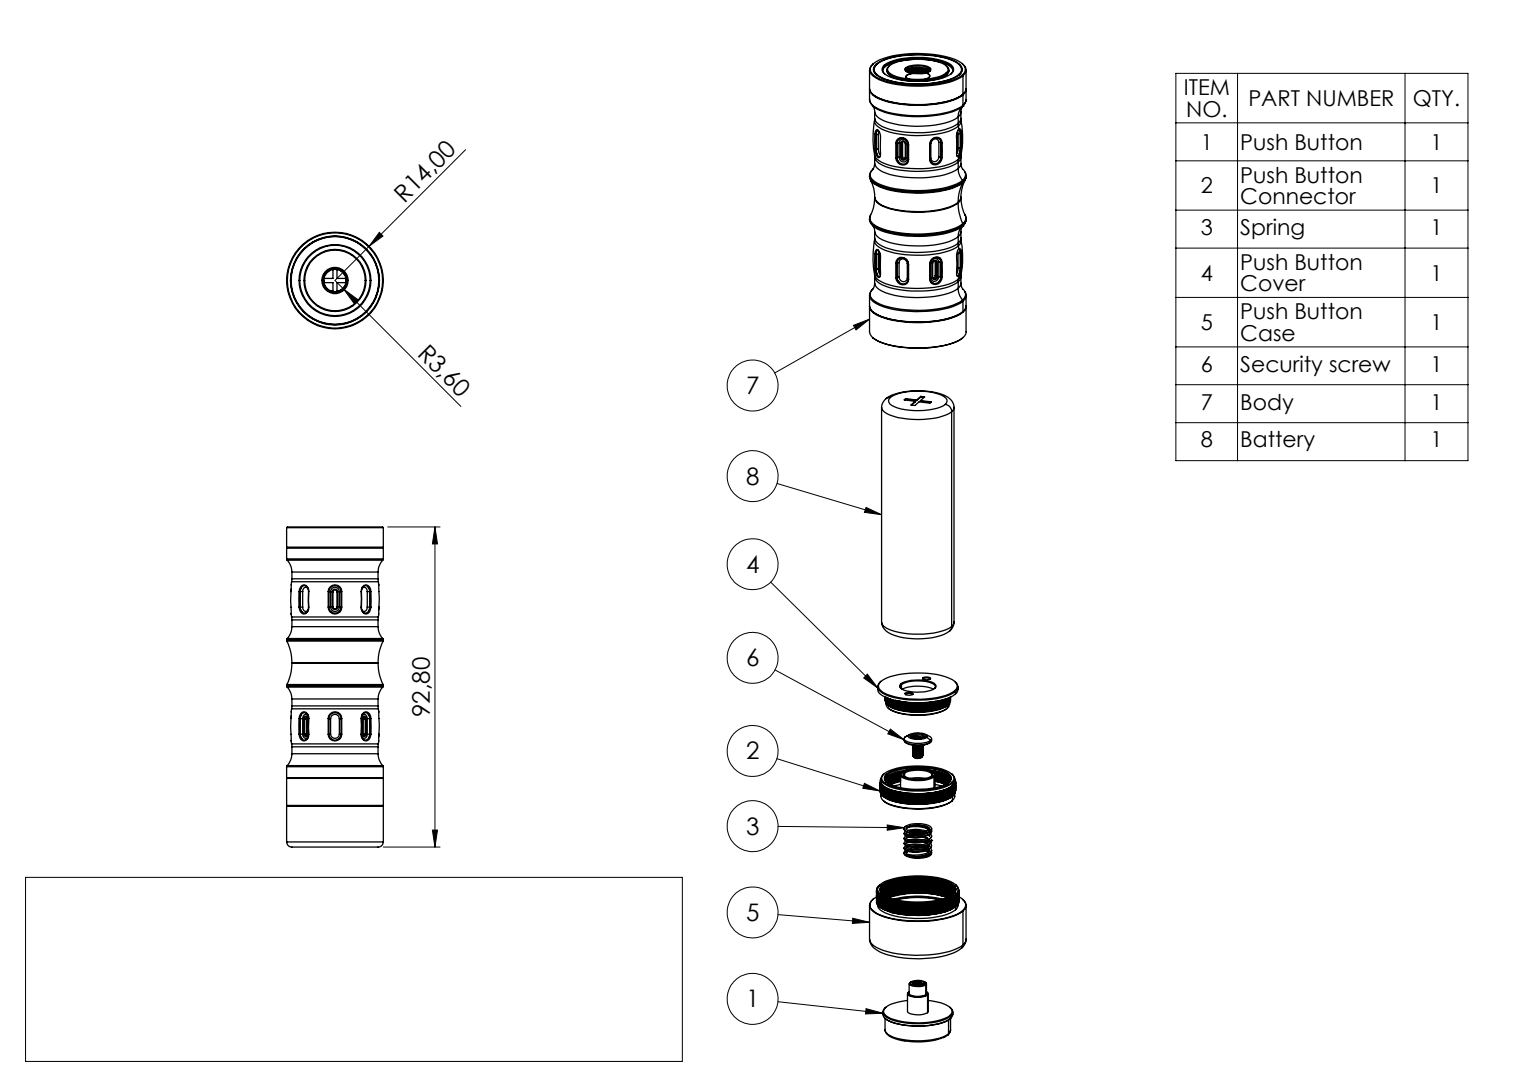
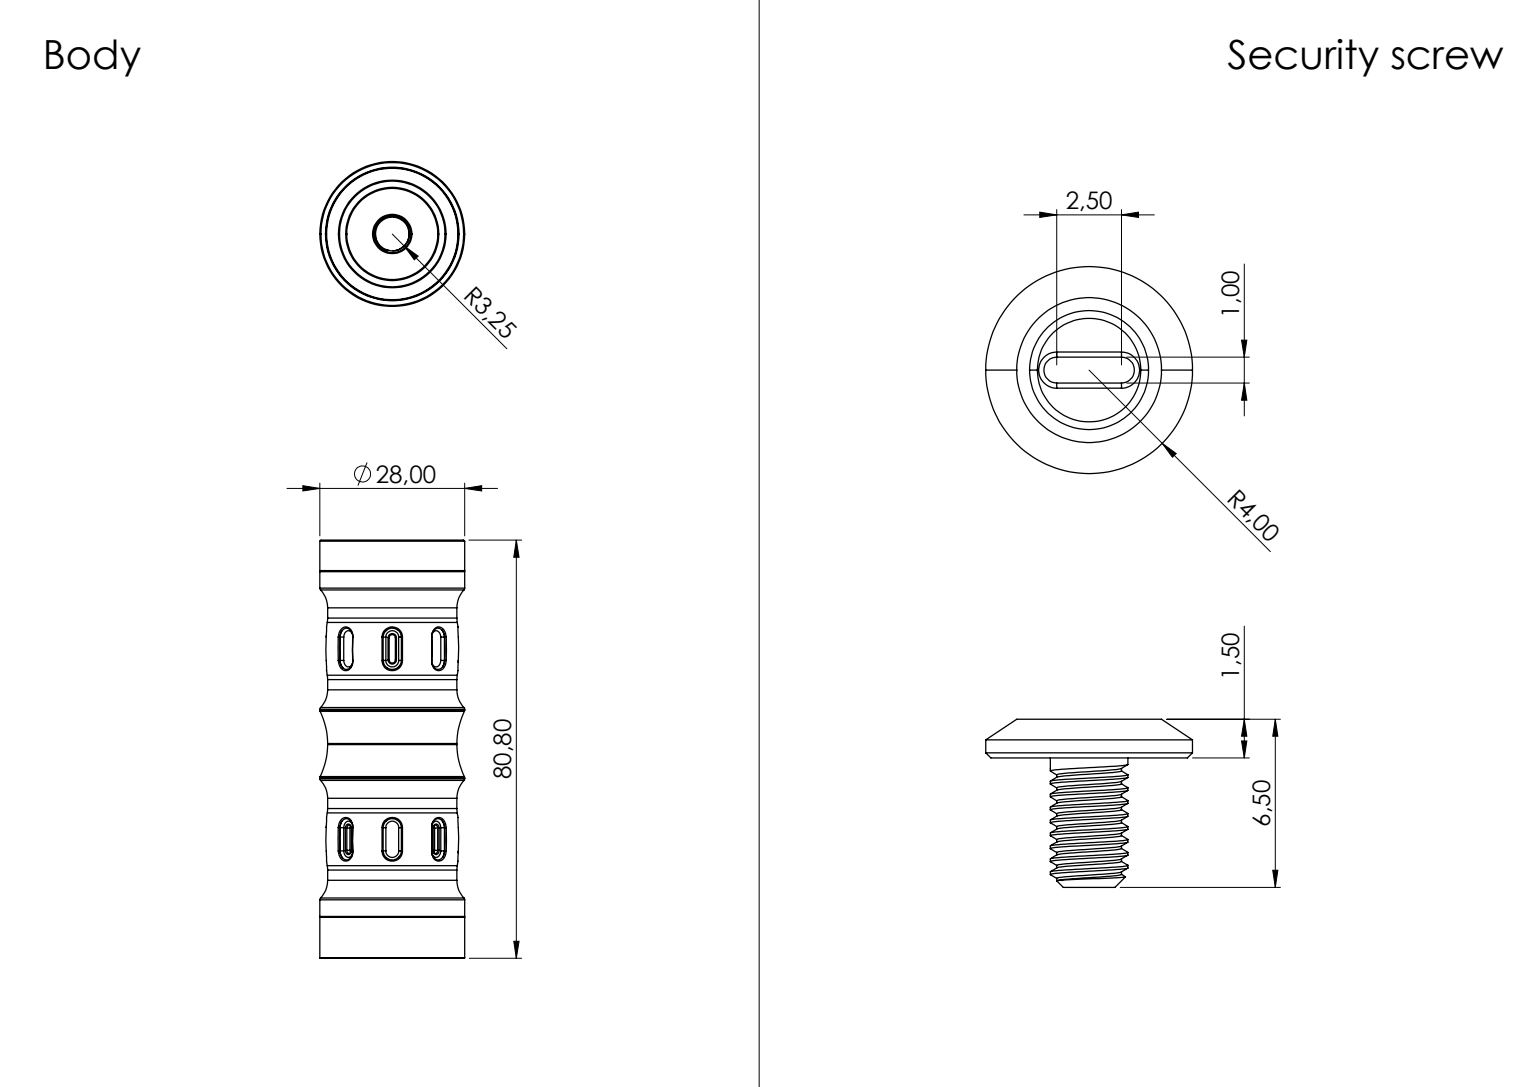
ISO-10303-21;
HEADER;
FILE_DESCRIPTION (('STEP AP214'),
    '1' );
FILE_NAME ('MAS-694',
    '2026-10-07T19:06:49',
    ( '' ),
    ( '' ),
    'SwSTEP 2.0',
    'SolidWorks 2020',
    '' );
FILE_SCHEMA (( 'AUTOMOTIVE_DESIGN' ));
ENDSEC;

DATA;
#1 = CIRCLE ( 'NONE', #2803, 1.199999999999999956 ) ;
#2 = CARTESIAN_POINT ( 'NONE',  ( 2.783482194004999855, -79.54451332859899537, 9.108908728793998932 ) ) ;
#3 = EDGE_CURVE ( 'NONE', #26450, #22997, #2825, .T. ) ;
#4 = CARTESIAN_POINT ( 'NONE',  ( 1.472546342128999930, -80.60010221862999913, -0.7790162248558000213 ) ) ;
#5 = EDGE_LOOP ( 'NONE', ( #45388, #8761, #11979 ) ) ;
#6 = EDGE_CURVE ( 'NONE', #36712, #34390, #42931, .T. ) ;
#7 = CARTESIAN_POINT ( 'NONE',  ( 5.443609589771999602, -77.26340414414998747, 9.675369385899999841 ) ) ;
#8 = CARTESIAN_POINT ( 'NONE',  ( 7.169653208691478596, -77.87460860825220266, -9.346314528427997814 ) ) ;
#9 = CARTESIAN_POINT ( 'NONE',  ( -3.165411199172024848, -1.020833333333333703, -0.8506806241676611036 ) ) ;
#10 = ORIENTED_EDGE ( 'NONE', *, *, #20290, .T. ) ;
#11 = ORIENTED_EDGE ( 'NONE', *, *, #14208, .F. ) ;
#12 = CARTESIAN_POINT ( 'NONE',  ( -9.835237363953000411, -54.71864156536999957, -7.760968332694998750 ) ) ;
#13 = CARTESIAN_POINT ( 'NONE',  ( 8.944729675425000082, -79.55274183760799644, 3.923329690209000908 ) ) ;
#14 = EDGE_CURVE ( 'NONE', #5429, #41516, #2225, .T. ) ;
#15 = EDGE_LOOP ( 'NONE', ( #31939, #1109, #23065, #57706 ) ) ;
#16 = CARTESIAN_POINT ( 'NONE',  ( 3.109033293168000256, -77.33638120859698972, -11.95479571607999958 ) ) ;
#17 = CARTESIAN_POINT ( 'NONE',  ( -7.954951288349001004, -60.04999999966999980, 9.722718241315000398 ) ) ;
#18 = CARTESIAN_POINT ( 'NONE',  ( -1.435687946562000272, -77.69186995290999675, 0.2750228405014999988 ) ) ;
#19 = VERTEX_POINT ( 'NONE', #36148 ) ;
#20 = CARTESIAN_POINT ( 'NONE',  ( 4.897371265365999982, -76.96065194988499059, 7.847181321287999722 ) ) ;
#21 = CARTESIAN_POINT ( 'NONE',  ( 0.06046471609518229429, -80.22932665438294464, -1.248482646815343600 ) ) ;
#22 = CARTESIAN_POINT ( 'NONE',  ( 11.95031029473000039, -77.77814994903998524, 5.399609419473999417 ) ) ;
#23 = CARTESIAN_POINT ( 'NONE',  ( -2.309466437478999712, -77.64150279751002870, 10.97654204954999990 ) ) ;
#24 = CARTESIAN_POINT ( 'NONE',  ( -2.375816180258031540, -86.25171435493598437, 3.206979491546134931 ) ) ;
#25 = CARTESIAN_POINT ( 'NONE',  ( 8.240135455977000589, -77.95571942709864288, -5.125512367919999868 ) ) ;
#26 = CARTESIAN_POINT ( 'NONE',  ( 6.712914363625387182, -79.91051976297769954, 6.366836982130202216 ) ) ;
#27 = CARTESIAN_POINT ( 'NONE',  ( -10.75000000000000000, -80.44999999999998863, 5.225043809877999334E-10 ) ) ;
#28 = ORIENTED_EDGE ( 'NONE', *, *, #14602, .F. ) ;
#29 = CARTESIAN_POINT ( 'NONE',  ( 7.764258067048000811, -77.05084123326183487, 5.767450660628000492 ) ) ;
#30 = CARTESIAN_POINT ( 'NONE',  ( -9.844172144369998989, -76.00075078459998679, 7.391061701651999272 ) ) ;
#31 = CARTESIAN_POINT ( 'NONE',  ( -1.435212230719999926, -80.44593403531600018, -0.7398511866349000154 ) ) ;
#32 = AXIS2_PLACEMENT_3D ( 'NONE', #6356, #50954, #38231 ) ;
#33 = ADVANCED_FACE ( 'NONE', ( #3684 ), #39982, .F. ) ;
#34 = B_SPLINE_SURFACE_WITH_KNOTS ( 'NONE', 3, 3, ( 
 ( #2089, #37490, #2662, #20656, #6495, #56101, #24505, #42521, #42233, #28631, #6789, #20087, #38079, #55512, #1505, #24796, #1797, #15059, #42810, #33053, #25080, #24214, #38655, #46967, #15646, #19794, #43104, #51683, #56674, #55808, #19495, #11231, #29210, #7079, #2374 ),
 ( #11521, #15360, #29498, #51101, #47553, #10652, #47257, #41935, #28333, #32758, #46681, #50806, #38365, #51387, #56387, #15937, #33925, #6201, #33354, #10944, #10350, #46384, #5908, #23917, #28924, #44244, #34791, #3513, #4087, #3796, #20938, #21798, #39803, #57525, #44532 ),
 ( #52815, #57816, #48399, #17375, #35362, #53387, #12933, #7650, #48682, #38940, #56957, #21514, #30931, #16518, #48971, #8512, #21224, #17086, #26506, #43963, #3233, #22085, #35069, #40099, #16230, #34209, #53105, #12654, #52246, #30648, #12085, #8226, #43380, #12370, #11803 ),
 ( #39520, #25649, #48118, #7364, #26228, #34499, #29777, #47833, #43675, #25364, #2939, #39229, #52528, #30067, #57242, #16806, #30358, #7936, #25938, #36844, #4690, #584, #41281, #27399, #45139, #46026, #18566, #5547, #54856, #9997, #36557, #54579, #14403, #14119, #53990 ) ),
 .UNSPECIFIED., .F., .F., .F.,
 ( 4, 4 ),
 ( 4, 1, 1, 1, 1, 1, 1, 1, 1, 1, 1, 1, 1, 1, 1, 1, 1, 1, 1, 1, 1, 1, 1, 1, 1, 1, 1, 1, 1, 1, 1, 1, 4 ),
 ( -0.1387574078320999993, 1.138757407831999968 ),
 ( 0.3298824860954999716, 0.3512342696267000131, 0.3725860531579999746, 0.3939378366892999916, 0.4152896202206000087, 0.4366414037517999946, 0.4579931872831000117, 0.4793449708143999732, 0.5006967543456000147, 0.5220485378768999762, 0.5434003214082000488, 0.5647521049395000103, 0.5861038884707000518, 0.6074556720019999023, 0.6288074555332999749, 0.6501592390646000474, 0.6715110225957999779, 0.6928628061271000504, 0.7142145896584000120, 0.7355663731896000535, 0.7569181567209000150, 0.7782699402522000875, 0.7996217237835000491, 0.8209735073147000906, 0.8423252908460000521, 0.8636770743773000136, 0.8850288579085000551, 0.9063806414398000166, 0.9277324249710999782, 0.9490842085024000507, 0.9704359920335999812, 0.9917877755649000537, 1.013139559096000175 ),
 .UNSPECIFIED. ) ;
#35 = CARTESIAN_POINT ( 'NONE',  ( -0.2380956042587999977, -78.76861702419900269, -1.297642515519999984 ) ) ;
#36 = CARTESIAN_POINT ( 'NONE',  ( -0.9024763166187672603, -2.953607843777506403, -3.403194172902606951 ) ) ;
#37 = AXIS2_PLACEMENT_3D ( 'NONE', #47276, #15952, #33942 ) ;
#38 = CARTESIAN_POINT ( 'NONE',  ( 12.71658872084999992, -23.31584731985000047, 1.931087888240000217 ) ) ;
#39 = CARTESIAN_POINT ( 'NONE',  ( -6.620362748380999918, -76.28137637478999977, -10.34376132320999986 ) ) ;
#40 = CARTESIAN_POINT ( 'NONE',  ( -9.243123480579969353, -61.71653773535206966, -8.441201026360992898 ) ) ;
#41 = CARTESIAN_POINT ( 'NONE',  ( 9.855576673225998618, -79.76811006564999218, -5.230603033304000782 ) ) ;
#42 = CARTESIAN_POINT ( 'NONE',  ( -6.243826001791999758, -76.87571332859899087, 7.064314876436000645 ) ) ;
#43 = CARTESIAN_POINT ( 'NONE',  ( 10.81044927328497174, -77.33600844987223866, 5.253279465540470206 ) ) ;
#44 = CARTESIAN_POINT ( 'NONE',  ( -0.9806565569677715422, -83.04738115356282435, 0.7753017405169410070 ) ) ;
#45 = CARTESIAN_POINT ( 'NONE',  ( 3.708203932500000022, -75.80000000000001137, 11.41267819554000162 ) ) ;
#46 = CARTESIAN_POINT ( 'NONE',  ( 2.813789756862229652, -77.85416666666665719, 10.47020627418440064 ) ) ;
#47 = ORIENTED_EDGE ( 'NONE', *, *, #21166, .F. ) ;
#48 = CARTESIAN_POINT ( 'NONE',  ( 1.362316189135000188, -81.60059162671998934, -0.8114345006153000917 ) ) ;
#49 = CARTESIAN_POINT ( 'NONE',  ( -1.300896064473999969, -80.54177512065000144, -0.3655689422679000433 ) ) ;
#50 = CARTESIAN_POINT ( 'NONE',  ( -10.20076187689604374, -79.12621043184928737, -3.463739626987611064 ) ) ;
#51 = DIRECTION ( 'NONE',  ( 0.000000000000000000, 0.000000000000000000, -1.000000000000000000 ) ) ;
#52 = CARTESIAN_POINT ( 'NONE',  ( 8.130811096541000538, -24.68523690389000080, 9.546858433121998999 ) ) ;
#53 = EDGE_CURVE ( 'NONE', #3236, #26282, #39951, .T. ) ;
#54 = CARTESIAN_POINT ( 'NONE',  ( -1.508789225394999933, -82.23555239048998544, 0.7062677124845000431 ) ) ;
#55 = CARTESIAN_POINT ( 'NONE',  ( -11.91766194687999914, -78.07234609596400787, 0.6362673702790999641 ) ) ;
#56 = CARTESIAN_POINT ( 'NONE',  ( 1.899930039692999895, -78.36919415034600434, 9.535935523283001203 ) ) ;
#57 = CARTESIAN_POINT ( 'NONE',  ( -1.698401934078999975, -54.57985954063000378, -12.66748707609000135 ) ) ;
#58 = CARTESIAN_POINT ( 'NONE',  ( 8.691395350247656637, -76.00817847884788137, 7.907189969528280571 ) ) ;
#59 = CARTESIAN_POINT ( 'NONE',  ( 7.698699457163000304, -79.83930274324279708, 7.739857405570000459 ) ) ;
#60 = CARTESIAN_POINT ( 'NONE',  ( 3.757989199629864441, -86.07389998728977787, 2.729540522068179875 ) ) ;
#61 = ORIENTED_EDGE ( 'NONE', *, *, #20316, .F. ) ;
#62 = CARTESIAN_POINT ( 'NONE',  ( 11.83799436920362957, -75.81835910994890071, 2.768346231419584136 ) ) ;
#63 = CARTESIAN_POINT ( 'NONE',  ( 1.978576907476575553, -78.62148120184446043, -3.425895241845613892 ) ) ;
#64 = AXIS2_PLACEMENT_3D ( 'NONE', #12751, #31031, #13327 ) ;
#65 = CARTESIAN_POINT ( 'NONE',  ( -14.00000000000000000, -46.09579702914000165, 0.000000000000000000 ) ) ;
#66 = CARTESIAN_POINT ( 'NONE',  ( -6.405050160242000246, -78.85473773677898635, 8.912875463421000788 ) ) ;
#67 = CARTESIAN_POINT ( 'NONE',  ( 11.00000000000000000, -79.34999999999999432, -1.064824513673000067E-14 ) ) ;
#68 = CARTESIAN_POINT ( 'NONE',  ( 1.570796326794856590, -77.76458333333333428, 12.00000000000000711 ) ) ;
#69 = CARTESIAN_POINT ( 'NONE',  ( -0.5999999999999999778, -5.000000000000000000, 0.5999999999999999778 ) ) ;
#70 = FACE_OUTER_BOUND ( 'NONE', #58213, .T. ) ;
#71 = ORIENTED_EDGE ( 'NONE', *, *, #32080, .F. ) ;
#72 = CARTESIAN_POINT ( 'NONE',  ( 6.724228645090999379, -79.38539396382098801, -8.890407735272999545 ) ) ;
#73 = CARTESIAN_POINT ( 'NONE',  ( 0.8787695232493443198, -79.91340179010917666, 0.8885763300944270471 ) ) ;
#74 = CARTESIAN_POINT ( 'NONE',  ( 7.921865660077126670, -75.80000000000001137, -8.886071780246803442 ) ) ;
#75 = CARTESIAN_POINT ( 'NONE',  ( -4.006190210801564788, -78.54828561723800817, 2.263637798799203349 ) ) ;
#76 = EDGE_CURVE ( 'NONE', #36029, #6234, #44439, .T. ) ;
#78 = CARTESIAN_POINT ( 'NONE',  ( -0.5731630996927263855, -81.51327970983244597, 1.110821756836525287 ) ) ;
#77 = CARTESIAN_POINT ( 'NONE',  ( 1.232689987415999999, -80.87906169571699877, -0.4701533967999000363 ) ) ;
#79 = CARTESIAN_POINT ( 'NONE',  ( -5.793600105730999594, -78.22586176634699484, 9.408086495002001115 ) ) ;
#80 = ADVANCED_FACE ( 'NONE', ( #13408 ), #31504, .F. ) ;
#81 = DIRECTION ( 'NONE',  ( -0.7071067811865475727, 0.000000000000000000, -0.7071067811865475727 ) ) ;
#82 = CARTESIAN_POINT ( 'NONE',  ( 10.98965142020543517, -23.51557447649318888, -0.4775239249309967127 ) ) ;
#83 = AXIS2_PLACEMENT_3D ( 'NONE', #16611, #21316, #34596 ) ;
#84 = TOROIDAL_SURFACE ( 'NONE', #10300, 17.50000000000000000, 5.000000000000000000 ) ;
#85 = CARTESIAN_POINT ( 'NONE',  ( -11.65000000000000036, -75.20000000000000284, 0.000000000000000000 ) ) ;
#86 = CARTESIAN_POINT ( 'NONE',  ( -12.00000000000000000, -60.04999999966999980, -1.250000000000000000 ) ) ;
#87 = DIRECTION ( 'NONE',  ( 0.000000000000000000, 1.000000000000000000, 0.000000000000000000 ) ) ;
#88 = CARTESIAN_POINT ( 'NONE',  ( -1.250000000000000000, -80.00000000000000000, 0.000000000000000000 ) ) ;
#89 = VERTEX_POINT ( 'NONE', #22267 ) ;
#90 = EDGE_CURVE ( 'NONE', #54593, #16250, #40282, .T. ) ;
#91 = ORIENTED_EDGE ( 'NONE', *, *, #55507, .T. ) ;
#92 = CARTESIAN_POINT ( 'NONE',  ( 0.000000000000000000, -18.75000000000000000, 12.00000000000000000 ) ) ;
#93 = CARTESIAN_POINT ( 'NONE',  ( 3.039902587998999817, -77.28013998579800159, -9.045419714114000698 ) ) ;
#94 = ORIENTED_EDGE ( 'NONE', *, *, #34546, .F. ) ;
#95 = CARTESIAN_POINT ( 'NONE',  ( -12.02296678431999943, -78.53620577153000681, 2.418109797047000242 ) ) ;
#96 = ORIENTED_EDGE ( 'NONE', *, *, #34117, .T. ) ;
#97 = CARTESIAN_POINT ( 'NONE',  ( 7.956422463014998669, -24.52889896183999596, 9.787948076355000637 ) ) ;
#98 = CARTESIAN_POINT ( 'NONE',  ( 6.225574660483999878, -77.96842036916400787, 9.107357164861998200 ) ) ;
#99 = CARTESIAN_POINT ( 'NONE',  ( 7.342356150419300675, -55.61035107871643390, -8.190836719257356791 ) ) ;
#100 = CARTESIAN_POINT ( 'NONE',  ( -9.706274203897999442, -78.20406332859900544, -1.344096209030999800 ) ) ;
#101 = FACE_OUTER_BOUND ( 'NONE', #29091, .T. ) ;
#102 = CARTESIAN_POINT ( 'NONE',  ( 10.54265532893000135, -78.47604828264000787, 3.830212845596999927 ) ) ;
#103 = CARTESIAN_POINT ( 'NONE',  ( 10.87736683009447525, -81.00000000000001421, 1.725104219249947057 ) ) ;
#104 = EDGE_LOOP ( 'NONE', ( #8306, #56264, #8122, #44410 ) ) ;
#105 = AXIS2_PLACEMENT_3D ( 'NONE', #46882, #51305, #55725 ) ;
#106 = ORIENTED_EDGE ( 'NONE', *, *, #28761, .F. ) ;
#107 = B_SPLINE_CURVE_WITH_KNOTS ( 'NONE', 3,
 ( #7548, #48867, #4281, #31114, #3130, #21981 ),
 .UNSPECIFIED., .F., .F.,
 ( 4, 2, 4 ),
 ( 0.000000000000000000, 0.5000000000000000000, 1.000000000000000000 ),
 .UNSPECIFIED. ) ;
#108 = CARTESIAN_POINT ( 'NONE',  ( -6.065106684382000068, -77.35143450949497890, 9.224892016835999797 ) ) ;
#109 = CARTESIAN_POINT ( 'NONE',  ( 1.243547092045969915, -77.53541666666666288, -9.500000000000000000 ) ) ;
#110 = CARTESIAN_POINT ( 'NONE',  ( -9.778086933892000232, -75.88734000069999297, -8.273004691245001041 ) ) ;
#111 = CARTESIAN_POINT ( 'NONE',  ( -5.219189444926520594, -79.47847823290939573, -7.938071756665344481 ) ) ;
#112 = DIRECTION ( 'NONE',  ( 0.000000000000000000, 0.7071067811866525998, -0.7071067811864425456 ) ) ;
#113 = CARTESIAN_POINT ( 'NONE',  ( -5.761654615528584600, -79.37404003602567570, -7.593432905074549488 ) ) ;
#114 = CARTESIAN_POINT ( 'NONE',  ( 12.61117324689999997, -18.78448536116999890, -1.798979683802999885 ) ) ;
#115 = CARTESIAN_POINT ( 'NONE',  ( -1.249999999999999778, -78.01041666666664298, -0.1636246173744686228 ) ) ;
#116 = CARTESIAN_POINT ( 'NONE',  ( 9.009247259181924150, -78.72916666666665719, -2.421167930323326001 ) ) ;
#117 = CARTESIAN_POINT ( 'NONE',  ( 2.039467698388000017, -84.90729426542299052, -3.154669836245999726 ) ) ;
#118 = ORIENTED_EDGE ( 'NONE', *, *, #11311, .T. ) ;
#119 = CARTESIAN_POINT ( 'NONE',  ( -10.96659098533000076, -79.41245439073298940, -5.858662427812999951 ) ) ;
#120 = CONICAL_SURFACE ( 'NONE', #10463, 13.94999999997000018, 0.7853981633972997312 ) ;
#121 = CARTESIAN_POINT ( 'NONE',  ( 2.970805461283999804, -76.56305898269899046, 11.10324980701000008 ) ) ;
#122 = CARTESIAN_POINT ( 'NONE',  ( -5.476929600924019148, -78.01766025678556105, 9.250714535254271453 ) ) ;
#123 = CARTESIAN_POINT ( 'NONE',  ( -4.085659785884999451, -78.53658950733898791, 11.26159174134999930 ) ) ;
#124 = CARTESIAN_POINT ( 'NONE',  ( 0.000000000000000000, -75.00000000000000000, -7.200000000000000178 ) ) ;
#125 = EDGE_CURVE ( 'NONE', #28960, #7174, #2934, .T. ) ;
#126 = AXIS2_PLACEMENT_3D ( 'NONE', #7144, #26004, #48189 ) ;
#127 = DIRECTION ( 'NONE',  ( 0.000000000000000000, -1.000000000000000000, 0.000000000000000000 ) ) ;
#128 = CYLINDRICAL_SURFACE ( 'NONE', #42114, 0.5000000000000004441 ) ;
#129 = CARTESIAN_POINT ( 'NONE',  ( 4.095273378172390899, -80.94411864974023274, 9.939233580224922093 ) ) ;
#130 = CARTESIAN_POINT ( 'NONE',  ( 11.22519961651999942, -80.38483504313998651, 1.998589004412999692 ) ) ;
#131 = CARTESIAN_POINT ( 'NONE',  ( 8.300970689365456678, -78.50833333333332575, -4.784380313523530326 ) ) ;
#132 = CARTESIAN_POINT ( 'NONE',  ( 8.145565103785999739, -77.70092985212998826, 7.609492079688000565 ) ) ;
#133 = CARTESIAN_POINT ( 'NONE',  ( 11.68767212001977995, -78.07083333333333997, 3.140974612311385972 ) ) ;
#134 = CARTESIAN_POINT ( 'NONE',  ( -1.803444444386999912, -80.27907522661350015, 10.99384993464000004 ) ) ;
#135 = ORIENTED_EDGE ( 'NONE', *, *, #46483, .F. ) ;
#136 = CARTESIAN_POINT ( 'NONE',  ( 2.839779323407650047, -1.393182233394845593, 1.634486084188475852 ) ) ;
#137 = CARTESIAN_POINT ( 'NONE',  ( 0.5154756746320998673, -53.66759400203999775, 12.66205448068000017 ) ) ;
#138 = CARTESIAN_POINT ( 'NONE',  ( 2.459440699436000077, -77.29584903538302854, -9.171074077620000153 ) ) ;
#139 = CARTESIAN_POINT ( 'NONE',  ( -9.850507815892395769, -24.30508874547875564, 7.836744050302930198 ) ) ;
#140 = CARTESIAN_POINT ( 'NONE',  ( 0.2654799511899000319, -78.39298939775198960, -11.21373274707999990 ) ) ;
#141 = CARTESIAN_POINT ( 'NONE',  ( -9.499999999999998224, -77.31041666666664014, -1.243547092045960367 ) ) ;
#142 = CYLINDRICAL_SURFACE ( 'NONE', #54331, 3.250000000000000000 ) ;
#143 = CARTESIAN_POINT ( 'NONE',  ( -1.484804496640999893, -61.51869153350000374, 12.77261165612999960 ) ) ;
#144 = CARTESIAN_POINT ( 'NONE',  ( 12.72554264791999934, -18.79839278105999867, 1.930240062458999928 ) ) ;
#145 = CARTESIAN_POINT ( 'NONE',  ( 2.284785568762000008, -82.74324735065199832, 3.494178859388000102 ) ) ;
#146 = CARTESIAN_POINT ( 'NONE',  ( 0.000000000000000000, -86.20000000000000284, 0.000000000000000000 ) ) ;
#147 = CARTESIAN_POINT ( 'NONE',  ( 10.31444587876999996, -54.49924218061999426, -7.758886158083000417 ) ) ;
#148 = AXIS2_PLACEMENT_3D ( 'NONE', #56838, #53267, #47996 ) ;
#149 = B_SPLINE_CURVE_WITH_KNOTS ( 'NONE', 3,
 ( #55404, #38266, #46279, #42423, #24107, #37685, #55701, #15248, #52939, #7198, #42935, #33761, #52652, #47672, #2489, #16927, #57077, #43805 ),
 .UNSPECIFIED., .F., .F.,
 ( 4, 2, 2, 2, 2, 2, 2, 2, 4 ),
 ( 0.000000000000000000, 0.1250000000000000833, 0.2500000000000001110, 0.3750000000000000000, 0.4999999999999999445, 0.6249999999999998890, 0.7499999999999997780, 0.8749999999999998890, 1.000000000000000000 ),
 .UNSPECIFIED. ) ;
#150 = CARTESIAN_POINT ( 'NONE',  ( 0.1384068119873999858, -77.08287542851299179, 11.14609546546000018 ) ) ;
#151 = EDGE_CURVE ( 'NONE', #15969, #4126, #39694, .T. ) ;
#152 = CARTESIAN_POINT ( 'NONE',  ( -0.8033051684372000123, -80.29613481679999154, -1.459438184619000101 ) ) ;
#153 = CARTESIAN_POINT ( 'NONE',  ( -1.297701781740999927, -78.99170572834999859, -0.6115961818822999163 ) ) ;
#154 = CARTESIAN_POINT ( 'NONE',  ( -1.722320550025187025, -61.03663688784200048, 12.71171904440437928 ) ) ;
#155 = DIRECTION ( 'NONE',  ( -0.0001230612157835738363, 0.000000000000000000, 0.9999999924279686647 ) ) ;
#156 = CARTESIAN_POINT ( 'NONE',  ( -12.72394223973000038, -60.02159774832999517, 1.930881086224999876 ) ) ;
#157 = DIRECTION ( 'NONE',  ( 0.000000000000000000, -1.000000000000000000, 0.000000000000000000 ) ) ;
#158 = CARTESIAN_POINT ( 'NONE',  ( 0.000000000000000000, -75.19999999999998863, -4.999999999999962697 ) ) ;
#159 = CARTESIAN_POINT ( 'NONE',  ( 10.58961540942159729, -78.57316667069575544, -3.698874623828772634 ) ) ;
#160 = LINE ( 'NONE', #46472, #43214 ) ;
#161 = ORIENTED_EDGE ( 'NONE', *, *, #35079, .T. ) ;
#162 = DIRECTION ( 'NONE',  ( 0.000000000000000000, 1.000000000000000000, 0.000000000000000000 ) ) ;
#163 = CARTESIAN_POINT ( 'NONE',  ( -5.539808784079908399, -79.51666666666666572, 9.611650271896829523 ) ) ;
#164 = CARTESIAN_POINT ( 'NONE',  ( -0.4120475804594999625, -79.51319421340399174, -11.13933648663000042 ) ) ;
#165 = CARTESIAN_POINT ( 'NONE',  ( -12.50000000000000000, -17.31762331506999786, -1.005384022379999909 ) ) ;
#166 = ORIENTED_EDGE ( 'NONE', *, *, #27076, .T. ) ;
#167 = EDGE_CURVE ( 'NONE', #8218, #23965, #8695, .T. ) ;
#168 = ORIENTED_EDGE ( 'NONE', *, *, #42200, .F. ) ;
#169 = CARTESIAN_POINT ( 'NONE',  ( -0.06134698815010001388, -80.66909307349899905, -1.515015350337000077 ) ) ;
#170 = AXIS2_PLACEMENT_3D ( 'NONE', #825, #36799, #54241 ) ;
#171 = EDGE_CURVE ( 'NONE', #313, #521, #53642, .T. ) ;
#172 = ORIENTED_EDGE ( 'NONE', *, *, #44103, .T. ) ;
#173 = CARTESIAN_POINT ( 'NONE',  ( -6.000000000000000000, -81.99999999999998579, 0.000000000000000000 ) ) ;
#174 = ORIENTED_EDGE ( 'NONE', *, *, #20456, .F. ) ;
#175 = CIRCLE ( 'NONE', #40670, 12.90000000000000036 ) ;
#176 = CARTESIAN_POINT ( 'NONE',  ( 1.250000000000000000, -78.75000000000000000, 0.000000000000000000 ) ) ;
#177 = CARTESIAN_POINT ( 'NONE',  ( 3.250000000000000000, -1.250000000000000000, 0.000000000000000000 ) ) ;
#178 = CARTESIAN_POINT ( 'NONE',  ( 0.000000000000000000, 0.000000000000000000, 0.000000000000000000 ) ) ;
#179 = CARTESIAN_POINT ( 'NONE',  ( -0.1963495408493673433, -78.38541666666668561, 1.499999999999999334 ) ) ;
#180 = CARTESIAN_POINT ( 'NONE',  ( 2.061649843245999758, -23.20561307587000144, -12.83797346714000120 ) ) ;
#181 = CARTESIAN_POINT ( 'NONE',  ( -3.368292805027000014, -80.61420806598900413, -1.663121790705999858 ) ) ;
#182 = CARTESIAN_POINT ( 'NONE',  ( -9.065329452404249366, -79.37552650030312407, 2.840436040226053560 ) ) ;
#183 = CARTESIAN_POINT ( 'NONE',  ( 4.145485675599949182, -78.25643109645689321, -9.984513293680489454 ) ) ;
#184 = CARTESIAN_POINT ( 'NONE',  ( -12.05956633327999938, -78.83299827204000110, -0.2332108555899000124 ) ) ;
#185 = VERTEX_POINT ( 'NONE', #55030 ) ;
#186 = ORIENTED_EDGE ( 'NONE', *, *, #27821, .T. ) ;
#187 = FACE_OUTER_BOUND ( 'NONE', #5, .T. ) ;
#188 = CARTESIAN_POINT ( 'NONE',  ( -0.8465867926663999121, -80.83273884615699956, -0.9556525628790000226 ) ) ;
#189 = CARTESIAN_POINT ( 'NONE',  ( -7.843978203195000276, -77.65945010111499869, 5.713380375430999969 ) ) ;
#190 = EDGE_CURVE ( 'NONE', #21248, #3192, #25838, .T. ) ;
#191 = CARTESIAN_POINT ( 'NONE',  ( -1.569340319482204205, -86.39318692756697260, -3.437241610844480988 ) ) ;
#192 = DIRECTION ( 'NONE',  ( 0.000000000000000000, -1.000000000000000000, 0.000000000000000000 ) ) ;
#193 = CARTESIAN_POINT ( 'NONE',  ( -3.331828115504000376, -76.81423739310000087, 12.52045872913000046 ) ) ;
#194 = B_SPLINE_CURVE_WITH_KNOTS ( 'NONE', 3,
 ( #52120, #52408, #39679, #34947 ),
 .UNSPECIFIED., .F., .F.,
 ( 4, 4 ),
 ( 0.000000000000000000, 1.000000000000000000 ),
 .UNSPECIFIED. ) ;
#195 = CARTESIAN_POINT ( 'NONE',  ( -0.6515920321739999688, -80.16498426945000233, -1.183807013712999900 ) ) ;
#196 = CARTESIAN_POINT ( 'NONE',  ( -7.859650249856000137, -76.58738468523199572, -7.529696512734999736 ) ) ;
#197 = CARTESIAN_POINT ( 'NONE',  ( 12.00000000000000000, -78.14999999999999147, 0.000000000000000000 ) ) ;
#198 = AXIS2_PLACEMENT_3D ( 'NONE', #57985, #8985, #18719 ) ;
#199 = CARTESIAN_POINT ( 'NONE',  ( 3.909622331879000434, -81.21546018839499936, -0.6487244410423000929 ) ) ;
#200 = CARTESIAN_POINT ( 'NONE',  ( -11.26045488449999965, -80.83153675553073469, 0.3336940576009999604 ) ) ;
#201 = LINE ( 'NONE', #48879, #40279 ) ;
#202 = CARTESIAN_POINT ( 'NONE',  ( 7.624341766639000539, -23.26485146254000114, 10.42531125024000005 ) ) ;
#203 = CARTESIAN_POINT ( 'NONE',  ( 0.7883518021343000060, -81.29032046129098887, 3.458764816093999883 ) ) ;
#204 = EDGE_CURVE ( 'NONE', #1538, #36787, #12747, .T. ) ;
#205 = CARTESIAN_POINT ( 'NONE',  ( -0.8668440880359000733, -77.83435542797239748, -1.013523202003999923 ) ) ;
#206 = CYLINDRICAL_SURFACE ( 'NONE', #36450, 4.100000000000000533 ) ;
#207 = CARTESIAN_POINT ( 'NONE',  ( 8.440675369999999234, -80.13928997744719140, 7.053722371789000967 ) ) ;
#208 = CARTESIAN_POINT ( 'NONE',  ( 0.6793464540269460450, -80.58066705791090101, 1.078661931325863188 ) ) ;
#209 = EDGE_CURVE ( 'NONE', #23895, #25757, #23322, .T. ) ;
#210 = ORIENTED_EDGE ( 'NONE', *, *, #29786, .F. ) ;
#211 = CARTESIAN_POINT ( 'NONE',  ( -0.5999663639300912843, -23.18964892095168295, 10.98362601162691199 ) ) ;
#212 = CARTESIAN_POINT ( 'NONE',  ( 8.130813118348999780, -54.11476110100999648, -9.546856411313999757 ) ) ;
#213 = DIRECTION ( 'NONE',  ( 0.000000000000000000, 0.000000000000000000, 1.000000000000000000 ) ) ;
#214 = CARTESIAN_POINT ( 'NONE',  ( 1.931087888049999979, -60.11584477251999203, 12.71658889743999943 ) ) ;
#215 = CARTESIAN_POINT ( 'NONE',  ( -10.59876350475000173, -77.46807671118999394, 7.550195564144000393 ) ) ;
#216 = AXIS2_PLACEMENT_3D ( 'NONE', #10223, #37949, #14925 ) ;
#217 = CARTESIAN_POINT ( 'NONE',  ( 8.824144518603999288, -79.29006001420199823, -3.570895061352000077 ) ) ;
#218 = CARTESIAN_POINT ( 'NONE',  ( 12.82904109062999964, -23.32452273707999879, -2.062673488410000200 ) ) ;
#219 = ORIENTED_EDGE ( 'NONE', *, *, #4233, .T. ) ;
#220 = DIRECTION ( 'NONE',  ( 0.7071067811865475727, 0.000000000000000000, 0.7071067811865475727 ) ) ;
#221 = LINE ( 'NONE', #4907, #38945 ) ;
#222 = CARTESIAN_POINT ( 'NONE',  ( 1.058064258495000187, -81.94170750542799908, -0.7735121372284999852 ) ) ;
#223 = CARTESIAN_POINT ( 'NONE',  ( 7.678690995204998870, -21.75648180056000314, -10.59551070212000035 ) ) ;
#224 = CARTESIAN_POINT ( 'NONE',  ( -0.5444512524326000635, -78.07738533478699594, -9.506521396690999381 ) ) ;
#226 = CARTESIAN_POINT ( 'NONE',  ( -1.182840957218999955, -1.349210179781999752, -3.838043326965000279 ) ) ;
#225 = CARTESIAN_POINT ( 'NONE',  ( 3.634969262962000069, -85.51626360600299392, 2.053437490576000446 ) ) ;
#227 = FACE_OUTER_BOUND ( 'NONE', #43271, .T. ) ;
#228 = CARTESIAN_POINT ( 'NONE',  ( -0.9898995639662998558, -79.60058255474299926, 0.8721608040441000131 ) ) ;
#229 = EDGE_LOOP ( 'NONE', ( #45666, #3172, #6374, #35575 ) ) ;
#230 = CARTESIAN_POINT ( 'NONE',  ( 0.2080084001491119827, -77.22664242507777033, -10.74806830262927981 ) ) ;
#231 = DIRECTION ( 'NONE',  ( -1.000000000000000000, 0.000000000000000000, 0.000000000000000000 ) ) ;
#232 = DIRECTION ( 'NONE',  ( 0.000000000000000000, -1.000000000000000000, 0.000000000000000000 ) ) ;
#233 = VERTEX_POINT ( 'NONE', #25182 ) ;
#234 = ORIENTED_EDGE ( 'NONE', *, *, #57744, .T. ) ;
#235 = CARTESIAN_POINT ( 'NONE',  ( 3.166366903731000271, -79.72244757809599491, 10.47195928638999973 ) ) ;
#236 = LINE ( 'NONE', #58354, #29407 ) ;
#237 = VERTEX_POINT ( 'NONE', #51785 ) ;
#238 = CARTESIAN_POINT ( 'NONE',  ( -0.7898276719169999849, -78.74313915747200099, -11.90847071177000061 ) ) ;
#239 = ORIENTED_EDGE ( 'NONE', *, *, #27026, .F. ) ;
#240 = ORIENTED_EDGE ( 'NONE', *, *, #54504, .F. ) ;
#241 = LINE ( 'NONE', #35610, #56530 ) ;
#242 = CARTESIAN_POINT ( 'NONE',  ( 9.597438627498371844, -76.59723940367341299, -7.375897342311914073 ) ) ;
#243 = CARTESIAN_POINT ( 'NONE',  ( 2.866892793968622843, -1.159673730758707721, 2.818444692989894751 ) ) ;
#244 = ORIENTED_EDGE ( 'NONE', *, *, #50771, .T. ) ;
#245 = VERTEX_POINT ( 'NONE', #11335 ) ;
#246 = CARTESIAN_POINT ( 'NONE',  ( 1.251671508224674323, -80.38505487870085631, -0.2410332141617578250 ) ) ;
#247 = CARTESIAN_POINT ( 'NONE',  ( 3.992904449609000483, -78.77851881763733388, -2.356505974700060513 ) ) ;
#248 = CARTESIAN_POINT ( 'NONE',  ( 0.000000000000000000, -80.69999999999998863, -2.899999999999999911 ) ) ;
#249 = ADVANCED_FACE ( 'NONE', ( #43204 ), #20212, .F. ) ;
#250 = CARTESIAN_POINT ( 'NONE',  ( -0.3116081092031571242, -18.31315380223933786, 10.99615594221668857 ) ) ;
#251 = CARTESIAN_POINT ( 'NONE',  ( 3.075537641221509411, -77.15416666666668277, 11.44417895085272008 ) ) ;
#252 = EDGE_CURVE ( 'NONE', #52871, #40540, #47362, .T. ) ;
#253 = AXIS2_PLACEMENT_3D ( 'NONE', #30100, #47864, #51996 ) ;
#254 = DIRECTION ( 'NONE',  ( 0.9957542217973192056, 0.04890179604787090600, -0.07798810240099150748 ) ) ;
#255 = CARTESIAN_POINT ( 'NONE',  ( 7.642147947524999374, -56.01514526721999943, -10.55910102243999837 ) ) ;
#256 = CARTESIAN_POINT ( 'NONE',  ( 7.620617093578522905, -78.80203626096795233, -5.244489908162002223 ) ) ;
#257 = CARTESIAN_POINT ( 'NONE',  ( -10.18949719146000099, -23.21529250218000229, 7.645392405660000001 ) ) ;
#258 = CARTESIAN_POINT ( 'NONE',  ( -7.396886230003165252, -77.65219327641052871, -5.684603129138253053 ) ) ;
#259 = CARTESIAN_POINT ( 'NONE',  ( 0.9082395157416487397, -78.08405139807857154, -12.04149494368141227 ) ) ;
#260 = CARTESIAN_POINT ( 'NONE',  ( 0.8807115773125999691, -80.96678455456799384, 3.863978249925000164 ) ) ;
#261 = CARTESIAN_POINT ( 'NONE',  ( -7.282392150664000141, -77.69888667140099869, 6.502067388700999651 ) ) ;
#262 = VECTOR ( 'NONE', #19954, 1000.000000000000000 ) ;
#263 = CARTESIAN_POINT ( 'NONE',  ( -1.879551087701830880, -76.29218749999812133, 11.88134584529343485 ) ) ;
#264 = FACE_BOUND ( 'NONE', #18208, .T. ) ;
#265 = CARTESIAN_POINT ( 'NONE',  ( -0.005119011380138999839, -24.93813862189000119, 12.43705489344000092 ) ) ;
#266 = CARTESIAN_POINT ( 'NONE',  ( 1.862898869916999933, -85.71183183321298316, 3.018969991366999839 ) ) ;
#267 = EDGE_CURVE ( 'NONE', #43339, #56949, #56033, .T. ) ;
#268 = AXIS2_PLACEMENT_3D ( 'NONE', #41715, #55289, #29005 ) ;
#269 = CARTESIAN_POINT ( 'NONE',  ( -3.200978647831000501, -0.8315460165489000355, 2.321879312794999706 ) ) ;
#270 = CARTESIAN_POINT ( 'NONE',  ( 7.686918321195999937, -58.55560170965000566, 10.48771805380999922 ) ) ;
#271 = CARTESIAN_POINT ( 'NONE',  ( 8.599926684958175471, -79.81921486858095705, -3.562059774102686038 ) ) ;
#272 = CARTESIAN_POINT ( 'NONE',  ( 12.70556836347999941, -25.22772277227999993, 2.424222353299999887E-09 ) ) ;
#273 = CARTESIAN_POINT ( 'NONE',  ( 0.1201880509156493942, -80.71773650514016651, 1.541718551563904693 ) ) ;
#274 = CARTESIAN_POINT ( 'NONE',  ( 12.65989858210999941, -61.74344101100000159, -0.9743214026256999949 ) ) ;
#275 = CARTESIAN_POINT ( 'NONE',  ( 2.269106295766999856E-14, -92.56607767729998670, -10.93038838648999977 ) ) ;
#276 = CARTESIAN_POINT ( 'NONE',  ( -12.99510751537000353, -26.30294702886003222, -6.911973076623003642 ) ) ;
#277 = CARTESIAN_POINT ( 'NONE',  ( 5.013494814495999208, -77.86362032395699373, 9.697434492446999954 ) ) ;
#278 = CARTESIAN_POINT ( 'NONE',  ( 12.18149635271999820, -78.11332874153899297, -1.551427017228999894 ) ) ;
#279 = FACE_OUTER_BOUND ( 'NONE', #48060, .T. ) ;
#280 = EDGE_CURVE ( 'NONE', #6234, #56598, #9324, .T. ) ;
#281 = CARTESIAN_POINT ( 'NONE',  ( 0.000000000000000000, -3.000000000000000000, 0.000000000000000000 ) ) ;
#282 = CARTESIAN_POINT ( 'NONE',  ( 0.000000000000000000, -86.20000000000000284, 0.000000000000000000 ) ) ;
#283 = EDGE_LOOP ( 'NONE', ( #8504, #30368, #4564, #9836 ) ) ;
#284 = CARTESIAN_POINT ( 'NONE',  ( 3.273752395723000586, -82.55440783550699280, -1.206381456434000077 ) ) ;
#285 = ADVANCED_FACE ( 'NONE', ( #47941, #16045, #34029, #6309 ), #29659, .T. ) ;
#286 = CARTESIAN_POINT ( 'NONE',  ( -4.648821459404000045, -81.05100055871760389, 9.896537447400001852 ) ) ;
#287 = FACE_OUTER_BOUND ( 'NONE', #40391, .T. ) ;
#288 = CARTESIAN_POINT ( 'NONE',  ( -2.857465951524460479, -84.55833334385054911, 1.921468474764645995 ) ) ;
#289 = CARTESIAN_POINT ( 'NONE',  ( 7.508079800428999917, -77.01725177193199556, -8.333477563431999968 ) ) ;
#290 = CARTESIAN_POINT ( 'NONE',  ( 0.000000000000000000, -76.75499999999999545, 0.000000000000000000 ) ) ;
#291 = CARTESIAN_POINT ( 'NONE',  ( 0.8649477812003000254, -78.46126277754198952, -9.701111330267998767 ) ) ;
#292 = VECTOR ( 'NONE', #35631, 1000.000000000000227 ) ;
#293 = CARTESIAN_POINT ( 'NONE',  ( 12.20990109347999919, -76.98480431993999673, -3.270330254029999661 ) ) ;
#294 = CARTESIAN_POINT ( 'NONE',  ( 8.002843206562666012, -78.09666666666663559, 5.305121725754472273 ) ) ;
#295 = FACE_OUTER_BOUND ( 'NONE', #22680, .T. ) ;
#296 = CARTESIAN_POINT ( 'NONE',  ( -1.799490220168999954, -56.02870851050000311, 12.64502302235999842 ) ) ;
#297 = ORIENTED_EDGE ( 'NONE', *, *, #43829, .F. ) ;
#298 = CARTESIAN_POINT ( 'NONE',  ( 1.495357591673911246, -54.24123662600908347, -12.70444646756140550 ) ) ;
#299 = DIRECTION ( 'NONE',  ( 0.000000000000000000, -1.000000000000000000, 1.006602208993000011E-13 ) ) ;
#300 = LINE ( 'NONE', #27694, #13909 ) ;
#301 = FACE_OUTER_BOUND ( 'NONE', #47142, .T. ) ;
#302 = AXIS2_PLACEMENT_3D ( 'NONE', #58162, #9457, #44888 ) ;
#303 = CARTESIAN_POINT ( 'NONE',  ( -12.82904109059999875, -55.47547726255000100, -2.062673488410000200 ) ) ;
#304 = CARTESIAN_POINT ( 'NONE',  ( 10.98960559191261765, -23.51693928699155833, 0.4813395862318616270 ) ) ;
#305 = ORIENTED_EDGE ( 'NONE', *, *, #4247, .T. ) ;
#306 = DIRECTION ( 'NONE',  ( 0.000000000000000000, -1.000000000000000000, 0.000000000000000000 ) ) ;
#307 = ORIENTED_EDGE ( 'NONE', *, *, #4039, .F. ) ;
#308 = VERTEX_POINT ( 'NONE', #1507 ) ;
#309 = TOROIDAL_SURFACE ( 'NONE', #16338, 13.50000000000000000, 0.5000000000000000000 ) ;
#310 = CARTESIAN_POINT ( 'NONE',  ( -7.605690612596999856, -55.37434870709000023, -10.52682230156000109 ) ) ;
#311 = AXIS2_PLACEMENT_3D ( 'NONE', #35658, #30929, #8510 ) ;
#312 = CARTESIAN_POINT ( 'NONE',  ( 8.944729675425000082, -79.61304476327899238, 3.923329690209000908 ) ) ;
#313 = VERTEX_POINT ( 'NONE', #37790 ) ;
#314 = CARTESIAN_POINT ( 'NONE',  ( 1.293235748077000036, -76.48998211639099054, 12.16612483867000094 ) ) ;
#315 = CARTESIAN_POINT ( 'NONE',  ( -10.47027344149396377, -78.61824586144523153, -2.436629557234976762 ) ) ;
#316 = CARTESIAN_POINT ( 'NONE',  ( 1.009608792702000102, -77.94743573086999788, -1.302912760256000224 ) ) ;
#317 = ORIENTED_EDGE ( 'NONE', *, *, #37608, .T. ) ;
#318 = CARTESIAN_POINT ( 'NONE',  ( 7.430757984336000099, -77.37342305011499377, 5.911115298933000695 ) ) ;
#319 = CARTESIAN_POINT ( 'NONE',  ( 1.156290009273217123, -80.31913236748124518, -0.4746485085928086600 ) ) ;
#320 = CARTESIAN_POINT ( 'NONE',  ( 0.3695519436384570033, -77.84114583351794181, -1.371859334843410050 ) ) ;
#321 = CARTESIAN_POINT ( 'NONE',  ( -1.570796326794885012, -78.91458333333333997, -12.00000000000000178 ) ) ;
#322 = CARTESIAN_POINT ( 'NONE',  ( -3.677663026309978989, -86.17851881763699851, 1.555017880481419423 ) ) ;
#323 = CARTESIAN_POINT ( 'NONE',  ( -7.203390125892000562, -78.80843430096776103, -6.502451851937000704 ) ) ;
#324 = CARTESIAN_POINT ( 'NONE',  ( 8.238920321119756807, -79.88802510210236107, 4.204434926243399318 ) ) ;
#325 = CARTESIAN_POINT ( 'NONE',  ( 1.131620348041424196, -79.14322915056125396, -3.849499586317910449 ) ) ;
#326 = VERTEX_POINT ( 'NONE', #36627 ) ;
#327 = CARTESIAN_POINT ( 'NONE',  ( -9.497876546326999403, -77.25168256874098915, -0.2008509664869000122 ) ) ;
#328 = CARTESIAN_POINT ( 'NONE',  ( 0.09829970619593025871, -77.22591789683764318, -9.271508350125035491 ) ) ;
#329 = CARTESIAN_POINT ( 'NONE',  ( 0.5881506857339000582, -79.69598562025299771, 1.397505295191999952 ) ) ;
#330 = AXIS2_PLACEMENT_3D ( 'NONE', #48177, #7132, #57011 ) ;
#331 = CARTESIAN_POINT ( 'NONE',  ( 1.081559480311999888, -3.500000000000000000, -3.328697807033000000 ) ) ;
#332 = CARTESIAN_POINT ( 'NONE',  ( 12.53241208775999915, -19.23537109840999904, 1.667936697358999965 ) ) ;
#333 = LINE ( 'NONE', #13274, #40446 ) ;
#334 = DIRECTION ( 'NONE',  ( 0.000000000000000000, 1.000000000000000000, 1.686839199259000058E-13 ) ) ;
#335 = ADVANCED_FACE ( 'NONE', ( #15362 ), #37204, .T. ) ;
#336 = CARTESIAN_POINT ( 'NONE',  ( 8.828604248290998768, -77.09468998579799859, -4.107095029376999662 ) ) ;
#337 = CARTESIAN_POINT ( 'NONE',  ( 11.73341735579898248, -77.28263860279511732, -2.603816878860229167 ) ) ;
#338 = CARTESIAN_POINT ( 'NONE',  ( 12.29321436482372754, -76.17567889517343360, -4.311296892563305505 ) ) ;
#339 = AXIS2_PLACEMENT_3D ( 'NONE', #14294, #32288, #37316 ) ;
#340 = B_SPLINE_SURFACE_WITH_KNOTS ( 'NONE', 3, 3, ( 
 ( #36923, #41947, #19221, #6213, #37214, #50233, #55227, #23928, #24228, #31902, #42247, #37801, #55822, #49944, #39721, #48600, #53600, #44746, #26424, #44446, #4297, #3998, #30274, #3150, #13435, #57729, #35875, #48887, #58323, #53307, #57447, #21432, #39146, #8430, #34703 ),
 ( #8725, #16720, #57155, #3713, #48315, #49172, #22002, #22298, #43587, #52734, #17286, #48037, #12850, #34988, #44166, #12285, #26718, #21716, #7855, #40314, #40008, #17886, #21139, #25855, #35274, #7567, #30850, #53017, #58025, #43884, #53904, #3430, #12570, #13140, #17586 ),
 ( #35573, #39440, #17006, #31133, #30567, #8146, #26145, #25567, #18470, #45931, #36461, #54769, #4602, #32306, #1348, #14311, #4892, #1063, #19341, #50354, #5464, #5751, #19052, #46227, #31729, #14024, #45049, #41773, #27596, #37336, #18758, #18182, #54488, #36177, #37041 ),
 ( #55058, #50064, #27310, #14605, #45341, #32600, #40901, #45638, #49476, #50648, #778, #23183, #41189, #9027, #27013, #22600, #22889, #490, #19628, #2500, #42945, #56231, #1935, #15781, #20505, #38502, #24051, #32892, #56518, #15194, #52095, #43230, #7208, #2219, #50937 ) ),
 .UNSPECIFIED., .F., .F., .F.,
 ( 4, 4 ),
 ( 4, 1, 1, 1, 1, 1, 1, 1, 1, 1, 1, 1, 1, 1, 1, 1, 1, 1, 1, 1, 1, 1, 1, 1, 1, 1, 1, 1, 1, 1, 1, 1, 4 ),
 ( -0.02000000000000999936, 1.020000000000000018 ),
 ( 0.1112507840917000002, 0.1395687738142999956, 0.1678867635369000189, 0.1962047532594000110, 0.2245227429820000065, 0.2528407327046000019, 0.2811587224271000496, 0.3094767121496999618, 0.3377947018722999850, 0.3661126915947999771, 0.3944306813174000004, 0.4227486710400000236, 0.4510666607625000157, 0.4793846504851000390, 0.5077026402076999512, 0.5360206299302000543, 0.5643386196528000776, 0.5926566093753999898, 0.6209745990978999819, 0.6492925888205000051, 0.6776105785431000283, 0.7059285682657000516, 0.7342465579881999327, 0.7625645477107999559, 0.7908825374333999791, 0.8192005271558999713, 0.8475185168785001055, 0.8758365066010999067, 0.9041544963236000099, 0.9324724860462000331, 0.9607904757688000563, 0.9891084654913000485, 1.017426455213999992 ),
 .UNSPECIFIED. ) ;
#341 = ORIENTED_EDGE ( 'NONE', *, *, #14163, .T. ) ;
#342 = CARTESIAN_POINT ( 'NONE',  ( 1.349879140156000190, -82.67445575724998719, -0.5781647238538999423 ) ) ;
#343 = CARTESIAN_POINT ( 'NONE',  ( -9.500000000000000000, -77.79999999999999716, 0.000000000000000000 ) ) ;
#344 = FACE_OUTER_BOUND ( 'NONE', #38978, .T. ) ;
#345 = CARTESIAN_POINT ( 'NONE',  ( -1.217465845835396188, -78.97916666666668561, 0.3271848554490955907 ) ) ;
#346 = CARTESIAN_POINT ( 'NONE',  ( 8.913108430814103755, -77.00000000000000000, -3.200251741501357383 ) ) ;
#347 = LINE ( 'NONE', #54049, #11944 ) ;
#348 = CARTESIAN_POINT ( 'NONE',  ( 1.899930039692999895, -78.42929805011500832, 9.535935523283001203 ) ) ;
#349 = CARTESIAN_POINT ( 'NONE',  ( -7.229693382246000333, -78.82924743682598034, -6.526195624661000672 ) ) ;
#350 = CARTESIAN_POINT ( 'NONE',  ( 8.381754473445653275, -76.01120442237058228, 8.234170154212950621 ) ) ;
#351 = CARTESIAN_POINT ( 'NONE',  ( -1.612912635236000147, -78.84554001676799828, 10.91330597072999886 ) ) ;
#352 = CARTESIAN_POINT ( 'NONE',  ( 3.647699722740942452, -86.02148118236289065, -1.624060551956035381 ) ) ;
#353 = VERTEX_POINT ( 'NONE', #51103 ) ;
#354 = AXIS2_PLACEMENT_3D ( 'NONE', #7083, #38659, #33359 ) ;
#355 = CARTESIAN_POINT ( 'NONE',  ( -7.450482419345999752, -76.12327025406412417, -9.799277032148999922 ) ) ;
#356 = EDGE_CURVE ( 'NONE', #56848, #20424, #2309, .T. ) ;
#357 = CARTESIAN_POINT ( 'NONE',  ( 3.485499217011998940, -78.48547957940618858, -2.057048905967550745 ) ) ;
#358 = CARTESIAN_POINT ( 'NONE',  ( -9.091539081997000338, -78.88283009111098920, 6.148815634104000338 ) ) ;
#359 = DIRECTION ( 'NONE',  ( 0.000000000000000000, 1.000000000000000000, 0.000000000000000000 ) ) ;
#360 = CARTESIAN_POINT ( 'NONE',  ( -3.140974612311405512, -77.79583333333334849, 11.68767212001977640 ) ) ;
#361 = CARTESIAN_POINT ( 'NONE',  ( -0.5999999999999999778, -5.200000000000000178, 0.5999999999999999778 ) ) ;
#362 = CARTESIAN_POINT ( 'NONE',  ( -0.2019459281704069076, -77.99218750000888178, 1.256926119276726483 ) ) ;
#363 = ORIENTED_EDGE ( 'NONE', *, *, #29731, .T. ) ;
#364 = CARTESIAN_POINT ( 'NONE',  ( -9.018305195942000196, -79.72548445825199792, 6.745675351750000104 ) ) ;
#365 = CARTESIAN_POINT ( 'NONE',  ( 12.74331394907039261, -55.27353206544193398, 1.980611464663725618 ) ) ;
#366 = CARTESIAN_POINT ( 'NONE',  ( 2.782842193290164801, -75.80000000000001137, -11.52882899609856082 ) ) ;
#367 = CARTESIAN_POINT ( 'NONE',  ( -2.309340847114626616, -78.43735716284257364, 3.830055409267042688 ) ) ;
#368 = CARTESIAN_POINT ( 'NONE',  ( -0.5212558242701900157, -81.50950461384270795, 1.136067814103569606 ) ) ;
#369 = CARTESIAN_POINT ( 'NONE',  ( -7.138937464960999790, -79.17331078153999613, 8.574798629027000629 ) ) ;
#370 = CYLINDRICAL_SURFACE ( 'NONE', #8132, 1.250000000000000000 ) ;
#371 = CARTESIAN_POINT ( 'NONE',  ( -0.9788204679455345669, -81.78049098935534289, 1.151159408688467778 ) ) ;
#372 = EDGE_CURVE ( 'NONE', #4267, #17174, #51583, .T. ) ;
#373 = DIRECTION ( 'NONE',  ( 1.000000000000000000, 0.000000000000000000, 0.000000000000000000 ) ) ;
#374 = CARTESIAN_POINT ( 'NONE',  ( -5.413904038987206846, -78.41666666666665719, 9.393203674808249914 ) ) ;
#375 = VECTOR ( 'NONE', #25081, 1000.000000000000000 ) ;
#376 =( LENGTH_UNIT ( ) NAMED_UNIT ( * ) SI_UNIT ( .MILLI., .METRE. ) );
#377 = DIRECTION ( 'NONE',  ( 0.000000000000000000, -1.000000000000000000, 0.000000000000000000 ) ) ;
#378 = VERTEX_POINT ( 'NONE', #14185 ) ;
#379 = EDGE_LOOP ( 'NONE', ( #35458, #39042, #39899, #1106 ) ) ;
#380 = DIRECTION ( 'NONE',  ( 0.000000000000000000, -1.000000000000000000, 0.000000000000000000 ) ) ;
#381 = CARTESIAN_POINT ( 'NONE',  ( -3.140974612311405512, -79.69583333333332575, 11.68767212001977640 ) ) ;
#382 = EDGE_LOOP ( 'NONE', ( #44129, #54601, #18071, #20029, #55022, #27124, #7591, #40469, #14418, #38243, #20068 ) ) ;
#383 = CARTESIAN_POINT ( 'NONE',  ( 8.628867348358941314, -76.05332450398152844, 6.837351357443815836 ) ) ;
#384 = ORIENTED_EDGE ( 'NONE', *, *, #55559, .T. ) ;
#385 = CARTESIAN_POINT ( 'NONE',  ( 7.620012114215000132, -23.20560398649000078, 10.53562503194000044 ) ) ;
#386 = AXIS2_PLACEMENT_3D ( 'NONE', #45632, #45042, #41184 ) ;
#387 = CARTESIAN_POINT ( 'NONE',  ( 11.00720109383000000, -77.39645716612599813, 0.7370606905150999255 ) ) ;
#388 = LINE ( 'NONE', #31625, #21184 ) ;
#389 = CARTESIAN_POINT ( 'NONE',  ( -3.218338554480999925, -78.22738998579799841, -9.136931980783000284 ) ) ;
#390 = CARTESIAN_POINT ( 'NONE',  ( -3.539318067648058452, -78.19389790816430263, -8.545993076014068990 ) ) ;
#391 = CARTESIAN_POINT ( 'NONE',  ( 1.099819419251000019, -79.63329055598900652, 11.16281809564999961 ) ) ;
#392 = CARTESIAN_POINT ( 'NONE',  ( 12.00000000000000000, -60.04999999966999980, 0.000000000000000000 ) ) ;
#393 = VERTEX_POINT ( 'NONE', #50514 ) ;
#394 = CARTESIAN_POINT ( 'NONE',  ( -9.848022987176388909, -24.82869493595770649, 8.114799025119214804 ) ) ;
#395 = EDGE_LOOP ( 'NONE', ( #41385, #43194, #13742, #37838 ) ) ;
#396 = CARTESIAN_POINT ( 'NONE',  ( 1.433348699817989180, -77.46263244500043754, 9.138269204909326149 ) ) ;
#397 = CARTESIAN_POINT ( 'NONE',  ( 7.528714304401000312, -78.05456459179299600, -8.074838600060001426 ) ) ;
#398 = DIRECTION ( 'NONE',  ( -0.7071067811865475727, 0.000000000000000000, 0.7071067811865475727 ) ) ;
#399 = CARTESIAN_POINT ( 'NONE',  ( 4.186942200393000135, -78.55095460635199345, -8.754440266352000677 ) ) ;
#400 = CARTESIAN_POINT ( 'NONE',  ( -9.898328264071000859, -75.97442085042999338, -8.374737995046999117 ) ) ;
#401 = CARTESIAN_POINT ( 'NONE',  ( -8.419758540101616617, -79.43829028770473144, -4.400681399932081739 ) ) ;
#402 = CARTESIAN_POINT ( 'NONE',  ( -0.9347040216968000026, -78.69407608247999519, 1.332288049216000081 ) ) ;
#403 = CARTESIAN_POINT ( 'NONE',  ( -8.838834764832000701, -60.04999999966999980, 8.838834764832000701 ) ) ;
#404 = CARTESIAN_POINT ( 'NONE',  ( -10.78159125964999987, -79.41561974942199242, 1.856099740267000087 ) ) ;
#405 = EDGE_CURVE ( 'NONE', #17140, #15196, #41355, .T. ) ;
#406 = CARTESIAN_POINT ( 'NONE',  ( -10.18114973714000016, -23.39009320411999937, -7.633087466104000463 ) ) ;
#407 = CARTESIAN_POINT ( 'NONE',  ( -11.49731019796060316, -76.68331092814908345, 2.423775870982253444 ) ) ;
#408 = CARTESIAN_POINT ( 'NONE',  ( 3.473823996146999882, -83.70093064074599454, -0.9034887262636999150 ) ) ;
#409 = VERTEX_POINT ( 'NONE', #50221 ) ;
#410 = EDGE_CURVE ( 'NONE', #18942, #44068, #5336, .T. ) ;
#411 = CARTESIAN_POINT ( 'NONE',  ( -12.01465389393999850, -78.95880199243299558, -2.711845028153999859 ) ) ;
#412 = CARTESIAN_POINT ( 'NONE',  ( -10.26547038271000112, -76.61176894222799660, 3.946724975948999958 ) ) ;
#413 = CARTESIAN_POINT ( 'NONE',  ( -6.822290318485905836, -78.02980255133013543, 8.307683877974495701 ) ) ;
#414 = CARTESIAN_POINT ( 'NONE',  ( 8.770451247185000909, -78.94352923869598726, 8.160602927202999624 ) ) ;
#415 = CARTESIAN_POINT ( 'NONE',  ( -0.8506806241676722058, -3.395833333333332593, 3.165411199172022627 ) ) ;
#417 = DIRECTION ( 'NONE',  ( 0.000000000000000000, -1.000000000000000000, 0.000000000000000000 ) ) ;
#416 = CARTESIAN_POINT ( 'NONE',  ( -11.44417895085270942, -78.32083333333335418, -3.075537641221545826 ) ) ;
#418 = DIRECTION ( 'NONE',  ( -6.735242868878000753E-11, 1.000000000000000000, 0.000000000000000000 ) ) ;
#419 = CARTESIAN_POINT ( 'NONE',  ( 6.307978547608708020, -80.92535043715515997, 8.704505370279399301 ) ) ;
#420 = CARTESIAN_POINT ( 'NONE',  ( -11.13667185325999931, -80.13800688576898779, -2.444338232200999439 ) ) ;
#421 = DIRECTION ( 'NONE',  ( -0.7071067811864976127, 0.7071067811865975328, -1.591673720108993631E-09 ) ) ;
#422 = CARTESIAN_POINT ( 'NONE',  ( -10.52129323452999898, -77.86434791014099233, 3.681981700656000278 ) ) ;
#423 = CARTESIAN_POINT ( 'NONE',  ( -3.250000000000002665, -1.989583333333334147, 0.4254240051736044581 ) ) ;
#424 = CARTESIAN_POINT ( 'NONE',  ( -11.00676540241999923, -80.45419303504098707, 0.6467430135644000044 ) ) ;
#425 = VERTEX_POINT ( 'NONE', #23343 ) ;
#426 = AXIS2_PLACEMENT_3D ( 'NONE', #17397, #35382, #53716 ) ;
#427 = CARTESIAN_POINT ( 'NONE',  ( 9.684822944874866835, -77.90969691107382289, -5.379607873393639217 ) ) ;
#428 = CARTESIAN_POINT ( 'NONE',  ( 0.7635722663974530144, -77.01859038055819440, 9.343284614800793975 ) ) ;
#429 = EDGE_CURVE ( 'NONE', #41458, #33230, #30416, .T. ) ;
#430 = CARTESIAN_POINT ( 'NONE',  ( -1.382299254417000078, -2.123118309747999977, 3.546132182520000065 ) ) ;
#431 = CARTESIAN_POINT ( 'NONE',  ( 9.070694317316998934, -77.99836472845399271, 6.598531290616000078 ) ) ;
#432 = CARTESIAN_POINT ( 'NONE',  ( -1.417334032777999964, -79.42654225787899236, -0.4910847579886000736 ) ) ;
#433 = CARTESIAN_POINT ( 'NONE',  ( -8.500000000000000000, -73.00000000000001421, 0.000000000000000000 ) ) ;
#434 = DIRECTION ( 'NONE',  ( 0.000000000000000000, -1.000000000000000000, 0.000000000000000000 ) ) ;
#435 = AXIS2_PLACEMENT_3D ( 'NONE', #56778, #6892, #24899 ) ;
#436 = CARTESIAN_POINT ( 'NONE',  ( -10.65295200446612967, -78.51231955895573833, -1.664190318615639042 ) ) ;
#437 = CARTESIAN_POINT ( 'NONE',  ( 12.57354471038000021, -18.27622323986999930, 1.757967544833999973 ) ) ;
#438 = CARTESIAN_POINT ( 'NONE',  ( -3.903103493260999812, -86.12136169985498668, 1.102340964906999954 ) ) ;
#439 = CARTESIAN_POINT ( 'NONE',  ( -4.801183948719927486, -76.05000000000001137, 10.79468190462868016 ) ) ;
#440 = CARTESIAN_POINT ( 'NONE',  ( 9.992014434659999722, -54.63915351680999777, -7.762970980286999279 ) ) ;
#441 = CARTESIAN_POINT ( 'NONE',  ( -3.610459473067000324, -77.11011177151499396, 10.54605058607999979 ) ) ;
#442 = CARTESIAN_POINT ( 'NONE',  ( 1.520902128651999918, -80.92772696789998577, -0.6797894616744000196 ) ) ;
#443 = CARTESIAN_POINT ( 'NONE',  ( 1.082149117140000172, -79.20679688847999955, 1.108446078784000033 ) ) ;
#444 = CARTESIAN_POINT ( 'NONE',  ( 7.559982449049000408, -77.02655527933319490, -6.032732969207000195 ) ) ;
#445 = CARTESIAN_POINT ( 'NONE',  ( 0.01073940206318611812, -82.87549824373742524, -1.509945108508129907 ) ) ;
#446 = CARTESIAN_POINT ( 'NONE',  ( -12.43410103870000150, -61.24137177736000126, 1.192638008239000014 ) ) ;
#447 = CARTESIAN_POINT ( 'NONE',  ( -7.579570500035162972, -80.16319179611589618, -7.622759937838323729 ) ) ;
#448 = DIRECTION ( 'NONE',  ( 0.000000000000000000, -1.000000000000000000, 0.000000000000000000 ) ) ;
#449 = CARTESIAN_POINT ( 'NONE',  ( -0.3527936601020746354, -78.04753704632268807, 1.224052721373980690 ) ) ;
#450 = CARTESIAN_POINT ( 'NONE',  ( 0.8593825103163911239, -81.78595333969393266, -0.9078339653130700349 ) ) ;
#451 = DIRECTION ( 'NONE',  ( 0.000000000000000000, 1.000000000000000000, 0.000000000000000000 ) ) ;
#452 = CARTESIAN_POINT ( 'NONE',  ( 0.9518616847512999524, -79.02294003937198852, -11.10623968335000100 ) ) ;
#453 = CIRCLE ( 'NONE', #45692, 1.750000000000001332 ) ;
#454 = FACE_OUTER_BOUND ( 'NONE', #42226, .T. ) ;
#455 = ORIENTED_EDGE ( 'NONE', *, *, #16747, .F. ) ;
#456 = VERTEX_POINT ( 'NONE', #36913 ) ;
#457 = CARTESIAN_POINT ( 'NONE',  ( 0.8888964087114000767, -80.66333400915199547, -1.347979478730999991 ) ) ;
#458 = ORIENTED_EDGE ( 'NONE', *, *, #10797, .T. ) ;
#460 = EDGE_CURVE ( 'NONE', #4894, #43600, #23630, .T. ) ;
#459 = EDGE_LOOP ( 'NONE', ( #6292, #27187, #8033, #17546, #22644, #44404 ) ) ;
#461 = CARTESIAN_POINT ( 'NONE',  ( -2.062312494845999655, -18.77284340107000205, 12.83634740209000036 ) ) ;
#462 = CARTESIAN_POINT ( 'NONE',  ( -12.50000000000000000, -60.04999999966999980, 0.000000000000000000 ) ) ;
#463 = ADVANCED_BREP_SHAPE_REPRESENTATION ( '', ( #16630, #43526 ), #6767 ) ;
#464 = CARTESIAN_POINT ( 'NONE',  ( -0.3695879074652637097, -80.54999998998307831, -3.516391212123742616 ) ) ;
#465 = CONICAL_SURFACE ( 'NONE', #46690, 11.09999999881999955, 0.7853981633972997312 ) ;
#466 = CARTESIAN_POINT ( 'NONE',  ( 0.7977265213099999919, -81.45982051858098316, 3.499625350527999945 ) ) ;
#467 = DIRECTION ( 'NONE',  ( 0.000000000000000000, 1.000000000000000000, 0.000000000000000000 ) ) ;
#468 = CARTESIAN_POINT ( 'NONE',  ( -9.088900789933001434, -78.68843598616000179, 7.702160993204000050 ) ) ;
#469 = VERTEX_POINT ( 'NONE', #14763 ) ;
#470 = VERTEX_POINT ( 'NONE', #32760 ) ;
#471 = CARTESIAN_POINT ( 'NONE',  ( 0.000000000000000000, -32.88214388149999934, 0.000000000000000000 ) ) ;
#472 = CARTESIAN_POINT ( 'NONE',  ( 10.75000000000000000, -78.25000000000000000, 1.005550720961999908E-14 ) ) ;
#473 = CARTESIAN_POINT ( 'NONE',  ( -1.154258600661999923, -79.76363727870300124, -0.6680293646364998672 ) ) ;
#474 = CARTESIAN_POINT ( 'NONE',  ( -1.959694873104000257, -77.31836415156699616, -9.504225410855001499 ) ) ;
#475 = CARTESIAN_POINT ( 'NONE',  ( 3.620209227049934420, -86.25171438276198899, -1.611820994701147480 ) ) ;
#476 = CARTESIAN_POINT ( 'NONE',  ( -10.59551070215999857, -20.24351820077000141, 7.678690995240000206 ) ) ;
#477 = CARTESIAN_POINT ( 'NONE',  ( -9.134707332315000983, -77.39321223492000001, -8.964724163292999037 ) ) ;
#478 = CARTESIAN_POINT ( 'NONE',  ( -0.5035993198763999423, -79.23880658815998856, -1.271638408173999979 ) ) ;
#479 = CARTESIAN_POINT ( 'NONE',  ( -12.56594317823000040, -23.25000001387000026, 1.750000000000000000 ) ) ;
#480 = CARTESIAN_POINT ( 'NONE',  ( 12.56594317825999951, -60.05000001354000005, -1.750000000000000000 ) ) ;
#481 = EDGE_CURVE ( 'NONE', #23446, #29038, #48572, .T. ) ;
#482 = CARTESIAN_POINT ( 'NONE',  ( 1.620852308002999953, -80.65768892718899963, -3.844855067022000306 ) ) ;
#483 = CARTESIAN_POINT ( 'NONE',  ( 9.755626371838998168, -80.97443200427989041, -5.633583086437000453 ) ) ;
#484 = CARTESIAN_POINT ( 'NONE',  ( 12.65375411752000012, -20.25022861081000158, 1.750000000000000000 ) ) ;
#485 = CARTESIAN_POINT ( 'NONE',  ( -10.66325342011819188, -78.26486258876667534, 5.043235781625580394 ) ) ;
#486 = CARTESIAN_POINT ( 'NONE',  ( -3.412705351263000342, -78.68490379462421913, 0.4935355394736000156 ) ) ;
#487 = CARTESIAN_POINT ( 'NONE',  ( 0.2086861075963999945, -78.58438338449100513, 1.317203954600000060 ) ) ;
#488 = FACE_BOUND ( 'NONE', #45895, .T. ) ;
#489 = CARTESIAN_POINT ( 'NONE',  ( 7.551392188974999975, -80.21711109272469287, 8.117862728809001283 ) ) ;
#490 = CARTESIAN_POINT ( 'NONE',  ( -0.3113020967593000399, -2.733516015699999802, 3.793306396812999637 ) ) ;
#491 = CARTESIAN_POINT ( 'NONE',  ( 10.25292700656883760, -77.20000000000000284, -3.413936412999044823 ) ) ;
#492 = ORIENTED_EDGE ( 'NONE', *, *, #5295, .T. ) ;
#493 = CARTESIAN_POINT ( 'NONE',  ( -10.75000000000000000, -80.00000000000000000, 0.000000000000000000 ) ) ;
#494 = CARTESIAN_POINT ( 'NONE',  ( 1.569236785184999737E-14, 0.000000000000000000, 0.000000000000000000 ) ) ;
#495 = LINE ( 'NONE', #35880, #7209 ) ;
#496 = VECTOR ( 'NONE', #9749, 1000.000000000000114 ) ;
#497 = EDGE_CURVE ( 'NONE', #24745, #8613, #21219, .T. ) ;
#498 = FACE_OUTER_BOUND ( 'NONE', #54806, .T. ) ;
#500 = EDGE_CURVE ( 'NONE', #21107, #21244, #3663, .T. ) ;
#499 = CARTESIAN_POINT ( 'NONE',  ( 3.414307247564000392, -79.67572032229998058, 9.134133468150000823 ) ) ;
#501 = CARTESIAN_POINT ( 'NONE',  ( 12.55073801092999908, -77.24605814734000830, -3.437763296274999991 ) ) ;
#502 = CARTESIAN_POINT ( 'NONE',  ( -6.340838181001343443, -79.52523374718921900, 8.680779125499762827 ) ) ;
#503 = CARTESIAN_POINT ( 'NONE',  ( -8.717770243732999802, -79.47198667140099815, 4.088898379276000306 ) ) ;
#504 = DIRECTION ( 'NONE',  ( 0.000000000000000000, 1.000000000000000000, 0.000000000000000000 ) ) ;
#505 = ORIENTED_EDGE ( 'NONE', *, *, #666, .F. ) ;
#506 = VECTOR ( 'NONE', #47712, 1000.000000000000000 ) ;
#507 = FACE_OUTER_BOUND ( 'NONE', #47869, .T. ) ;
#508 = CARTESIAN_POINT ( 'NONE',  ( -0.8958779135676999683, -82.17683127161700440, 0.9567003624791000638 ) ) ;
#509 = CARTESIAN_POINT ( 'NONE',  ( 7.705119999441000012, -20.24828923609000242, -10.24996238031000040 ) ) ;
#510 = CARTESIAN_POINT ( 'NONE',  ( 1.825776387079000029, -78.88028063292298953, 9.234594473601999809 ) ) ;
#512 = CARTESIAN_POINT ( 'NONE',  ( -1.488596180559999871, -0.8774472721615999005, -3.730054860412999940 ) ) ;
#511 = CARTESIAN_POINT ( 'NONE',  ( 3.297963199104999799, -82.02128429901999596, -1.885709654497000010 ) ) ;
#513 = CARTESIAN_POINT ( 'NONE',  ( -0.7681833999686477066, -82.42708333333332860, 0.9995835529977223910 ) ) ;
#514 = CARTESIAN_POINT ( 'NONE',  ( -0.4820197951951999960, -79.25329419107600870, -1.228125725326999929 ) ) ;
#515 = VERTEX_POINT ( 'NONE', #57244 ) ;
#516 = CARTESIAN_POINT ( 'NONE',  ( 0.01050698433460529012, -77.22515890467916222, -10.74994752102681339 ) ) ;
#517 = FACE_OUTER_BOUND ( 'NONE', #48566, .T. ) ;
#518 = PRODUCT_DEFINITION ( 'UNKNOWN', '', #41419, #21544 ) ;
#519 = CARTESIAN_POINT ( 'NONE',  ( -3.992904449609034678, -78.77851881763731967, 7.985808899218018730 ) ) ;
#520 = ORIENTED_EDGE ( 'NONE', *, *, #57168, .F. ) ;
#521 = VERTEX_POINT ( 'NONE', #12372 ) ;
#522 = CARTESIAN_POINT ( 'NONE',  ( -10.75843888410000027, -79.38533932610398836, -1.985902594052000092 ) ) ;
#523 = DIRECTION ( 'NONE',  ( 0.000000000000000000, 1.000000000000000000, 0.000000000000000000 ) ) ;
#524 = CARTESIAN_POINT ( 'NONE',  ( 6.436424241555000592, -80.32391735373440156, 8.610165096135999008 ) ) ;
#525 = VERTEX_POINT ( 'NONE', #2664 ) ;
#526 = CARTESIAN_POINT ( 'NONE',  ( 11.27339212957999948, -77.96985744374799765, 4.255161755617000274 ) ) ;
#527 = ORIENTED_EDGE ( 'NONE', *, *, #54959, .T. ) ;
#529 = ADVANCED_FACE ( 'NONE', ( #2091 ), #20293, .T. ) ;
#528 = EDGE_LOOP ( 'NONE', ( #13546, #35244, #44133, #4500 ) ) ;
#530 = CARTESIAN_POINT ( 'NONE',  ( -0.4127567104095349881, -2.716300734224319946, -3.229589481510274585 ) ) ;
#531 = EDGE_CURVE ( 'NONE', #49275, #46028, #19327, .T. ) ;
#532 = CARTESIAN_POINT ( 'NONE',  ( -1.750000000000000000, -18.75000000310999937, -12.50000000000000000 ) ) ;
#533 = FACE_OUTER_BOUND ( 'NONE', #5641, .T. ) ;
#534 = CIRCLE ( 'NONE', #25023, 12.09999999999999964 ) ;
#535 = ORIENTED_EDGE ( 'NONE', *, *, #50020, .F. ) ;
#536 = DIRECTION ( 'NONE',  ( 0.000000000000000000, 0.7071067811866525998, -0.7071067811864425456 ) ) ;
#537 = EDGE_LOOP ( 'NONE', ( #15741, #44098, #34888 ) ) ;
#538 = CARTESIAN_POINT ( 'NONE',  ( -0.1647286073852369803, -79.76489708643704546, -1.263362412047110306 ) ) ;
#539 = CIRCLE ( 'NONE', #2291, 14.00000000000000000 ) ;
#540 = CARTESIAN_POINT ( 'NONE',  ( 3.999999999999675815, -78.69999999999997442, -1.477225460011499791E-15 ) ) ;
#541 = CARTESIAN_POINT ( 'NONE',  ( 0.000000000000000000, -74.99999999999998579, 0.000000000000000000 ) ) ;
#542 = VECTOR ( 'NONE', #54840, 1000.000000000000114 ) ;
#543 = CARTESIAN_POINT ( 'NONE',  ( -11.08400893143999966, -76.20894737471998326, -1.489506537590000068 ) ) ;
#544 = CARTESIAN_POINT ( 'NONE',  ( 0.000000000000000000, -15.89905023022000030, 0.000000000000000000 ) ) ;
#545 = CARTESIAN_POINT ( 'NONE',  ( 14.00000000000000000, -46.09579702914000165, 0.000000000000000000 ) ) ;
#546 = CARTESIAN_POINT ( 'NONE',  ( -11.92766985523999956, -77.65742819841213418, -1.116582401450000095 ) ) ;
#547 = CARTESIAN_POINT ( 'NONE',  ( -1.374291557126987362, -78.71317509820548253, -9.148177845238967265 ) ) ;
#548 = CARTESIAN_POINT ( 'NONE',  ( -6.660059710594288696, -76.92432036743132073, -9.025807911732075084 ) ) ;
#549 = CARTESIAN_POINT ( 'NONE',  ( -6.920864301812000186, -77.01268501420199186, 6.182201926393999791 ) ) ;
#550 = CARTESIAN_POINT ( 'NONE',  ( -13.94241847916999966, -9.539970597795999652, -4.312626734363999664E-05 ) ) ;
#551 = CARTESIAN_POINT ( 'NONE',  ( 1.323534079420999987, -79.87453973706999477, -0.1638099207045999872 ) ) ;
#552 = CARTESIAN_POINT ( 'NONE',  ( -9.250401410528953150, -77.61051319238347901, -1.210813435511432834 ) ) ;
#553 = CARTESIAN_POINT ( 'NONE',  ( 10.26699006316251683, -76.59166666666665435, 5.917523019358090330 ) ) ;
#554 = CARTESIAN_POINT ( 'NONE',  ( -2.970001969328999625, -81.56803455456798702, -2.623941025421000273 ) ) ;
#555 = DIRECTION ( 'NONE',  ( 0.000000000000000000, -1.000000000000000000, 0.000000000000000000 ) ) ;
#556 = LINE ( 'NONE', #14374, #7797 ) ;
#557 = LINE ( 'NONE', #55415, #9432 ) ;
#558 = CARTESIAN_POINT ( 'NONE',  ( -0.5506765233277000071, -25.25954292244000143, 12.77514798311000099 ) ) ;
#559 = CARTESIAN_POINT ( 'NONE',  ( -1.250002149560441644, -82.24413779550083348, 0.09476315643046410997 ) ) ;
#560 = CARTESIAN_POINT ( 'NONE',  ( 2.902193781656972504, -80.00000000000000000, 8.901354151454830443 ) ) ;
#561 = CARTESIAN_POINT ( 'NONE',  ( -2.851845075913000294, -2.090913946620000186, -1.354809779547999860 ) ) ;
#562 = CARTESIAN_POINT ( 'NONE',  ( -0.2428088493965334382, -78.22329368912637904, -10.77973457647781785 ) ) ;
#563 = EDGE_CURVE ( 'NONE', #20195, #7399, #29212, .T. ) ;
#564 = CARTESIAN_POINT ( 'NONE',  ( 0.7999999999999001243, -18.84999999997999964, 12.00000000000000000 ) ) ;
#565 = CARTESIAN_POINT ( 'NONE',  ( -1.511461402894981321, -79.84725243224966107, 0.03864653979242833881 ) ) ;
#566 = CARTESIAN_POINT ( 'NONE',  ( 7.686941364964000378, -58.55472017773000459, -10.48774103561000182 ) ) ;
#567 = CARTESIAN_POINT ( 'NONE',  ( -3.465920916155000420, -3.052832871923000013, -0.3696040369545000037 ) ) ;
#568 = EDGE_CURVE ( 'NONE', #9279, #11445, #48735, .T. ) ;
#569 = CARTESIAN_POINT ( 'NONE',  ( 1.764045786578000152, -77.01006991430598703, -11.99279291753999921 ) ) ;
#570 = CARTESIAN_POINT ( 'NONE',  ( -8.485281374238999419, -23.25000000000000000, -8.485281374238999419 ) ) ;
#572 = CARTESIAN_POINT ( 'NONE',  ( 0.6680689699263999692, -78.46136003831350081, -1.250497193771000104 ) ) ;
#571 = CARTESIAN_POINT ( 'NONE',  ( 0.000000000000000000, -18.75000000000000000, -12.00000000000000000 ) ) ;
#573 = CARTESIAN_POINT ( 'NONE',  ( -0.5918520097389999846, -82.86672773667999081, -1.596724312065999962 ) ) ;
#574 = ORIENTED_EDGE ( 'NONE', *, *, #53036, .T. ) ;
#575 = B_SPLINE_SURFACE_WITH_KNOTS ( 'NONE', 3, 3, ( 
 ( #12579, #9256, #48608, #54128, #29991, #34424, #52454, #57162, #48044, #8155, #7577, #25576, #21148, #39156, #26155, #46752, #46163, #1286, #33424, #51461, #37270, #11015, #28406, #50289, #28112, #9843, #10723, #36691, #23698, #15430, #1871, #41125, #19565, #36981, #27823, #50582, #28999, #41711, #18989, #45869, #28701, #19280, #54994, #47039, #33127, #19865, #5688, #1004, #6271, #24287, #10136, #23410, #6569, #55285, #42304, #14833, #37859, #55880, #719, #18697, #37566, #14543, #51169, #54706, #14250, #32536, #32830 ),
 ( #50875, #10421, #32246, #46453, #5402, #23988, #5981, #42004, #1572, #41421, #55581, #15129, #56458, #34575, #29282, #39020, #12159, #52608, #20445, #20159, #21300, #11301, #39308, #34863, #48195, #11594, #57318, #2158, #43753, #38441, #47910, #38148, #16012, #25728, #21014, #12443, #25441, #52893, #29855, #34001, #52037, #15718, #43460, #47331, #42886, #34289, #56748, #42596, #2732, #7149, #29570, #20731, #57032, #33714, #47626, #25151, #52323, #6860, #30438, #38729, #7442, #43177, #48469, #11877, #16308, #3017, #16591 ),
 ( #30145, #7727, #3306, #16882, #24580, #56170, #51751, #24868, #2443, #13596, #18336, #36328, #4752, #39595, #49044, #30719, #31886, #48754, #44315, #44035, #40764, #8301, #40472, #8590, #4460, #45204, #54353, #66, #358, #54060, #57892, #53767, #13892, #3871, #22754, #22460, #26578, #31593, #36036, #9182, #21871, #17448, #13006, #8012, #44905, #35736, #44612, #4167, #53464, #22165, #13303, #26009, #49635, #12726, #27167, #3585, #49340, #21588, #40172, #57598, #26301, #17159, #35145, #53176, #39879, #35435, #31006 ),
 ( #58185, #17748, #31296, #8886, #26881, #18044, #32756, #41932, #10348, #1217, #23914, #27461, #41637, #50509, #55510, #46676, #28331, #46381, #6199, #5905, #45796, #1503, #18630, #28042, #24212, #45499, #5331, #5614, #1795, #14179, #42231, #19493, #37199, #14758, #50803, #37488, #19208, #55212, #645, #51098, #15057, #33051, #10649, #28629, #19792, #46088, #37786, #23625, #54641, #36907, #55806, #15358, #49930, #9475, #23044, #32463, #32176, #5046, #50216, #27752, #41059, #36622, #9764, #23338, #10062, #41350, #932 ) ),
 .UNSPECIFIED., .F., .F., .F.,
 ( 4, 4 ),
 ( 4, 1, 1, 1, 1, 1, 1, 1, 1, 1, 1, 1, 1, 1, 1, 1, 1, 1, 1, 1, 1, 1, 1, 1, 1, 1, 1, 1, 1, 1, 1, 1, 1, 1, 1, 1, 1, 1, 1, 1, 1, 1, 1, 1, 1, 1, 1, 1, 1, 1, 1, 1, 1, 1, 1, 1, 1, 1, 1, 1, 1, 1, 1, 1, 4 ),
 ( -0.4045438850611000059, 1.404543885061000141 ),
 ( -0.02000000000000000042, -0.003749999999999999861, 0.01250000000000000069, 0.02875000000000000125, 0.04499999999999999833, 0.06124999999999999889, 0.07749999999999999944, 0.09375000000000000000, 0.1100000000000000006, 0.1262500000000000011, 0.1424999999999999878, 0.1587500000000000022, 0.1749999999999999889, 0.1912500000000000033, 0.2074999999999999900, 0.2237500000000000044, 0.2399999999999999911, 0.2562499999999999778, 0.2725000000000000200, 0.2887500000000000067, 0.3049999999999999933, 0.3212499999999999800, 0.3375000000000000222, 0.3537500000000000089, 0.3699999999999999956, 0.3862499999999999822, 0.4025000000000000244, 0.4187500000000000111, 0.4349999999999999978, 0.4512499999999999845, 0.4675000000000000266, 0.4837500000000000133, 0.5000000000000000000, 0.5162499999999999867, 0.5324999999999999734, 0.5487499999999999600, 0.5649999999999999467, 0.5812500000000000444, 0.5975000000000000311, 0.6137500000000000178, 0.6300000000000000044, 0.6462499999999999911, 0.6624999999999999778, 0.6787499999999999645, 0.6949999999999999512, 0.7112500000000000488, 0.7275000000000000355, 0.7437500000000000222, 0.7600000000000000089, 0.7762499999999999956, 0.7924999999999999822, 0.8087499999999999689, 0.8249999999999999556, 0.8412500000000000533, 0.8575000000000000400, 0.8737500000000000266, 0.8900000000000000133, 0.9062500000000000000, 0.9224999999999999867, 0.9387499999999999734, 0.9549999999999999600, 0.9712499999999999467, 0.9875000000000000444, 1.003749999999999920, 1.020000000000000018 ),
 .UNSPECIFIED. ) ;
#576 = CARTESIAN_POINT ( 'NONE',  ( 3.640440263105999552, -84.31421544543098889, 0.9265833904223998996 ) ) ;
#577 = AXIS2_PLACEMENT_3D ( 'NONE', #17957, #12922, #35948 ) ;
#578 = CARTESIAN_POINT ( 'NONE',  ( -7.249076177254000442, -80.50531345225510904, 8.347662706485998285 ) ) ;
#579 = CARTESIAN_POINT ( 'NONE',  ( -9.599999999999999645, -90.39999999999999147, 0.000000000000000000 ) ) ;
#580 = CARTESIAN_POINT ( 'NONE',  ( 1.992291055985653481, -85.67604167370414814, 2.768826960839078311 ) ) ;
#581 = CYLINDRICAL_SURFACE ( 'NONE', #57781, 12.00000000000000000 ) ;
#582 = CARTESIAN_POINT ( 'NONE',  ( -8.623695280723000067, -78.29071980276798115, 4.526762133323999571 ) ) ;
#583 = CARTESIAN_POINT ( 'NONE',  ( -12.59654320151999940, -77.26232752475000609, -1.064070293361000008 ) ) ;
#584 = CARTESIAN_POINT ( 'NONE',  ( 5.916979755548000597, -79.44684362032798219, -7.926218594775000348 ) ) ;
#585 = CARTESIAN_POINT ( 'NONE',  ( -8.441176280277392863, -61.71652561705167983, 9.243148036170415693 ) ) ;
#586 = DIRECTION ( 'NONE',  ( 0.000000000000000000, -1.000000000000000000, 0.000000000000000000 ) ) ;
#587 = VERTEX_POINT ( 'NONE', #21516 ) ;
#588 = AXIS2_PLACEMENT_3D ( 'NONE', #42436, #2004, #24713 ) ;
#589 = CARTESIAN_POINT ( 'NONE',  ( -0.9870767835202884921, -80.56949413944577998, -1.171048524979026340 ) ) ;
#590 = DIRECTION ( 'NONE',  ( 0.7071067811865969777, 1.533578360404995178E-11, 0.7071067811864980568 ) ) ;
#591 = ADVANCED_FACE ( 'NONE', ( #7938 ), #54289, .F. ) ;
#592 = DIRECTION ( 'NONE',  ( -1.000000000000000000, 0.000000000000000000, 0.000000000000000000 ) ) ;
#593 = CARTESIAN_POINT ( 'NONE',  ( 0.6849175148897999055, -77.80225862199890230, -1.144319635748999975 ) ) ;
#594 = CARTESIAN_POINT ( 'NONE',  ( -12.53239398061000109, -59.56486430393999854, -1.667936688463999895 ) ) ;
#595 = ORIENTED_EDGE ( 'NONE', *, *, #38393, .T. ) ;
#596 = CARTESIAN_POINT ( 'NONE',  ( -7.370930946996000266, -78.06097405823999225, -8.448440252239999282 ) ) ;
#597 = CARTESIAN_POINT ( 'NONE',  ( -12.70556836347999941, -25.22772277227999993, -2.424223956931999920E-09 ) ) ;
#598 = EDGE_LOOP ( 'NONE', ( #27192, #166, #40123, #43861 ) ) ;
#599 = ORIENTED_EDGE ( 'NONE', *, *, #4461, .F. ) ;
#600 = CARTESIAN_POINT ( 'NONE',  ( -10.53495272788000214, -55.57289072595000334, -7.618387390351999855 ) ) ;
#601 = ADVANCED_FACE ( 'NONE', ( #35967 ), #30933, .T. ) ;
#602 =( LENGTH_UNIT ( ) NAMED_UNIT ( * ) SI_UNIT ( .MILLI., .METRE. ) );
#603 = CARTESIAN_POINT ( 'NONE',  ( -4.465297566879000257, -79.92309116543150083, 8.686876450551999085 ) ) ;
#604 = VERTEX_POINT ( 'NONE', #30650 ) ;
#605 = DIRECTION ( 'NONE',  ( -1.000000000000000000, 0.000000000000000000, 0.000000000000000000 ) ) ;
#606 = DIRECTION ( 'NONE',  ( 1.000000000000000000, 0.000000000000000000, 0.000000000000000000 ) ) ;
#607 = CARTESIAN_POINT ( 'NONE',  ( -1.485771955761999941, -77.72682433276000324, -0.3846555688014000052 ) ) ;
#608 = ORIENTED_EDGE ( 'NONE', *, *, #33338, .F. ) ;
#609 = CARTESIAN_POINT ( 'NONE',  ( 8.256620083228000340, -77.33895194988498645, -4.688888258373000717 ) ) ;
#610 = CARTESIAN_POINT ( 'NONE',  ( -10.75000000000000000, -76.50000000000000000, 0.000000000000000000 ) ) ;
#611 = CARTESIAN_POINT ( 'NONE',  ( 0.8048611780553004413, -80.28119307227865420, -0.9591988868156666737 ) ) ;
#612 = CARTESIAN_POINT ( 'NONE',  ( -13.06702859930000038, -77.00108497556999509, -1.103813699724999875 ) ) ;
#613 = LINE ( 'NONE', #54606, #57976 ) ;
#614 = CARTESIAN_POINT ( 'NONE',  ( 7.027773501905277165, -79.90642805933067905, 6.014294227121073533 ) ) ;
#615 = CARTESIAN_POINT ( 'NONE',  ( -1.232226823824171147, -24.52290911267661144, 12.50408896749710053 ) ) ;
#616 = VERTEX_POINT ( 'NONE', #44246 ) ;
#617 = CARTESIAN_POINT ( 'NONE',  ( 2.632967082928999947, -77.10305996719816335, 9.306700570505000769 ) ) ;
#618 = CARTESIAN_POINT ( 'NONE',  ( -12.22985280536000019, -76.56108432191999214, -1.402219185755000153 ) ) ;
#619 = CARTESIAN_POINT ( 'NONE',  ( -0.5539667471886999817, -79.44792250334801054, -1.411437496924000001 ) ) ;
#620 = CIRCLE ( 'NONE', #30735, 0.5000000000000000000 ) ;
#621 = CARTESIAN_POINT ( 'NONE',  ( 0.9174690372081734102, -2.203321940176160343, 3.400067753488194011 ) ) ;
#622 = CARTESIAN_POINT ( 'NONE',  ( 12.60552522436000089, -18.71082434677000350, 1.799501877760999902 ) ) ;
#623 = CARTESIAN_POINT ( 'NONE',  ( -11.55418265775999842, -78.99013131216000261, 4.110954701505000308 ) ) ;
#624 = CARTESIAN_POINT ( 'NONE',  ( 2.548493721447000038, -77.06004840258400179, 12.01365081398999912 ) ) ;
#625 = DIRECTION ( 'NONE',  ( -0.8320502943378438321, -0.5547001962252288143, -2.960716109815154402E-12 ) ) ;
#626 = AXIS2_PLACEMENT_3D ( 'NONE', #27825, #9845, #41713 ) ;
#627 = CARTESIAN_POINT ( 'NONE',  ( 9.014599915542000019, -77.66018998579799870, 3.680982378367999797 ) ) ;
#628 = CARTESIAN_POINT ( 'NONE',  ( 1.347303718401573480, -77.41606322048822619, 11.98951635918131764 ) ) ;
#629 = CARTESIAN_POINT ( 'NONE',  ( -9.971217743844798420, -75.89688248555343364, 8.384385000145641698 ) ) ;
#630 = MECHANICAL_DESIGN_GEOMETRIC_PRESENTATION_REPRESENTATION (  '', ( #12843 ), #25113 ) ;
#631 = ORIENTED_EDGE ( 'NONE', *, *, #11984, .F. ) ;
#632 = CARTESIAN_POINT ( 'NONE',  ( 0.6959559787155999988, -82.23218377781998356, 1.424795421937999906 ) ) ;
#633 = CARTESIAN_POINT ( 'NONE',  ( 8.838834764832000701, -18.75000000000000000, 8.838834764832000701 ) ) ;
#634 = CARTESIAN_POINT ( 'NONE',  ( -0.1636246173744726473, -79.38541666666664298, 1.249999999999999112 ) ) ;
#635 = CARTESIAN_POINT ( 'NONE',  ( 11.20799393363000007, -77.77703814603999888, 4.230477091134000389 ) ) ;
#636 = CARTESIAN_POINT ( 'NONE',  ( 9.443547551318811628, -77.00000000000000000, 0.1845321678459553028 ) ) ;
#637 = CARTESIAN_POINT ( 'NONE',  ( 4.928445265185000146, -78.16739492409399759, -10.99573548889999941 ) ) ;
#638 = CARTESIAN_POINT ( 'NONE',  ( -9.375068251199000002, -78.22531894259199703, -2.204836785425999590 ) ) ;
#639 = CARTESIAN_POINT ( 'NONE',  ( 0.007133794492888097249, -76.07462582236088622, 11.74977943346025455 ) ) ;
#640 = CARTESIAN_POINT ( 'NONE',  ( -10.57985553746999940, -78.98172173177698596, -3.125442558719000008 ) ) ;
#641 = CARTESIAN_POINT ( 'NONE',  ( -0.4871519710315541096, -86.07390000031791999, 3.917790784211977240 ) ) ;
#642 = ORIENTED_EDGE ( 'NONE', *, *, #17291, .F. ) ;
#643 = CARTESIAN_POINT ( 'NONE',  ( 6.099999999940000528, -80.79999999975800051, 5.338249915816000005E-09 ) ) ;
#644 = CARTESIAN_POINT ( 'NONE',  ( -2.171318179221914058, -78.40681307385639798, -3.601143365367586835 ) ) ;
#645 = CARTESIAN_POINT ( 'NONE',  ( 10.74341457190999982, -79.22405656010899122, -2.245675826504000216 ) ) ;
#646 = CARTESIAN_POINT ( 'NONE',  ( -14.00000000000000000, -80.89999999999999147, 0.000000000000000000 ) ) ;
#647 = CARTESIAN_POINT ( 'NONE',  ( -7.374560639699019760, -77.82708333333329165, 9.596002108778129980 ) ) ;
#648 = DIRECTION ( 'NONE',  ( 0.7071067811865473507, 1.433669009702094715E-08, 0.7071067811865473507 ) ) ;
#649 = CARTESIAN_POINT ( 'NONE',  ( 7.618386520043000765, -18.77287536652999833, -10.53495200520000097 ) ) ;
#650 = CARTESIAN_POINT ( 'NONE',  ( 12.51072239526000196, -63.10294702885996543, 0.7871079366006996647 ) ) ;
#651 = ORIENTED_EDGE ( 'NONE', *, *, #26448, .T. ) ;
#652 = CARTESIAN_POINT ( 'NONE',  ( 10.16136252780999882, -79.56206640024099386, 4.855993836148999598 ) ) ;
#653 = CARTESIAN_POINT ( 'NONE',  ( 12.70457850620686990, -16.82128713317816704, 0.5106122238172051686 ) ) ;
#654 = CARTESIAN_POINT ( 'NONE',  ( 9.393203674808260573, -79.79166666666665719, 5.413904038987188194 ) ) ;
#655 = CARTESIAN_POINT ( 'NONE',  ( -2.089807114238836583, -78.48547957940617437, 3.465957419068643297 ) ) ;
#656 = EDGE_CURVE ( 'NONE', #20949, #16041, #34601, .T. ) ;
#657 = CARTESIAN_POINT ( 'NONE',  ( 11.41636098306275215, -76.43082762775702577, -2.781676017839413539 ) ) ;
#658 = CARTESIAN_POINT ( 'NONE',  ( 10.92979202429999930, -79.06863239632698992, 1.617881315982000245 ) ) ;
#659 = CARTESIAN_POINT ( 'NONE',  ( 1.250000000000000000, -23.25000000000000000, -12.00000000000000000 ) ) ;
#660 = CARTESIAN_POINT ( 'NONE',  ( 10.48771805367000098, -20.24439828562999821, 7.686918321060999482 ) ) ;
#661 = VECTOR ( 'NONE', #54709, 1000.000000000000000 ) ;
#662 = CARTESIAN_POINT ( 'NONE',  ( -0.7554284705563480973, -81.08333333333332860, -1.310679582531387277 ) ) ;
#663 = DIRECTION ( 'NONE',  ( -2.716802477432000171E-13, 0.000000000000000000, 1.000000000000000000 ) ) ;
#664 = CIRCLE ( 'NONE', #23179, 0.5000000000000006661 ) ;
#665 = CARTESIAN_POINT ( 'NONE',  ( 8.318716844523411424, -78.25665627052904938, 7.160083125396178083 ) ) ;
#666 = EDGE_CURVE ( 'NONE', #18159, #52919, #43291, .T. ) ;
#667 = CARTESIAN_POINT ( 'NONE',  ( 0.000000000000000000, -76.79999999999999716, 0.000000000000000000 ) ) ;
#668 = ORIENTED_EDGE ( 'NONE', *, *, #34683, .T. ) ;
#669 = TOROIDAL_SURFACE ( 'NONE', #20457, 1.250000000000000000, 0.5000000000000000000 ) ;
#670 = VERTEX_POINT ( 'NONE', #3515 ) ;
#671 = CARTESIAN_POINT ( 'NONE',  ( 7.605248831740031967, -78.78754124960966010, -7.597529869121465218 ) ) ;
#672 = CARTESIAN_POINT ( 'NONE',  ( -12.00000000000000000, -79.79999999999999716, 6.639246269807000381E-13 ) ) ;
#673 = CIRCLE ( 'NONE', #41223, 10.14999999999999858 ) ;
#674 = ORIENTED_EDGE ( 'NONE', *, *, #44519, .F. ) ;
#675 = CARTESIAN_POINT ( 'NONE',  ( -12.49999991316347270, -39.30476017083000073, -0.001473401919593436823 ) ) ;
#676 = CARTESIAN_POINT ( 'NONE',  ( 8.643979526155998627, -25.25953772911000073, 9.422807787372999400 ) ) ;
#677 = ADVANCED_FACE ( 'NONE', ( #12656 ), #53694, .F. ) ;
#678 = CARTESIAN_POINT ( 'NONE',  ( 8.870414881026999154, -61.86963060230000622, 8.878264461126001095 ) ) ;
#679 = CARTESIAN_POINT ( 'NONE',  ( -6.549634241348975650, -76.96947804690607597, 10.29244451497932467 ) ) ;
#680 = CARTESIAN_POINT ( 'NONE',  ( 6.917883603915965907, -78.72389193389439299, -9.780740130690492862 ) ) ;
#681 = CARTESIAN_POINT ( 'NONE',  ( 10.93160348586000019, -79.03409100994899461, 2.513594203403000105 ) ) ;
#682 = CARTESIAN_POINT ( 'NONE',  ( 10.14177821597014173, -81.00000000000002842, 4.213176577505078235 ) ) ;
#683 = EDGE_CURVE ( 'NONE', #40118, #56133, #44534, .T. ) ;
#684 = ORIENTED_EDGE ( 'NONE', *, *, #58361, .T. ) ;
#685 = CARTESIAN_POINT ( 'NONE',  ( 7.958776490642000212, -61.27699850017000216, -9.723157983989999309 ) ) ;
#686 = ORIENTED_EDGE ( 'NONE', *, *, #25485, .T. ) ;
#687 = CARTESIAN_POINT ( 'NONE',  ( -1.468596516428545717, -77.48775315375499417, 9.132634440082403771 ) ) ;
#688 = CARTESIAN_POINT ( 'NONE',  ( -10.79754810892000094, -77.44686363549098473, -2.301543980133000211 ) ) ;
#689 = DIRECTION ( 'NONE',  ( 0.000000000000000000, 1.000000000000000000, 0.000000000000000000 ) ) ;
#690 = CARTESIAN_POINT ( 'NONE',  ( 7.405962610586999340, -77.52424149029599221, -6.270759699041999369 ) ) ;
#691 = CARTESIAN_POINT ( 'NONE',  ( -2.192937812663000141, -76.11726098207999769, -12.93882154009999930 ) ) ;
#692 = CARTESIAN_POINT ( 'NONE',  ( -10.75000000000000000, -81.00000000000000000, 2.851355842494999902E-13 ) ) ;
#693 = CARTESIAN_POINT ( 'NONE',  ( -0.9347040216968000026, -78.63485975860999133, 1.332288049216000081 ) ) ;
#694 = DIRECTION ( 'NONE',  ( 0.000000000000000000, -1.000000000000000000, 0.000000000000000000 ) ) ;
#695 = CARTESIAN_POINT ( 'NONE',  ( -3.661365483191000081, -79.33134268642398013, 10.30932680317000028 ) ) ;
#696 = CARTESIAN_POINT ( 'NONE',  ( -7.633478499826000352, -23.20098177597000344, -10.36292345935000014 ) ) ;
#697 = CARTESIAN_POINT ( 'NONE',  ( -7.452378523309739045, -60.34721902435786234, 8.090910852015730015 ) ) ;
#698 = CARTESIAN_POINT ( 'NONE',  ( 1.964355310900000262, -82.49842648807799605, 3.004164177009000181 ) ) ;
#699 = ORIENTED_EDGE ( 'NONE', *, *, #33110, .F. ) ;
#700 = CARTESIAN_POINT ( 'NONE',  ( -12.29903597714999997, -79.44542282429898705, -0.6631160193374000533 ) ) ;
#701 = CARTESIAN_POINT ( 'NONE',  ( -3.222839321634999976, -76.53899580226399735, 10.90918487679000037 ) ) ;
#702 = CARTESIAN_POINT ( 'NONE',  ( 1.078297123321654505, -77.96723831660007420, 10.71709050783147710 ) ) ;
#703 = CARTESIAN_POINT ( 'NONE',  ( -8.885616033064000163, -78.07539114513500067, 8.035041515002001589 ) ) ;
#704 = ADVANCED_FACE ( 'NONE', ( #4089 ), #7371, .F. ) ;
#705 = FACE_OUTER_BOUND ( 'NONE', #29095, .T. ) ;
#706 = AXIS2_PLACEMENT_3D ( 'NONE', #56290, #17001, #47739 ) ;
#707 = CARTESIAN_POINT ( 'NONE',  ( 0.000000000000000000, -75.19999999999998863, 0.000000000000000000 ) ) ;
#708 = CARTESIAN_POINT ( 'NONE',  ( 1.320786595080246428, -2.595329183020129271, 3.336226784969741566 ) ) ;
#709 = CARTESIAN_POINT ( 'NONE',  ( 8.032001238464035353, -80.90813382219710093, 7.145123807818250405 ) ) ;
#710 = CARTESIAN_POINT ( 'NONE',  ( -9.163349670171998085, -78.09756746102598868, -2.155044623588000086 ) ) ;
#711 = CARTESIAN_POINT ( 'NONE',  ( -6.019522479259990178, -85.88547957940599531, -4.950643703664905360 ) ) ;
#712 = CARTESIAN_POINT ( 'NONE',  ( -11.10013370946000144, -76.88383956207499637, 1.020686637641000205 ) ) ;
#713 = CARTESIAN_POINT ( 'NONE',  ( -0.6669403506045999963, -76.27067270026404344, -12.26286337364000012 ) ) ;
#714 = VECTOR ( 'NONE', #13948, 1000.000000000000000 ) ;
#715 = ORIENTED_EDGE ( 'NONE', *, *, #40383, .T. ) ;
#716 = DIRECTION ( 'NONE',  ( -1.000000000000000000, 0.000000000000000000, 0.000000000000000000 ) ) ;
#717 = CARTESIAN_POINT ( 'NONE',  ( -0.5366960857496999582, -3.191422503149000001, 3.929767262548999884 ) ) ;
#718 = CARTESIAN_POINT ( 'NONE',  ( 1.633411169670999863, -77.83494667044399762, -11.09730050697999992 ) ) ;
#719 = CARTESIAN_POINT ( 'NONE',  ( 9.233664981878000333, -79.60499486974998717, 5.933249305785000871 ) ) ;
#720 = CIRCLE ( 'NONE', #32727, 1.000000000000000000 ) ;
#721 = CARTESIAN_POINT ( 'NONE',  ( 7.620037246293000166, -23.20567269824999812, -10.53559750859000133 ) ) ;
#722 = CYLINDRICAL_SURFACE ( 'NONE', #626, 1.500000000000000000 ) ;
#723 = CARTESIAN_POINT ( 'NONE',  ( -11.75000000000000000, -76.79999999999999716, -1.435311119447000145E-14 ) ) ;
#724 = CARTESIAN_POINT ( 'NONE',  ( 12.55458938220999876, -17.83720883386000011, 1.575070636625000242 ) ) ;
#725 = CARTESIAN_POINT ( 'NONE',  ( -3.976098536387000060, -86.16144503318800218, 0.4347513405908999817 ) ) ;
#726 = CARTESIAN_POINT ( 'NONE',  ( -7.624341764923000753, -18.73514850530999709, -10.42531124853000080 ) ) ;
#727 = CARTESIAN_POINT ( 'NONE',  ( 10.18948933931000234, -55.58467389893999666, -7.645397892281000196 ) ) ;
#728 = CARTESIAN_POINT ( 'NONE',  ( -11.25716098398999954, -78.18238734777798982, -0.4530573336216000002 ) ) ;
#729 = CARTESIAN_POINT ( 'NONE',  ( 0.7545134501129999727, -80.60798800110998741, 1.485250302772000097 ) ) ;
#730 = CARTESIAN_POINT ( 'NONE',  ( 1.315513048017999953, -78.77661456821999764, 0.1100150488083000005 ) ) ;
#731 = CARTESIAN_POINT ( 'NONE',  ( 7.764258067048000811, -77.13099274720589449, 5.767450660628000492 ) ) ;
#732 = CARTESIAN_POINT ( 'NONE',  ( 1.328728262137743421, -81.53943792409916114, 0.7184295318478360892 ) ) ;
#733 = CARTESIAN_POINT ( 'NONE',  ( -1.321725462025712616, -83.30889907083121670, 0.7346322590915946860 ) ) ;
#734 = CARTESIAN_POINT ( 'NONE',  ( -1.297526016723000053, -78.46556992798305430, -10.89864408161000142 ) ) ;
#735 = DIRECTION ( 'NONE',  ( -1.000000000000000000, 0.000000000000000000, 0.000000000000000000 ) ) ;
#736 = ORIENTED_EDGE ( 'NONE', *, *, #4110, .T. ) ;
#737 = CARTESIAN_POINT ( 'NONE',  ( 1.250000000000000000, -81.84999999999999432, 0.000000000000000000 ) ) ;
#738 = EDGE_CURVE ( 'NONE', #45494, #38673, #46264, .T. ) ;
#739 = FACE_OUTER_BOUND ( 'NONE', #12321, .T. ) ;
#740 = CARTESIAN_POINT ( 'NONE',  ( -0.2300833467695000134, -78.44680123892500490, -11.11357981391999949 ) ) ;
#741 = CARTESIAN_POINT ( 'NONE',  ( 0.9995835529977264988, -80.19791666666665719, -0.7681833999686417114 ) ) ;
#742 = ORIENTED_EDGE ( 'NONE', *, *, #42939, .F. ) ;
#743 = ORIENTED_EDGE ( 'NONE', *, *, #12057, .F. ) ;
#744 = EDGE_CURVE ( 'NONE', #35616, #18221, #56482, .T. ) ;
#745 = CARTESIAN_POINT ( 'NONE',  ( -1.570404433027000168, -81.01062237281999501, -0.3755580415715000231 ) ) ;
#746 = ORIENTED_EDGE ( 'NONE', *, *, #37529, .T. ) ;
#747 = CIRCLE ( 'NONE', #43161, 1.750000000000000000 ) ;
#748 = EDGE_LOOP ( 'NONE', ( #31767, #5492, #24875, #32117, #7880, #37736, #17183, #44247, #13256, #15462, #16551 ) ) ;
#749 = CARTESIAN_POINT ( 'NONE',  ( -1.798336774608999988, -18.80355501948000096, 12.61277771566000006 ) ) ;
#750 = FACE_OUTER_BOUND ( 'NONE', #23794, .T. ) ;
#751 = CARTESIAN_POINT ( 'NONE',  ( 3.425474844296876764, -80.97395832166205309, 0.3498287032621968939 ) ) ;
#752 = CARTESIAN_POINT ( 'NONE',  ( -3.329695900066999670, -78.41871001420200571, -9.453077866293002174 ) ) ;
#753 = CARTESIAN_POINT ( 'NONE',  ( 3.185848383111141935, -78.25305747739967899, -8.692436244180706595 ) ) ;
#754 = CARTESIAN_POINT ( 'NONE',  ( 10.75000000000000355, -78.23958333333330017, -1.407171709420407035 ) ) ;
#756 = EDGE_CURVE ( 'NONE', #5144, #34885, #31774, .T. ) ;
#755 = CARTESIAN_POINT ( 'NONE',  ( 0.4408833872559000389, -78.45936893705000159, -12.05376079588999971 ) ) ;
#757 = ORIENTED_EDGE ( 'NONE', *, *, #19037, .T. ) ;
#758 = ORIENTED_EDGE ( 'NONE', *, *, #11996, .T. ) ;
#759 = DIRECTION ( 'NONE',  ( 0.000000000000000000, 0.000000000000000000, -1.000000000000000000 ) ) ;
#760 = CARTESIAN_POINT ( 'NONE',  ( -0.3926218265389255779, -79.39583333333335702, 1.460959015002472494 ) ) ;
#761 = VECTOR ( 'NONE', #45339, 1000.000000000000000 ) ;
#762 = LINE ( 'NONE', #36733, #5023 ) ;
#763 = CARTESIAN_POINT ( 'NONE',  ( 2.260091721765999928, -78.85325092453199147, -9.437303113984999214 ) ) ;
#764 = AXIS2_PLACEMENT_3D ( 'NONE', #15536, #51568, #1982 ) ;
#765 = CARTESIAN_POINT ( 'NONE',  ( -1.181111693982000110, -79.17654225787899236, -0.4092372983238000139 ) ) ;
#766 = CARTESIAN_POINT ( 'NONE',  ( -10.55911395187000146, -19.21538333566000034, 7.642160924884000117 ) ) ;
#767 = CARTESIAN_POINT ( 'NONE',  ( -9.194628130165000357, -76.98075131598999121, -9.128060447331000304 ) ) ;
#768 = CARTESIAN_POINT ( 'NONE',  ( -1.436931233250000162, -79.65986802222998620, -0.3027821832741999786 ) ) ;
#769 = CARTESIAN_POINT ( 'NONE',  ( -12.92177931904999966, -21.75736537952000305, -2.062503053667999797 ) ) ;
#770 = CARTESIAN_POINT ( 'NONE',  ( 10.07627163191000008, -18.75000000310999937, 7.601397897754999633 ) ) ;
#771 = CARTESIAN_POINT ( 'NONE',  ( 2.775756403448000231, -81.13869062511399477, 3.115324875632000001 ) ) ;
#772 = CARTESIAN_POINT ( 'NONE',  ( -9.578166812159000898, -80.15420130091290218, 5.930253639820000089 ) ) ;
#773 = CARTESIAN_POINT ( 'NONE',  ( -5.809342935555999787, -78.93238667140099096, 7.891128111295000025 ) ) ;
#774 = CARTESIAN_POINT ( 'NONE',  ( 2.986710853074932448, -2.883334572040014088, 1.279778411999374477 ) ) ;
#775 = CARTESIAN_POINT ( 'NONE',  ( 9.494399870356199145, -76.17369791634894227, -7.297544775540704798 ) ) ;
#776 = CARTESIAN_POINT ( 'NONE',  ( -0.1765672563250000049, -78.38009428516419064, -1.321892640673999919 ) ) ;
#777 = DIRECTION ( 'NONE',  ( 0.000000000000000000, 0.000000000000000000, 1.000000000000000000 ) ) ;
#778 = CARTESIAN_POINT ( 'NONE',  ( 3.594201416108000036, -3.128676228555999916, 1.252117639952999850 ) ) ;
#779 = CARTESIAN_POINT ( 'NONE',  ( 0.04837777540751588695, -77.19999999999998863, -10.99285280508881080 ) ) ;
#780 = EDGE_LOOP ( 'NONE', ( #684, #45447, #45553, #30245 ) ) ;
#781 = CARTESIAN_POINT ( 'NONE',  ( -1.439896632895311113, -78.31458333333333144, -11.00000000000000355 ) ) ;
#782 = CARTESIAN_POINT ( 'NONE',  ( 8.140250184781665510, -60.25160423313176494, -7.398464061246547097 ) ) ;
#783 = CARTESIAN_POINT ( 'NONE',  ( -9.344422729779601866, -77.64679824576278122, 7.168946966961233791 ) ) ;
#784 = CARTESIAN_POINT ( 'NONE',  ( 5.348414924440999307, -79.50038437275298975, -8.153793349671000001 ) ) ;
#785 = CARTESIAN_POINT ( 'NONE',  ( -12.97295173694999981, -77.52358135215001766, -1.020668466325000079 ) ) ;
#786 = CARTESIAN_POINT ( 'NONE',  ( -9.038474301085981821, -79.55454762255861567, 5.819977710880431587 ) ) ;
#787 = EDGE_CURVE ( 'NONE', #12448, #10446, #50841, .T. ) ;
#788 = CARTESIAN_POINT ( 'NONE',  ( -8.611000706001480154, -61.97488119190911959, -9.355851007328045199 ) ) ;
#789 = CYLINDRICAL_SURFACE ( 'NONE', #25534, 11.00000000000000000 ) ;
#790 = ORIENTED_EDGE ( 'NONE', *, *, #51975, .F. ) ;
#791 = DIRECTION ( 'NONE',  ( 0.000000000000000000, -1.000000000000000000, 0.000000000000000000 ) ) ;
#792 = CARTESIAN_POINT ( 'NONE',  ( -11.06454125523000087, -77.73236022357899344, 1.497041118686999850 ) ) ;
#793 = CARTESIAN_POINT ( 'NONE',  ( 0.5862232456189999663, -82.13815345286899117, 1.280678996225000033 ) ) ;
#794 = DIRECTION ( 'NONE',  ( 0.000000000000000000, -1.000000000000000000, 0.000000000000000000 ) ) ;
#795 = CARTESIAN_POINT ( 'NONE',  ( 4.459991035765999534, -77.79314704349698673, 8.413017068390001185 ) ) ;
#797 = CARTESIAN_POINT ( 'NONE',  ( -3.616527695712999702, -1.828510311347000039, -0.5438149879621999583 ) ) ;
#796 = CARTESIAN_POINT ( 'NONE',  ( -4.092573046463000352, -82.97942814914499365, 0.5562009154790999998 ) ) ;
#798 = CARTESIAN_POINT ( 'NONE',  ( 0.3271848554490964789, -82.35416666666665719, 1.217465845835395521 ) ) ;
#799 = CARTESIAN_POINT ( 'NONE',  ( -1.199500263597274685, -81.44791666666668561, 0.9218200799623673669 ) ) ;
#800 = VERTEX_POINT ( 'NONE', #46611 ) ;
#801 = CARTESIAN_POINT ( 'NONE',  ( -6.221842943951165772, -77.17604202210270614, -8.766351684138484757 ) ) ;
#802 = FACE_OUTER_BOUND ( 'NONE', #19750, .T. ) ;
#803 = TOROIDAL_SURFACE ( 'NONE', #14878, 17.50000000000000000, 5.000000000000000000 ) ;
#804 = EDGE_LOOP ( 'NONE', ( #53108, #929, #5072, #12373 ) ) ;
#805 = ORIENTED_EDGE ( 'NONE', *, *, #405, .F. ) ;
#806 = CARTESIAN_POINT ( 'NONE',  ( 9.468750000004000356, -79.53124999999600675, -6.681056941828999630E-10 ) ) ;
#807 = DIRECTION ( 'NONE',  ( 0.000000000000000000, 1.000000000000000000, 0.000000000000000000 ) ) ;
#808 = CARTESIAN_POINT ( 'NONE',  ( 12.50000000000000000, -63.73717104351998586, 1.868318442826999995E-13 ) ) ;
#809 = ORIENTED_EDGE ( 'NONE', *, *, #15642, .T. ) ;
#810 = ADVANCED_FACE ( 'NONE', ( #55743 ), #50973, .T. ) ;
#811 = CARTESIAN_POINT ( 'NONE',  ( 7.527227981725999939, -78.51244375222299254, 9.409389490551998136 ) ) ;
#812 = EDGE_LOOP ( 'NONE', ( #37953, #24356, #35317, #52754 ) ) ;
#813 = ORIENTED_EDGE ( 'NONE', *, *, #41982, .F. ) ;
#814 = DIRECTION ( 'NONE',  ( 0.000000000000000000, 1.000000000000000000, 0.000000000000000000 ) ) ;
#815 = ORIENTED_EDGE ( 'NONE', *, *, #52470, .F. ) ;
#816 = CARTESIAN_POINT ( 'NONE',  ( -11.68619273497913014, -76.42035715448702149, -3.140303762288782163 ) ) ;
#817 = CARTESIAN_POINT ( 'NONE',  ( -12.80088938722999892, -22.76256651757000071, -1.980532758767000301 ) ) ;
#818 = B_SPLINE_SURFACE_WITH_KNOTS ( 'NONE', 3, 3, ( 
 ( #39006, #21856, #17146, #8578, #52308, #11864, #12432, #20715, #44020, #25714, #16866, #29841, #57878, #34561, #43740, #3858, #35133, #7424, #26565, #12713, #26288, #8000, #30425, #3572, #34847, #53164, #52878, #25428, #57304, #38715, #52593, #12143, #30131, #48180, #48457 ),
 ( #25997, #21576, #30706, #39581, #48743, #13881, #36609, #54631, #14168, #5322, #4446, #27154, #41337, #4151, #58171, #36896, #22447, #54909, #54, #17737, #18029, #36021, #25219, #43239, #9841, #26576, #58184, #12725, #44610, #35735, #21870, #22164, #35433, #39306, #30717 ),
 ( #4165, #39878, #26008, #34574, #8299, #3305, #53462, #16880, #30437, #40171, #57891, #17447, #48468, #44034, #34861, #39593, #31005, #47909, #8588, #52607, #7441, #25440, #43458, #21013, #39018, #16589, #12157, #30144, #48193, #7726, #32983, #11453, #2595, #25012, #20022 ),
 ( #15871, #33280, #10282, #55444, #14986, #46316, #32692, #6427, #6135, #51320, #15580, #24442, #10878, #38299, #29432, #11170, #29145, #47485, #47191, #51029, #5841, #56605, #42456, #20593, #33575, #43033, #38006, #42162, #24142, #23847, #51614, #19432, #10578, #2024, #56031 ) ),
 .UNSPECIFIED., .F., .F., .F.,
 ( 4, 4 ),
 ( 4, 1, 1, 1, 1, 1, 1, 1, 1, 1, 1, 1, 1, 1, 1, 1, 1, 1, 1, 1, 1, 1, 1, 1, 1, 1, 1, 1, 1, 1, 1, 1, 4 ),
 ( -0.3882448580381000491, 1.388244858038000018 ),
 ( -0.02000000000000000042, 0.01250000000000000069, 0.04499999999999999833, 0.07749999999999999944, 0.1100000000000000006, 0.1424999999999999878, 0.1749999999999999889, 0.2074999999999999900, 0.2399999999999999911, 0.2725000000000000200, 0.3049999999999999933, 0.3375000000000000222, 0.3699999999999999956, 0.4025000000000000244, 0.4349999999999999978, 0.4675000000000000266, 0.5000000000000000000, 0.5324999999999999734, 0.5649999999999999467, 0.5975000000000000311, 0.6300000000000000044, 0.6624999999999999778, 0.6949999999999999512, 0.7275000000000000355, 0.7600000000000000089, 0.7924999999999999822, 0.8249999999999999556, 0.8575000000000000400, 0.8900000000000000133, 0.9224999999999999867, 0.9549999999999999600, 0.9875000000000000444, 1.020000000000000018 ),
 .UNSPECIFIED. ) ;
#819 = ORIENTED_EDGE ( 'NONE', *, *, #11465, .T. ) ;
#821 = EDGE_CURVE ( 'NONE', #25723, #3607, #50108, .T. ) ;
#820 = CARTESIAN_POINT ( 'NONE',  ( 0.8847132563061232968, -82.78824692404089092, -0.8824945250560863874 ) ) ;
#822 = VERTEX_POINT ( 'NONE', #43035 ) ;
#823 = CARTESIAN_POINT ( 'NONE',  ( 0.000000000000000000, -76.00000000000000000, 0.000000000000000000 ) ) ;
#824 = DIRECTION ( 'NONE',  ( 0.000000000000000000, 0.000000000000000000, 1.000000000000000000 ) ) ;
#825 = CARTESIAN_POINT ( 'NONE',  ( 0.000000000000000000, -74.64999999999999147, 0.000000000000000000 ) ) ;
#826 = DIRECTION ( 'NONE',  ( 0.000000000000000000, -1.000000000000000000, 0.000000000000000000 ) ) ;
#827 = CARTESIAN_POINT ( 'NONE',  ( -10.61943132853148697, -78.49189918985904058, -6.134787038820419092 ) ) ;
#828 = CONICAL_SURFACE ( 'NONE', #33783, 10.96250000000000036, 0.7853981633972997312 ) ;
#829 = CARTESIAN_POINT ( 'NONE',  ( -4.800187936532999800, -76.10861960676400884, 10.10109298474000106 ) ) ;
#830 = CARTESIAN_POINT ( 'NONE',  ( 0.000000000000000000, -92.79999999999999716, 0.000000000000000000 ) ) ;
#831 = LINE ( 'NONE', #40059, #35552 ) ;
#832 = CARTESIAN_POINT ( 'NONE',  ( -7.627487525433000570, -60.09778754156999980, -10.35845608626999947 ) ) ;
#833 = CARTESIAN_POINT ( 'NONE',  ( 0.03267024647290020511, -78.72542977318258295, -9.249861488902391571 ) ) ;
#834 = CARTESIAN_POINT ( 'NONE',  ( -0.4515105396345309163, -23.54721902468446615, -10.99076531923747169 ) ) ;
#835 = CARTESIAN_POINT ( 'NONE',  ( -1.261445002938999860, -79.14688792748098933, -0.1968185027220000216 ) ) ;
#836 = CARTESIAN_POINT ( 'NONE',  ( -9.170121691637055150, -80.14671525588798318, -6.075096402074364299 ) ) ;
#837 = CARTESIAN_POINT ( 'NONE',  ( 6.877869950458871173, -78.27974359454508146, 9.927636754982094303 ) ) ;
#838 = CARTESIAN_POINT ( 'NONE',  ( 2.359552285272000116, -78.92253455456848599, -3.184099749658000356 ) ) ;
#839 = CARTESIAN_POINT ( 'NONE',  ( -8.920186055527000946, -77.16191332859899887, 3.688297430249000364 ) ) ;
#840 = CARTESIAN_POINT ( 'NONE',  ( 0.1762382865323051384, -79.63606589178333195, -1.250387681160788134 ) ) ;
#841 = CIRCLE ( 'NONE', #12100, 9.250000000000000000 ) ;
#842 = LINE ( 'NONE', #22663, #35837 ) ;
#843 = CARTESIAN_POINT ( 'NONE',  ( -8.022734517049746273E-06, -82.01564364893640402, -1.484164386985079798 ) ) ;
#844 = CARTESIAN_POINT ( 'NONE',  ( 2.076026496572000113, -1.729178536415000078, -2.969150124377000211 ) ) ;
#845 = FACE_OUTER_BOUND ( 'NONE', #7013, .T. ) ;
#846 = CARTESIAN_POINT ( 'NONE',  ( 2.264809212410999647E-14, -92.79999999999999716, 0.000000000000000000 ) ) ;
#847 = CARTESIAN_POINT ( 'NONE',  ( 12.70722176274191106, -24.41036110619398869, -1.610175936229214955 ) ) ;
#848 = CARTESIAN_POINT ( 'NONE',  ( -0.4056890888208716794, -79.74603335400661308, 1.458054600993641259 ) ) ;
#849 = CARTESIAN_POINT ( 'NONE',  ( 13.98934701301999972, -69.37813015403000350, 1.420884290687999928E-05 ) ) ;
#850 = CARTESIAN_POINT ( 'NONE',  ( 0.5999999999999999778, -18.84999999999999787, -12.00000000000000000 ) ) ;
#851 = EDGE_CURVE ( 'NONE', #37067, #54376, #38681, .T. ) ;
#852 = CARTESIAN_POINT ( 'NONE',  ( 11.48873525783000105, -77.65213037933499152, 4.336443399433000501 ) ) ;
#853 = LINE ( 'NONE', #23260, #22232 ) ;
#855 = CARTESIAN_POINT ( 'NONE',  ( 0.7281259072094999896, -77.96523380450278751, -1.216509659635999885 ) ) ;
#854 = FACE_OUTER_BOUND ( 'NONE', #17770, .T. ) ;
#856 = CARTESIAN_POINT ( 'NONE',  ( 1.606311393998999915, -82.99304616690000103, -0.5653197666394998988 ) ) ;
#857 = ORIENTED_EDGE ( 'NONE', *, *, #38891, .F. ) ;
#858 = ADVANCED_FACE ( 'NONE', ( #52466 ), #2310, .T. ) ;
#859 = CARTESIAN_POINT ( 'NONE',  ( -3.348285028641999617, -83.47632450217398059, -1.293338634809000132 ) ) ;
#860 = CARTESIAN_POINT ( 'NONE',  ( -6.095058532100999571, -81.19811224954469253, 9.210169058603000281 ) ) ;
#861 = DIRECTION ( 'NONE',  ( -1.205798306211979422E-11, -1.868136817095964273E-07, -0.9999999999999824585 ) ) ;
#862 = CARTESIAN_POINT ( 'NONE',  ( 0.8812128323519314854, -85.13645834205065910, -3.328407071930476580 ) ) ;
#863 = CARTESIAN_POINT ( 'NONE',  ( 12.54981748959999877, -53.75163512338999539, 0.03767836620429999839 ) ) ;
#864 = CARTESIAN_POINT ( 'NONE',  ( -3.180509609271000127, -77.65086001149001049, 12.23476839664999893 ) ) ;
#865 = CARTESIAN_POINT ( 'NONE',  ( 11.75000000000000000, -79.80000000000002558, -1.240340237986687466 ) ) ;
#866 = CARTESIAN_POINT ( 'NONE',  ( 0.9783655976132111798, -77.00000000000000000, 9.249733681752722703 ) ) ;
#867 = ORIENTED_EDGE ( 'NONE', *, *, #17371, .T. ) ;
#868 = CARTESIAN_POINT ( 'NONE',  ( 1.779623408300066600, -54.66369130952791267, -12.71471627654026193 ) ) ;
#869 = CARTESIAN_POINT ( 'NONE',  ( 9.235752227612000098, -79.39493998579798983, 1.834089355993999915 ) ) ;
#870 = VECTOR ( 'NONE', #48376, 1000.000000000000000 ) ;
#871 = CARTESIAN_POINT ( 'NONE',  ( 9.533274928461036524, -75.89964387654679001, -6.929128638878494506 ) ) ;
#872 = CARTESIAN_POINT ( 'NONE',  ( -1.295435361468000091, -77.65342075185570536, -0.3166359884281000348 ) ) ;
#873 = CARTESIAN_POINT ( 'NONE',  ( -12.50000000000000000, -17.31762331506999786, -1.005384022379999909 ) ) ;
#874 = CARTESIAN_POINT ( 'NONE',  ( 1.249565383984963862, -80.84028809121133463, -0.1639645281534745924 ) ) ;
#875 = ORIENTED_EDGE ( 'NONE', *, *, #15950, .F. ) ;
#876 = EDGE_CURVE ( 'NONE', #34959, #39806, #20595, .T. ) ;
#877 = CARTESIAN_POINT ( 'NONE',  ( 11.26957934775000147, -79.10909624325299205, 4.877733875464000057 ) ) ;
#878 = CARTESIAN_POINT ( 'NONE',  ( 8.003872304214999289, -77.24441679105500214, -8.008117534469000987 ) ) ;
#879 = CARTESIAN_POINT ( 'NONE',  ( -2.062597265787999845, -19.21538333566000034, 12.87024489160000051 ) ) ;
#880 = ORIENTED_EDGE ( 'NONE', *, *, #55863, .T. ) ;
#881 = AXIS2_PLACEMENT_3D ( 'NONE', #18000, #35097, #17705 ) ;
#882 = CARTESIAN_POINT ( 'NONE',  ( 12.50485692589171194, -24.86593462704852797, -0.6924071800257274312 ) ) ;
#883 = SHAPE_REPRESENTATION_RELATIONSHIP ( 'NONE' , 'NONE' ,  #7439, #51784 ) ;
#884 = CARTESIAN_POINT ( 'NONE',  ( 6.728605944993000243, -79.69578255762351660, -7.080011783993000130 ) ) ;
#885 = ORIENTED_EDGE ( 'NONE', *, *, #57938, .F. ) ;
#887 = EDGE_CURVE ( 'NONE', #29780, #37236, #38592, .T. ) ;
#886 = CARTESIAN_POINT ( 'NONE',  ( 5.438910196678000020, -76.28506842486599737, -10.95925680354000065 ) ) ;
#888 = CARTESIAN_POINT ( 'NONE',  ( 7.861032689861890077, -24.46660299217103329, -10.10708926022225107 ) ) ;
#889 = CARTESIAN_POINT ( 'NONE',  ( -1.113811846534999983, -78.14627689099999941, 1.056031667973999832 ) ) ;
#890 = EDGE_CURVE ( 'NONE', #52925, #8280, #49060, .T. ) ;
#891 = VERTEX_POINT ( 'NONE', #42458 ) ;
#892 = CARTESIAN_POINT ( 'NONE',  ( 1.009320482739999969, -77.49657694988499657, 9.441330439200999791 ) ) ;
#893 = DIRECTION ( 'NONE',  ( -0.7071067811865475727, 0.000000000000000000, 0.7071067811865475727 ) ) ;
#894 = CARTESIAN_POINT ( 'NONE',  ( -0.8733059116898821417, -80.16394694085556694, -0.8939094887366128006 ) ) ;
#895 = CARTESIAN_POINT ( 'NONE',  ( 0.5135400119170026034, -16.82131466139542297, -12.70453250098683284 ) ) ;
#896 = CARTESIAN_POINT ( 'NONE',  ( -3.485499217011999828, -78.48547958007489456, -1.904403262310999906E-08 ) ) ;
#897 = CARTESIAN_POINT ( 'NONE',  ( 9.249687267056886597, -79.85225412240586707, 0.2014328667283708241 ) ) ;
#898 = CARTESIAN_POINT ( 'NONE',  ( 0.4567011726104230895, -78.99889090922864909, -1.468873967789304125 ) ) ;
#899 = CARTESIAN_POINT ( 'NONE',  ( 0.8163124805188861632, -79.12395831701307714, -3.929161116704327217 ) ) ;
#900 = VERTEX_POINT ( 'NONE', #11455 ) ;
#901 = CARTESIAN_POINT ( 'NONE',  ( -8.300970689365472666, -77.75833333333333997, 4.784380313523514339 ) ) ;
#902 = CARTESIAN_POINT ( 'NONE',  ( 6.153863461931999623, -76.18399160466999831, -10.66140155521000032 ) ) ;
#903 = CARTESIAN_POINT ( 'NONE',  ( 0.3023484132065000218, -79.99366136053998844, -1.485775080250999913 ) ) ;
#904 = CARTESIAN_POINT ( 'NONE',  ( -0.05152873501919019023, -1.973120583389267546, -3.519131412915782242 ) ) ;
#906 = ADVANCED_FACE ( 'NONE', ( #47487 ), #15853, .F. ) ;
#905 = CIRCLE ( 'NONE', #55587, 0.5000000000000001110 ) ;
#907 = CARTESIAN_POINT ( 'NONE',  ( 12.49306764015999960, -18.71943464842000182, 1.667917367065999912 ) ) ;
#908 = CARTESIAN_POINT ( 'NONE',  ( 10.16243366810999937, -79.22005705677000265, -6.864696462387000153 ) ) ;
#909 = FACE_OUTER_BOUND ( 'NONE', #1382, .T. ) ;
#910 = CARTESIAN_POINT ( 'NONE',  ( 9.386754667005000385, -79.85238712864799027, 6.031619700400000283 ) ) ;
#911 = CARTESIAN_POINT ( 'NONE',  ( 1.337313094397592161, -2.759813985991205865, -2.961831082111990643 ) ) ;
#912 = B_SPLINE_CURVE_WITH_KNOTS ( 'NONE', 3,
 ( #17029, #35299, #12028, #30008, #21457, #34727, #52756, #30299, #53328, #12874, #12309, #4021, #30876, #2881, #48911, #53625, #48340, #8452 ),
 .UNSPECIFIED., .F., .F.,
 ( 4, 2, 2, 2, 2, 2, 2, 2, 4 ),
 ( 0.000000000000000000, 0.1249999999999999722, 0.2499999999999999445, 0.3749999999999998890, 0.4999999999999998890, 0.6249999999999998890, 0.7499999999999997780, 0.8749999999999998890, 1.000000000000000000 ),
 .UNSPECIFIED. ) ;
#913 = CARTESIAN_POINT ( 'NONE',  ( -1.206136157490516725, -77.16700393412037329, -11.95863077309826750 ) ) ;
#914 = CARTESIAN_POINT ( 'NONE',  ( -2.848564863371000122, -78.85456761274453186, -10.84913769894000168 ) ) ;
#915 = EDGE_LOOP ( 'NONE', ( #29593, #53331, #24815, #5796 ) ) ;
#916 = CARTESIAN_POINT ( 'NONE',  ( -0.3643839585117999991, -81.91670264959000747, 1.301227969886000091 ) ) ;
#917 = CARTESIAN_POINT ( 'NONE',  ( -1.322249586278000155, -80.03650139976998901, -0.2786171024073000324 ) ) ;
#918 = DIRECTION ( 'NONE',  ( 1.558073931336000057E-11, -1.000000000000000000, 1.336740861260999965E-10 ) ) ;
#919 = CIRCLE ( 'NONE', #14073, 10.25000000000000000 ) ;
#920 = DIRECTION ( 'NONE',  ( 0.000000000000000000, -0.7071067811866525998, -0.7071067811864425456 ) ) ;
#921 = CARTESIAN_POINT ( 'NONE',  ( 7.970414252932632060, -24.52292089079952930, 9.713036876646206963 ) ) ;
#922 = ADVANCED_FACE ( 'NONE', ( #50957, #28492, #5484, #46543, #10509, #6065 ), #55373, .F. ) ;
#923 = CONICAL_SURFACE ( 'NONE', #8425, 0.6999999997695030007, 0.7853981633972997312 ) ;
#924 = CARTESIAN_POINT ( 'NONE',  ( -4.771559678803999560, -78.60146397087400771, -11.06471824780000013 ) ) ;
#925 = CARTESIAN_POINT ( 'NONE',  ( 8.177883213696999221, -77.91265682217398592, -5.086790354254000057 ) ) ;
#926 = CARTESIAN_POINT ( 'NONE',  ( 1.068457326610549929, -76.06767717856887145, 11.70300179015460351 ) ) ;
#927 = CARTESIAN_POINT ( 'NONE',  ( 10.41480047653000085, -78.68212195875699422, -3.637813056042999982 ) ) ;
#928 = CARTESIAN_POINT ( 'NONE',  ( 3.549939863155112008, -85.80681307243297340, 2.578428034955769999 ) ) ;
#929 = ORIENTED_EDGE ( 'NONE', *, *, #4950, .T. ) ;
#930 = ADVANCED_FACE ( 'NONE', ( #13751 ), #32043, .F. ) ;
#931 = CARTESIAN_POINT ( 'NONE',  ( 5.684875707061095795, -77.92308321104999891, 7.397310562483891516 ) ) ;
#932 = CARTESIAN_POINT ( 'NONE',  ( -10.69701368780000017, -79.98255012709098821, 1.066019776055000090 ) ) ;
#933 = CARTESIAN_POINT ( 'NONE',  ( -10.71369944335147473, -79.12083333333333712, -2.879226727952079123 ) ) ;
#934 = CARTESIAN_POINT ( 'NONE',  ( 12.50483450299711130, -17.13545441866522623, -0.6958183770738737284 ) ) ;
#935 = CARTESIAN_POINT ( 'NONE',  ( 0.1759108568145950069, -79.23653620316339641, -1.251611073654840034 ) ) ;
#936 = CARTESIAN_POINT ( 'NONE',  ( 8.533817832784000856, -16.99473856456000220, -9.213092693308000847 ) ) ;
#937 = CARTESIAN_POINT ( 'NONE',  ( 8.096452064242996016, -56.01421830980998351, -13.15643568217000769 ) ) ;
#938 = ORIENTED_EDGE ( 'NONE', *, *, #40154, .T. ) ;
#939 = CARTESIAN_POINT ( 'NONE',  ( -3.994755123096000560, -79.11303053380299843, 10.40656197200999955 ) ) ;
#940 = CARTESIAN_POINT ( 'NONE',  ( 1.500000000000000000, -80.65000000000000568, 0.000000000000000000 ) ) ;
#941 = CARTESIAN_POINT ( 'NONE',  ( -3.037998163973060883, -79.44541822414515764, 11.43917581953734697 ) ) ;
#942 = CARTESIAN_POINT ( 'NONE',  ( 3.485499217012000717, -78.48547957940617437, 2.057048811703057645 ) ) ;
#943 = CARTESIAN_POINT ( 'NONE',  ( -7.713973254602257690, -76.88321291978049032, 9.284400534344989353 ) ) ;
#945 = CARTESIAN_POINT ( 'NONE',  ( -1.173001147021014212, -81.57218295784426232, 0.4318201719082435108 ) ) ;
#944 = CARTESIAN_POINT ( 'NONE',  ( -1.220882145615000081, -81.12712481262300912, 0.5000124012157000086 ) ) ;
#946 = B_SPLINE_CURVE_WITH_KNOTS ( 'NONE', 3,
 ( #53761, #12615, #7899, #26191, #7041, #7324 ),
 .UNSPECIFIED., .F., .F.,
 ( 4, 1, 1, 4 ),
 ( 0.000000000000000000, 0.3333333333333000081, 0.6666666666667000474, 1.000000000000000000 ),
 .UNSPECIFIED. ) ;
#947 = LINE ( 'NONE', #41653, #22243 ) ;
#948 = DIRECTION ( 'NONE',  ( -1.000000000000000000, 0.000000000000000000, 0.000000000000000000 ) ) ;
#949 = CARTESIAN_POINT ( 'NONE',  ( -0.9491653955992001013, -78.01964351345999660, 0.8999264274451000967 ) ) ;
#950 = B_SPLINE_CURVE_WITH_KNOTS ( 'NONE', 3,
 ( #46073, #45780, #6184, #14456, #37471, #23607, #15041, #51080, #28612, #20350, #48379, #16211, #43654, #11783, #39207, #57222, #25631, #7630, #34479, #15919, #48098, #25060, #3214, #20919, #33904, #38920, #7060, #47535, #51946, #16787, #56655, #51666, #56938, #38638, #29756, #11503, #30047, #21202, #38060, #29476, #43084, #11213, #3492, #47813, #25918, #16498, #7917, #43358, #2642, #34770, #52510, #12066, #52794, #12349, #38347, #29191, #56081, #7344, #43941, #30336, #15627, #24778, #33622, #47239, #6769, #20635, #42791, #2354, #56368, #34188, #2919, #52226, #25343, #16064, #11355, #29621, #10475, #10775, #29051, #25203, #37617, #46509, #2778, #51511, #28753, #33474, #15186, #38778, #43222, #42644, #2210, #55634, #42058, #47090, #19919, #42356, #15484, #32884, #1924, #29333, #37909, #20777, #14886, #11643, #6034, #55933, #33176 ),
 .UNSPECIFIED., .F., .F.,
 ( 4, 2, 2, 2, 2, 2, 1, 2, 2, 2, 2, 2, 2, 2, 2, 2, 2, 2, 2, 2, 2, 2, 2, 2, 2, 2, 2, 1, 2, 2, 2, 2, 2, 2, 2, 2, 2, 2, 2, 2, 2, 2, 2, 2, 2, 2, 2, 2, 1, 2, 2, 2, 2, 2, 4 ),
 ( 0.000000000000000000, 0.01562500000000001388, 0.03125000000000003469, 0.04687500000000005551, 0.06250000000000008327, 0.07812500000000009714, 0.09375000000000011102, 0.1093750000000001249, 0.1250000000000001388, 0.1406250000000001110, 0.1562500000000001110, 0.1718750000000000833, 0.1875000000000000833, 0.2031250000000000833, 0.2187500000000001110, 0.2343750000000001110, 0.2500000000000001110, 0.2656250000000001110, 0.2812500000000001110, 0.2968750000000001665, 0.3125000000000001665, 0.3281250000000001665, 0.3437500000000001665, 0.3750000000000001665, 0.4062500000000001110, 0.4375000000000001110, 0.4687500000000000555, 0.5000000000000000000, 0.5312500000000000000, 0.5624999999999998890, 0.5937499999999998890, 0.6249999999999997780, 0.6562499999999997780, 0.6718749999999997780, 0.6874999999999997780, 0.7031249999999998890, 0.7187499999999998890, 0.7343749999999998890, 0.7499999999999998890, 0.7656249999999998890, 0.7812499999999998890, 0.7968749999999998890, 0.8124999999999998890, 0.8281250000000000000, 0.8437500000000000000, 0.8593750000000000000, 0.8750000000000000000, 0.8906250000000000000, 0.9062500000000000000, 0.9218750000000000000, 0.9375000000000000000, 0.9531250000000001110, 0.9687500000000001110, 0.9843750000000001110, 1.000000000000000000 ),
 .UNSPECIFIED. ) ;
#951 = CARTESIAN_POINT ( 'NONE',  ( -2.421167930323375295, -79.89583333333331439, 9.009247259181911716 ) ) ;
#952 = CARTESIAN_POINT ( 'NONE',  ( -0.5194061720425894313, -79.07133454617610369, -10.96348649343952353 ) ) ;
#953 = DIRECTION ( 'NONE',  ( -1.000000000000000000, 0.000000000000000000, 0.000000000000000000 ) ) ;
#954 = ORIENTED_EDGE ( 'NONE', *, *, #20729, .T. ) ;
#955 = EDGE_LOOP ( 'NONE', ( #118, #10532, #10822 ) ) ;
#956 = CARTESIAN_POINT ( 'NONE',  ( 1.958352037450999727, -78.23868998579800405, 9.829161269560000136 ) ) ;
#957 = CARTESIAN_POINT ( 'NONE',  ( 7.478737840490471633, -78.78621029007136656, -7.724116019082565288 ) ) ;
#958 = CIRCLE ( 'NONE', #32, 10.25000000000000000 ) ;
#959 = ORIENTED_EDGE ( 'NONE', *, *, #25485, .F. ) ;
#960 = CARTESIAN_POINT ( 'NONE',  ( 10.63539757175482059, -80.28072916675431259, -2.857308679526295414 ) ) ;
#961 = CARTESIAN_POINT ( 'NONE',  ( 3.441149770290139909, -83.94166667910380397, -0.1250751152382284792 ) ) ;
#962 = AXIS2_PLACEMENT_3D ( 'NONE', #18788, #9054, #54519 ) ;
#963 = CARTESIAN_POINT ( 'NONE',  ( 8.950141054477999347, -62.00112627243999697, 8.958565985388998953 ) ) ;
#964 = DIRECTION ( 'NONE',  ( 0.9999548435846228323, 0.000000000000000000, 0.009503199022040118363 ) ) ;
#965 = CARTESIAN_POINT ( 'NONE',  ( -9.690759288037638086, -78.09991767914834782, -7.043378150385348313 ) ) ;
#966 = CARTESIAN_POINT ( 'NONE',  ( 2.407803015296000382, -80.19133328329790800, 10.73324203768999929 ) ) ;
#967 = CARTESIAN_POINT ( 'NONE',  ( 4.500641208133613347, -81.00000000000001421, 9.880214559888472081 ) ) ;
#968 = ORIENTED_EDGE ( 'NONE', *, *, #8365, .F. ) ;
#969 = PLANE ( 'NONE',  #18971 ) ;
#970 = ORIENTED_EDGE ( 'NONE', *, *, #39826, .F. ) ;
#971 = CARTESIAN_POINT ( 'NONE',  ( 8.041760575514985021, -77.39131006114457989, 4.573409923808502420 ) ) ;
#972 = CARTESIAN_POINT ( 'NONE',  ( -11.00724581733999941, -77.92400926547099971, 0.8512868710715000287 ) ) ;
#973 = CARTESIAN_POINT ( 'NONE',  ( 9.576266942756152645, -76.04999999999998295, 5.533717098124343536 ) ) ;
#974 = CARTESIAN_POINT ( 'NONE',  ( 0.3299670982549000042, -78.85056507792100433, 1.580613947285000043 ) ) ;
#975 = CARTESIAN_POINT ( 'NONE',  ( 6.139551537448999063, -76.07905556059000673, 11.06116137296999824 ) ) ;
#976 = ADVANCED_FACE ( 'NONE', ( #22913 ), #84, .F. ) ;
#977 = CARTESIAN_POINT ( 'NONE',  ( 1.570796326794910547, -78.53541666666664867, -11.99999999999999822 ) ) ;
#978 = CARTESIAN_POINT ( 'NONE',  ( 0.4326115402657000342, -78.91680236158998696, -1.568920109259999807 ) ) ;
#979 = DIRECTION ( 'NONE',  ( 0.000000000000000000, 0.000000000000000000, -1.000000000000000000 ) ) ;
#980 = CARTESIAN_POINT ( 'NONE',  ( 5.312973029106999867, -78.26383322178199364, 9.563478878364000124 ) ) ;
#981 = EDGE_CURVE ( 'NONE', #9701, #31705, #54281, .T. ) ;
#982 = CARTESIAN_POINT ( 'NONE',  ( -7.981656248348999227, -24.71865039503999739, -10.08154475890999890 ) ) ;
#983 = CARTESIAN_POINT ( 'NONE',  ( -7.387512494710427369, -60.21532333328988784, 8.150146600852218981 ) ) ;
#984 = CARTESIAN_POINT ( 'NONE',  ( -3.341510155812000171, -84.42243313234698121, 1.310745937740000144 ) ) ;
#985 = EDGE_LOOP ( 'NONE', ( #21475, #16744, #42328, #26988, #17962 ) ) ;
#986 = DIRECTION ( 'NONE',  ( 0.000000000000000000, 1.000000000000000000, 0.000000000000000000 ) ) ;
#987 = CARTESIAN_POINT ( 'NONE',  ( -8.615867236575999399, -76.71811381506900318, 7.785367480540000606 ) ) ;
#988 = FACE_OUTER_BOUND ( 'NONE', #44636, .T. ) ;
#989 = CARTESIAN_POINT ( 'NONE',  ( -11.86109855473999986, -78.57731821575799813, -1.682380905046999997 ) ) ;
#990 = CARTESIAN_POINT ( 'NONE',  ( -12.70556836352000118, -62.02772277195000328, -2.424224025342999716E-09 ) ) ;
#991 = LINE ( 'NONE', #50567, #22240 ) ;
#992 = CARTESIAN_POINT ( 'NONE',  ( 1.577025133314267302, -2.911963968962991700, -3.150092931446307087 ) ) ;
#993 = CARTESIAN_POINT ( 'NONE',  ( 1.544981608555010544, -80.96391980284444401, 10.63828215852447023 ) ) ;
#994 = FACE_OUTER_BOUND ( 'NONE', #35902, .T. ) ;
#995 = CARTESIAN_POINT ( 'NONE',  ( 0.3402453830687809933, -86.10000000000019327, -7.595013698427217186 ) ) ;
#996 = CARTESIAN_POINT ( 'NONE',  ( 10.69210609810000001, -78.16394768316000352, 3.151740433137000252 ) ) ;
#997 = FACE_OUTER_BOUND ( 'NONE', #46850, .T. ) ;
#998 = CARTESIAN_POINT ( 'NONE',  ( 8.209261416751999718, -80.19853216860269640, 7.218337095169999884 ) ) ;
#999 = ORIENTED_EDGE ( 'NONE', *, *, #41614, .F. ) ;
#1000 = EDGE_CURVE ( 'NONE', #57298, #36426, #32062, .T. ) ;
#1001 = CARTESIAN_POINT ( 'NONE',  ( 0.000000000000000000, -77.49999999999998579, 0.000000000000000000 ) ) ;
#1002 = CARTESIAN_POINT ( 'NONE',  ( 2.352429030880999861, -3.130096044169000447, 3.193304126848000024 ) ) ;
#1003 = CARTESIAN_POINT ( 'NONE',  ( -6.984027423104000043, -77.12680175239600544, 8.777327129872999123 ) ) ;
#1004 = CARTESIAN_POINT ( 'NONE',  ( -10.81649518602000093, -79.29597897209099244, 1.862108609190000097 ) ) ;
#1005 = CARTESIAN_POINT ( 'NONE',  ( 9.422842877294000274, -25.25952027282999879, -8.643944052295999825 ) ) ;
#1006 = LINE ( 'NONE', #27243, #16655 ) ;
#1007 = CARTESIAN_POINT ( 'NONE',  ( 7.056385154380720337, -79.75000000000000000, -6.024759004142000940 ) ) ;
#1008 = CARTESIAN_POINT ( 'NONE',  ( -8.485281374238999419, -55.54999999966999980, -8.485281374238999419 ) ) ;
#1009 = B_SPLINE_SURFACE_WITH_KNOTS ( 'NONE', 3, 3, ( 
 ( #41246, #835, #14955, #14085, #50997, #55409, #41834, #15255, #51290, #32953, #10545, #23240, #10845, #4944, #28529, #46578, #551, #18817, #18528, #36809, #36520, #32082, #54828, #32369, #27942, #45990, #5516, #23526, #1120, #37099, #55115, #14659, #10249, #56001, #57149 ),
 ( #15842, #33544, #24983, #2847, #19990, #33830, #38269, #56576, #11141, #16714, #43004, #52155, #51868, #34696, #38560, #11422, #42713, #38847, #16135, #11712, #29115, #15550, #2561, #29401, #47454, #6980, #20562, #6693, #24411, #29688, #47738, #2279, #7271, #52725, #25272 ),
 ( #28820, #56866, #16425, #6396, #39138, #29975, #48027, #7560, #46869, #25560, #42427, #3696, #473, #49758, #45323, #17566, #9008, #57712, #44731, #36442, #22871, #21698, #49462, #12836, #4875, #54177, #9298, #26993, #53887, #45028, #58307, #27287, #4580, #26407, #40593 ),
 ( #32004, #18452, #35259, #4282, #44430, #27578, #3983, #39994, #39705, #54471, #53289, #17868, #40881, #26700, #14007, #21985, #50045, #58007, #13418, #30836, #17269, #9592, #35558, #48869, #18164, #22279, #8410, #31709, #53584, #13122, #31116, #8709, #49157, #188, #22580 ) ),
 .UNSPECIFIED., .F., .F., .F.,
 ( 4, 4 ),
 ( 4, 1, 1, 1, 1, 1, 1, 1, 1, 1, 1, 1, 1, 1, 1, 1, 1, 1, 1, 1, 1, 1, 1, 1, 1, 1, 1, 1, 1, 1, 1, 1, 4 ),
 ( -0.1566102636784000024, 1.156610263678000017 ),
 ( -0.02000000000000000042, 0.01250000000000000069, 0.04499999999999999833, 0.07749999999999999944, 0.1100000000000000006, 0.1424999999999999878, 0.1749999999999999889, 0.2074999999999999900, 0.2399999999999999911, 0.2725000000000000200, 0.3049999999999999933, 0.3375000000000000222, 0.3699999999999999956, 0.4025000000000000244, 0.4349999999999999978, 0.4675000000000000266, 0.5000000000000000000, 0.5324999999999999734, 0.5649999999999999467, 0.5975000000000000311, 0.6300000000000000044, 0.6624999999999999778, 0.6949999999999999512, 0.7275000000000000355, 0.7600000000000000089, 0.7924999999999999822, 0.8249999999999999556, 0.8575000000000000400, 0.8900000000000000133, 0.9224999999999999867, 0.9549999999999999600, 0.9875000000000000444, 1.020000000000000018 ),
 .UNSPECIFIED. ) ;
#1010 = CIRCLE ( 'NONE', #13211, 1.250000000000000444 ) ;
#1011 = CARTESIAN_POINT ( 'NONE',  ( 12.00000000000000000, -23.15000000000000213, -0.5999999999999999778 ) ) ;
#1012 = VECTOR ( 'NONE', #4692, 1000.000000000000114 ) ;
#1013 = CARTESIAN_POINT ( 'NONE',  ( -10.48774103543000180, -21.75472018390999907, -7.686941364778000718 ) ) ;
#1014 = EDGE_CURVE ( 'NONE', #4724, #21904, #41618, .T. ) ;
#1016 = ADVANCED_FACE ( 'NONE', ( #23425 ), #43407, .T. ) ;
#1015 = CARTESIAN_POINT ( 'NONE',  ( 9.414496040419999545, -53.53736393982000408, -8.652369398682999702 ) ) ;
#1017 = CARTESIAN_POINT ( 'NONE',  ( 8.229676506584999274, -77.58638398095499156, 7.688067972860000765 ) ) ;
#1018 = CARTESIAN_POINT ( 'NONE',  ( -0.8981901762082999952, -79.79086109591999332, -1.403037214508999986 ) ) ;
#1019 = CARTESIAN_POINT ( 'NONE',  ( 0.06763567127574998672, -79.64895916143998988, -1.247532485737999908 ) ) ;
#1020 = CARTESIAN_POINT ( 'NONE',  ( -9.596002108778161954, -79.35208333333332575, -7.374560639698982456 ) ) ;
#1021 = CARTESIAN_POINT ( 'NONE',  ( 0.6046126565052558632, -81.40785622595326743, -1.385375599882785025 ) ) ;
#1022 = CARTESIAN_POINT ( 'NONE',  ( -1.181111693982000110, -79.27654225787900089, -0.4092372983238000139 ) ) ;
#1023 = CARTESIAN_POINT ( 'NONE',  ( -5.970525758963701080, -80.17821961223123139, -8.939477884329102508 ) ) ;
#1024 = CARTESIAN_POINT ( 'NONE',  ( 9.252740428349003565, -78.02916666666668277, -2.486604901413146607 ) ) ;
#1025 = VERTEX_POINT ( 'NONE', #19004 ) ;
#1026 = CARTESIAN_POINT ( 'NONE',  ( -0.8193159871064622513, -81.66856760969551488, -0.9439107478074511004 ) ) ;
#1027 =( NAMED_UNIT ( * ) SI_UNIT ( $, .STERADIAN. ) SOLID_ANGLE_UNIT ( ) );
#1028 = CARTESIAN_POINT ( 'NONE',  ( -10.27879708628000088, -78.85952198136099867, 4.312879667924000238 ) ) ;
#1029 = CARTESIAN_POINT ( 'NONE',  ( -0.7999999999999001243, -23.15000000002000036, 12.00000000000000000 ) ) ;
#1030 = ORIENTED_EDGE ( 'NONE', *, *, #26943, .F. ) ;
#1031 = EDGE_LOOP ( 'NONE', ( #26691, #45091, #56194 ) ) ;
#1032 = CARTESIAN_POINT ( 'NONE',  ( -0.6920646488899999671, -81.51826673532400491, 1.237378641307999905 ) ) ;
#1033 = VERTEX_POINT ( 'NONE', #32844 ) ;
#1034 = B_SPLINE_CURVE_WITH_KNOTS ( 'NONE', 3,
 ( #49375, #18950, #54094, #41384, #54954, #14506, #40408, #3520, #4396, #22091, #26235, #52821, #30938, #21521, #13236, #12660, #58118 ),
 .UNSPECIFIED., .F., .F.,
 ( 4, 2, 1, 2, 2, 2, 2, 2, 4 ),
 ( 0.000000000000000000, 0.1250000000000000278, 0.2500000000000000555, 0.3750000000000001110, 0.5000000000000001110, 0.6250000000000001110, 0.7500000000000002220, 0.8750000000000002220, 1.000000000000000000 ),
 .UNSPECIFIED. ) ;
#1035 = ORIENTED_EDGE ( 'NONE', *, *, #29087, .T. ) ;
#1036 = DIRECTION ( 'NONE',  ( -0.7071067811865474617, 0.000000000000000000, -0.7071067811865474617 ) ) ;
#1037 = FACE_OUTER_BOUND ( 'NONE', #4709, .T. ) ;
#1038 = CARTESIAN_POINT ( 'NONE',  ( 0.6175300363197693265, -81.28229165379221399, 3.388491480252034282 ) ) ;
#1039 = CARTESIAN_POINT ( 'NONE',  ( -0.5475862000146000108, -78.94131001420200278, -10.00738244094000073 ) ) ;
#1040 = CARTESIAN_POINT ( 'NONE',  ( 6.432069509746887626, -78.28619479064511211, -6.649389305992823296 ) ) ;
#1041 = LINE ( 'NONE', #37019, #38264 ) ;
#1042 = VERTEX_POINT ( 'NONE', #55012 ) ;
#1043 = VERTEX_POINT ( 'NONE', #41143 ) ;
#1044 = AXIS2_PLACEMENT_3D ( 'NONE', #18633, #54064, #19210 ) ;
#1045 = CARTESIAN_POINT ( 'NONE',  ( -1.733997378023027114, -18.47616783230456861, -12.54437956612009764 ) ) ;
#1046 = CARTESIAN_POINT ( 'NONE',  ( 0.7554284705563453217, -79.33333333333334281, 1.310679582531389276 ) ) ;
#1047 = CARTESIAN_POINT ( 'NONE',  ( 0.2494208068450905480, -17.00711039237138422, 12.50614183113019529 ) ) ;
#1048 = AXIS2_PLACEMENT_3D ( 'NONE', #52317, #57594, #33995 ) ;
#1049 = CARTESIAN_POINT ( 'NONE',  ( 4.545264886168000729, -77.60605771026999378, 8.573871732259998879 ) ) ;
#1050 = DIRECTION ( 'NONE',  ( -1.000000000000000000, 0.000000000000000000, 0.000000000000000000 ) ) ;
#1051 = CARTESIAN_POINT ( 'NONE',  ( -0.7770281622696295631, -85.98458445108748549, 3.914531931580598645 ) ) ;
#1052 = CARTESIAN_POINT ( 'NONE',  ( 5.488127745643000210, -77.17119367106998595, 11.56242237764000080 ) ) ;
#1053 = CARTESIAN_POINT ( 'NONE',  ( 0.6229729438976999711, -81.04952822830999537, 1.458184003450999855 ) ) ;
#1054 = CARTESIAN_POINT ( 'NONE',  ( -9.221371799403371483, -77.06727193750342053, -2.052095926117649682 ) ) ;
#1055 = CARTESIAN_POINT ( 'NONE',  ( 4.163357712510999953, -79.52423699984079519, 0.3099401135692000375 ) ) ;
#1056 = CARTESIAN_POINT ( 'NONE',  ( 11.02326530841000007, -81.02459481428599020, 1.187788371667000131 ) ) ;
#1057 = CARTESIAN_POINT ( 'NONE',  ( -7.459109567305000077, -79.06303667140099378, -6.354485205484000865 ) ) ;
#1058 = CYLINDRICAL_SURFACE ( 'NONE', #386, 12.00000000000000000 ) ;
#1059 = CARTESIAN_POINT ( 'NONE',  ( 3.098607378237295595, -76.14114583267888747, -11.53327867144136043 ) ) ;
#1060 = CARTESIAN_POINT ( 'NONE',  ( 0.9384621721472999889, -78.57854477868900744, 0.9475573338641000154 ) ) ;
#1061 = DIRECTION ( 'NONE',  ( -1.000000000000000000, 0.000000000000000000, 0.000000000000000000 ) ) ;
#1062 = DIRECTION ( 'NONE',  ( 0.000000000000000000, 0.000000000000000000, 1.000000000000000000 ) ) ;
#1063 = CARTESIAN_POINT ( 'NONE',  ( -0.3113020967593000399, -2.698849349032999889, 3.793306396812999637 ) ) ;
#1064 = CARTESIAN_POINT ( 'NONE',  ( -1.250000000000000000, -79.00000000000000000, 0.000000000000000000 ) ) ;
#1065 = B_SPLINE_CURVE_WITH_KNOTS ( 'NONE', 3,
 ( #13567, #49605, #16421, #24978, #38844, #21128, #30263, #34404, #16710, #29972, #33825, #29683, #34692, #38265, #33540, #29398, #51864, #11709, #47158 ),
 .UNSPECIFIED., .F., .F.,
 ( 4, 1, 1, 1, 1, 1, 1, 1, 1, 1, 1, 1, 1, 1, 1, 1, 4 ),
 ( 0.000000000000000000, 0.04500013125675292325, 0.1100001148193760075, 0.1750000983819555711, 0.2400000819445786693, 0.3050000655072017119, 0.3700000490698248656, 0.4350000326324479638, 0.5000000161948968680, 0.5649999997576505839, 0.6299999833204042998, 0.6949999668831581268, 0.7599999504454763022, 0.8249999340082300181, 0.8899999175709837340, 0.9549999011333020205, 1.000000000000000000 ),
 .UNSPECIFIED. ) ;
#1066 = VERTEX_POINT ( 'NONE', #5137 ) ;
#1067 = CARTESIAN_POINT ( 'NONE',  ( -1.230457122653977109, -78.91666666666665719, -11.75000000000022737 ) ) ;
#1068 = EDGE_CURVE ( 'NONE', #47711, #11745, #22843, .T. ) ;
#1069 = CARTESIAN_POINT ( 'NONE',  ( 7.555116226634086551, -60.48684619743404056, -7.995796640818108258 ) ) ;
#1070 = FACE_BOUND ( 'NONE', #30736, .T. ) ;
#1071 = CIRCLE ( 'NONE', #52915, 4.000000000000000000 ) ;
#1072 = CARTESIAN_POINT ( 'NONE',  ( -0.09271117443256000901, -79.70494298055800186, 9.750963687110999700 ) ) ;
#1073 = CARTESIAN_POINT ( 'NONE',  ( 12.50409217856652511, -17.47871355535288629, -1.233808107085542449 ) ) ;
#1074 = CARTESIAN_POINT ( 'NONE',  ( 7.189755216797094839, -79.41669502080303289, 7.992951545765084376 ) ) ;
#1075 = CARTESIAN_POINT ( 'NONE',  ( -8.895437731725001740, -79.41463998579799011, -4.226908468493999038 ) ) ;
#1076 = CARTESIAN_POINT ( 'NONE',  ( 8.356119038218036366, -78.50935930058759027, 8.269166890618505406 ) ) ;
#1077 = DIRECTION ( 'NONE',  ( 0.000000000000000000, 0.000000000000000000, -1.000000000000000000 ) ) ;
#1078 = CARTESIAN_POINT ( 'NONE',  ( 4.884263559594000270, -77.83984273478799309, -10.16119218727999929 ) ) ;
#1079 = EDGE_CURVE ( 'NONE', #43122, #24529, #36790, .T. ) ;
#1080 = CARTESIAN_POINT ( 'NONE',  ( 0.2104032054905000115, -81.54352552975799995, -1.590243660542000059 ) ) ;
#1081 = CARTESIAN_POINT ( 'NONE',  ( 0.7999999997951999786, -18.85000000927000130, -11.99999999979999821 ) ) ;
#1082 = AXIS2_PLACEMENT_3D ( 'NONE', #46716, #41673, #6235 ) ;
#1083 = CARTESIAN_POINT ( 'NONE',  ( 3.151000900302999952, -78.36865170860198759, 8.870309342620000592 ) ) ;
#1085 = CARTESIAN_POINT ( 'NONE',  ( 3.165411199172024848, -2.770833333333333481, 0.8506806241676669877 ) ) ;
#1084 = CARTESIAN_POINT ( 'NONE',  ( 3.835477222130000197, -83.58453969748799750, -0.9975492235297998000 ) ) ;
#1086 = CARTESIAN_POINT ( 'NONE',  ( 12.00000000000000000, -76.64999999999999147, 0.000000000000000000 ) ) ;
#1087 = CARTESIAN_POINT ( 'NONE',  ( -1.092232985442822102, -82.54166666666664298, -0.6295237254636245616 ) ) ;
#1088 = CARTESIAN_POINT ( 'NONE',  ( 0.000000000000000000, -80.99999999999998579, 0.000000000000000000 ) ) ;
#1089 = CARTESIAN_POINT ( 'NONE',  ( -10.75033332359620708, -77.11068282368783855, -1.411355356088692670 ) ) ;
#1090 = CARTESIAN_POINT ( 'NONE',  ( -1.417334032777999964, -79.42654225787899236, -0.4910847579886000736 ) ) ;
#1091 = AXIS2_PLACEMENT_3D ( 'NONE', #18206, #13750, #55665 ) ;
#1092 = CARTESIAN_POINT ( 'NONE',  ( -3.999999999999815259, -78.72610001270986402, -1.678385095468384722E-14 ) ) ;
#1093 = ORIENTED_EDGE ( 'NONE', *, *, #15590, .T. ) ;
#1094 = ORIENTED_EDGE ( 'NONE', *, *, #7570, .F. ) ;
#1095 = CARTESIAN_POINT ( 'NONE',  ( 6.536979956083999177, -79.30461158636299501, -10.09826910480999906 ) ) ;
#1096 = CARTESIAN_POINT ( 'NONE',  ( 1.249999992656000147, -76.50000000027618796, -0.4999999997238000482 ) ) ;
#1097 = DIRECTION ( 'NONE',  ( 0.000000000000000000, -1.000000000000000000, 0.000000000000000000 ) ) ;
#1098 = ORIENTED_EDGE ( 'NONE', *, *, #44386, .F. ) ;
#1099 = CARTESIAN_POINT ( 'NONE',  ( 11.66178877871000097, -78.39045805696299851, 2.537357863477000208 ) ) ;
#1100 = EDGE_CURVE ( 'NONE', #27284, #51275, #44330, .T. ) ;
#1101 = VERTEX_POINT ( 'NONE', #40564 ) ;
#1102 = EDGE_LOOP ( 'NONE', ( #2121, #31598, #23793, #22455 ) ) ;
#1103 = EDGE_LOOP ( 'NONE', ( #58066, #39904, #42472, #9931 ) ) ;
#1104 = CARTESIAN_POINT ( 'NONE',  ( -3.480702090310999974, -78.73368213548980066, -0.6826041573473999868 ) ) ;
#1105 = CARTESIAN_POINT ( 'NONE',  ( -8.343860018000999190, -60.54999999966955926, 8.343860018000999190 ) ) ;
#1106 = ORIENTED_EDGE ( 'NONE', *, *, #18235, .F. ) ;
#1107 = CARTESIAN_POINT ( 'NONE',  ( 1.228744581380641687, -82.83562427784806914, -0.2287525698557267839 ) ) ;
#1108 = CIRCLE ( 'NONE', #35958, 5.000000000000000000 ) ;
#1109 = ORIENTED_EDGE ( 'NONE', *, *, #57711, .T. ) ;
#1110 = CARTESIAN_POINT ( 'NONE',  ( -10.75000000000000000, -80.50000000000000000, -1.711887504597999906E-14 ) ) ;
#1111 = CARTESIAN_POINT ( 'NONE',  ( 6.983681292383111305, -78.53882967120196668, -6.738102358712994011 ) ) ;
#1112 = CARTESIAN_POINT ( 'NONE',  ( 2.318769295210185710, -78.77851881763733388, -4.014936526035610243 ) ) ;
#1113 = LINE ( 'NONE', #19098, #19955 ) ;
#1114 = CARTESIAN_POINT ( 'NONE',  ( 9.776276929627000456, -75.90796407085099418, -5.431214116490000521 ) ) ;
#1115 = DIRECTION ( 'NONE',  ( 0.000000000000000000, -1.000000000000000000, 0.000000000000000000 ) ) ;
#1116 = CARTESIAN_POINT ( 'NONE',  ( -7.641012386020999969, -55.51082434643999619, -10.18589234707000202 ) ) ;
#1117 = CARTESIAN_POINT ( 'NONE',  ( 0.3203968975889366910, -78.72793535945164933, -9.244731248301008009 ) ) ;
#1118 = CARTESIAN_POINT ( 'NONE',  ( 2.296255511297609964, -76.55894423758236655, 11.52317862450651198 ) ) ;
#1119 = CARTESIAN_POINT ( 'NONE',  ( 9.515085579998999066, -77.75946167140099874, 0.3080020932329999850 ) ) ;
#1120 = CARTESIAN_POINT ( 'NONE',  ( 0.6343572851480000496, -80.46989121764299568, 1.173101423079000005 ) ) ;
#1121 = CARTESIAN_POINT ( 'NONE',  ( -9.147467037885974150, -80.14699925185365714, -6.109202993256466208 ) ) ;
#1122 = CARTESIAN_POINT ( 'NONE',  ( 11.23426925451733283, -78.17300239647218518, -4.441224278447778673 ) ) ;
#1123 = CARTESIAN_POINT ( 'NONE',  ( -3.617957113613000431, -78.32128455456849281, 1.158813396440000032 ) ) ;
#1124 = VECTOR ( 'NONE', #51841, 1000.000000000000000 ) ;
#1125 = CARTESIAN_POINT ( 'NONE',  ( -1.750000000001000089, -55.54999998977000075, 12.56594317853999954 ) ) ;
#1126 = CARTESIAN_POINT ( 'NONE',  ( -0.4851089960429650905, -83.00678479282305489, 1.152015161174709146 ) ) ;
#1127 = DIRECTION ( 'NONE',  ( 0.000000000000000000, 0.000000000000000000, 1.000000000000000000 ) ) ;
#1128 = CARTESIAN_POINT ( 'NONE',  ( 0.5515549627219517026, -82.09100159915311679, 1.204941737300085691 ) ) ;
#1129 = CARTESIAN_POINT ( 'NONE',  ( 9.499693205731109202, -80.00008708754018016, -1.997583897032410100E-06 ) ) ;
#1130 = CARTESIAN_POINT ( 'NONE',  ( 6.100000000000000533, -80.79999999999999716, 0.000000000000000000 ) ) ;
#1131 = EDGE_CURVE ( 'NONE', #31999, #28960, #48632, .T. ) ;
#1132 = CARTESIAN_POINT ( 'NONE',  ( 10.38645071868999992, -56.02180874340999850, 7.655542440077000244 ) ) ;
#1134 = EDGE_CURVE ( 'NONE', #37723, #31238, #6712, .T. ) ;
#1133 = CARTESIAN_POINT ( 'NONE',  ( 0.1624548541070857943, -79.48286375057362818, -1.504788102669172734 ) ) ;
#1135 = DIRECTION ( 'NONE',  ( 0.000000000000000000, 1.000000000000000000, 0.000000000000000000 ) ) ;
#1136 = CARTESIAN_POINT ( 'NONE',  ( 4.009386773507102042, -79.41013248972129190, -8.520383303337226266 ) ) ;
#1137 = CARTESIAN_POINT ( 'NONE',  ( -7.864802647417423742, -24.45123893519480163, -10.10444599041134417 ) ) ;
#1138 = CARTESIAN_POINT ( 'NONE',  ( 10.68454778250440640, -77.21060221147246239, 1.377222071623238620 ) ) ;
#1139 = LINE ( 'NONE', #27384, #57130 ) ;
#1141 = CARTESIAN_POINT ( 'NONE',  ( -2.928603948516999900, -78.74649347130959143, 10.57767911663000149 ) ) ;
#1140 = CARTESIAN_POINT ( 'NONE',  ( 2.065550207748000133, -60.22565079297999802, 12.82162303857000119 ) ) ;
#1142 = CARTESIAN_POINT ( 'NONE',  ( -11.56077433994999915, -76.14243477331000065, 3.934723564722999445 ) ) ;
#1143 = ORIENTED_EDGE ( 'NONE', *, *, #46270, .T. ) ;
#1144 = CARTESIAN_POINT ( 'NONE',  ( -2.892792818793000542, -85.03957450217399128, -2.124967581011000028 ) ) ;
#1145 = CARTESIAN_POINT ( 'NONE',  ( -10.20620196243999978, -80.81341270350478112, -5.091275341613999750 ) ) ;
#1146 = EDGE_CURVE ( 'NONE', #4486, #43269, #17668, .T. ) ;
#1147 =( GEOMETRIC_REPRESENTATION_CONTEXT ( 3 ) GLOBAL_UNCERTAINTY_ASSIGNED_CONTEXT ( ( #42560 ) ) GLOBAL_UNIT_ASSIGNED_CONTEXT ( ( #602, #9716, #54595 ) ) REPRESENTATION_CONTEXT ( 'NONE', 'WORKASPACE' ) );
#1148 = CARTESIAN_POINT ( 'NONE',  ( 8.244325742278693525, -78.31259323136428918, -4.194771269908470934 ) ) ;
#1149 = FACE_OUTER_BOUND ( 'NONE', #35371, .T. ) ;
#1150 = CARTESIAN_POINT ( 'NONE',  ( 10.79417609527999922, -77.62976718524500086, -3.050225076229999832 ) ) ;
#1151 = CARTESIAN_POINT ( 'NONE',  ( 12.43645963087999995, -53.88248289507999544, 0.05235777564056001004 ) ) ;
#1152 = CARTESIAN_POINT ( 'NONE',  ( 1.867960828343000035, -78.75252915135698117, 9.447959161044998666 ) ) ;
#1153 = DIRECTION ( 'NONE',  ( 0.000000000000000000, -1.000000000000000000, 0.000000000000000000 ) ) ;
#1154 = CARTESIAN_POINT ( 'NONE',  ( 4.000000000000000000, -78.69999999999998863, 0.000000000000000000 ) ) ;
#1155 = CARTESIAN_POINT ( 'NONE',  ( 1.147008568205678536, -76.09166666666237688, 10.95833333328629067 ) ) ;
#1156 = ORIENTED_EDGE ( 'NONE', *, *, #53762, .F. ) ;
#1157 = CARTESIAN_POINT ( 'NONE',  ( 1.980611416588874185, -55.27402268162217780, -12.74335092660349389 ) ) ;
#1158 = CARTESIAN_POINT ( 'NONE',  ( 6.052764987364000149, -79.37291332859899740, -7.354162135516000731 ) ) ;
#1159 = CARTESIAN_POINT ( 'NONE',  ( 0.000000000000000000, -87.64999999984398471, 0.000000000000000000 ) ) ;
#1160 = EDGE_LOOP ( 'NONE', ( #26593, #42845, #38961, #39472 ) ) ;
#1161 = CARTESIAN_POINT ( 'NONE',  ( 1.500000000000000000, -78.64999999999999147, 0.000000000000000000 ) ) ;
#1162 = DIRECTION ( 'NONE',  ( 0.000000000000000000, -1.000000000000000000, 5.958196898821999917E-14 ) ) ;
#1163 = ORIENTED_EDGE ( 'NONE', *, *, #16816, .F. ) ;
#1164 = CARTESIAN_POINT ( 'NONE',  ( 2.263099670254000273, -78.11897245443199722, 11.95244370277000101 ) ) ;
#1165 = CARTESIAN_POINT ( 'NONE',  ( -11.07550907487999936, -77.92372890012597964, 0.7607607059370000702 ) ) ;
#1166 = CARTESIAN_POINT ( 'NONE',  ( 8.838834764832000701, -55.54999999966999980, -8.838834764832000701 ) ) ;
#1167 = AXIS2_PLACEMENT_3D ( 'NONE', #42050, #50336, #23163 ) ;
#1168 = ORIENTED_EDGE ( 'NONE', *, *, #49819, .F. ) ;
#1169 = AXIS2_PLACEMENT_3D ( 'NONE', #31596, #41353, #13599 ) ;
#1170 = ORIENTED_EDGE ( 'NONE', *, *, #30015, .T. ) ;
#1171 = CARTESIAN_POINT ( 'NONE',  ( 12.50728630770444560, -24.99975539312146822, -0.1757873578727420505 ) ) ;
#1172 = CARTESIAN_POINT ( 'NONE',  ( 9.523132023602000729, -80.26946618684752366, 1.108936319727999997 ) ) ;
#1173 = VERTEX_POINT ( 'NONE', #7578 ) ;
#1174 = CARTESIAN_POINT ( 'NONE',  ( 12.44180763921999855, -54.70743932605000026, 1.459474665415000150 ) ) ;
#1175 = CARTESIAN_POINT ( 'NONE',  ( 8.586577278446998918, -79.87637572403669139, 6.741381070085999738 ) ) ;
#1176 = CARTESIAN_POINT ( 'NONE',  ( -12.61117499582000079, -23.21550664553999965, -1.798980867984000032 ) ) ;
#1177 = CARTESIAN_POINT ( 'NONE',  ( -9.204193785523999694, -77.14980194988498852, -2.332437886131999871 ) ) ;
#1178 = EDGE_CURVE ( 'NONE', #29062, #16887, #38796, .T. ) ;
#1179 = DIRECTION ( 'NONE',  ( 0.000000000000000000, -1.000000000000000000, 0.000000000000000000 ) ) ;
#1180 = CARTESIAN_POINT ( 'NONE',  ( -1.190204951956445267, -80.12538959866201083, -0.3913796594779095916 ) ) ;
#1181 = CARTESIAN_POINT ( 'NONE',  ( 0.9935076046793005489, -17.03183812245195483, -12.70250268216991962 ) ) ;
#1182 = CARTESIAN_POINT ( 'NONE',  ( -10.31421052434999908, -76.72175206120299151, 3.823226550887000030 ) ) ;
#1183 = CARTESIAN_POINT ( 'NONE',  ( 9.707557378189999753, -77.00399869373629258, -2.082535605504000298 ) ) ;
#1184 = CARTESIAN_POINT ( 'NONE',  ( -0.7887420553019258707, -78.26716755245251989, 1.320791577295096442 ) ) ;
#1185 = CARTESIAN_POINT ( 'NONE',  ( -1.618935784642312470, -23.92751168673102669, 12.52134385800258798 ) ) ;
#1186 = VERTEX_POINT ( 'NONE', #51887 ) ;
#1187 = CARTESIAN_POINT ( 'NONE',  ( -9.662446363796000526, -76.46415837332999388, 7.627099640079999965 ) ) ;
#1188 = CARTESIAN_POINT ( 'NONE',  ( -10.75000000000000000, -77.51041666666665719, -1.407171709420429018 ) ) ;
#1189 = B_SPLINE_CURVE_WITH_KNOTS ( 'NONE', 3,
 ( #4361, #44223, #31494, #12630, #4058, #30626, #12911, #35936, #45113, #4665, #39201, #13202, #3772, #57216, #30910, #48944, #22062, #31197, #22957, #40968, #36237, #32377, #54552, #41256, #23533, #50420, #18826, #46292, #19408, #1128, #19117, #55417, #37107, #559, #54260 ),
 .UNSPECIFIED., .F., .F.,
 ( 4, 1, 1, 1, 1, 1, 1, 1, 1, 1, 1, 1, 1, 1, 1, 1, 1, 1, 1, 1, 1, 1, 1, 1, 1, 1, 1, 1, 1, 1, 1, 1, 4 ),
 ( 0.000000000000000000, 0.01250524777966226068, 0.04500492809905208558, 0.07750460841844190873, 0.1100042887377895434, 0.1425039690572004469, 0.1750036493766114198, 0.2075033296960223372, 0.2400030100154332546, 0.2725026903347386731, 0.3050023706541495905, 0.3375020509735605079, 0.3700017312929714808, 0.4025014116123823427, 0.4350010919316877334, 0.4675007722510986508, 0.5000004525705096237, 0.5325001328899204855, 0.5649998132093314585, 0.5974994935287424314, 0.6299991738480477110, 0.6624988541674586839, 0.6949985344868696568, 0.7274982148062805187, 0.7599978951256914916, 0.7924975754449967713, 0.8249972557644078552, 0.8574969360838187171, 0.8899966164032295790, 0.9224962967226405519, 0.9549959770419459426, 0.9874956573613570265, 1.000000000000000000 ),
 .UNSPECIFIED. ) ;
#1190 = CARTESIAN_POINT ( 'NONE',  ( -3.184394476902560722, -2.314159630480875141, 1.502279350439443606 ) ) ;
#1191 = CARTESIAN_POINT ( 'NONE',  ( 7.647735717269999789, -60.52294882350999927, -10.13404777204000062 ) ) ;
#1192 = CARTESIAN_POINT ( 'NONE',  ( 7.914613980750001332, -79.36968659573999219, 9.019916049260999102 ) ) ;
#1193 = CARTESIAN_POINT ( 'NONE',  ( 10.16964605767000052, -76.26874748315199781, -6.884832982024000181 ) ) ;
#1194 = DIRECTION ( 'NONE',  ( -1.000000000000000000, 0.000000000000000000, 0.000000000000000000 ) ) ;
#1195 = DIRECTION ( 'NONE',  ( 0.7071067811865475727, 0.000000000000000000, -0.7071067811865475727 ) ) ;
#1196 = CARTESIAN_POINT ( 'NONE',  ( -8.811774560614452412, -78.10987123251830155, -8.257849517617557922 ) ) ;
#1197 = CARTESIAN_POINT ( 'NONE',  ( -6.324515969367999979, -78.82733126974268600, -9.263833350438000380 ) ) ;
#1198 = ORIENTED_EDGE ( 'NONE', *, *, #12691, .T. ) ;
#1200 = EDGE_CURVE ( 'NONE', #35836, #20895, #57455, .T. ) ;
#1199 = CARTESIAN_POINT ( 'NONE',  ( 0.4274279416557000277, -83.36936459712099179, 1.281884980902999960 ) ) ;
#1201 = CARTESIAN_POINT ( 'NONE',  ( -3.075537641221531615, -77.90416666666671119, -11.44417895085270942 ) ) ;
#1202 = CARTESIAN_POINT ( 'NONE',  ( 9.841120606706802221, -24.83627250047061352, 8.121699444506939258 ) ) ;
#1203 = AXIS2_PLACEMENT_3D ( 'NONE', #10695, #42275, #13936 ) ;
#1204 = CYLINDRICAL_SURFACE ( 'NONE', #30513, 9.500000000000000000 ) ;
#1205 = CARTESIAN_POINT ( 'NONE',  ( 1.785023577804000228, -3.459384265120000190, -3.219039020423000164 ) ) ;
#1206 = CARTESIAN_POINT ( 'NONE',  ( 10.75624577990000041, -78.22165355494099970, -5.431293436759999871 ) ) ;
#1207 = CARTESIAN_POINT ( 'NONE',  ( -2.552693750765000047, -78.31059042997900121, -9.286385980553001573 ) ) ;
#1208 = CARTESIAN_POINT ( 'NONE',  ( 1.986041313562282973, -76.06139900838468293, 11.58506530393337286 ) ) ;
#1209 = CARTESIAN_POINT ( 'NONE',  ( -1.288646058034000008, -83.05573296103600001, 0.4058063692239000098 ) ) ;
#1210 = CARTESIAN_POINT ( 'NONE',  ( 4.020839152126976401, -85.88547957940600952, 0.4615274515358095964 ) ) ;
#1211 = ORIENTED_EDGE ( 'NONE', *, *, #32322, .T. ) ;
#1212 = CARTESIAN_POINT ( 'NONE',  ( 1.343749999883000035, -77.90625000011999646, 3.156563468101999814E-09 ) ) ;
#1213 = CIRCLE ( 'NONE', #8729, 9.499999999999996447 ) ;
#1214 = CARTESIAN_POINT ( 'NONE',  ( 4.658318423525466656, -77.93349885897991669, 8.082338094468221712 ) ) ;
#1215 = EDGE_CURVE ( 'NONE', #44340, #8841, #2830, .T. ) ;
#1216 = CARTESIAN_POINT ( 'NONE',  ( 0.000000000000000000, -46.43897132165000130, 0.000000000000000000 ) ) ;
#1217 = CARTESIAN_POINT ( 'NONE',  ( -5.755176823513999729, -78.40937828446098479, 9.345691860246999383 ) ) ;
#1218 = EDGE_CURVE ( 'NONE', #30942, #41447, #16073, .T. ) ;
#1219 = CARTESIAN_POINT ( 'NONE',  ( 6.758989304250999197, -77.04505930305400341, -10.14916591256000089 ) ) ;
#1220 = CARTESIAN_POINT ( 'NONE',  ( 1.062167859419960614, -79.30478719906479057, -0.6841706396682687430 ) ) ;
#1221 = CARTESIAN_POINT ( 'NONE',  ( 8.950130560568000604, -16.79887407354000217, -8.958576480220999727 ) ) ;
#1222 = CARTESIAN_POINT ( 'NONE',  ( -7.714303428875997959, -63.10294702886003648, -12.53545825868000385 ) ) ;
#1223 = ORIENTED_EDGE ( 'NONE', *, *, #43625, .T. ) ;
#1224 = AXIS2_PLACEMENT_3D ( 'NONE', #7015, #33862, #6432 ) ;
#1225 = CARTESIAN_POINT ( 'NONE',  ( -2.299999999264999762, -77.49999999927000260, -2.080610052828999912E-10 ) ) ;
#1226 = CARTESIAN_POINT ( 'NONE',  ( -11.77076513002849012, -79.55082450634814961, -0.1443961957164959509 ) ) ;
#1227 = CARTESIAN_POINT ( 'NONE',  ( -1.720923278860959860, -77.83943615250160519, 11.89782049558834487 ) ) ;
#1228 = CIRCLE ( 'NONE', #34175, 0.5000000000000006661 ) ;
#1229 = CARTESIAN_POINT ( 'NONE',  ( -1.143190144809757669, -81.56692634864619151, 0.5063306831769307514 ) ) ;
#1230 = B_SPLINE_CURVE_WITH_KNOTS ( 'NONE', 3,
 ( #22828, #141, #18409, #57669, #53244, #53839, #17225, #26948, #36401, #54129, #35214, #44981, #40248, #35809, #35510, #13670, #31666, #12793 ),
 .UNSPECIFIED., .F., .F.,
 ( 4, 2, 2, 2, 2, 2, 2, 2, 4 ),
 ( 0.000000000000000000, 0.1250000000000000833, 0.2500000000000001665, 0.3750000000000002220, 0.5000000000000002220, 0.6250000000000002220, 0.7500000000000001110, 0.8750000000000001110, 1.000000000000000000 ),
 .UNSPECIFIED. ) ;
#1231 = CARTESIAN_POINT ( 'NONE',  ( 0.000000000000000000, -77.19999999999998863, 0.000000000000000000 ) ) ;
#1232 = CARTESIAN_POINT ( 'NONE',  ( 1.249999993052000047, -76.30000000069199473, 0.6999999993075000093 ) ) ;
#1233 = EDGE_CURVE ( 'NONE', #47045, #42541, #31119, .T. ) ;
#1234 = CARTESIAN_POINT ( 'NONE',  ( -1.280405559996000031, -78.59639078104000021, -0.2671032044805999872 ) ) ;
#1235 = CARTESIAN_POINT ( 'NONE',  ( 9.393203674808260573, -79.29166666666665719, 5.413904038987188194 ) ) ;
#1236 = CARTESIAN_POINT ( 'NONE',  ( 9.694993915875986801, -79.66127398716234609, -5.145377715137363417 ) ) ;
#1237 = LINE ( 'NONE', #18653, #57315 ) ;
#1238 = ORIENTED_EDGE ( 'NONE', *, *, #38746, .F. ) ;
#1239 = VERTEX_POINT ( 'NONE', #21149 ) ;
#1240 = CARTESIAN_POINT ( 'NONE',  ( 6.874531804813999614, -78.06448998579800502, -7.293035489291000317 ) ) ;
#1241 = CARTESIAN_POINT ( 'NONE',  ( 6.122270975308672369, -78.77338805014832701, -8.836258741097333669 ) ) ;
#1242 = EDGE_LOOP ( 'NONE', ( #57133, #25375, #53679, #42631 ) ) ;
#1243 = LINE ( 'NONE', #28361, #50083 ) ;
#1244 = CARTESIAN_POINT ( 'NONE',  ( 0.8378965770218049780, -83.63333334673063746, -3.340896199513284870 ) ) ;
#1245 = EDGE_CURVE ( 'NONE', #20659, #25961, #47754, .T. ) ;
#1246 = CARTESIAN_POINT ( 'NONE',  ( -8.428125188755409170, -79.36138179854771124, 4.406741964346048590 ) ) ;
#1247 = EDGE_CURVE ( 'NONE', #50686, #10829, #57163, .T. ) ;
#1248 = CARTESIAN_POINT ( 'NONE',  ( 7.753906807064999462, -61.08933445950000163, 10.31979621052999896 ) ) ;
#1249 = CARTESIAN_POINT ( 'NONE',  ( 8.190859204290999784, -55.64999999967000122, -7.342331066867000544 ) ) ;
#1250 = CARTESIAN_POINT ( 'NONE',  ( 8.049776716670494991, -77.23386658315779130, -8.806146062382781636 ) ) ;
#1251 = AXIS2_PLACEMENT_3D ( 'NONE', #2632, #56072, #6466 ) ;
#1252 = CARTESIAN_POINT ( 'NONE',  ( -7.301194973305000779, -79.19750906795999867, 8.515319286630999684 ) ) ;
#1253 = VERTEX_POINT ( 'NONE', #11443 ) ;
#1254 = DIRECTION ( 'NONE',  ( 0.000000000000000000, -1.000000000000000000, 0.000000000000000000 ) ) ;
#1255 = VERTEX_POINT ( 'NONE', #57739 ) ;
#1256 = CARTESIAN_POINT ( 'NONE',  ( 8.765487326333861517, -77.37590140598007338, 2.954454027020771978 ) ) ;
#1257 = CARTESIAN_POINT ( 'NONE',  ( -0.4820197951951999960, -79.33717912789200000, -1.228125725326999929 ) ) ;
#1258 = CARTESIAN_POINT ( 'NONE',  ( 9.500000000000000000, -79.14999999999999147, 0.000000000000000000 ) ) ;
#1259 = CARTESIAN_POINT ( 'NONE',  ( -1.568439782227999846, -77.51102424663160662, -0.3833649254202000090 ) ) ;
#1260 = CIRCLE ( 'NONE', #4991, 0.5000000000000000000 ) ;
#1261 = CARTESIAN_POINT ( 'NONE',  ( 6.675876141078999737, -76.41361125212999639, -10.74461650742999907 ) ) ;
#1262 = CARTESIAN_POINT ( 'NONE',  ( -0.1360749694821127842, -2.121642350341124139, -3.272092924714451456 ) ) ;
#1263 = CARTESIAN_POINT ( 'NONE',  ( 1.341343219651000229, -78.97248393136999312, -0.9216622887798999741 ) ) ;
#1264 = LINE ( 'NONE', #48090, #9187 ) ;
#1265 = CARTESIAN_POINT ( 'NONE',  ( 7.294482259529999624, -79.61226622975098621, -8.153425347847999660 ) ) ;
#1266 = CARTESIAN_POINT ( 'NONE',  ( 12.70259419122522360, -61.53882758488509808, 1.314635108493669824 ) ) ;
#1267 = CARTESIAN_POINT ( 'NONE',  ( 12.82904091336000008, -55.47547470607999998, -2.062673488738000049 ) ) ;
#1268 = CARTESIAN_POINT ( 'NONE',  ( -2.936781018647000252, -85.86543811554798822, 2.063666607083000315 ) ) ;
#1269 = ORIENTED_EDGE ( 'NONE', *, *, #11855, .T. ) ;
#1270 = CARTESIAN_POINT ( 'NONE',  ( -3.140974612311352221, -79.50416666666664867, -11.68767212001979061 ) ) ;
#1271 = CARTESIAN_POINT ( 'NONE',  ( -0.9334586162929999764, -81.40447863951000329, -1.282259494539000011 ) ) ;
#1272 = CARTESIAN_POINT ( 'NONE',  ( 3.165837231865861856, -77.95154321140272202, 10.30965284180923724 ) ) ;
#1273 = CARTESIAN_POINT ( 'NONE',  ( -7.618386520043000765, -18.77287536652999833, 10.53495200520000097 ) ) ;
#1274 = CARTESIAN_POINT ( 'NONE',  ( 0.000000000000000000, -80.35000000001998899, 0.000000000000000000 ) ) ;
#1275 = CARTESIAN_POINT ( 'NONE',  ( -3.520054962697148238, -3.246692171245472824, 0.1437326420056305454 ) ) ;
#1276 = CARTESIAN_POINT ( 'NONE',  ( 10.45256899451774757, -80.86916725350319268, 2.510129016786621925 ) ) ;
#1277 = CARTESIAN_POINT ( 'NONE',  ( -2.495045882587000108, -78.18283894841299286, -9.076670124625998426 ) ) ;
#1278 = CARTESIAN_POINT ( 'NONE',  ( 3.380118192975977820, -85.79678895079199208, -1.504925579246050527 ) ) ;
#1279 = CARTESIAN_POINT ( 'NONE',  ( -3.573177736666999671, -77.36011177151499396, 10.43715168250999881 ) ) ;
#1280 = CARTESIAN_POINT ( 'NONE',  ( 2.548493721447000038, -77.00836198975264324, 12.01365081398999912 ) ) ;
#1281 = CARTESIAN_POINT ( 'NONE',  ( -6.382578252665999763, -80.53473609305189029, -8.990542599477999275 ) ) ;
#1282 = ORIENTED_EDGE ( 'NONE', *, *, #26492, .F. ) ;
#1283 = CARTESIAN_POINT ( 'NONE',  ( 7.479653633103032995, -77.95140769025543648, 5.651087642253929566 ) ) ;
#1284 = CARTESIAN_POINT ( 'NONE',  ( -7.342331066867000544, -55.64999999967000122, 8.190859204290999784 ) ) ;
#1285 = CARTESIAN_POINT ( 'NONE',  ( -7.712695008784000272, -77.26298346740499312, -8.144473358846001432 ) ) ;
#1286 = CARTESIAN_POINT ( 'NONE',  ( 2.550499813263000348, -78.45320834210998839, -10.67515654612000020 ) ) ;
#1287 = CARTESIAN_POINT ( 'NONE',  ( 7.760939450736999312, -24.23085356333000107, -10.15321588359000060 ) ) ;
#1288 = EDGE_CURVE ( 'NONE', #26886, #33815, #5598, .T. ) ;
#1289 = CARTESIAN_POINT ( 'NONE',  ( -0.3065357972716182267, -82.84322915123868825, 4.000656104458952811 ) ) ;
#1290 = CARTESIAN_POINT ( 'NONE',  ( 0.000000000000000000, -0.09999999858569999511, -8.899999998586000771 ) ) ;
#1291 = DIRECTION ( 'NONE',  ( 0.000000000000000000, 1.000000000000000000, 0.000000000000000000 ) ) ;
#1292 = CARTESIAN_POINT ( 'NONE',  ( 3.044330217611999956, -84.11092953870900146, 2.852822925048999814 ) ) ;
#1293 = CARTESIAN_POINT ( 'NONE',  ( 1.310679582531385279, -80.29166666666668561, 0.7554284705563519831 ) ) ;
#1294 = AXIS2_PLACEMENT_3D ( 'NONE', #2770, #29610, #20769 ) ;
#1295 = CARTESIAN_POINT ( 'NONE',  ( 10.53494359612999887, -55.57285042800999264, -7.618393753177000072 ) ) ;
#1296 = B_SPLINE_SURFACE_WITH_KNOTS ( 'NONE', 3, 3, ( 
 ( #3151, #6406, #48038, #56011 ),
 ( #43015, #29125, #29984, #25282 ),
 ( #24422, #37986, #38571, #46877 ),
 ( #15852, #24994, #15561, #7568 ),
 ( #51877, #52446, #7280, #33554 ),
 ( #20853, #16433, #16145, #34122 ),
 ( #2571, #43300, #11721, #51592 ),
 ( #25568, #57156, #16721, #43588 ) ),
 .UNSPECIFIED., .F., .F., .F.,
 ( 4, 1, 1, 1, 1, 4 ),
 ( 4, 4 ),
 ( -0.01200407345747999885, 0.000000000000000000, 0.3333333333333000081, 0.6666666666667000474, 1.000000000000000000, 1.011997855551999947 ),
 ( -0.3559705542741000150, 1.355970554273999928 ),
 .UNSPECIFIED. ) ;
#1297 = CARTESIAN_POINT ( 'NONE',  ( -2.226613147434000073, -78.07001793044798887, 11.04405396508999893 ) ) ;
#1298 = CARTESIAN_POINT ( 'NONE',  ( 1.640574411872000038, -79.59349766811000393, 0.2893137654249999802 ) ) ;
#1299 = CARTESIAN_POINT ( 'NONE',  ( -1.000000000000000000, -78.00000000000000000, 7.200000000000000178 ) ) ;
#1300 = CARTESIAN_POINT ( 'NONE',  ( -7.374560639698971798, -79.37291666666664014, -9.596002108778163731 ) ) ;
#1301 = CARTESIAN_POINT ( 'NONE',  ( -0.1061383120418225301, -81.63053294589249731, 1.507463295298500761 ) ) ;
#1302 = CARTESIAN_POINT ( 'NONE',  ( -13.86363625866555438, -46.43897132165000130, -0.001706075946091080518 ) ) ;
#1303 = CARTESIAN_POINT ( 'NONE',  ( -7.600460745173878152, -80.16297109611984695, -7.601925197388003319 ) ) ;
#1304 = CARTESIAN_POINT ( 'NONE',  ( 8.300970689365456678, -78.00833333333332575, -4.784380313523530326 ) ) ;
#1305 = VECTOR ( 'NONE', #37563, 1000.000000000000000 ) ;
#1306 = EDGE_CURVE ( 'NONE', #10320, #25686, #34712, .T. ) ;
#1307 = ORIENTED_EDGE ( 'NONE', *, *, #22440, .T. ) ;
#1308 = CONICAL_SURFACE ( 'NONE', #57824, 9.431249999994999911, 0.7853981633972997312 ) ;
#1309 = CARTESIAN_POINT ( 'NONE',  ( -0.5392730711932351984, -81.68971611294774959, -1.130938875651418929 ) ) ;
#1310 = EDGE_CURVE ( 'NONE', #19532, #6714, #17878, .T. ) ;
#1311 = CARTESIAN_POINT ( 'NONE',  ( -5.305451056584999492, -80.04393910884809316, -9.672327717035999584 ) ) ;
#1312 = CARTESIAN_POINT ( 'NONE',  ( 8.799999998347999508, 1.651506244335999933E-09, 5.811483786157999589E-09 ) ) ;
#1313 = EDGE_LOOP ( 'NONE', ( #17606, #9356, #29670, #17047, #4604 ) ) ;
#1314 = ORIENTED_EDGE ( 'NONE', *, *, #47629, .F. ) ;
#1315 = CARTESIAN_POINT ( 'NONE',  ( -0.6310361675857999453, -82.01439296913500243, 1.269589084679000113 ) ) ;
#1316 = ORIENTED_EDGE ( 'NONE', *, *, #31004, .F. ) ;
#1317 = VERTEX_POINT ( 'NONE', #7865 ) ;
#1318 = CARTESIAN_POINT ( 'NONE',  ( 1.761265949708000100, -18.29141781213999707, 12.57448205042999945 ) ) ;
#1319 = CARTESIAN_POINT ( 'NONE',  ( -1.447950951198242908, -77.76302083339091098, -0.3900009942188623069 ) ) ;
#1320 = APPLICATION_PROTOCOL_DEFINITION ( 'draft international standard', 'automotive_design', 1998, #39066 ) ;
#1321 = CARTESIAN_POINT ( 'NONE',  ( 3.159418921492714638, -79.54791666055969301, 1.368597868856442856 ) ) ;
#1322 = EDGE_CURVE ( 'NONE', #23950, #1742, #20864, .T. ) ;
#1323 = CARTESIAN_POINT ( 'NONE',  ( 1.902005808056935310, -78.24161995856391627, -9.052334553967094521 ) ) ;
#1324 = LINE ( 'NONE', #28445, #17527 ) ;
#1325 = ORIENTED_EDGE ( 'NONE', *, *, #7961, .F. ) ;
#1326 = ORIENTED_EDGE ( 'NONE', *, *, #45707, .F. ) ;
#1327 = CARTESIAN_POINT ( 'NONE',  ( -8.805853231905880207, -77.57526559296016444, 2.831825794683833220 ) ) ;
#1328 = CARTESIAN_POINT ( 'NONE',  ( 0.000000000000000000, -75.67500000000001137, 0.000000000000000000 ) ) ;
#1329 = CARTESIAN_POINT ( 'NONE',  ( 1.460959015002472494, -79.27083333333335702, 0.3926218265389233020 ) ) ;
#1330 = CARTESIAN_POINT ( 'NONE',  ( -1.247385801055000076, -17.52277743740000204, 12.50301438876999960 ) ) ;
#1331 = CARTESIAN_POINT ( 'NONE',  ( -6.766389538252999714, -77.83344834330198125, -6.956053621355001049 ) ) ;
#1332 = DIRECTION ( 'NONE',  ( -1.000000000000000000, 0.000000000000000000, 0.000000000000000000 ) ) ;
#1333 = CARTESIAN_POINT ( 'NONE',  ( -10.04115011118000211, -22.76486430425999785, 7.682331425175999762 ) ) ;
#1334 = CARTESIAN_POINT ( 'NONE',  ( -12.00000000000000000, -76.89999999999999147, 0.000000000000000000 ) ) ;
#1335 = CARTESIAN_POINT ( 'NONE',  ( -1.125831293927000099, -79.53339211834999389, 0.7473110439769999891 ) ) ;
#1336 = AXIS2_PLACEMENT_3D ( 'NONE', #29778, #12086, #56675 ) ;
#1337 = EDGE_CURVE ( 'NONE', #38648, #12253, #38058, .T. ) ;
#1338 = CARTESIAN_POINT ( 'NONE',  ( -8.932802644879007659, -77.57622193750340500, -3.074066805765899080 ) ) ;
#1339 = CARTESIAN_POINT ( 'NONE',  ( 0.1632771479509232126, -76.57380765581523008, 11.74886050266104220 ) ) ;
#1340 = B_SPLINE_CURVE_WITH_KNOTS ( 'NONE', 3,
 ( #54873, #14420, #882, #32417, #1171, #1749 ),
 .UNSPECIFIED., .F., .F.,
 ( 4, 2, 4 ),
 ( 0.000000000000000000, 0.5000000000000001110, 1.000000000000000000 ),
 .UNSPECIFIED. ) ;
#1341 = CARTESIAN_POINT ( 'NONE',  ( -2.068348282409000038, -80.00523869776598929, 3.626505972287000112 ) ) ;
#1342 = CARTESIAN_POINT ( 'NONE',  ( 8.440675369999999234, -80.07150142417098948, 7.053722371789000967 ) ) ;
#1343 = LINE ( 'NONE', #46804, #52543 ) ;
#1344 = CARTESIAN_POINT ( 'NONE',  ( 5.413936244485441307, -76.76681587759365755, -9.393431973814015734 ) ) ;
#1345 = CARTESIAN_POINT ( 'NONE',  ( 2.971106681726000343, -79.60682046129089429, 1.938318254092999959 ) ) ;
#1346 = CARTESIAN_POINT ( 'NONE',  ( -1.210648453353548426, -79.48564454928481382, 9.248615044363743820 ) ) ;
#1347 = FACE_BOUND ( 'NONE', #23375, .T. ) ;
#1348 = CARTESIAN_POINT ( 'NONE',  ( -3.054513261463999818, -2.868203725971999685, -2.270689576097000284 ) ) ;
#1349 = CARTESIAN_POINT ( 'NONE',  ( 9.865351076058296087, -77.19999999999998863, -4.411030472467261987 ) ) ;
#1350 = EDGE_LOOP ( 'NONE', ( #56104, #21727, #7177, #50239 ) ) ;
#1351 = CARTESIAN_POINT ( 'NONE',  ( 0.8205724371039223586, -3.500000000000000000, -3.402696673547657813 ) ) ;
#1352 = DIRECTION ( 'NONE',  ( -5.380858151921000126E-11, -1.000000000000000000, 8.802973286544000911E-11 ) ) ;
#1353 = CARTESIAN_POINT ( 'NONE',  ( 1.439896632895317108, -79.06458333333331723, 10.99999999999999822 ) ) ;
#1354 = CARTESIAN_POINT ( 'NONE',  ( 1.931086388455000025, -60.09778595451999905, 12.71798280857999863 ) ) ;
#1355 = FACE_OUTER_BOUND ( 'NONE', #6251, .T. ) ;
#1356 = CARTESIAN_POINT ( 'NONE',  ( 10.07201971379686967, -79.37863564844947462, 3.781752685250035828 ) ) ;
#1357 = DIRECTION ( 'NONE',  ( 0.000000000000000000, 0.000000000000000000, -1.000000000000000000 ) ) ;
#1358 = CARTESIAN_POINT ( 'NONE',  ( -12.00000000000000000, -23.15000000002000036, -0.7999999999999001243 ) ) ;
#1359 = CARTESIAN_POINT ( 'NONE',  ( -6.565417933280000895, -77.81803934957498825, -9.031084880605000365 ) ) ;
#1360 = CIRCLE ( 'NONE', #7946, 12.50000000000000000 ) ;
#1361 = CARTESIAN_POINT ( 'NONE',  ( -1.414458455730000175, -82.43699584127701030, -0.5383077919788999965 ) ) ;
#1362 = LINE ( 'NONE', #9627, #50266 ) ;
#1363 = CARTESIAN_POINT ( 'NONE',  ( -8.420145992286000691, -77.48751300560297750, 3.744741888101000171 ) ) ;
#1365 = CARTESIAN_POINT ( 'NONE',  ( -1.818468715484000065E-14, -79.21250000010999770, 0.000000000000000000 ) ) ;
#1364 = CARTESIAN_POINT ( 'NONE',  ( 3.755995663163999687, -82.14153471428599573, -0.05909197296705000213 ) ) ;
#1366 = CARTESIAN_POINT ( 'NONE',  ( 7.507056363060000237, -79.76904805011500343, -5.572808305725000189 ) ) ;
#1367 = CARTESIAN_POINT ( 'NONE',  ( 0.7554284705563452107, -80.73333333333332007, 1.310679582531388609 ) ) ;
#1368 = CARTESIAN_POINT ( 'NONE',  ( 0.3256773761571999937, -79.30290681445698908, -1.278468177226000035 ) ) ;
#1369 = CARTESIAN_POINT ( 'NONE',  ( -6.271765859646529329, -77.17558322877896160, -8.730771744879000096 ) ) ;
#1370 = CARTESIAN_POINT ( 'NONE',  ( 9.252740428348992907, -77.17083333333333428, 2.486604901413179025 ) ) ;
#1371 = ADVANCED_FACE ( 'NONE', ( #22609 ), #37635, .F. ) ;
#1372 = LINE ( 'NONE', #42391, #21489 ) ;
#1373 = ORIENTED_EDGE ( 'NONE', *, *, #42922, .T. ) ;
#1374 = CARTESIAN_POINT ( 'NONE',  ( 2.377756013412999803, -79.34251650879200213, -11.79209151100000064 ) ) ;
#1375 = AXIS2_PLACEMENT_3D ( 'NONE', #5775, #23782, #51256 ) ;
#1376 = DIRECTION ( 'NONE',  ( 0.000000000000000000, -1.000000000000000000, 0.000000000000000000 ) ) ;
#1377 = CARTESIAN_POINT ( 'NONE',  ( -8.414570695956999913, -60.64999999943950826, -8.414570695956999913 ) ) ;
#1378 = EDGE_LOOP ( 'NONE', ( #40195, #20507, #12745, #17622 ) ) ;
#1379 = B_SPLINE_CURVE_WITH_KNOTS ( 'NONE', 3,
 ( #54929, #32472, #36631, #36336, #46687, #49939, #54361, #10071, #37209, #28052, #41359, #5340, #36918, #27471, #654, #51107, #41940, #10659 ),
 .UNSPECIFIED., .F., .F.,
 ( 4, 2, 2, 2, 2, 2, 2, 2, 4 ),
 ( 0.000000000000000000, 0.1250000000000000000, 0.2500000000000000000, 0.3750000000000000000, 0.5000000000000000000, 0.6250000000000000000, 0.7500000000000000000, 0.8750000000000000000, 1.000000000000000000 ),
 .UNSPECIFIED. ) ;
#1380 = CARTESIAN_POINT ( 'NONE',  ( 10.65351345285000129, -78.33619942611500164, -5.379419444189999844 ) ) ;
#1381 = VECTOR ( 'NONE', #38761, 1000.000000000000000 ) ;
#1382 = EDGE_LOOP ( 'NONE', ( #1591, #17664, #4339, #1641 ) ) ;
#1383 = ORIENTED_EDGE ( 'NONE', *, *, #50103, .T. ) ;
#1384 = CARTESIAN_POINT ( 'NONE',  ( 8.180687091746225548, -60.10655143787244725, 7.353725627631166439 ) ) ;
#1385 = ORIENTED_EDGE ( 'NONE', *, *, #17552, .F. ) ;
#1386 = ADVANCED_FACE ( 'NONE', ( #41198 ), #6893, .F. ) ;
#1387 = CARTESIAN_POINT ( 'NONE',  ( -3.180479912003000287, -80.29693765374598513, -1.570387657113000213 ) ) ;
#1388 = CARTESIAN_POINT ( 'NONE',  ( -12.80090744921000123, -19.23767312576000066, -1.980532734072999901 ) ) ;
#1389 = ORIENTED_EDGE ( 'NONE', *, *, #429, .F. ) ;
#1390 = CARTESIAN_POINT ( 'NONE',  ( 1.179782483562120010, -82.82318035081991070, -0.4135125750267664158 ) ) ;
#1391 = CARTESIAN_POINT ( 'NONE',  ( -7.678690995210999404, -58.55648180022999583, 10.59551070212999946 ) ) ;
#1392 = ORIENTED_EDGE ( 'NONE', *, *, #10378, .T. ) ;
#1393 = CARTESIAN_POINT ( 'NONE',  ( -10.75000000000000000, -80.51041666666664298, -1.407171709420429018 ) ) ;
#1394 = CARTESIAN_POINT ( 'NONE',  ( 9.703646361260002351, -77.60084330994595803, 0.1143463288009116258 ) ) ;
#1395 = CARTESIAN_POINT ( 'NONE',  ( -2.170944906844886724, -79.79999999999999716, -11.61767828058813024 ) ) ;
#1396 = DIRECTION ( 'NONE',  ( 0.000000000000000000, 1.000000000000000000, 0.000000000000000000 ) ) ;
#1397 = B_SPLINE_CURVE_WITH_KNOTS ( 'NONE', 3,
 ( #16488, #34467, #48651, #35328, #26198, #53356, #25907, #12337, #48937, #12902, #30902, #39194, #43644, #8479, #43930, #16776, #22052, #21193, #52497, #39491, #48088, #57493, #3202, #12622, #30326, #40061, #48367, #17056, #35037, #53072, #14366, #49826, #14656, #54541, #37096, #41243, #23523, #9372, #40663, #36227, #35927, #27939, #54249, #256, #32654, #50706, #18239, #55112, #58374, #10246, #45987, #41534, #13782, #5233, #53957, #40957, #28229, #19104, #17936, #36805, #31783, #27362, #4942, #46281, #54824, #45694, #13494, #5806, #5514, #18524, #23237, #23813, #1117, #4655, #31485, #49530, #833, #9076, #36516, #27063, #22653, #32077, #45101, #45399, #22947, #547, #14082, #32366, #50118, #9662, #18814, #27652, #50409, #9959, #20561, #46867, #42711, #24982, #11138, #28818, #29685, #42127, #11711, #47737, #33828, #51866, #41831, #15252, #11419, #46575, #56289, #29400, #47453, #37687, #37388, #38559, #28526, #56575, #52153, #6978, #19987, #16133, #7270, #10842, #34110, #32949, #6394, #6101, #37976, #15840, #50993, #24409, #33244, #29114, #24110, #1405, #19396, #15546, #6690, #33542, #51581, #47160, #24699, #10542, #43003, #2560, #55407, #1693, #14952, #19686, #2277, #42425, #55703, #20274, #51287, #1994, #55999, #38268, #25271, #3704, #21130, #34695, #30265, #17578, #21708, #12562, #43290, #44438, #53299, #43874, #30560, #13130, #12844, #29974, #30843, #48877, #8137, #53591, #3423, #40001, #48025, #57439, #26416, #3990, #8419, #21993, #16712, #57719, #7559, #25558, #48591, #58016, #43578, #35565 ),
 .UNSPECIFIED., .F., .F.,
 ( 4, 2, 2, 1, 1, 1, 1, 1, 2, 2, 2, 2, 2, 1, 1, 1, 1, 1, 2, 2, 2, 2, 2, 1, 1, 1, 1, 2, 2, 2, 2, 2, 2, 2, 2, 1, 1, 1, 1, 2, 2, 2, 2, 2, 2, 2, 1, 1, 1, 1, 1, 2, 2, 2, 2, 2, 1, 1, 1, 2, 2, 2, 2, 1, 1, 1, 2, 2, 2, 2, 1, 1, 1, 1, 1, 2, 2, 2, 2, 2, 1, 1, 1, 2, 2, 2, 1, 2, 2, 1, 1, 2, 2, 2, 2, 2, 1, 2, 2, 2, 2, 2, 2, 2, 2, 1, 1, 1, 2, 2, 2, 2, 2, 2, 2, 2, 1, 1, 2, 4 ),
 ( 0.000000000000000000, 0.03124999999998840511, 0.04687499999998261807, 0.05468749999997975231, 0.05859374999997830208, 0.06054687499997758043, 0.06152343749997721267, 0.06201171874997703226, 0.06225585937497695593, 0.06249999999997687961, 0.09374999999996236344, 0.1093749999999550915, 0.1171874999999514694, 0.1210937499999496514, 0.1230468749999487216, 0.1240234374999482914, 0.1245117187499480693, 0.1247558593749479861, 0.1248779296874479167, 0.1249999999999478612, 0.1562499999999539535, 0.1718749999999570344, 0.1796874999999586442, 0.1835937499999594491, 0.1855468749999598932, 0.1865234374999601152, 0.1870117187499601985, 0.1872558593749602263, 0.1874999999999602263, 0.2031249999999644174, 0.2109374999999664713, 0.2148437499999675537, 0.2187499999999686362, 0.2343749999999729661, 0.2421874999999751310, 0.2460937499999762690, 0.2480468749999769074, 0.2490234374999772959, 0.2495117187499775180, 0.2497558593749775180, 0.2499999999999775180, 0.3124999999999837352, 0.3749999999999899525, 0.4374999999999962252, 0.4687499999999993894, 0.4843750000000009437, 0.4921875000000017208, 0.4960937500000021094, 0.4980468750000022760, 0.4990234375000023870, 0.4995117187500023870, 0.4997558593750024425, 0.5000000000000024425, 0.5312500000000072164, 0.5468750000000095479, 0.5546875000000107692, 0.5585937500000113243, 0.5605468750000116573, 0.5615234375000117684, 0.5620117187500118794, 0.5625000000000118794, 0.5937500000000155431, 0.6093750000000173195, 0.6171875000000182077, 0.6210937500000186517, 0.6230468750000188738, 0.6240234375000189848, 0.6250000000000189848, 0.6562500000000210942, 0.6718750000000220934, 0.6796875000000224265, 0.6835937500000226485, 0.6855468750000228706, 0.6865234375000229816, 0.6870117187500229816, 0.6872558593750229816, 0.6875000000000229816, 0.7187500000000279776, 0.7343750000000304201, 0.7421875000000316414, 0.7460937500000323075, 0.7480468750000325295, 0.7490234375000327516, 0.7495117187500327516, 0.7500000000000327516, 0.7812500000000329736, 0.7851562500000329736, 0.7856445312500329736, 0.7861328125000330846, 0.7871093750000330846, 0.7890625000000331957, 0.7968750000000335287, 0.8125000000000343059, 0.8203125000000346390, 0.8212890625000344169, 0.8222656250000343059, 0.8242187500000338618, 0.8281250000000331957, 0.8437500000000311973, 0.8515625000000301981, 0.8593750000000291989, 0.8750000000000273115, 0.8906250000000254241, 0.8925781250000250910, 0.8930664062500248690, 0.8935546875000247580, 0.8945312500000244249, 0.8984375000000235367, 0.9062500000000217604, 0.9375000000000144329, 0.9453125000000125455, 0.9492187500000116573, 0.9531250000000107692, 0.9687500000000071054, 0.9726562500000062172, 0.9736328125000059952, 0.9746093750000057732, 0.9765625000000053291, 0.9843750000000035527, 1.000000000000000000 ),
 .UNSPECIFIED. ) ;
#1398 = CARTESIAN_POINT ( 'NONE',  ( -8.771427373352999268, -77.78517645232463451, -4.151237309591000013 ) ) ;
#1400 = EDGE_CURVE ( 'NONE', #3338, #53933, #13132, .T. ) ;
#1399 = CARTESIAN_POINT ( 'NONE',  ( 11.09875712452000052, -76.02591650810499857, 1.375294608629999971 ) ) ;
#1401 = CARTESIAN_POINT ( 'NONE',  ( -3.250000000000000000, -3.100000000000000089, 0.000000000000000000 ) ) ;
#1402 = EDGE_CURVE ( 'NONE', #2960, #30023, #33196, .T. ) ;
#1403 = AXIS2_PLACEMENT_3D ( 'NONE', #46658, #38348, #55199 ) ;
#1404 = CARTESIAN_POINT ( 'NONE',  ( -7.640030139773000606, -60.10716934574000447, -10.18491068061999982 ) ) ;
#1405 = CARTESIAN_POINT ( 'NONE',  ( -7.198099468258734035, -78.65408334510459554, -5.809580251814940866 ) ) ;
#1406 = CARTESIAN_POINT ( 'NONE',  ( 8.944043683863377225, -76.50578467936081495, 7.623615284876848364 ) ) ;
#1407 = CARTESIAN_POINT ( 'NONE',  ( -0.5200379331645087477, -23.45155696398142808, -10.98772212209864385 ) ) ;
#1408 = DIRECTION ( 'NONE',  ( 1.000000000000000000, 0.000000000000000000, 0.000000000000000000 ) ) ;
#1409 = VECTOR ( 'NONE', #7391, 1000.000000000000000 ) ;
#1410 = DIRECTION ( 'NONE',  ( 0.000000000000000000, -1.000000000000000000, 0.000000000000000000 ) ) ;
#1411 = CARTESIAN_POINT ( 'NONE',  ( -0.5668640744825168554, -61.71659694886608349, -12.50470739229184325 ) ) ;
#1412 = CARTESIAN_POINT ( 'NONE',  ( -0.4317228448582000055, -80.36167549782599906, -4.107568489194999728 ) ) ;
#1413 = LINE ( 'NONE', #40964, #10798 ) ;
#1414 = PLANE ( 'NONE',  #5891 ) ;
#1415 = CARTESIAN_POINT ( 'NONE',  ( 1.136635571591867233, -82.88416972722252751, 0.5202534302794125098 ) ) ;
#1416 = CARTESIAN_POINT ( 'NONE',  ( -2.226051307435857662, -77.00624999999999432, -9.265603215652616242 ) ) ;
#1417 = DIRECTION ( 'NONE',  ( -1.000000000000000000, 0.000000000000000000, 0.000000000000000000 ) ) ;
#1418 = CARTESIAN_POINT ( 'NONE',  ( 1.101534974885716833, -79.99999999999997158, 9.249201346533595824 ) ) ;
#1419 = B_SPLINE_CURVE_WITH_KNOTS ( 'NONE', 3,
 ( #10060, #14755, #10346, #5902, #41633, #10938, #24210, #19206, #32754, #50801 ),
 .UNSPECIFIED., .F., .F.,
 ( 4, 2, 2, 2, 4 ),
 ( 0.000000000000000000, 0.2500000000000000000, 0.5000000000000000000, 0.7500000000000000000, 1.000000000000000000 ),
 .UNSPECIFIED. ) ;
#1420 = CARTESIAN_POINT ( 'NONE',  ( -10.53494356941000021, -60.02715052954999919, -7.618393677181999557 ) ) ;
#1421 = CONICAL_SURFACE ( 'NONE', #16485, 1.546875000130000011, 0.7853981633972997312 ) ;
#1423 = CARTESIAN_POINT ( 'NONE',  ( 9.250054636821570142, -79.84526209104460293, -0.6055073710143449306 ) ) ;
#1422 = SHAPE_REPRESENTATION ( 'Push Button Cover', ( #43526 ), #24646 ) ;
#1424 = CARTESIAN_POINT ( 'NONE',  ( -1.669849926071999890, -23.37228600417000024, -12.48404299553000030 ) ) ;
#1425 = CARTESIAN_POINT ( 'NONE',  ( -3.170501611485000204, -2.010283069270999867, 1.448148066727999783 ) ) ;
#1426 = CARTESIAN_POINT ( 'NONE',  ( -0.5312504855272001114, -78.63049415034599576, -9.708839960653000034 ) ) ;
#1427 = CARTESIAN_POINT ( 'NONE',  ( -7.712213536729100483, -24.06179137615005814, -10.27334987165781399 ) ) ;
#1428 = EDGE_CURVE ( 'NONE', #49604, #32986, #23478, .T. ) ;
#1429 = CARTESIAN_POINT ( 'NONE',  ( 10.68616709762000028, -77.08241475543599108, -6.049920594266999352 ) ) ;
#1430 = CARTESIAN_POINT ( 'NONE',  ( 7.651160336710000287, -19.23767313813999991, 10.45205658995999976 ) ) ;
#1431 = CARTESIAN_POINT ( 'NONE',  ( 9.233664981878000333, -79.64544880995556753, 5.933249305785000871 ) ) ;
#1432 = CARTESIAN_POINT ( 'NONE',  ( -6.591778134092000307, -75.74638372273000186, -9.790090750544999665 ) ) ;
#1433 = ORIENTED_EDGE ( 'NONE', *, *, #28938, .T. ) ;
#1434 = CARTESIAN_POINT ( 'NONE',  ( -1.739781828957000176, -86.23821544543099549, 3.560805514105999769 ) ) ;
#1435 = CARTESIAN_POINT ( 'NONE',  ( -9.360432184603999062, -80.25606803504099673, -6.310659218800999781 ) ) ;
#1436 = CARTESIAN_POINT ( 'NONE',  ( 7.548260755434943903, -78.30112507871334060, -5.346425350760562800 ) ) ;
#1437 = CYLINDRICAL_SURFACE ( 'NONE', #24296, 1.750000000000000000 ) ;
#1438 = CARTESIAN_POINT ( 'NONE',  ( 5.151324428776999476, -77.73871255725200058, 9.964033682248000900 ) ) ;
#1439 = CARTESIAN_POINT ( 'NONE',  ( 10.28132586880103894, -76.61033914466867145, -6.022081058836299405 ) ) ;
#1440 = CARTESIAN_POINT ( 'NONE',  ( 6.930806504809000401, -78.58198617658298701, -6.687086896242999678 ) ) ;
#1441 = CARTESIAN_POINT ( 'NONE',  ( 2.283260173233999879, -82.70557145154198508, 3.491877656328999713 ) ) ;
#1442 = CARTESIAN_POINT ( 'NONE',  ( -1.000000000000000000, -81.99999999999998579, -7.000000000000000000 ) ) ;
#1443 = DIRECTION ( 'NONE',  ( 0.000000000000000000, 1.000000000000000000, 0.000000000000000000 ) ) ;
#1444 = ORIENTED_EDGE ( 'NONE', *, *, #36214, .F. ) ;
#1445 = CARTESIAN_POINT ( 'NONE',  ( 3.599999993293999889, -0.2000000067061999953, 5.600095136020000205E-09 ) ) ;
#1446 = DIRECTION ( 'NONE',  ( 0.000000000000000000, 1.000000000000000000, 0.000000000000000000 ) ) ;
#1447 = ORIENTED_EDGE ( 'NONE', *, *, #10114, .F. ) ;
#1448 = CARTESIAN_POINT ( 'NONE',  ( 0.2725326480772000126, -78.99296158314500360, 1.305490477442999842 ) ) ;
#1449 = CARTESIAN_POINT ( 'NONE',  ( 0.000000000000000000, -78.69999999999998863, 0.000000000000000000 ) ) ;
#1450 = CARTESIAN_POINT ( 'NONE',  ( -0.2327570447753271599, -80.71078059628793255, -1.249194938801351462 ) ) ;
#1451 = EDGE_LOOP ( 'NONE', ( #14582, #26391, #19013, #53979, #53142, #45615, #22892 ) ) ;
#1452 = CARTESIAN_POINT ( 'NONE',  ( -0.08650930969203998733, -78.63442944748399555, 12.16449944406000050 ) ) ;
#1453 = CARTESIAN_POINT ( 'NONE',  ( -8.699139934798001406, -77.54738813692499377, -7.073312318721999503 ) ) ;
#1454 = AXIS2_PLACEMENT_3D ( 'NONE', #14439, #40440, #50479 ) ;
#1455 = CARTESIAN_POINT ( 'NONE',  ( 10.10447584125107490, -61.25118490511742664, -7.864774383105173960 ) ) ;
#1456 = ORIENTED_EDGE ( 'NONE', *, *, #46971, .F. ) ;
#1457 = ORIENTED_EDGE ( 'NONE', *, *, #20680, .F. ) ;
#1458 = FACE_OUTER_BOUND ( 'NONE', #537, .T. ) ;
#1459 = EDGE_CURVE ( 'NONE', #10086, #28795, #8421, .T. ) ;
#1460 = AXIS2_PLACEMENT_3D ( 'NONE', #35793, #57963, #39088 ) ;
#1461 = CARTESIAN_POINT ( 'NONE',  ( -9.687172913667000174, -80.02050914020550465, -1.248753675804000096 ) ) ;
#1462 = VERTEX_POINT ( 'NONE', #46530 ) ;
#1463 = CARTESIAN_POINT ( 'NONE',  ( -7.639893379675799068, -55.41284423887100985, 10.11462454828661528 ) ) ;
#1464 = CARTESIAN_POINT ( 'NONE',  ( 10.20678250197623882, -24.23575784472138039, -7.770339463571165339 ) ) ;
#1465 = EDGE_CURVE ( 'NONE', #49740, #9279, #54779, .T. ) ;
#1466 = ORIENTED_EDGE ( 'NONE', *, *, #21295, .F. ) ;
#1467 = CARTESIAN_POINT ( 'NONE',  ( 4.763443004301499251, -80.76150222777162924, -9.661361922714023720 ) ) ;
#1468 = FACE_OUTER_BOUND ( 'NONE', #54531, .T. ) ;
#1469 = CARTESIAN_POINT ( 'NONE',  ( -0.4548846362379543873, -80.19556477582571574, -1.164187075856578879 ) ) ;
#1470 = CARTESIAN_POINT ( 'NONE',  ( 1.718598679953219799, -17.75037066952814513, -12.71111582767946935 ) ) ;
#1471 = CARTESIAN_POINT ( 'NONE',  ( -1.850935023731000051, -77.10928756760588954, 9.663325317366000533 ) ) ;
#1472 = EDGE_CURVE ( 'NONE', #35427, #47711, #38605, .T. ) ;
#1473 = CARTESIAN_POINT ( 'NONE',  ( 0.7757320150892573762, -78.51702430842580327, -1.327015570253983867 ) ) ;
#1474 = CARTESIAN_POINT ( 'NONE',  ( -1.711240663526480743, -78.96979164862780465, -3.629922989123440136 ) ) ;
#1475 = VERTEX_POINT ( 'NONE', #10794 ) ;
#1476 = CARTESIAN_POINT ( 'NONE',  ( -12.19234209666000091, -75.99367673319000005, -1.697737568323999913 ) ) ;
#1477 = B_SPLINE_SURFACE_WITH_KNOTS ( 'NONE', 3, 3, ( 
 ( #29757, #29477, #47536, #7061 ),
 ( #47814, #25632, #43360, #2643 ),
 ( #43655, #39208, #20920, #26489 ),
 ( #4368, #26785, #58389, #17355 ),
 ( #13799, #44814, #22670, #30914 ),
 ( #28475, #58092, #45415, #22369 ),
 ( #18253, #274, #32898, #27378 ),
 ( #40381, #17951, #50943, #10490 ),
 ( #46526, #45121, #8493, #35943 ),
 ( #4958, #53366, #53970, #6050 ),
 ( #57797, #36245, #53668, #44513 ) ),
 .UNSPECIFIED., .F., .F., .F.,
 ( 4, 1, 1, 1, 1, 1, 1, 1, 4 ),
 ( 4, 4 ),
 ( -0.02001474922158999817, 0.000000000000000000, 0.1666666666667000196, 0.3333333333333000081, 0.5000000000000000000, 0.6666666666667000474, 0.8333333333333000637, 1.000000000000000000, 1.020283381528000133 ),
 ( -0.3582002740342999925, 1.358862457857999972 ),
 .UNSPECIFIED. ) ;
#1478 = CARTESIAN_POINT ( 'NONE',  ( -3.219784822078160857, -2.382367439899148565, -1.420610107900855068 ) ) ;
#1479 = CARTESIAN_POINT ( 'NONE',  ( 7.762981007074000850, -60.96089459184000248, -9.992000916374999875 ) ) ;
#1480 = CARTESIAN_POINT ( 'NONE',  ( 11.03890801094999929, -78.69679818280999939, -5.342433469444999972 ) ) ;
#1481 = CARTESIAN_POINT ( 'NONE',  ( -3.699256142337000064, -76.96545403433599120, 11.71059914860999918 ) ) ;
#1482 = CARTESIAN_POINT ( 'NONE',  ( -3.518657424384993959, -85.83735716284299144, 1.566607219110014659 ) ) ;
#1483 = CARTESIAN_POINT ( 'NONE',  ( 10.12290050255000118, -60.04999997790999799, -7.648026768390999486 ) ) ;
#1484 = CARTESIAN_POINT ( 'NONE',  ( 11.55486890050020143, -78.32335062082758270, 3.501387709252974823 ) ) ;
#1485 = FACE_OUTER_BOUND ( 'NONE', #53120, .T. ) ;
#1486 = AXIS2_PLACEMENT_3D ( 'NONE', #44518, #48386, #13514 ) ;
#1487 = ORIENTED_EDGE ( 'NONE', *, *, #35079, .F. ) ;
#1488 = DIRECTION ( 'NONE',  ( 0.000000000000000000, 0.000000000000000000, -1.000000000000000000 ) ) ;
#1489 = CARTESIAN_POINT ( 'NONE',  ( 7.792609338710000166, -77.13002767319579789, 5.788510568612999840 ) ) ;
#1490 = CARTESIAN_POINT ( 'NONE',  ( 7.730443418312603399, -24.12191635826273739, 10.25197760564498140 ) ) ;
#1491 = CARTESIAN_POINT ( 'NONE',  ( -0.3271848554491046945, -78.89583333333328596, 1.217465845835393301 ) ) ;
#1492 = CARTESIAN_POINT ( 'NONE',  ( -0.4714591427245999888, -2.679096200086999779, 3.841621304652000024 ) ) ;
#1493 = CARTESIAN_POINT ( 'NONE',  ( -10.32936100969000037, -78.46581739375498898, 6.204842689816000068 ) ) ;
#1494 = CARTESIAN_POINT ( 'NONE',  ( -4.491587152465999822, -78.85767126595499121, -8.642068059767000321 ) ) ;
#1496 = CARTESIAN_POINT ( 'NONE',  ( 0.000000000000000000, -28.92928575306000383, 0.000000000000000000 ) ) ;
#1495 = CARTESIAN_POINT ( 'NONE',  ( -11.06942781765597239, -76.17262117212699479, 3.959973230732274807 ) ) ;
#1497 = CARTESIAN_POINT ( 'NONE',  ( -10.76888293467999880, -79.53970297022300429, -1.790677617362999907 ) ) ;
#1498 = CARTESIAN_POINT ( 'NONE',  ( 1.387607402548059143, -85.88547957940599531, 3.197381817704088469 ) ) ;
#1499 = EDGE_LOOP ( 'NONE', ( #5788, #41984, #28707, #17470, #27775, #26159 ) ) ;
#1500 = CARTESIAN_POINT ( 'NONE',  ( 12.70249480706760359, -24.96498603299019692, 0.9989402950733060615 ) ) ;
#1501 = CARTESIAN_POINT ( 'NONE',  ( 9.250000000000000000, -77.84999999999999432, 0.000000000000000000 ) ) ;
#1502 = DIRECTION ( 'NONE',  ( 0.000000000000000000, 0.000000000000000000, -1.000000000000000000 ) ) ;
#1503 = CARTESIAN_POINT ( 'NONE',  ( 10.94409238582999855, -78.74648653645297713, 0.8311789410725000105 ) ) ;
#1504 = DIRECTION ( 'NONE',  ( 0.000000000000000000, -1.000000000000000000, 0.000000000000000000 ) ) ;
#1505 = CARTESIAN_POINT ( 'NONE',  ( -6.756755724436000143, -79.51665000578398690, 6.762936965852000881 ) ) ;
#1506 = CARTESIAN_POINT ( 'NONE',  ( 10.31444587878999997, -17.69924218095000157, -7.758886158107999975 ) ) ;
#1507 = CARTESIAN_POINT ( 'NONE',  ( -8.130813118010999929, -17.31476110167000115, 9.546856411653001473 ) ) ;
#1508 = EDGE_LOOP ( 'NONE', ( #37769, #21742, #3756, #37883, #53212, #55093 ) ) ;
#1509 = ADVANCED_FACE ( 'NONE', ( #10204 ), #6533, .F. ) ;
#1510 = CARTESIAN_POINT ( 'NONE',  ( -6.349996674360999904, -78.85392148219399644, -9.301156207373001195 ) ) ;
#1511 = CARTESIAN_POINT ( 'NONE',  ( 12.70619604129601754, -54.33855724441239943, 1.571828507126210583 ) ) ;
#1512 = CARTESIAN_POINT ( 'NONE',  ( 11.75000000000000000, -79.79999999999999716, -4.009019365174000020E-13 ) ) ;
#1513 = CARTESIAN_POINT ( 'NONE',  ( -3.444390397065229426, -78.62148120184446043, 1.946201225192911943 ) ) ;
#1514 = CARTESIAN_POINT ( 'NONE',  ( -5.207681435413956450, -77.36354831110318742, 10.89428926699400613 ) ) ;
#1515 = CARTESIAN_POINT ( 'NONE',  ( 1.137232763453390971, -81.38436038258944905, 0.5186267222472648042 ) ) ;
#1516 = CARTESIAN_POINT ( 'NONE',  ( -9.735746418238305111, -79.30854793174478345, 5.571072665431956672 ) ) ;
#1517 = CARTESIAN_POINT ( 'NONE',  ( -9.155305986995932344, -76.99999999999998579, 1.687095892431314637 ) ) ;
#1518 = CARTESIAN_POINT ( 'NONE',  ( 10.98676125741665643, -23.41445108201793346, -0.5397229578417962470 ) ) ;
#1519 = CARTESIAN_POINT ( 'NONE',  ( 1.980532734072999901, -22.76232686847000153, 12.80090744964000038 ) ) ;
#1520 = CARTESIAN_POINT ( 'NONE',  ( 10.92224869643393070, -78.20263265991563628, 0.3426835237561569047 ) ) ;
#1521 = AXIS2_PLACEMENT_3D ( 'NONE', #570, #37410, #50142 ) ;
#1522 = CARTESIAN_POINT ( 'NONE',  ( -1.570796326794938524, -77.18541666666666856, 11.99999999999999645 ) ) ;
#1523 = VERTEX_POINT ( 'NONE', #42081 ) ;
#1524 = VERTEX_POINT ( 'NONE', #16378 ) ;
#1525 = FACE_OUTER_BOUND ( 'NONE', #27120, .T. ) ;
#1526 = CARTESIAN_POINT ( 'NONE',  ( 7.078252940824787842, -78.78224352234950345, -8.090973445952867493 ) ) ;
#1527 = EDGE_CURVE ( 'NONE', #5139, #52771, #40497, .T. ) ;
#1528 = EDGE_LOOP ( 'NONE', ( #31135, #36616, #40114, #40612 ) ) ;
#1529 = CARTESIAN_POINT ( 'NONE',  ( 5.177752511601999785, -76.58669514303510084, 9.912858493839999952 ) ) ;
#1530 = VECTOR ( 'NONE', #9099, 1000.000000000000227 ) ;
#1531 = CARTESIAN_POINT ( 'NONE',  ( -8.093517052318336624, -79.35576814611899010, 4.979337055998752426 ) ) ;
#1532 = CIRCLE ( 'NONE', #49613, 10.20000000000000107 ) ;
#1533 = CARTESIAN_POINT ( 'NONE',  ( 10.01749676171999859, -59.99181054660999735, 7.660430254678000317 ) ) ;
#1534 = DIRECTION ( 'NONE',  ( 0.000000000000000000, 0.000000000000000000, -1.000000000000000000 ) ) ;
#1535 = CARTESIAN_POINT ( 'NONE',  ( 3.925131995945446928, -78.39834014880939606, 11.31871592374366031 ) ) ;
#1536 = CARTESIAN_POINT ( 'NONE',  ( -9.735611069857000643, -79.22474541096200085, 5.570995215215999607 ) ) ;
#1537 = EDGE_CURVE ( 'NONE', #26186, #2183, #11950, .T. ) ;
#1538 = VERTEX_POINT ( 'NONE', #8091 ) ;
#1539 = CARTESIAN_POINT ( 'NONE',  ( 0.000000000000000000, -74.80000000000001137, 0.000000000000000000 ) ) ;
#1540 = ORIENTED_EDGE ( 'NONE', *, *, #15656, .T. ) ;
#1541 = CARTESIAN_POINT ( 'NONE',  ( 8.744325593625859483, -77.37646171839476494, 3.016781543199777094 ) ) ;
#1542 = CARTESIAN_POINT ( 'NONE',  ( -1.247892825656000015, -79.25449142225700427, -0.1947040076506000028 ) ) ;
#1543 = FACE_OUTER_BOUND ( 'NONE', #16314, .T. ) ;
#1544 = CARTESIAN_POINT ( 'NONE',  ( 4.545264886168000729, -77.72666356161099088, 8.573871732259998879 ) ) ;
#1545 = FACE_OUTER_BOUND ( 'NONE', #50328, .T. ) ;
#1546 = CARTESIAN_POINT ( 'NONE',  ( -6.043427764450784778, -78.48333333333333428, -10.48543666025109822 ) ) ;
#1547 = CARTESIAN_POINT ( 'NONE',  ( -0.6580604922749000441, -79.48068756757000131, -1.488334326434000099 ) ) ;
#1548 = CARTESIAN_POINT ( 'NONE',  ( -0.4361047888467999845, -80.56882046129099706, -4.149259901320998978 ) ) ;
#1549 = CARTESIAN_POINT ( 'NONE',  ( -6.447812191272999982, -78.91764840355199340, 8.972380486426999369 ) ) ;
#1550 = CARTESIAN_POINT ( 'NONE',  ( -7.646092217281999837, -23.70851177913000285, -10.13691708057999996 ) ) ;
#1551 = CARTESIAN_POINT ( 'NONE',  ( 12.60552511008000032, -55.51082276539999327, -1.799501877793999949 ) ) ;
#1552 = CARTESIAN_POINT ( 'NONE',  ( -2.265281180526000249, -84.43400986860198998, 2.726439490990999914 ) ) ;
#1553 = ORIENTED_EDGE ( 'NONE', *, *, #47173, .F. ) ;
#1554 = PLANE ( 'NONE',  #49481 ) ;
#1555 = CARTESIAN_POINT ( 'NONE',  ( -1.478021081765000133, -80.28866583923000633, 0.8457367421919999018 ) ) ;
#1556 = CARTESIAN_POINT ( 'NONE',  ( 10.44750279757892208, -77.86896311195575038, 2.532177459664171515 ) ) ;
#1557 = CARTESIAN_POINT ( 'NONE',  ( -4.743879332790999825, -78.65870616202899157, -11.00053059214000051 ) ) ;
#1558 = CARTESIAN_POINT ( 'NONE',  ( -7.761025538858000061, -17.91850014421000026, 9.835174270523999951 ) ) ;
#1559 = CARTESIAN_POINT ( 'NONE',  ( 0.7505602511881427352, -77.92510946887425405, -1.030241528371574677 ) ) ;
#1560 = CARTESIAN_POINT ( 'NONE',  ( 3.432173245281677776, -3.481906583660260068, -0.7953295766101289299 ) ) ;
#1561 = CARTESIAN_POINT ( 'NONE',  ( 10.56032766684168145, -80.86570825649420158, 2.052053817749484033 ) ) ;
#1562 = CARTESIAN_POINT ( 'NONE',  ( -9.411482030169999291, -78.58077255621898871, -0.1876179646513999877 ) ) ;
#1563 = CARTESIAN_POINT ( 'NONE',  ( 0.4002886859638069006, -86.07389998728979208, -8.935310233444662131 ) ) ;
#1564 = CARTESIAN_POINT ( 'NONE',  ( 5.176319218327999572, -78.12272937556599572, -9.742045664616000522 ) ) ;
#1565 = CARTESIAN_POINT ( 'NONE',  ( 3.350260413882198751, -0.8997395809787506193, -0.4376960103309309735 ) ) ;
#1566 = CARTESIAN_POINT ( 'NONE',  ( 7.215203368301000175, -80.84409233149752083, 8.184401438574999688 ) ) ;
#1567 = VERTEX_POINT ( 'NONE', #3093 ) ;
#1568 = CYLINDRICAL_SURFACE ( 'NONE', #18933, 1.000000000000000000 ) ;
#1569 = CARTESIAN_POINT ( 'NONE',  ( -1.288488638071999981, -61.33564939335000332, -12.54709296486000092 ) ) ;
#1570 = CARTESIAN_POINT ( 'NONE',  ( 9.329667775425885878, -80.39183487745914647, 5.387493164505086085 ) ) ;
#1571 = CARTESIAN_POINT ( 'NONE',  ( -7.712695008784000272, -77.33077202068200506, -8.144473358846001432 ) ) ;
#1572 = CARTESIAN_POINT ( 'NONE',  ( -2.169167664939000151, -78.26068007878699007, 10.75912301088999889 ) ) ;
#1573 = DIRECTION ( 'NONE',  ( 0.000000000000000000, -1.000000000000000000, 0.000000000000000000 ) ) ;
#1574 = CARTESIAN_POINT ( 'NONE',  ( -2.959121675647450989, -86.02291668546635606, 2.710146891174588291 ) ) ;
#1575 = DIRECTION ( 'NONE',  ( -0.7071067811865475727, 0.000000000000000000, 0.7071067811865475727 ) ) ;
#1576 = CARTESIAN_POINT ( 'NONE',  ( 7.601397897754999633, -60.04999999966999980, 9.369164850722000892 ) ) ;
#1577 = VECTOR ( 'NONE', #43379, 1000.000000000000114 ) ;
#1578 = EDGE_CURVE ( 'NONE', #53933, #18065, #51819, .T. ) ;
#1579 = CARTESIAN_POINT ( 'NONE',  ( -4.137408106676000230, -84.71844503318800434, -0.5402929373543000624 ) ) ;
#1580 = DIRECTION ( 'NONE',  ( -1.000000000000000000, 0.000000000000000000, 0.000000000000000000 ) ) ;
#1581 = AXIS2_PLACEMENT_3D ( 'NONE', #4302, #35280, #26150 ) ;
#1582 = EDGE_CURVE ( 'NONE', #30942, #30461, #15044, .T. ) ;
#1583 = CARTESIAN_POINT ( 'NONE',  ( 8.220399303298000504, -53.98050618241000365, -9.523318109972001011 ) ) ;
#1584 = AXIS2_PLACEMENT_3D ( 'NONE', #55642, #9900, #14892 ) ;
#1585 = CARTESIAN_POINT ( 'NONE',  ( 9.267785752250999209, -77.88273556822998955, -6.128505448192000493 ) ) ;
#1586 = CARTESIAN_POINT ( 'NONE',  ( 1.520902128651999918, -81.04615961563999349, -0.6797894616744000196 ) ) ;
#1587 = CARTESIAN_POINT ( 'NONE',  ( -0.7899273271878000102, -77.87807433275999358, 1.197381041534999913 ) ) ;
#1588 = DIRECTION ( 'NONE',  ( 0.000000000000000000, 1.000000000000000000, 1.898821519315000128E-14 ) ) ;
#1589 = CYLINDRICAL_SURFACE ( 'NONE', #17101, 1.500000000000000000 ) ;
#1590 = DIRECTION ( 'NONE',  ( -1.000000000000000000, 0.000000000000000000, 0.000000000000000000 ) ) ;
#1591 = ORIENTED_EDGE ( 'NONE', *, *, #32952, .F. ) ;
#1592 = CARTESIAN_POINT ( 'NONE',  ( 1.008924559857650838, -79.79982627189708921, -0.7395781483535016632 ) ) ;
#1593 = CARTESIAN_POINT ( 'NONE',  ( -9.164374456753368037, -53.58432317374141007, 8.803712804513708079 ) ) ;
#1594 = VERTEX_POINT ( 'NONE', #11378 ) ;
#1595 = CARTESIAN_POINT ( 'NONE',  ( -0.6881529071261847097, -81.67893781361996730, -1.045368128735210345 ) ) ;
#1596 = CARTESIAN_POINT ( 'NONE',  ( -1.751509483276000090, -80.07117545184989638, -10.89192126806999994 ) ) ;
#1597 = CARTESIAN_POINT ( 'NONE',  ( -8.061017305527000687, -55.64999999967000122, -8.909545442949999838 ) ) ;
#1598 = EDGE_LOOP ( 'NONE', ( #30301, #26182, #32852, #20081 ) ) ;
#1599 = ORIENTED_EDGE ( 'NONE', *, *, #8311, .T. ) ;
#1600 = CARTESIAN_POINT ( 'NONE',  ( 1.388711894915000133, -81.26444455407199996, -0.6086225636969000430 ) ) ;
#1601 = EDGE_CURVE ( 'NONE', #6077, #42913, #31029, .T. ) ;
#1602 = ORIENTED_EDGE ( 'NONE', *, *, #43595, .T. ) ;
#1603 = VERTEX_POINT ( 'NONE', #57101 ) ;
#1604 = CARTESIAN_POINT ( 'NONE',  ( -0.7554284705563544255, -81.91666666667600794, 1.310679582531384169 ) ) ;
#1605 = DIRECTION ( 'NONE',  ( 0.000000000000000000, 1.000000000000000000, 0.000000000000000000 ) ) ;
#1606 = SHAPE_DEFINITION_REPRESENTATION ( #29966, #7879 ) ;
#1607 = CARTESIAN_POINT ( 'NONE',  ( 2.124321423109925444, -81.16666665424342852, 2.711257319178282277 ) ) ;
#1608 = CARTESIAN_POINT ( 'NONE',  ( 7.265173101945999967, -78.12837668086899612, 6.414655419558000560 ) ) ;
#1609 = CARTESIAN_POINT ( 'NONE',  ( 6.558477970958472625, -78.28771851464713905, -6.522947137475199497 ) ) ;
#1610 = CARTESIAN_POINT ( 'NONE',  ( 10.34999999999999964, -82.00000000000000000, 0.000000000000000000 ) ) ;
#1611 = EDGE_CURVE ( 'NONE', #3961, #32937, #13372, .T. ) ;
#1612 = ORIENTED_EDGE ( 'NONE', *, *, #744, .T. ) ;
#1613 = VERTEX_POINT ( 'NONE', #15795 ) ;
#1614 = CARTESIAN_POINT ( 'NONE',  ( 12.56594317991999965, -60.04999999381999487, 1.750000000001000089 ) ) ;
#1615 = DIRECTION ( 'NONE',  ( 0.000000000000000000, 0.000000000000000000, -1.000000000000000000 ) ) ;
#1616 = CARTESIAN_POINT ( 'NONE',  ( -0.1963495408493673433, -79.38541666666668561, 1.499999999999999334 ) ) ;
#1617 = EDGE_CURVE ( 'NONE', #32631, #55158, #12186, .T. ) ;
#1618 = CIRCLE ( 'NONE', #53470, 5.000000000000000888 ) ;
#1619 = CARTESIAN_POINT ( 'NONE',  ( -1.495357591794768792, -61.35876337328221553, -12.70444646763206187 ) ) ;
#1620 = CARTESIAN_POINT ( 'NONE',  ( 9.051070938631999852, -77.54921005201198625, 3.499832029064999794 ) ) ;
#1621 = CARTESIAN_POINT ( 'NONE',  ( 1.750000000000000000, -23.24999999758999536, 12.50000000000000000 ) ) ;
#1622 = CARTESIAN_POINT ( 'NONE',  ( -10.35845608625999859, -23.29778754190000001, 7.627487525415999947 ) ) ;
#1623 = VECTOR ( 'NONE', #17349, 1000.000000000000000 ) ;
#1624 = CARTESIAN_POINT ( 'NONE',  ( -12.00000000000000000, -77.29999999999999716, 0.000000000000000000 ) ) ;
#1625 = CARTESIAN_POINT ( 'NONE',  ( -0.4634070002434999558, -79.17548989939000137, -1.170148800580000037 ) ) ;
#1626 = CARTESIAN_POINT ( 'NONE',  ( 8.414570695956999913, -55.64999999967000122, 8.414570695956999913 ) ) ;
#1627 = CARTESIAN_POINT ( 'NONE',  ( -7.814543345298289978, -76.63258160818318743, 8.778123181643341155 ) ) ;
#1628 = CARTESIAN_POINT ( 'NONE',  ( 3.793743692741000206, -79.33493425789589537, -1.737118776092000161 ) ) ;
#1629 = AXIS2_PLACEMENT_3D ( 'NONE', #41502, #32619, #24074 ) ;
#1630 = CARTESIAN_POINT ( 'NONE',  ( -10.18114972180999978, -55.40990354248999950, 7.633087078966999783 ) ) ;
#1631 = CARTESIAN_POINT ( 'NONE',  ( -9.595602112029999020, -78.08161001420199909, -1.328770664336999863 ) ) ;
#1632 = CARTESIAN_POINT ( 'NONE',  ( -10.75000000000000000, -76.59999999999999432, 0.000000000000000000 ) ) ;
#1633 = CARTESIAN_POINT ( 'NONE',  ( 1.930989144707000005, -20.24634220924000161, -12.80900240957999969 ) ) ;
#1635 = CARTESIAN_POINT ( 'NONE',  ( 0.5045596072230998930, -16.86471086961999788, -12.66210649709999991 ) ) ;
#1634 = CARTESIAN_POINT ( 'NONE',  ( -7.954951288349001004, -55.35321828636000419, 9.722718241315000398 ) ) ;
#1636 = ADVANCED_FACE ( 'NONE', ( #3379 ), #43531, .F. ) ;
#1637 = DIRECTION ( 'NONE',  ( 0.000000000000000000, 1.000000000000000000, 0.000000000000000000 ) ) ;
#1638 = DIRECTION ( 'NONE',  ( 0.000000000000000000, 1.000000000000000000, 0.000000000000000000 ) ) ;
#1639 = CARTESIAN_POINT ( 'NONE',  ( 0.000000000000000000, -80.79999999999999716, -9.000000000000000000 ) ) ;
#1640 = CARTESIAN_POINT ( 'NONE',  ( 3.469760739495959978, -77.20000000000000284, -10.38643556155824577 ) ) ;
#1641 = ORIENTED_EDGE ( 'NONE', *, *, #1869, .F. ) ;
#1642 = CARTESIAN_POINT ( 'NONE',  ( -1.729821627806567008, -3.500000000000000000, -2.913428096262390632 ) ) ;
#1643 = B_SPLINE_CURVE_WITH_KNOTS ( 'NONE', 3,
 ( #34375, #34084, #11680, #11964, #12528, #39107, #29655, #47707, #7236, #25241, #29940, #52690, #3108, #7529, #25527, #30236, #48279, #7815, #43844, #3391, #39399, #57408, #16965, #31391, #10665, #22555, #58278, #40566, #33064, #37502, #5921, #51111, #13982, #1516, #26967, #40265, #50817, #28345, #49431, #4257, #28642, #26670, #31093, #39968, #46395, #22254, #19508, #46692, #15069, #9273, #17841, #4553, #44702, #55521, #10360, #49130, #23926, #54446, #35829, #41945, #159, #57982, #13687, #18135, #21956 ),
 .UNSPECIFIED., .F., .F.,
 ( 4, 1, 1, 1, 1, 1, 1, 1, 1, 1, 1, 1, 1, 1, 1, 1, 1, 1, 1, 1, 1, 1, 1, 1, 1, 1, 1, 1, 1, 1, 1, 1, 1, 1, 1, 1, 1, 1, 1, 1, 1, 1, 1, 1, 1, 1, 1, 1, 1, 1, 1, 1, 1, 1, 1, 1, 1, 1, 1, 1, 1, 1, 4 ),
 ( 0.000000000000000000, 0.01249977918653635833, 0.02874978664248438107, 0.04499979409843239686, 0.06124980155438042306, 0.07749980901032844927, 0.09374981646627647547, 0.1099998239222245017, 0.1262498313781725279, 0.1424998388341205402, 0.1587498462900685803, 0.1749998537460165648, 0.1912498612019646049, 0.2074998686579126173, 0.2237498761138606573, 0.2399998835698086697, 0.2562498910257566265, 0.2724998984817046943, 0.2887499059376527066, 0.3049999133936007190, 0.3212499208495487313, 0.3374999283054967991, 0.3537499357614448114, 0.3699999432173928238, 0.3862499506733408361, 0.4024999581292889039, 0.4187499655852369163, 0.4349999730411849286, 0.4512499804971329409, 0.4674999879530810087, 0.4837499954090290211, 0.5000000028649770334, 0.5162500103209249902, 0.5325000177768730580, 0.5487500252328210149, 0.5650000326887690827, 0.5812500401447171505, 0.5975000476006652184, 0.6137500550566131752, 0.6300000625125612430, 0.6462500699685091998, 0.6625000774244572677, 0.6787500848804052245, 0.6950000923363532923, 0.7112500997923013601, 0.7275001072482493170, 0.7437501147041973848, 0.7600001221601453416, 0.7762501296160934094, 0.7925001370720413663, 0.8087501445279894341, 0.8250001519839373909, 0.8412501594398855698, 0.8575001668958335266, 0.8737501743517815944, 0.8900001818077295512, 0.9062501892636776191, 0.9225001967196255759, 0.9387502041755736437, 0.9550002116315216005, 0.9712502190874696684, 0.9875002265434177362, 1.000000000000000000 ),
 .UNSPECIFIED. ) ;
#1644 = CARTESIAN_POINT ( 'NONE',  ( -0.4820079653506728623, -18.48385402702410119, -10.98957811953281904 ) ) ;
#1645 = CARTESIAN_POINT ( 'NONE',  ( 6.760013919724070064, -79.02291666666666003, 8.796335266379978535 ) ) ;
#1646 = CARTESIAN_POINT ( 'NONE',  ( 0.1128515190273495367, -78.46792679642489077, 1.249931857778512345 ) ) ;
#1647 = CARTESIAN_POINT ( 'NONE',  ( 1.640398859540999954, -80.09569838644598860, -9.391438764149000917 ) ) ;
#1648 = CARTESIAN_POINT ( 'NONE',  ( 7.349802007153999561, -77.62076194170001031, -10.73869877321999944 ) ) ;
#1649 = CARTESIAN_POINT ( 'NONE',  ( 10.75346375278748745, -79.35200905115739545, 0.2566943562741798579 ) ) ;
#1650 = CARTESIAN_POINT ( 'NONE',  ( 1.848914204786999971, -79.30291332859900422, 9.561723555723999013 ) ) ;
#1651 = ADVANCED_FACE ( 'NONE', ( #6935 ), #57395, .F. ) ;
#1652 = CARTESIAN_POINT ( 'NONE',  ( 0.000000000000000000, -79.79999999999999716, -9.199999999999999289 ) ) ;
#1653 = CARTESIAN_POINT ( 'NONE',  ( -8.051994348227001552, -77.30396459359899097, -7.735023745693999864 ) ) ;
#1654 = CARTESIAN_POINT ( 'NONE',  ( 1.426927307065000150, -81.12030275061700024, -0.7328213294338999928 ) ) ;
#1655 = DIRECTION ( 'NONE',  ( 0.000000000000000000, 1.000000000000000000, 0.000000000000000000 ) ) ;
#1656 = CARTESIAN_POINT ( 'NONE',  ( -5.004442145019999622, -77.60120832211899256, -7.972877152348999630 ) ) ;
#1658 = CARTESIAN_POINT ( 'NONE',  ( 7.655983890326024444, -55.09663439855413714, 10.06694524866116147 ) ) ;
#1657 = CARTESIAN_POINT ( 'NONE',  ( 2.151616641007000119, -84.90729426542299052, -3.328142986482999888 ) ) ;
#1659 = CARTESIAN_POINT ( 'NONE',  ( -6.090475762158000350, -79.49994805011499466, 7.362120511650999788 ) ) ;
#1660 = CARTESIAN_POINT ( 'NONE',  ( 0.1963495408493571848, -80.76458333333334849, 1.500000000000000666 ) ) ;
#1661 = CARTESIAN_POINT ( 'NONE',  ( 10.75000000000000000, -80.34999999999999432, 0.000000000000000000 ) ) ;
#1662 = VECTOR ( 'NONE', #23671, 1000.000000000000000 ) ;
#1663 = DIRECTION ( 'NONE',  ( -1.000000000000000000, 0.000000000000000000, 0.000000000000000000 ) ) ;
#1664 = DIRECTION ( 'NONE',  ( 0.000000000000000000, 0.000000000000000000, -1.000000000000000000 ) ) ;
#1665 = ORIENTED_EDGE ( 'NONE', *, *, #51212, .F. ) ;
#1666 = ORIENTED_EDGE ( 'NONE', *, *, #14435, .T. ) ;
#1667 = CARTESIAN_POINT ( 'NONE',  ( 7.520016693046000178, -79.81263331077090584, -9.389162645085001202 ) ) ;
#1668 = CARTESIAN_POINT ( 'NONE',  ( 0.7677661701836960839, -78.27713689064573543, -0.9989898656190768778 ) ) ;
#1669 = CARTESIAN_POINT ( 'NONE',  ( 0.000000000000000000, -87.15000000002500258, 0.000000000000000000 ) ) ;
#1670 = VECTOR ( 'NONE', #32559, 1000.000000000000000 ) ;
#1671 = ORIENTED_EDGE ( 'NONE', *, *, #7254, .T. ) ;
#1672 = CARTESIAN_POINT ( 'NONE',  ( 2.687462146607000335, -77.76648380221600121, -11.62811462177000088 ) ) ;
#1673 = ORIENTED_EDGE ( 'NONE', *, *, #15183, .F. ) ;
#1674 = ORIENTED_EDGE ( 'NONE', *, *, #38865, .T. ) ;
#1675 = CARTESIAN_POINT ( 'NONE',  ( 7.889735440107603637, -60.55042584425824259, 7.666647577135394798 ) ) ;
#1676 = CIRCLE ( 'NONE', #40298, 12.80000000000000071 ) ;
#1677 = VERTEX_POINT ( 'NONE', #34934 ) ;
#1678 = CARTESIAN_POINT ( 'NONE',  ( -2.502852178527999794, -81.49944189855800403, 2.513424115303000139 ) ) ;
#1679 = CARTESIAN_POINT ( 'NONE',  ( 7.689480989199970473, -79.19964970209089472, 5.578385363880753012 ) ) ;
#1680 = ORIENTED_EDGE ( 'NONE', *, *, #30027, .T. ) ;
#1681 = DIRECTION ( 'NONE',  ( 0.000000000000000000, -1.000000000000000000, 0.000000000000000000 ) ) ;
#1682 = CARTESIAN_POINT ( 'NONE',  ( -7.655555357447999754, -59.57795407677000554, 10.38646360829999971 ) ) ;
#1683 = ORIENTED_EDGE ( 'NONE', *, *, #42399, .F. ) ;
#1684 = CARTESIAN_POINT ( 'NONE',  ( -1.249681228189473803, -79.59559394467255800, 0.07758196913156252539 ) ) ;
#1685 = CARTESIAN_POINT ( 'NONE',  ( -0.6712347860653230525, -78.16172226271685020, 1.350201467282728274 ) ) ;
#1686 = DIRECTION ( 'NONE',  ( 0.000000000000000000, 1.000000000000000000, 0.000000000000000000 ) ) ;
#1687 = CARTESIAN_POINT ( 'NONE',  ( -10.61294613146216115, -80.08761099959438923, 1.709916667674025392 ) ) ;
#1688 = CARTESIAN_POINT ( 'NONE',  ( 1.514295266944117202, -0.9609374997565883758, 2.965304924911553286 ) ) ;
#1689 = CARTESIAN_POINT ( 'NONE',  ( 7.658860137759998743, -78.55261983880677690, 5.959242465009999989 ) ) ;
#1690 = CARTESIAN_POINT ( 'NONE',  ( 9.886069181790999139, -76.40960291063299792, -5.228720670581999741 ) ) ;
#1691 = CARTESIAN_POINT ( 'NONE',  ( 9.470019493006097022, -76.39166030756085490, 5.309339906474421333 ) ) ;
#1692 = CARTESIAN_POINT ( 'NONE',  ( -7.612971414731999786, -60.12452529330000317, -10.53003223724999948 ) ) ;
#1693 = CARTESIAN_POINT ( 'NONE',  ( -7.826484408841155371, -78.64491150884613546, -4.930180270834215506 ) ) ;
#1694 = CARTESIAN_POINT ( 'NONE',  ( 4.595623807310805553, -76.54268455229363610, 10.81386401082669302 ) ) ;
#1695 = CARTESIAN_POINT ( 'NONE',  ( 8.533343070146999665, -77.28601001420200589, -3.969738581741999450 ) ) ;
#1696 = CYLINDRICAL_SURFACE ( 'NONE', #3139, 1.000000000000000000 ) ;
#1697 = CARTESIAN_POINT ( 'NONE',  ( -3.823994368487737994, -80.19708611470613846, -10.32339281103722328 ) ) ;
#1698 = CARTESIAN_POINT ( 'NONE',  ( -3.069186940681134068, -3.074782183695690563, 1.066787720914930793 ) ) ;
#1699 = CARTESIAN_POINT ( 'NONE',  ( 2.137066360725999647, -79.03892549782628407, -2.883865937898999920 ) ) ;
#1700 = CARTESIAN_POINT ( 'NONE',  ( 6.799660072434999591, -77.38031332859900147, -6.851122554325000280 ) ) ;
#1701 = CARTESIAN_POINT ( 'NONE',  ( -9.947467367995102450, -78.06912791544839081, 4.075482521126458479 ) ) ;
#1702 = ADVANCED_FACE ( 'NONE', ( #52967 ), #24938, .F. ) ;
#1703 = CARTESIAN_POINT ( 'NONE',  ( 0.4639973262319513347, -82.94477574862143854, 1.160677889351085623 ) ) ;
#1704 = CARTESIAN_POINT ( 'NONE',  ( -3.778552491321000240, -78.99318692756679638, -1.585466545969598184E-14 ) ) ;
#1705 = CARTESIAN_POINT ( 'NONE',  ( -8.748876674203279080, -76.25764068747936619, -7.844724932001823525 ) ) ;
#1706 = CARTESIAN_POINT ( 'NONE',  ( 0.7369903609914696396, -80.00000000000000000, 9.280290198084212960 ) ) ;
#1707 = B_SPLINE_SURFACE_WITH_KNOTS ( 'NONE', 3, 3, ( 
 ( #44007, #38, #17722, #54031 ),
 ( #7983, #35403, #57286, #25981 ),
 ( #57568, #17132, #35115, #53149 ),
 ( #12696, #30691, #8271, #26273 ),
 ( #44287, #17417, #18889, #10035 ),
 ( #41906, #36303, #45770, #332 ),
 ( #27140, #41322, #622, #907 ),
 ( #45181, #36882, #32729, #55189 ) ),
 .UNSPECIFIED., .F., .F., .F.,
 ( 4, 1, 1, 1, 1, 4 ),
 ( 4, 4 ),
 ( -0.01200407347462000007, 0.000000000000000000, 0.3333333333333000081, 0.6666666666667000474, 1.000000000000000000, 1.011997855551999947 ),
 ( -0.3559705542741999906, 1.355970554273999928 ),
 .UNSPECIFIED. ) ;
#1708 = CARTESIAN_POINT ( 'NONE',  ( 0.9356112518272206025, -24.74107830239327299, 12.50329130247346221 ) ) ;
#1709 = DIRECTION ( 'NONE',  ( 0.000000000000000000, 1.000000000000000000, 0.000000000000000000 ) ) ;
#1710 = AXIS2_PLACEMENT_3D ( 'NONE', #14779, #1816, #28063 ) ;
#1711 = CARTESIAN_POINT ( 'NONE',  ( -0.8719406389885000497, -81.20263150142500308, -1.009106372638000071 ) ) ;
#1712 = DIRECTION ( 'NONE',  ( -0.7071067811865475727, 0.000000000000000000, -0.7071067811865475727 ) ) ;
#1713 = CARTESIAN_POINT ( 'NONE',  ( -3.039602602086000083, -79.10954415034599663, -9.236151215514999180 ) ) ;
#1714 = DIRECTION ( 'NONE',  ( -0.7071067811865975328, 0.7071067811864976127, -4.569514892260985645E-09 ) ) ;
#1715 = CARTESIAN_POINT ( 'NONE',  ( 1.092232985442823212, -80.70833333333331439, -0.6295237254636224522 ) ) ;
#1716 = CARTESIAN_POINT ( 'NONE',  ( 6.075386672233462626, -78.12318722923399150, -8.895901220742821636 ) ) ;
#1717 = CARTESIAN_POINT ( 'NONE',  ( 7.764656528435081917, -78.37973930036693559, -8.854160864976853063 ) ) ;
#1718 = AXIS2_PLACEMENT_3D ( 'NONE', #37899, #17194, #40515 ) ;
#1719 = CARTESIAN_POINT ( 'NONE',  ( 6.718030245586000149, -79.02741701463656909, -8.679405866825000260 ) ) ;
#1720 = CARTESIAN_POINT ( 'NONE',  ( 6.025108025436000325, -76.50248118292999777, 10.62222322076999959 ) ) ;
#1721 = EDGE_LOOP ( 'NONE', ( #52266, #3590, #38822, #18146 ) ) ;
#1722 = ADVANCED_FACE ( 'NONE', ( #34071 ), #52108, .F. ) ;
#1723 = CARTESIAN_POINT ( 'NONE',  ( 3.766997741046000048, -82.55440783550699280, -1.388142923443000054 ) ) ;
#1724 = CARTESIAN_POINT ( 'NONE',  ( -3.103714625783000169, -80.67352195949028726, 10.97518102889000069 ) ) ;
#1725 = CYLINDRICAL_SURFACE ( 'NONE', #17188, 4.000000000000000000 ) ;
#1726 = CARTESIAN_POINT ( 'NONE',  ( 12.66315196852000113, -61.97802884675999735, -0.06065366946605000448 ) ) ;
#1727 = CARTESIAN_POINT ( 'NONE',  ( -4.531904799951000484, -77.49358547023599897, -10.26060180864999971 ) ) ;
#1728 = CARTESIAN_POINT ( 'NONE',  ( 12.44209697057999975, -54.71557297424000410, -1.464771213333999844 ) ) ;
#1729 = CARTESIAN_POINT ( 'NONE',  ( -3.549595971449000409, -78.23387214450998783, 9.069733410961998032 ) ) ;
#1730 = CARTESIAN_POINT ( 'NONE',  ( -0.8074440912466001041, -83.54732435840999472, -4.093237021270000220 ) ) ;
#1731 = DIRECTION ( 'NONE',  ( -0.9999999999999998890, 1.433665241479999788E-08, 0.000000000000000000 ) ) ;
#1732 = CARTESIAN_POINT ( 'NONE',  ( 11.00000000000000178, -81.00000000000002842, -0.5732958683357214369 ) ) ;
#1733 = ORIENTED_EDGE ( 'NONE', *, *, #18790, .F. ) ;
#1734 = CARTESIAN_POINT ( 'NONE',  ( -12.00000000000000000, -18.84999999997999964, 0.7999999999999001243 ) ) ;
#1735 = CARTESIAN_POINT ( 'NONE',  ( 9.755626371838998168, -80.90664345100368848, -5.633583086437000453 ) ) ;
#1736 = CARTESIAN_POINT ( 'NONE',  ( 2.433585806321822531, -78.97658474417778507, -2.631032898609783288 ) ) ;
#1737 = ADVANCED_FACE ( 'NONE', ( #2804 ), #31377, .F. ) ;
#1738 = ORIENTED_EDGE ( 'NONE', *, *, #53660, .F. ) ;
#1739 = CARTESIAN_POINT ( 'NONE',  ( -1.256362333281000110, -77.66411968718020375, 0.2270125678640999844 ) ) ;
#1740 = EDGE_CURVE ( 'NONE', #34146, #1317, #10335, .T. ) ;
#1741 = DIRECTION ( 'NONE',  ( 0.000000000000000000, 1.000000000000000000, 0.000000000000000000 ) ) ;
#1742 = VERTEX_POINT ( 'NONE', #48830 ) ;
#1743 = CARTESIAN_POINT ( 'NONE',  ( 8.400721904471998513, -78.44452423951798892, -8.798318138657000631 ) ) ;
#1744 = CARTESIAN_POINT ( 'NONE',  ( -8.784718048239000154, -77.61126387770899271, -7.142896292375000122 ) ) ;
#1745 = CARTESIAN_POINT ( 'NONE',  ( -1.009397235748368260, -81.20718188826208461, -0.8706472256294847112 ) ) ;
#1746 = ORIENTED_EDGE ( 'NONE', *, *, #40301, .T. ) ;
#1747 = VERTEX_POINT ( 'NONE', #53544 ) ;
#1748 = AXIS2_PLACEMENT_3D ( 'NONE', #19915, #3558, #48166 ) ;
#1749 = CARTESIAN_POINT ( 'NONE',  ( 12.50745077490000057, -24.99994448286999926, 2.662071812989000278E-09 ) ) ;
#1750 = CARTESIAN_POINT ( 'NONE',  ( 8.582508435409000214, -76.84333998579799641, -4.171307237795000233 ) ) ;
#1751 = CARTESIAN_POINT ( 'NONE',  ( 8.249323304235000265, -80.09549224630299591, -5.229696851825000437 ) ) ;
#1752 = EDGE_LOOP ( 'NONE', ( #3176, #25878, #22986, #48986 ) ) ;
#1753 = CARTESIAN_POINT ( 'NONE',  ( 12.77568125274000010, -53.53490786090000597, 0.5296379231471999294 ) ) ;
#1754 = DIRECTION ( 'NONE',  ( 0.0001230612157847738313, 0.000000000000000000, -0.9999999924279686647 ) ) ;
#1755 = VERTEX_POINT ( 'NONE', #50010 ) ;
#1756 = CARTESIAN_POINT ( 'NONE',  ( -12.46165725306000027, -23.67155322522999938, -1.631637378453000053 ) ) ;
#1757 = CARTESIAN_POINT ( 'NONE',  ( 8.130811096541000538, -24.68523690389000080, 9.546858433121998999 ) ) ;
#1758 = DIRECTION ( 'NONE',  ( 0.000000000000000000, 1.000000000000000000, 0.000000000000000000 ) ) ;
#1759 = TOROIDAL_SURFACE ( 'NONE', #4568, 26.50000000000000000, 14.00000000000000000 ) ;
#1760 = CARTESIAN_POINT ( 'NONE',  ( -0.5573453952815472512, -80.18842898730592594, -1.122125656035228625 ) ) ;
#1761 = DIRECTION ( 'NONE',  ( -0.7071067810866970005, -6.386274622742979319E-09, -0.7071067812863980340 ) ) ;
#1762 = CARTESIAN_POINT ( 'NONE',  ( 1.900228162289573586, -78.40847913613843900, 9.537431829883434631 ) ) ;
#1763 = CARTESIAN_POINT ( 'NONE',  ( -1.834092791198999928, -77.05770150572999455, 9.575395719654000715 ) ) ;
#1764 = CARTESIAN_POINT ( 'NONE',  ( 1.505383061368419151, -79.10597237606836529, 0.1212336400873940262 ) ) ;
#1765 =( REPRESENTATION_RELATIONSHIP ('NONE','NONE', #58051, #46016 ) REPRESENTATION_RELATIONSHIP_WITH_TRANSFORMATION ( #26040 )SHAPE_REPRESENTATION_RELATIONSHIP( ) );
#1766 = CARTESIAN_POINT ( 'NONE',  ( -1.213234814083022917, -81.39791667569573974, 3.866117327208635324 ) ) ;
#1767 = CARTESIAN_POINT ( 'NONE',  ( 3.295079792876999925, -76.33610278377001634, 11.86077433336000020 ) ) ;
#1768 = CARTESIAN_POINT ( 'NONE',  ( -6.606377239730330864, -77.57291666666665719, -8.596418555780440229 ) ) ;
#1769 = CARTESIAN_POINT ( 'NONE',  ( 3.456100946708223542, -2.083958273693990115, -0.6710332831642513707 ) ) ;
#1770 = FACE_OUTER_BOUND ( 'NONE', #2963, .T. ) ;
#1771 = CARTESIAN_POINT ( 'NONE',  ( -4.802691730569000228, -78.35556385665999812, 11.09149278351999968 ) ) ;
#1772 = CARTESIAN_POINT ( 'NONE',  ( -7.650089724727000551, -76.70538068117299701, -9.607224057717001386 ) ) ;
#1773 = CARTESIAN_POINT ( 'NONE',  ( -3.576074390005993475, -85.88547955769999476, 1.592170899228015024 ) ) ;
#1774 = CARTESIAN_POINT ( 'NONE',  ( 2.314286229412385598, -2.788778792593855638, -2.281192321292274894 ) ) ;
#1775 = CARTESIAN_POINT ( 'NONE',  ( 8.405332047648236937, -77.73628230296297659, -8.661069329411425599 ) ) ;
#1776 = CARTESIAN_POINT ( 'NONE',  ( 4.653115705712000505, -78.90904029874850778, -10.20620521156999949 ) ) ;
#1777 = B_SPLINE_CURVE_WITH_KNOTS ( 'NONE', 3,
 ( #32109, #22978, #18559, #18266, #22683, #13818 ),
 .UNSPECIFIED., .F., .F.,
 ( 4, 1, 1, 4 ),
 ( 0.000000000000000000, 0.3333333333333000081, 0.6666666666667000474, 1.000000000000000000 ),
 .UNSPECIFIED. ) ;
#1778 = ORIENTED_EDGE ( 'NONE', *, *, #11133, .F. ) ;
#1779 = CARTESIAN_POINT ( 'NONE',  ( -0.6142531002814000107, -83.43252381223099690, 1.203711489715000305 ) ) ;
#1780 = CARTESIAN_POINT ( 'NONE',  ( 1.500000000000000000, -80.75000000000000000, 0.000000000000000000 ) ) ;
#1781 = CARTESIAN_POINT ( 'NONE',  ( -1.750000000000000000, -23.24999999758999536, -12.50000000000000000 ) ) ;
#1782 = DIRECTION ( 'NONE',  ( 1.000000000000000000, 0.000000000000000000, 0.000000000000000000 ) ) ;
#1783 = CARTESIAN_POINT ( 'NONE',  ( 0.5334547282266999257, -3.244990180630999976, 3.675578036170999763 ) ) ;
#1784 = CARTESIAN_POINT ( 'NONE',  ( 3.268459929338999981, -78.65572260172200458, -11.59797143510999895 ) ) ;
#1785 = CARTESIAN_POINT ( 'NONE',  ( 9.546865209729000767, -78.00495639208598675, -1.927967938976999918 ) ) ;
#1786 = AXIS2_PLACEMENT_3D ( 'NONE', #26851, #36596, #14156 ) ;
#1788 = CARTESIAN_POINT ( 'NONE',  ( 3.747727186550271483, -77.85250684441733426, -10.42547443909606919 ) ) ;
#1787 = CARTESIAN_POINT ( 'NONE',  ( -8.706989617445008989, -76.14134214265790490, 7.890437978471732450 ) ) ;
#1789 = CARTESIAN_POINT ( 'NONE',  ( -0.5525270872808000222, -82.17150394948998837, -1.233160589678000019 ) ) ;
#1790 = ORIENTED_EDGE ( 'NONE', *, *, #40283, .F. ) ;
#1791 = ADVANCED_FACE ( 'NONE', ( #35516 ), #44242, .T. ) ;
#1792 = CARTESIAN_POINT ( 'NONE',  ( 12.74366183107850858, -23.52185227222615183, 1.980611001122018822 ) ) ;
#1793 = FACE_OUTER_BOUND ( 'NONE', #34736, .T. ) ;
#1794 = CARTESIAN_POINT ( 'NONE',  ( -1.997276839918484148, -2.427083333333333481, 2.598917237794077018 ) ) ;
#1795 = CARTESIAN_POINT ( 'NONE',  ( -9.091539081997000338, -78.94313301678198513, 6.148815634104000338 ) ) ;
#1796 = CARTESIAN_POINT ( 'NONE',  ( -1.821913034590999979E-14, -80.79999999999999716, -12.24999999999996980 ) ) ;
#1797 = CARTESIAN_POINT ( 'NONE',  ( 1.463649432154999985, -79.44195468926798753, 9.447158020454001104 ) ) ;
#1798 = CARTESIAN_POINT ( 'NONE',  ( 7.761025538858000061, -17.91850014422000115, -9.835174270523999951 ) ) ;
#1799 = CARTESIAN_POINT ( 'NONE',  ( 0.000000000000000000, -75.15999999999999659, 0.000000000000000000 ) ) ;
#1800 = ORIENTED_EDGE ( 'NONE', *, *, #8778, .F. ) ;
#1801 = CARTESIAN_POINT ( 'NONE',  ( -5.290207344092000774, -78.69050342418300659, 9.942216594703999988 ) ) ;
#1802 = CARTESIAN_POINT ( 'NONE',  ( 8.155100784587984819, -76.15986216400646924, 7.653265680561434969 ) ) ;
#1803 = TOROIDAL_SURFACE ( 'NONE', #34751, 13.50000000000000000, 0.5000000000000000000 ) ;
#1804 = CARTESIAN_POINT ( 'NONE',  ( 12.50386430097127999, -54.01495444323656869, 0.8574444996622476722 ) ) ;
#1805 = ADVANCED_BREP_SHAPE_REPRESENTATION ( '', ( #17895, #43526 ), #24646 ) ;
#1806 = CARTESIAN_POINT ( 'NONE',  ( -13.99609303072000088, -45.84137733103999324, -3.303213538035000172E-05 ) ) ;
#1807 = CARTESIAN_POINT ( 'NONE',  ( -9.420089102920373492, -77.39912871045925158, 7.564612592004372082 ) ) ;
#1808 = CARTESIAN_POINT ( 'NONE',  ( 0.9748194815771379362, -81.40464457030101642, 0.7859197306878139555 ) ) ;
#1809 = EDGE_CURVE ( 'NONE', #22170, #17027, #27255, .T. ) ;
#1810 = CARTESIAN_POINT ( 'NONE',  ( -12.50409217853025190, -54.27871355468437287, 1.233808106764427315 ) ) ;
#1811 = CARTESIAN_POINT ( 'NONE',  ( -7.401644128749154561, -77.00000000000002842, -5.852483073979606765 ) ) ;
#1812 = CARTESIAN_POINT ( 'NONE',  ( 13.98934701867000108, -9.421869816320000979, 1.420930502849999897E-05 ) ) ;
#1813 = CARTESIAN_POINT ( 'NONE',  ( 0.05227849266716000365, -79.20809242846999609, -1.244609249457999889 ) ) ;
#1814 = CARTESIAN_POINT ( 'NONE',  ( -1.980532734072999901, -19.23767313188999850, 12.80090744966999949 ) ) ;
#1815 = CARTESIAN_POINT ( 'NONE',  ( 0.9090516009123569274, -78.81850335718206679, 10.93807314156140542 ) ) ;
#1816 = DIRECTION ( 'NONE',  ( 0.000000000000000000, 1.000000000000000000, 0.000000000000000000 ) ) ;
#1817 = ORIENTED_EDGE ( 'NONE', *, *, #6048, .F. ) ;
#1818 = ORIENTED_EDGE ( 'NONE', *, *, #32581, .T. ) ;
#1819 = CARTESIAN_POINT ( 'NONE',  ( 6.894123566350000232, -77.49915716295998891, -10.09017945751000056 ) ) ;
#1820 = CARTESIAN_POINT ( 'NONE',  ( 9.939632792372378844, -78.81897174444549137, -4.094538100961752747 ) ) ;
#1821 = AXIS2_PLACEMENT_3D ( 'NONE', #11334, #46489, #50906 ) ;
#1822 = ORIENTED_EDGE ( 'NONE', *, *, #37892, .T. ) ;
#1823 = ADVANCED_FACE ( 'NONE', ( #39668 ), #54136, .F. ) ;
#1824 = CARTESIAN_POINT ( 'NONE',  ( 7.619389775686000732, -18.59213701582999789, 10.35398629635000134 ) ) ;
#1825 = AXIS2_PLACEMENT_3D ( 'NONE', #48424, #20395, #7104 ) ;
#1826 = CARTESIAN_POINT ( 'NONE',  ( 1.199500263597268246, -80.20208333333334849, 0.9218200799623752495 ) ) ;
#1827 = CARTESIAN_POINT ( 'NONE',  ( -4.665534009026000462, -78.15194258207000644, 10.77473627194999928 ) ) ;
#1828 = CARTESIAN_POINT ( 'NONE',  ( 9.643350356198000739, -61.74034317005999384, 8.260133465614998727 ) ) ;
#1829 = CARTESIAN_POINT ( 'NONE',  ( -11.00000000000000000, -77.19999999999998863, 5.688460190305999883E-13 ) ) ;
#1830 = CARTESIAN_POINT ( 'NONE',  ( -3.085217259120516697, -78.15417630999539256, -11.57589848832679280 ) ) ;
#1831 = CARTESIAN_POINT ( 'NONE',  ( -11.06493808903000087, -79.34700665024199395, -1.839906431680000010 ) ) ;
#1832 = ORIENTED_EDGE ( 'NONE', *, *, #17700, .T. ) ;
#1833 = DIRECTION ( 'NONE',  ( 0.7071067811865474617, -0.7071067811865474617, 3.010143267812197750E-10 ) ) ;
#1834 = ORIENTED_EDGE ( 'NONE', *, *, #5380, .F. ) ;
#1835 = CARTESIAN_POINT ( 'NONE',  ( 9.215540093376933584, -77.35694448704265369, 0.7975452914727456655 ) ) ;
#1836 = CARTESIAN_POINT ( 'NONE',  ( -0.5413127449341000874, -78.11155102580298148, -11.02683867434999954 ) ) ;
#1837 = VECTOR ( 'NONE', #32904, 1000.000000000000114 ) ;
#1838 = CARTESIAN_POINT ( 'NONE',  ( -10.93323770240847814, -78.36784654652733195, -2.507174414007888430 ) ) ;
#1839 = EDGE_CURVE ( 'NONE', #54390, #24385, #25400, .T. ) ;
#1840 = CARTESIAN_POINT ( 'NONE',  ( -1.347317391812999920, -79.03247803031800345, -0.7577098654840999092 ) ) ;
#1841 = CARTESIAN_POINT ( 'NONE',  ( -8.838834764832000701, -18.75000000000000000, 8.838834764832000701 ) ) ;
#1842 = TOROIDAL_SURFACE ( 'NONE', #25412, 13.50000000000000000, 0.5000000000000000000 ) ;
#1843 = CARTESIAN_POINT ( 'NONE',  ( -0.06603165175717734536, -81.62109302337999850, -1.273657571949194489 ) ) ;
#1844 = CARTESIAN_POINT ( 'NONE',  ( 0.1660104325307999729, -78.25569303241999819, 1.618982269915999916 ) ) ;
#1845 = CARTESIAN_POINT ( 'NONE',  ( 11.04877620194000087, -78.24343189956698552, 0.05135089858452999978 ) ) ;
#1846 = CARTESIAN_POINT ( 'NONE',  ( 10.98362417419999915, -23.15000000000000213, 0.5999999999999999778 ) ) ;
#1847 = CARTESIAN_POINT ( 'NONE',  ( 12.70556836333273409, -62.02772277294081960, 0.2642470008508416290 ) ) ;
#1848 = DIRECTION ( 'NONE',  ( 0.000000000000000000, -1.000000000000000000, 0.000000000000000000 ) ) ;
#1849 = CARTESIAN_POINT ( 'NONE',  ( -0.6865545683297000767, -83.54732435840999472, -3.480402676389000138 ) ) ;
#1850 = ORIENTED_EDGE ( 'NONE', *, *, #25889, .F. ) ;
#1851 = CARTESIAN_POINT ( 'NONE',  ( -10.82422835087974278, -77.20000000000001705, 1.830986660789992504 ) ) ;
#1852 = FACE_OUTER_BOUND ( 'NONE', #12679, .T. ) ;
#1853 = CARTESIAN_POINT ( 'NONE',  ( -2.102085772900874616, -77.99079252367346271, 10.54238248243097686 ) ) ;
#1854 = CARTESIAN_POINT ( 'NONE',  ( 10.99419336675999936, -78.84861136999599296, 4.758540471090999979 ) ) ;
#1855 = CARTESIAN_POINT ( 'NONE',  ( -8.588893914429998944, -16.86760216306999993, 9.317954958010000510 ) ) ;
#1856 = CARTESIAN_POINT ( 'NONE',  ( -2.814036715996205196, -78.99599336343645462, 10.47066865085466958 ) ) ;
#1857 = CARTESIAN_POINT ( 'NONE',  ( 3.354383128917739487, -2.975290926151756832, -1.074698072248829295 ) ) ;
#1858 = CARTESIAN_POINT ( 'NONE',  ( -8.997179024602999675, -79.15920584965400053, 3.687079342327000298 ) ) ;
#1859 = CARTESIAN_POINT ( 'NONE',  ( -6.987523971486999663, -78.63762021447698203, -6.307590925213999888 ) ) ;
#1860 = DIRECTION ( 'NONE',  ( 0.000000000000000000, -1.000000000000000000, 0.000000000000000000 ) ) ;
#1861 = CARTESIAN_POINT ( 'NONE',  ( -6.868829560331000117, -77.38734811451699613, 8.632549730677999023 ) ) ;
#1862 = CARTESIAN_POINT ( 'NONE',  ( 12.24159337356999977, -76.39362091517861586, -0.9828625608234000666 ) ) ;
#1863 = CARTESIAN_POINT ( 'NONE',  ( -9.596002108778161954, -78.35208333333332575, -7.374560639698982456 ) ) ;
#1864 = ORIENTED_EDGE ( 'NONE', *, *, #30051, .T. ) ;
#1865 = CARTESIAN_POINT ( 'NONE',  ( -0.9657971644277000278, -82.32620602178199931, -0.9195906491977999808 ) ) ;
#1866 = EDGE_CURVE ( 'NONE', #50613, #31027, #57970, .T. ) ;
#1867 = CARTESIAN_POINT ( 'NONE',  ( 1.890224871705999954, -60.54789247981999267, -12.68696160876999990 ) ) ;
#1868 = CARTESIAN_POINT ( 'NONE',  ( 10.75087127669428000, -80.36060727671831216, 1.407091297144698938 ) ) ;
#1869 = EDGE_CURVE ( 'NONE', #14050, #10331, #7738, .T. ) ;
#1870 = CARTESIAN_POINT ( 'NONE',  ( 10.75916580684000046, -78.03891693872900248, 3.171507801093999657 ) ) ;
#1871 = CARTESIAN_POINT ( 'NONE',  ( -10.90760146693999921, -78.81840894843499257, -1.219937219691999974 ) ) ;
#1872 = CARTESIAN_POINT ( 'NONE',  ( 8.596763593952999827, -25.13532396123000012, -9.310159863706001460 ) ) ;
#1873 = CARTESIAN_POINT ( 'NONE',  ( -0.9057240420843423179, -85.02083334134603376, -3.948137167706869288 ) ) ;
#1874 = CARTESIAN_POINT ( 'NONE',  ( -9.546819346760001324, -61.48527546573999558, 8.130850182904000079 ) ) ;
#1875 = CARTESIAN_POINT ( 'NONE',  ( -11.79999999999999893, -18.84999999999000053, 0.5999999999999999778 ) ) ;
#1876 = EDGE_LOOP ( 'NONE', ( #7673, #4757, #30532, #1778 ) ) ;
#1877 = CARTESIAN_POINT ( 'NONE',  ( -0.4900037880837543325, -80.00730615406503432, 1.149793150307434342 ) ) ;
#1878 = VECTOR ( 'NONE', #57307, 1000.000000000000000 ) ;
#1879 = CARTESIAN_POINT ( 'NONE',  ( -0.7554284705563544255, -80.41666666666667140, 1.310679582531384169 ) ) ;
#1880 = CARTESIAN_POINT ( 'NONE',  ( 7.606021555054999439, -55.37841460039999930, -10.52692944503000128 ) ) ;
#1881 = EDGE_CURVE ( 'NONE', #7116, #37205, #34789, .T. ) ;
#1882 = CARTESIAN_POINT ( 'NONE',  ( 6.459716167540999976, -77.45020226594600388, -9.225293035625000471 ) ) ;
#1883 = CARTESIAN_POINT ( 'NONE',  ( 1.417725061834000044, -79.97639585000999318, -0.8748226493128999914 ) ) ;
#1884 = CARTESIAN_POINT ( 'NONE',  ( -1.375650254229000113, -77.93375590253999974, 0.4072090767667999600 ) ) ;
#1885 = CARTESIAN_POINT ( 'NONE',  ( 10.98362417419999915, -23.15000000000000213, -0.5999999999999999778 ) ) ;
#1886 = CARTESIAN_POINT ( 'NONE',  ( 1.076979181859827106, -81.43822123321770334, -1.059161443897362664 ) ) ;
#1887 = CIRCLE ( 'NONE', #6584, 13.79999999999999893 ) ;
#1888 = LINE ( 'NONE', #10740, #54428 ) ;
#1889 = CARTESIAN_POINT ( 'NONE',  ( -1.980584515752000119, -18.73514853375999678, -12.76303204602000108 ) ) ;
#1890 = CIRCLE ( 'NONE', #16031, 9.549999999999998934 ) ;
#1891 = CARTESIAN_POINT ( 'NONE',  ( 0.000000000000000000, -13.07071424677999971, 0.000000000000000000 ) ) ;
#1892 = ORIENTED_EDGE ( 'NONE', *, *, #36548, .T. ) ;
#1893 = CARTESIAN_POINT ( 'NONE',  ( -0.4068589336182526495, -81.69886620421327450, -1.181800740598763166 ) ) ;
#1894 = CARTESIAN_POINT ( 'NONE',  ( 10.46019799182000121, -80.23459350986080096, 3.505129431450999977 ) ) ;
#1895 = B_SPLINE_CURVE_WITH_KNOTS ( 'NONE', 3,
 ( #56841, #11971, #44130, #11685, #30534, #51843 ),
 .UNSPECIFIED., .F., .F.,
 ( 4, 2, 4 ),
 ( 0.000000000000000000, 0.5000000000000000000, 1.000000000000000000 ),
 .UNSPECIFIED. ) ;
#1896 = CARTESIAN_POINT ( 'NONE',  ( -1.249999999999999778, -80.01041666666664298, -0.1636246173744686228 ) ) ;
#1897 = VERTEX_POINT ( 'NONE', #18415 ) ;
#1898 = ORIENTED_EDGE ( 'NONE', *, *, #44653, .F. ) ;
#1899 = CARTESIAN_POINT ( 'NONE',  ( -1.340601520916999911, -82.00863390478799886, 0.7083111249264000264 ) ) ;
#1900 = ORIENTED_EDGE ( 'NONE', *, *, #42868, .F. ) ;
#1901 = ORIENTED_EDGE ( 'NONE', *, *, #36924, .F. ) ;
#1902 = CARTESIAN_POINT ( 'NONE',  ( -0.9113424693944999211, -17.17464206440000041, 12.54674099557999867 ) ) ;
#1903 = CARTESIAN_POINT ( 'NONE',  ( 1.250000000000000000, -80.74999999999998579, 0.000000000000000000 ) ) ;
#1904 = APPLICATION_PROTOCOL_DEFINITION ( 'draft international standard', 'automotive_design', 1998, #16063 ) ;
#1905 = CARTESIAN_POINT ( 'NONE',  ( -0.1963495408493605987, -78.11458333333332860, -1.500000000000000444 ) ) ;
#1906 = CARTESIAN_POINT ( 'NONE',  ( -5.674993058560000136, -78.89776001420199236, -8.260872093916999503 ) ) ;
#1907 = CARTESIAN_POINT ( 'NONE',  ( 6.614009670233677696, -78.28839456110405592, -6.466760316368186601 ) ) ;
#1908 = CARTESIAN_POINT ( 'NONE',  ( 1.343749999883000035, -77.90625000011999646, 3.156563468101999814E-09 ) ) ;
#1909 = ORIENTED_EDGE ( 'NONE', *, *, #16619, .F. ) ;
#1910 = AXIS2_PLACEMENT_3D ( 'NONE', #58084, #57214, #26204 ) ;
#1911 = VERTEX_POINT ( 'NONE', #57674 ) ;
#1912 = FACE_OUTER_BOUND ( 'NONE', #13839, .T. ) ;
#1913 = CARTESIAN_POINT ( 'NONE',  ( -12.70722176274329485, -24.41036110618716748, 1.610175936224433002 ) ) ;
#1914 = ADVANCED_FACE ( 'NONE', ( #13969 ), #18807, .F. ) ;
#1915 = CARTESIAN_POINT ( 'NONE',  ( 11.05000000000000071, -81.00000000000000000, 0.000000000000000000 ) ) ;
#1916 = CARTESIAN_POINT ( 'NONE',  ( 4.186942200393000135, -78.43034875501000158, -8.754440266352000677 ) ) ;
#1917 = FACE_OUTER_BOUND ( 'NONE', #16158, .T. ) ;
#1918 = CARTESIAN_POINT ( 'NONE',  ( 0.000000000000000000, -76.00000000000000000, 0.000000000000000000 ) ) ;
#1919 = CARTESIAN_POINT ( 'NONE',  ( 8.743470003752999986, -79.05248508179001021, 7.836700939358999030 ) ) ;
#1920 = CARTESIAN_POINT ( 'NONE',  ( 1.676986109946000170, -79.53386453932999700, 0.2957349343760000138 ) ) ;
#1921 = CARTESIAN_POINT ( 'NONE',  ( -1.500000000000000000, -81.50000000000000000, 0.000000000000000000 ) ) ;
#1922 = CARTESIAN_POINT ( 'NONE',  ( 1.330267261658839351, -76.56584803886862289, 11.68086291702384116 ) ) ;
#1923 = CARTESIAN_POINT ( 'NONE',  ( -3.198047453352999892, -78.84766706549169157, -2.679415071575999896 ) ) ;
#1925 = VECTOR ( 'NONE', #56762, 1000.000000000000000 ) ;
#1924 = CARTESIAN_POINT ( 'NONE',  ( 1.434073767539737476, -79.47461743011145074, -0.4734074842604066302 ) ) ;
#1926 = B_SPLINE_CURVE_WITH_KNOTS ( 'NONE', 3,
 ( #18537, #14092, #32091, #50131, #9673, #9970 ),
 .UNSPECIFIED., .F., .F.,
 ( 4, 2, 4 ),
 ( 0.000000000000000000, 0.4999999999999998890, 1.000000000000000000 ),
 .UNSPECIFIED. ) ;
#1927 = CARTESIAN_POINT ( 'NONE',  ( -0.5292728922702000238, -78.69131001420200278, -9.672698560386999489 ) ) ;
#1928 = CARTESIAN_POINT ( 'NONE',  ( 6.043427764450763462, -77.23333333333330586, 10.48543666025111065 ) ) ;
#1929 = CARTESIAN_POINT ( 'NONE',  ( 1.799501877760999902, -18.71082434677000350, -12.60552522436000089 ) ) ;
#1930 = VECTOR ( 'NONE', #10304, 1000.000000000000114 ) ;
#1932 = CARTESIAN_POINT ( 'NONE',  ( 0.2725326480772000126, -79.12428363588000479, 1.305490477442999842 ) ) ;
#1931 = DIRECTION ( 'NONE',  ( 0.000000000000000000, 1.000000000000000000, 0.000000000000000000 ) ) ;
#1933 = DIRECTION ( 'NONE',  ( 0.000000000000000000, 3.441642669434999888E-11, 1.000000000000000000 ) ) ;
#1934 = DIRECTION ( 'NONE',  ( 0.000000000000000000, -1.000000000000000000, 0.000000000000000000 ) ) ;
#1935 = CARTESIAN_POINT ( 'NONE',  ( -1.209804193477999945, -2.451258720802000024, -3.608664049297999998 ) ) ;
#1936 = CARTESIAN_POINT ( 'NONE',  ( -3.463096647710298903, -1.235411181636255629, 0.6470415087195192649 ) ) ;
#1937 = ORIENTED_EDGE ( 'NONE', *, *, #30455, .T. ) ;
#1938 = CARTESIAN_POINT ( 'NONE',  ( 9.611650271896843734, -78.40833333333330302, -5.539808784079876425 ) ) ;
#1939 = CARTESIAN_POINT ( 'NONE',  ( -0.6999999999999999556, -21.00000000000000000, -11.90000000000000036 ) ) ;
#1940 = CARTESIAN_POINT ( 'NONE',  ( 0.7924526256690966886, -78.42054099154100300, 0.9668092435737775103 ) ) ;
#1941 = EDGE_CURVE ( 'NONE', #51047, #53789, #919, .T. ) ;
#1942 = CARTESIAN_POINT ( 'NONE',  ( -9.629491761460998944, -79.38892416398799412, 0.5011777547001000643 ) ) ;
#1943 = LINE ( 'NONE', #9911, #18716 ) ;
#1944 = DIRECTION ( 'NONE',  ( -0.7071067811865475727, 0.000000000000000000, -0.7071067811865475727 ) ) ;
#1945 = CARTESIAN_POINT ( 'NONE',  ( -1.399903487910991728, -79.48551242492223423, 10.65869450429586962 ) ) ;
#1946 = CARTESIAN_POINT ( 'NONE',  ( -6.239533324134999503, -79.44973998579799002, -7.619964241536999694 ) ) ;
#1947 = FACE_OUTER_BOUND ( 'NONE', #780, .T. ) ;
#1948 = CARTESIAN_POINT ( 'NONE',  ( -7.895114074556000006, -77.43171607516499932, -7.584319138910000646 ) ) ;
#1949 = EDGE_CURVE ( 'NONE', #5424, #31838, #47110, .T. ) ;
#1950 = AXIS2_PLACEMENT_3D ( 'NONE', #10801, #37352, #28487 ) ;
#1951 = CARTESIAN_POINT ( 'NONE',  ( -0.4716608572466999827, -81.25303007584000170, 1.430537295918000051 ) ) ;
#1952 = CARTESIAN_POINT ( 'NONE',  ( 9.377128579935000374, -78.37869514476064126, -2.571625947824999869 ) ) ;
#1953 = CARTESIAN_POINT ( 'NONE',  ( -9.163349670171998085, -78.53919468337598175, -2.155044623588000086 ) ) ;
#1954 = EDGE_CURVE ( 'NONE', #4693, #53569, #56526, .T. ) ;
#1956 = CARTESIAN_POINT ( 'NONE',  ( 0.8506806241676515556, -2.854166666666666963, 3.165411199172028844 ) ) ;
#1955 = CARTESIAN_POINT ( 'NONE',  ( -2.415600723022000462, -83.10353803642099990, -2.876846102162000207 ) ) ;
#1957 = CARTESIAN_POINT ( 'NONE',  ( -2.317989000404999889, -79.73555194988499295, -9.269382932261999386 ) ) ;
#1958 = CARTESIAN_POINT ( 'NONE',  ( -0.3926218265389256890, -80.79583333333334849, 1.460959015002472050 ) ) ;
#1959 = CARTESIAN_POINT ( 'NONE',  ( 10.70855674592274909, -80.34275261640850374, -1.007396462679471805 ) ) ;
#1960 = CARTESIAN_POINT ( 'NONE',  ( -6.227654752595058518, -77.17598872457767811, -8.762225621070838244 ) ) ;
#1961 = CARTESIAN_POINT ( 'NONE',  ( 4.999999999872000167, -80.49999999987198862, -4.857398774947999725E-10 ) ) ;
#1962 = ORIENTED_EDGE ( 'NONE', *, *, #31274, .F. ) ;
#1963 = ORIENTED_EDGE ( 'NONE', *, *, #25227, .F. ) ;
#1964 = CARTESIAN_POINT ( 'NONE',  ( 7.313768098873999257, -78.95596922647499127, 9.313141831727000053 ) ) ;
#1965 = CARTESIAN_POINT ( 'NONE',  ( -5.051502324002999760E-14, -80.79999999999999716, 0.000000000000000000 ) ) ;
#1966 = DIRECTION ( 'NONE',  ( 1.040437577282999923E-11, 1.000000000000000000, -2.038011343141999906E-09 ) ) ;
#1967 = ORIENTED_EDGE ( 'NONE', *, *, #20245, .T. ) ;
#1968 = B_SPLINE_CURVE_WITH_KNOTS ( 'NONE', 3,
 ( #13129, #31125, #31425, #49162, #26706, #40305, #58313, #17875, #23747, #14300, #10472, #28750, #1338, #41761, #15182, #28458, #46506, #6032, #46800, #32588, #5168, #41176, #10772, #24041, #32293, #28162, #33174, #36739, #37615, #55339, #1054, #27584, #5740, #54757, #42056 ),
 .UNSPECIFIED., .F., .F.,
 ( 4, 1, 1, 1, 1, 1, 1, 1, 1, 1, 1, 1, 1, 1, 1, 1, 1, 1, 1, 1, 1, 1, 1, 1, 1, 1, 1, 1, 1, 1, 1, 1, 4 ),
 ( 0.000000000000000000, 0.01250064086135114876, 0.04500059900521829331, 0.07750055714907158610, 0.1100005152929402902, 0.1425004734368089665, 0.1750004315807084654, 0.2075003897244847573, 0.2400003478684150648, 0.2725003060121913845, 0.3050002641561216365, 0.3375002223000519441, 0.3700001804438282638, 0.4025001385877585158, 0.4350000967315347800, 0.4675000548754650875, 0.5000000130192413517, 0.5324999711631716037, 0.5649999293071019668, 0.5974998874508783420, 0.6299998455948085940, 0.6624998037385848582, 0.6949997618825151102, 0.7274997200262914854, 0.7599996781702217374, 0.7924996363141521005, 0.8249995944579283647, 0.8574995526018586167, 0.8899995107456349919, 0.9224994688895652439, 0.9549994270333415081, 0.9874993851772717601, 1.000000000000000000 ),
 .UNSPECIFIED. ) ;
#1969 = CARTESIAN_POINT ( 'NONE',  ( -0.08487245167305000615, -78.49897531865799749, 11.93433278878999992 ) ) ;
#1970 = EDGE_LOOP ( 'NONE', ( #26913, #5398, #49202, #22425, #58036, #56197 ) ) ;
#1971 = EDGE_LOOP ( 'NONE', ( #53330, #3740, #34324, #47946 ) ) ;
#1972 = VECTOR ( 'NONE', #18173, 1000.000000000000000 ) ;
#1973 = ADVANCED_FACE ( 'NONE', ( #17526 ), #8669, .F. ) ;
#1974 = ORIENTED_EDGE ( 'NONE', *, *, #13655, .T. ) ;
#1975 = CARTESIAN_POINT ( 'NONE',  ( -2.719239774786999853, -78.84766706549169157, -2.278256386769999864 ) ) ;
#1976 = CARTESIAN_POINT ( 'NONE',  ( 8.331125690395985828, -79.18975047827684932, 4.575408606511675913 ) ) ;
#1977 = ORIENTED_EDGE ( 'NONE', *, *, #13124, .T. ) ;
#1978 = CARTESIAN_POINT ( 'NONE',  ( -0.6292794791536331367, -82.68371027185608568, -1.092639821175960479 ) ) ;
#1979 = ORIENTED_EDGE ( 'NONE', *, *, #58164, .T. ) ;
#1980 = CARTESIAN_POINT ( 'NONE',  ( -7.613962745591999592, -55.49360215019999742, 10.53101990617999917 ) ) ;
#1981 = ORIENTED_EDGE ( 'NONE', *, *, #44185, .T. ) ;
#1982 = DIRECTION ( 'NONE',  ( 0.000000000000000000, 0.000000000000000000, -1.000000000000000000 ) ) ;
#1983 = CARTESIAN_POINT ( 'NONE',  ( 0.7149329466314869874, -78.08609980630498626, 1.354438294650810892 ) ) ;
#1984 = CARTESIAN_POINT ( 'NONE',  ( 11.34981816413709055, -79.79999999999996874, 3.212464588891036588 ) ) ;
#1985 = ADVANCED_FACE ( 'NONE', ( #13379 ), #26655, .T. ) ;
#1986 = CARTESIAN_POINT ( 'NONE',  ( -0.5999999999999999778, -5.200000000000000178, -4.000000000000000000 ) ) ;
#1987 = CARTESIAN_POINT ( 'NONE',  ( 9.708203932494999577, -79.25000000000000000, 7.053423027515000499 ) ) ;
#1988 = CARTESIAN_POINT ( 'NONE',  ( 0.8618009059429999619, -78.38207686403322327, -9.665816497589000633 ) ) ;
#1989 = CARTESIAN_POINT ( 'NONE',  ( 1.546553306619000256, -76.53772274449399049, -11.07619323537999989 ) ) ;
#1990 = CARTESIAN_POINT ( 'NONE',  ( 10.83694732149156081, -76.34642857556234219, -0.6522557621669171635 ) ) ;
#1991 = ADVANCED_FACE ( 'NONE', ( #46760 ), #55002, .T. ) ;
#1992 = DIRECTION ( 'NONE',  ( 0.000000000000000000, -1.000000000000000000, 0.000000000000000000 ) ) ;
#1993 = CARTESIAN_POINT ( 'NONE',  ( -7.642160924870000649, -56.01538333533000014, -10.55911395186000057 ) ) ;
#1994 = CARTESIAN_POINT ( 'NONE',  ( -8.040862526687783784, -78.64132310946500581, -4.575129970445035887 ) ) ;
#1995 = CARTESIAN_POINT ( 'NONE',  ( 4.502314056123180919, -76.54333886560480948, 10.85294518812557563 ) ) ;
#1996 = AXIS2_PLACEMENT_3D ( 'NONE', #18789, #8756, #54801 ) ;
#1997 = CARTESIAN_POINT ( 'NONE',  ( -7.031989167851816269, -80.17030741383769055, -8.461875502256187787 ) ) ;
#1998 = CARTESIAN_POINT ( 'NONE',  ( 2.486604901413132840, -77.15416666666668277, 9.252740428349005342 ) ) ;
#1999 = CARTESIAN_POINT ( 'NONE',  ( 0.5992999846766000616, -81.80853455456798429, -3.708388589188999607 ) ) ;
#2000 = CARTESIAN_POINT ( 'NONE',  ( 4.607226558409000639, -78.92046296702099539, 11.17099812874999998 ) ) ;
#2001 = CARTESIAN_POINT ( 'NONE',  ( -8.509317581196993885, -78.04784009799371347, 6.570080670988565075 ) ) ;
#2002 = CARTESIAN_POINT ( 'NONE',  ( 0.9590251478797268136, -82.90587166377093808, 0.8014916951292889724 ) ) ;
#2003 = LINE ( 'NONE', #37697, #3765 ) ;
#2004 = DIRECTION ( 'NONE',  ( 0.000000000000000000, -1.000000000000000000, 0.000000000000000000 ) ) ;
#2005 = CARTESIAN_POINT ( 'NONE',  ( -8.485281374238999419, -59.94999999967000548, 8.485281374238999419 ) ) ;
#2006 = CARTESIAN_POINT ( 'NONE',  ( -6.969094100096229205, -79.65772208930626164, -6.112482804795786429 ) ) ;
#2007 = CARTESIAN_POINT ( 'NONE',  ( -0.6509962010243000030, -81.54991986509199364, 1.163950211895000031 ) ) ;
#2008 = VECTOR ( 'NONE', #20832, 1000.000000000000000 ) ;
#2009 = CARTESIAN_POINT ( 'NONE',  ( 0.9186508726441413586, -79.17551408595964801, -1.236643120628077241 ) ) ;
#2010 = CARTESIAN_POINT ( 'NONE',  ( 12.43571054526000097, -24.87980566418999828, 0.4385525234353999657 ) ) ;
#2011 = VECTOR ( 'NONE', #36511, 1000.000000000000000 ) ;
#2012 = CARTESIAN_POINT ( 'NONE',  ( 0.3028628213633383637, -77.57767551470611522, -10.76873991355842008 ) ) ;
#2013 = CARTESIAN_POINT ( 'NONE',  ( 5.209066090324155240, -78.35914083083440573, -10.56088534199699858 ) ) ;
#2014 = CARTESIAN_POINT ( 'NONE',  ( 3.915498778898000687, -79.19597114063257948, 10.25343288338999947 ) ) ;
#2015 = CARTESIAN_POINT ( 'NONE',  ( 5.951017151798000171, -76.58956203265999818, 10.49160152982999961 ) ) ;
#2016 = EDGE_LOOP ( 'NONE', ( #45371, #52569, #19655, #5257 ) ) ;
#2017 = CARTESIAN_POINT ( 'NONE',  ( 3.437035393651000081, -82.51432450217399150, -1.965223482742000316 ) ) ;
#2018 = CARTESIAN_POINT ( 'NONE',  ( -8.360726197242001945, -80.08342291261719481, 7.410943183935000178 ) ) ;
#2019 = CARTESIAN_POINT ( 'NONE',  ( 9.235083398947233846, -78.34478105551114879, -0.6060572195536756412 ) ) ;
#2020 = CARTESIAN_POINT ( 'NONE',  ( 8.532671860860467916, -53.67201063362983859, 9.433519686857682274 ) ) ;
#2021 = CARTESIAN_POINT ( 'NONE',  ( 3.895497176768000003, -77.24845838321999736, 10.51870773133999926 ) ) ;
#2022 = DIRECTION ( 'NONE',  ( 1.000000000000000000, 0.000000000000000000, 0.000000000000000000 ) ) ;
#2023 = CARTESIAN_POINT ( 'NONE',  ( 9.546865209729000767, -78.06332916973599367, -1.927967938976999918 ) ) ;
#2024 = CARTESIAN_POINT ( 'NONE',  ( -1.374853770045000090, -81.42764988327999731, -0.7192078502473999713 ) ) ;
#2025 = CARTESIAN_POINT ( 'NONE',  ( 3.962812355711000212, -78.85171438276199751, 0.000000000000000000 ) ) ;
#2026 = CARTESIAN_POINT ( 'NONE',  ( -1.527286180810999872, -79.00449142225700427, -0.2382966983378000114 ) ) ;
#2027 = ORIENTED_EDGE ( 'NONE', *, *, #34529, .T. ) ;
#2028 = CARTESIAN_POINT ( 'NONE',  ( 1.942774989866609348, -78.95669558350101624, -2.968542881336678985 ) ) ;
#2029 = EDGE_LOOP ( 'NONE', ( #48789, #6811, #30313 ) ) ;
#2030 = CARTESIAN_POINT ( 'NONE',  ( 1.196963559360000096, -78.34799747919070967, -0.5880938590690999446 ) ) ;
#2031 = CARTESIAN_POINT ( 'NONE',  ( -1.306188688584000168, -78.42250824667499387, -10.97140668998000024 ) ) ;
#2032 = CARTESIAN_POINT ( 'NONE',  ( -3.586137557470999937, -80.27811558971397687, -10.61272749461999965 ) ) ;
#2033 = ORIENTED_EDGE ( 'NONE', *, *, #37633, .F. ) ;
#2034 = AXIS2_PLACEMENT_3D ( 'NONE', #39750, #40643, #9350 ) ;
#2035 = CARTESIAN_POINT ( 'NONE',  ( 6.129172116842999785, -78.09184313900898644, 10.50789130831999962 ) ) ;
#2036 = CARTESIAN_POINT ( 'NONE',  ( -2.871267467966999831, -78.16153450768899802, -10.95208408865000216 ) ) ;
#2037 = CARTESIAN_POINT ( 'NONE',  ( 3.042547531669000271, -78.64783470746900207, -10.31045122763999977 ) ) ;
#2038 = ORIENTED_EDGE ( 'NONE', *, *, #42332, .T. ) ;
#2039 = ORIENTED_EDGE ( 'NONE', *, *, #54936, .F. ) ;
#2040 = EDGE_CURVE ( 'NONE', #43546, #45130, #55631, .T. ) ;
#2041 = CARTESIAN_POINT ( 'NONE',  ( -0.04600636030614828342, -80.47847291610720788, 1.248880407862982711 ) ) ;
#2042 = EDGE_CURVE ( 'NONE', #30255, #39723, #43715, .T. ) ;
#2043 = CARTESIAN_POINT ( 'NONE',  ( -6.043427764450832740, -79.71666666666668277, 10.48543666025107512 ) ) ;
#2044 = CARTESIAN_POINT ( 'NONE',  ( 9.226480760116999136, -79.24116534201449724, -2.263195259622999611 ) ) ;
#2045 = ORIENTED_EDGE ( 'NONE', *, *, #38374, .F. ) ;
#2046 = CARTESIAN_POINT ( 'NONE',  ( -12.70451681027687130, -25.17641660207490872, -0.5206746370451510453 ) ) ;
#2047 = CARTESIAN_POINT ( 'NONE',  ( -7.210617325615999995, -79.14099446298800444, -8.196484842528999337 ) ) ;
#2048 = VERTEX_POINT ( 'NONE', #45581 ) ;
#2049 = AXIS2_PLACEMENT_3D ( 'NONE', #57784, #26474, #30619 ) ;
#2050 = CARTESIAN_POINT ( 'NONE',  ( -12.83677138648000060, -23.22737696056999823, -2.062839765281999860 ) ) ;
#2051 = CARTESIAN_POINT ( 'NONE',  ( 9.426477049435000310, -77.25026915034599995, -1.139727483088999849 ) ) ;
#2052 = CIRCLE ( 'NONE', #46344, 5.000000000000000000 ) ;
#2053 = DIRECTION ( 'NONE',  ( -0.7071067811865475727, 0.000000000000000000, 0.7071067811865475727 ) ) ;
#2054 = CARTESIAN_POINT ( 'NONE',  ( 1.308715794663198873, -17.25595500802067406, -12.70256747357078453 ) ) ;
#2055 = CARTESIAN_POINT ( 'NONE',  ( -9.632966741362359642, -78.06007913613844096, -1.333944807945767863 ) ) ;
#2056 = EDGE_CURVE ( 'NONE', #14405, #24318, #19041, .T. ) ;
#2057 = CARTESIAN_POINT ( 'NONE',  ( -6.202661310057998811, -77.14850630154218436, 7.637685261898999656 ) ) ;
#2058 = CARTESIAN_POINT ( 'NONE',  ( -1.279096942007310611, -78.80257488668075894, 0.8515545081673395744 ) ) ;
#2059 = CARTESIAN_POINT ( 'NONE',  ( -10.71369944335147117, -79.62083333333332291, -2.879226727952084453 ) ) ;
#2060 = CARTESIAN_POINT ( 'NONE',  ( -10.62397638184999948, -76.05947304082000926, -6.218250916117999516 ) ) ;
#2061 = CARTESIAN_POINT ( 'NONE',  ( 1.243547092045969915, -78.03541666666666288, -9.500000000000000000 ) ) ;
#2062 = CARTESIAN_POINT ( 'NONE',  ( 10.08161778468999970, -61.51855282861000518, -7.981584069293999661 ) ) ;
#2063 = CARTESIAN_POINT ( 'NONE',  ( 9.889431646000000242, -78.74835367037000822, 7.252463523969000292 ) ) ;
#2064 = CARTESIAN_POINT ( 'NONE',  ( -12.17466003208999936, -76.62341520456298838, 1.612538369963999907 ) ) ;
#2065 = CARTESIAN_POINT ( 'NONE',  ( -9.252740428349007118, -78.87916666666666288, 2.486604901413125734 ) ) ;
#2066 = CARTESIAN_POINT ( 'NONE',  ( 9.756232907440029578, -78.35003554436862316, 7.102215872803408381 ) ) ;
#2067 = CARTESIAN_POINT ( 'NONE',  ( 3.507155896972999898, -79.09969469976067558, 10.65448112794999957 ) ) ;
#2068 = EDGE_CURVE ( 'NONE', #35842, #42334, #57094, .T. ) ;
#2069 = MECHANICAL_DESIGN_GEOMETRIC_PRESENTATION_REPRESENTATION (  '', ( #22777 ), #23708 ) ;
#2070 = ORIENTED_EDGE ( 'NONE', *, *, #1949, .T. ) ;
#2072 = B_SPLINE_CURVE_WITH_KNOTS ( 'NONE', 3,
 ( #17844, #21959, #40860, #26384 ),
 .UNSPECIFIED., .F., .F.,
 ( 4, 4 ),
 ( 0.000000000000000000, 1.000000000000000000 ),
 .UNSPECIFIED. ) ;
#2071 = CARTESIAN_POINT ( 'NONE',  ( -0.6329778402533998705, -82.10618029491999437, -1.193863583722999833 ) ) ;
#2073 = CARTESIAN_POINT ( 'NONE',  ( 11.75000000000000178, -78.03958333333331154, -1.538071403319980268 ) ) ;
#2074 = DIRECTION ( 'NONE',  ( 0.000000000000000000, 1.000000000000000000, 0.000000000000000000 ) ) ;
#2075 = DIRECTION ( 'NONE',  ( 0.000000000000000000, 1.000000000000000000, 0.000000000000000000 ) ) ;
#2076 = CARTESIAN_POINT ( 'NONE',  ( 1.070339692688000000, -2.147081610292000065, 3.719502945170999997 ) ) ;
#2077 = CARTESIAN_POINT ( 'NONE',  ( 7.966054476048999078, -77.32638614595698812, 9.040893068079999040 ) ) ;
#2078 = CARTESIAN_POINT ( 'NONE',  ( -6.791097082272000485, -77.83441341731199259, -6.981453725808999700 ) ) ;
#2080 = CARTESIAN_POINT ( 'NONE',  ( 8.140362823347699006, -77.89063355552166001, -7.514683589434229205 ) ) ;
#2079 = CARTESIAN_POINT ( 'NONE',  ( -11.24578562917078628, -76.17646087094038876, 3.410865946175021257 ) ) ;
#2081 = CARTESIAN_POINT ( 'NONE',  ( -1.596083865962000026, -78.91326708118100441, 10.79943897993000057 ) ) ;
#2082 = CYLINDRICAL_SURFACE ( 'NONE', #50228, 0.6000000000000008660 ) ;
#2083 = ORIENTED_EDGE ( 'NONE', *, *, #26596, .F. ) ;
#2084 = CARTESIAN_POINT ( 'NONE',  ( -11.84062247810999935, -76.52795558657410879, 3.366775603358000080 ) ) ;
#2085 = DIRECTION ( 'NONE',  ( 0.000000000000000000, -1.000000000000000000, 0.000000000000000000 ) ) ;
#2086 = DIRECTION ( 'NONE',  ( -1.000000000000000000, 0.000000000000000000, 0.000000000000000000 ) ) ;
#2087 = CARTESIAN_POINT ( 'NONE',  ( -9.108250977419000805, -61.67811334458999539, 8.478720681770999690 ) ) ;
#2088 = CARTESIAN_POINT ( 'NONE',  ( -10.95971813569178188, -80.09360419250441510, 0.9376767887256405309 ) ) ;
#2089 = CARTESIAN_POINT ( 'NONE',  ( -5.225954845719999575, -80.00216956313799699, 7.590213850110999694 ) ) ;
#2090 = CARTESIAN_POINT ( 'NONE',  ( 0.8495058540349734733, -3.246012347106654428, -3.252519878219170213 ) ) ;
#2091 = FACE_OUTER_BOUND ( 'NONE', #22774, .T. ) ;
#2092 = ORIENTED_EDGE ( 'NONE', *, *, #33501, .T. ) ;
#2093 = AXIS2_PLACEMENT_3D ( 'NONE', #49507, #50097, #22330 ) ;
#2094 = CARTESIAN_POINT ( 'NONE',  ( 9.414214675708999280, -79.48035737123599631, -6.181142822975999707 ) ) ;
#2095 = CARTESIAN_POINT ( 'NONE',  ( -9.831872778489293196, -76.31035381594146827, 5.330330710487904078 ) ) ;
#2096 = CARTESIAN_POINT ( 'NONE',  ( 5.000677505783216681, -78.88963964525443373, 10.65720018581769502 ) ) ;
#2097 = CARTESIAN_POINT ( 'NONE',  ( 3.437187628289000152, -78.54828564506388489, -4.209340827053006789E-16 ) ) ;
#2098 = CARTESIAN_POINT ( 'NONE',  ( 8.408834629392076820, -77.63929640612045091, -8.664705538047067890 ) ) ;
#2099 = CARTESIAN_POINT ( 'NONE',  ( -0.003982218678106667215, -81.47577399763491712, 1.249684034757714279 ) ) ;
#2100 = CARTESIAN_POINT ( 'NONE',  ( -0.9641794813156493449, -78.20655186485167576, -0.8343030551515581150 ) ) ;
#2101 = CARTESIAN_POINT ( 'NONE',  ( 1.093387357835452933, -82.30899171049304641, -0.6298603018139183884 ) ) ;
#2102 = FACE_OUTER_BOUND ( 'NONE', #15724, .T. ) ;
#2103 = CARTESIAN_POINT ( 'NONE',  ( 0.0004826309679763999953, -77.70505409477999592, -1.307959744758000031 ) ) ;
#2104 = CARTESIAN_POINT ( 'NONE',  ( 0.000000000000000000, -91.29999999999999716, 0.000000000000000000 ) ) ;
#2105 = DIRECTION ( 'NONE',  ( 1.000000000000000000, 0.000000000000000000, 0.000000000000000000 ) ) ;
#2106 = DIRECTION ( 'NONE',  ( 0.000000000000000000, 0.000000000000000000, -1.000000000000000000 ) ) ;
#2107 = ORIENTED_EDGE ( 'NONE', *, *, #50023, .T. ) ;
#2108 = ORIENTED_EDGE ( 'NONE', *, *, #13353, .T. ) ;
#2109 = CARTESIAN_POINT ( 'NONE',  ( -9.372585790538636275, -77.88499999999999091, 1.790612804732441221 ) ) ;
#2110 =( REPRESENTATION_RELATIONSHIP ('NONE','NONE', #58051, #7439 ) REPRESENTATION_RELATIONSHIP_WITH_TRANSFORMATION ( #24898 )SHAPE_REPRESENTATION_RELATIONSHIP( ) );
#2111 = CARTESIAN_POINT ( 'NONE',  ( -4.169758043522275415, -78.69350354638132217, -9.910626147760272175 ) ) ;
#2112 = ORIENTED_EDGE ( 'NONE', *, *, #54091, .F. ) ;
#2113 = CARTESIAN_POINT ( 'NONE',  ( 9.996785040898998886, -17.84937852891999910, 7.758588586541999454 ) ) ;
#2114 = CARTESIAN_POINT ( 'NONE',  ( -9.379567534213441249, -79.38691803057906782, 1.514930929802611681 ) ) ;
#2115 = CARTESIAN_POINT ( 'NONE',  ( 8.961184493456999078, -79.22664678124000659, 8.031836662962000162 ) ) ;
#2116 = DIRECTION ( 'NONE',  ( -1.000000000000000000, 0.000000000000000000, 0.000000000000000000 ) ) ;
#2118 = EDGE_CURVE ( 'NONE', #2960, #53336, #53536, .T. ) ;
#2117 = DIRECTION ( 'NONE',  ( -0.7071067811865474617, 0.000000000000000000, 0.7071067811865474617 ) ) ;
#2119 = CARTESIAN_POINT ( 'NONE',  ( 10.18499221075000172, -21.74977139925000102, 7.710118476595999581 ) ) ;
#2120 = CARTESIAN_POINT ( 'NONE',  ( -10.75729140709000120, -78.85675247620899597, -3.177859684493999914 ) ) ;
#2121 = ORIENTED_EDGE ( 'NONE', *, *, #46302, .T. ) ;
#2122 = CARTESIAN_POINT ( 'NONE',  ( -1.929239059888873564, -78.18805851086665371, 11.63526571105258434 ) ) ;
#2123 = ORIENTED_EDGE ( 'NONE', *, *, #50879, .T. ) ;
#2124 = CARTESIAN_POINT ( 'NONE',  ( 9.218103714844254171, -77.35667536906545649, 0.7669798150075999299 ) ) ;
#2125 = CARTESIAN_POINT ( 'NONE',  ( 10.71768947918000059, -78.22818662424299418, -1.656903943290000125 ) ) ;
#2126 = CARTESIAN_POINT ( 'NONE',  ( -6.984124517864168880, -77.27839282645433627, 8.777449155807051540 ) ) ;
#2127 = CARTESIAN_POINT ( 'NONE',  ( 0.2218511837006999776, -78.46518221956569050, 1.400300479361000106 ) ) ;
#2128 = CARTESIAN_POINT ( 'NONE',  ( -0.5999999999999999778, -5.000000000000000000, -0.5999999999999999778 ) ) ;
#2129 = CARTESIAN_POINT ( 'NONE',  ( -6.606377239730371720, -80.92708333333332860, 8.596418555780411808 ) ) ;
#2130 = CARTESIAN_POINT ( 'NONE',  ( 0.08338359222296000406, -79.51780861409000067, -1.538001148114999994 ) ) ;
#2131 = CARTESIAN_POINT ( 'NONE',  ( -7.691916945395000482, -21.75365779208000205, 10.42274798264000069 ) ) ;
#2132 = CARTESIAN_POINT ( 'NONE',  ( -4.306297750730000651, -79.08620252954798957, -10.17515077672999979 ) ) ;
#2133 = CARTESIAN_POINT ( 'NONE',  ( 10.52307592342000042, -79.44025170634557753, 5.828552047478999576 ) ) ;
#2134 = AXIS2_PLACEMENT_3D ( 'NONE', #3276, #56998, #16849 ) ;
#2135 = EDGE_CURVE ( 'NONE', #40540, #25833, #3746, .T. ) ;
#2136 = CARTESIAN_POINT ( 'NONE',  ( -1.473215862480999894, -82.93980678759699288, 3.226639527409000063 ) ) ;
#2137 = VERTEX_POINT ( 'NONE', #21308 ) ;
#2138 = CARTESIAN_POINT ( 'NONE',  ( -10.81093112166862724, -77.19999999999998863, 1.902172181339564450 ) ) ;
#2139 = CARTESIAN_POINT ( 'NONE',  ( 1.653747448240000084, -80.09918819389999101, 0.4061235413877000155 ) ) ;
#2140 = LINE ( 'NONE', #2715, #54946 ) ;
#2141 = CARTESIAN_POINT ( 'NONE',  ( -9.964549960864999889, -77.58706346750800265, 6.650098383618000319 ) ) ;
#2142 = CARTESIAN_POINT ( 'NONE',  ( -9.636775127282000142, -17.55967715742000124, 7.948072248883998547 ) ) ;
#2143 = CIRCLE ( 'NONE', #6843, 13.86363636363999952 ) ;
#2144 = CARTESIAN_POINT ( 'NONE',  ( -1.184494039570261226, -78.72019068799889396, 0.4727986017936515184 ) ) ;
#2145 = CARTESIAN_POINT ( 'NONE',  ( 2.360403478625465734, -2.432488435963918949, -2.699818710255091680 ) ) ;
#2146 = FACE_OUTER_BOUND ( 'NONE', #52697, .T. ) ;
#2147 = CARTESIAN_POINT ( 'NONE',  ( 7.038692338534999315, -77.38697173280098696, 6.250440358128999563 ) ) ;
#2148 = CARTESIAN_POINT ( 'NONE',  ( 2.062312494845999655, -55.57284340075000273, -12.83634740207000036 ) ) ;
#2149 = CARTESIAN_POINT ( 'NONE',  ( 2.807878695492000087, -78.31338377657900196, 10.66853090226000056 ) ) ;
#2150 = DIRECTION ( 'NONE',  ( -0.7071067811865475727, 0.000000000000000000, -0.7071067811865475727 ) ) ;
#2151 = CARTESIAN_POINT ( 'NONE',  ( -0.7807745468539649680, -81.57766601766863346, 1.007917326718190898 ) ) ;
#2152 = ORIENTED_EDGE ( 'NONE', *, *, #25335, .T. ) ;
#2153 = VECTOR ( 'NONE', #16088, 1000.000000000000114 ) ;
#2154 = CARTESIAN_POINT ( 'NONE',  ( -1.200131629027000102, -80.78821469696899271, -0.3495483843597000373 ) ) ;
#2155 = CARTESIAN_POINT ( 'NONE',  ( 0.005523896503684000252, -61.86963456192999899, -12.55021156886000000 ) ) ;
#2156 = CARTESIAN_POINT ( 'NONE',  ( -9.393714757630084122, -80.55838208141010170, 5.413950316515291128 ) ) ;
#2157 = CARTESIAN_POINT ( 'NONE',  ( 9.144378690012999300, -77.46695373569099274, -6.496033325431000094 ) ) ;
#2158 = CARTESIAN_POINT ( 'NONE',  ( -6.405050160242000246, -78.79443481110797620, 8.912875463421000788 ) ) ;
#2159 = CARTESIAN_POINT ( 'NONE',  ( 10.48771805367000098, -58.55560171494000343, -7.686918321054999836 ) ) ;
#2160 = CARTESIAN_POINT ( 'NONE',  ( -4.027474705542414490, -84.67395833761210611, 0.4353081749068463124 ) ) ;
#2161 = EDGE_CURVE ( 'NONE', #4986, #1613, #46217, .T. ) ;
#2162 = CARTESIAN_POINT ( 'NONE',  ( -11.95099068536000075, -76.09110318827499952, -2.203773976563000225 ) ) ;
#2163 = CARTESIAN_POINT ( 'NONE',  ( 6.004401788877678392, -78.53175237169041623, 10.09960146651490298 ) ) ;
#2164 = LINE ( 'NONE', #46757, #39820 ) ;
#2165 = VERTEX_POINT ( 'NONE', #16600 ) ;
#2166 = CARTESIAN_POINT ( 'NONE',  ( -0.9620943986040956242, -80.04521171774420907, 0.7983770923343646020 ) ) ;
#2167 = CARTESIAN_POINT ( 'NONE',  ( 8.130811096204000776, -61.48523690322999613, 9.546858433459998849 ) ) ;
#2168 = CARTESIAN_POINT ( 'NONE',  ( 7.646091287746999754, -55.09149945095000334, -10.13691902390999999 ) ) ;
#2169 = CARTESIAN_POINT ( 'NONE',  ( 11.16390912141999792, -79.41845093841598668, -1.515278025736000123 ) ) ;
#2170 = CARTESIAN_POINT ( 'NONE',  ( -11.57893382125400450, -79.13802082858391884, -3.110875827410843009 ) ) ;
#2171 = DIRECTION ( 'NONE',  ( 1.000000000000000000, 0.000000000000000000, 0.000000000000000000 ) ) ;
#2172 = FACE_OUTER_BOUND ( 'NONE', #45792, .T. ) ;
#2173 = VECTOR ( 'NONE', #15689, 1000.000000000000000 ) ;
#2174 = CARTESIAN_POINT ( 'NONE',  ( 1.052209778380920779, -83.03560755957414585, -1.084595603600321256 ) ) ;
#2175 = CARTESIAN_POINT ( 'NONE',  ( -1.249989095222701962, -79.61143095040115725, -0.1792705600110044706 ) ) ;
#2176 = DIRECTION ( 'NONE',  ( 0.9999999924279685537, 0.000000000000000000, 0.0001230612157848962919 ) ) ;
#2177 = VERTEX_POINT ( 'NONE', #16317 ) ;
#2178 = CARTESIAN_POINT ( 'NONE',  ( -0.7575910999740240737, -81.67355912156841669, -0.9946733871216205669 ) ) ;
#2179 = AXIS2_PLACEMENT_3D ( 'NONE', #21470, #21177, #30603 ) ;
#2180 =( LENGTH_UNIT ( ) NAMED_UNIT ( * ) SI_UNIT ( .MILLI., .METRE. ) );
#2181 = DIRECTION ( 'NONE',  ( 0.000000000000000000, 0.000000000000000000, -1.000000000000000000 ) ) ;
#2182 = ORIENTED_EDGE ( 'NONE', *, *, #27467, .F. ) ;
#2183 = VERTEX_POINT ( 'NONE', #34586 ) ;
#2184 = CARTESIAN_POINT ( 'NONE',  ( -12.49989298246999958, -55.60773379962999741, -1.666426105558999948 ) ) ;
#2185 = VERTEX_POINT ( 'NONE', #2167 ) ;
#2186 = CARTESIAN_POINT ( 'NONE',  ( 7.733411907489287529, -79.95018592149614278, -5.588733307671408745 ) ) ;
#2187 = ORIENTED_EDGE ( 'NONE', *, *, #1402, .T. ) ;
#2188 = CARTESIAN_POINT ( 'NONE',  ( 1.801614160558000055, -18.61347738095000182, 12.59687422887999908 ) ) ;
#2189 = AXIS2_PLACEMENT_3D ( 'NONE', #21585, #8882, #43453 ) ;
#2190 = DIRECTION ( 'NONE',  ( 0.7071067811865974218, -0.7071067811864975017, -1.156399806128994869E-08 ) ) ;
#2191 = DIRECTION ( 'NONE',  ( 1.000000000000000000, 0.000000000000000000, 0.000000000000000000 ) ) ;
#2192 = CARTESIAN_POINT ( 'NONE',  ( -7.850076762416701825, -61.11471440996241711, 9.837736659316185239 ) ) ;
#2194 = EDGE_CURVE ( 'NONE', #37084, #11745, #25450, .T. ) ;
#2193 = CARTESIAN_POINT ( 'NONE',  ( 6.711318802534000483, -78.57268667140098728, 7.292371261484999145 ) ) ;
#2195 = DIRECTION ( 'NONE',  ( 0.7071067811865474617, 0.7071067811865474617, -7.240421654463485624E-10 ) ) ;
#2196 = ORIENTED_EDGE ( 'NONE', *, *, #30060, .T. ) ;
#2198 = ORIENTED_EDGE ( 'NONE', *, *, #38015, .F. ) ;
#2197 = EDGE_CURVE ( 'NONE', #36484, #7601, #29291, .T. ) ;
#2199 = DIRECTION ( 'NONE',  ( 0.000000000000000000, -1.000000000000000000, 0.000000000000000000 ) ) ;
#2200 = CARTESIAN_POINT ( 'NONE',  ( -12.76303204294999993, -23.26485150694999859, 1.980584515756000030 ) ) ;
#2201 = CARTESIAN_POINT ( 'NONE',  ( -12.72558241039000038, -60.00131830475000072, -1.930284820929999867 ) ) ;
#2202 = CARTESIAN_POINT ( 'NONE',  ( -4.475245744599999576, -78.85670619194497988, -8.610626265545000990 ) ) ;
#2203 = CARTESIAN_POINT ( 'NONE',  ( 7.792426477869834223, -61.09102098674993186, 10.18245125510161131 ) ) ;
#2204 = CARTESIAN_POINT ( 'NONE',  ( 1.217465845835393967, -79.77083333333330017, 0.3271848554491025851 ) ) ;
#2205 = CARTESIAN_POINT ( 'NONE',  ( 7.688584395383999848, -79.06206532115000130, 8.762320683322998960 ) ) ;
#2206 = CARTESIAN_POINT ( 'NONE',  ( 0.8102226603197999477, -80.03898078654999892, 1.363061245571999924 ) ) ;
#2207 = PLANE ( 'NONE',  #6327 ) ;
#2208 = EDGE_CURVE ( 'NONE', #30305, #55096, #33018, .T. ) ;
#2209 = CARTESIAN_POINT ( 'NONE',  ( 0.9387899161113768542, -79.20703122369496896, -11.95703176532392398 ) ) ;
#2211 = AXIS2_PLACEMENT_3D ( 'NONE', #47537, #6478, #46952 ) ;
#2210 = CARTESIAN_POINT ( 'NONE',  ( 0.1655257079421880717, -79.61632079734550871, 1.501053824981346763 ) ) ;
#2212 = CARTESIAN_POINT ( 'NONE',  ( 6.797895215277000247, -78.12826332859900447, -7.211733462747999646 ) ) ;
#2213 = CARTESIAN_POINT ( 'NONE',  ( -10.48543666025111776, -77.35833333333330586, 6.043427764450754580 ) ) ;
#2214 = LINE ( 'NONE', #38204, #7077 ) ;
#2216 = CARTESIAN_POINT ( 'NONE',  ( -0.2406813341972999787, -78.87622051897500342, -1.311734976874999958 ) ) ;
#2215 = CARTESIAN_POINT ( 'NONE',  ( 7.000000000000000000, -81.10000000285099020, -1.099999997148999986 ) ) ;
#2217 = CARTESIAN_POINT ( 'NONE',  ( -3.140974612311405512, -78.29583333333334849, 11.68767212001977640 ) ) ;
#2218 = CARTESIAN_POINT ( 'NONE',  ( 10.78580061008000079, -80.22182239623498390, -2.949165541278000013 ) ) ;
#2219 = CARTESIAN_POINT ( 'NONE',  ( -3.593558748265999636, -1.849109825020999853, 0.1459214154804999997 ) ) ;
#2220 = DIRECTION ( 'NONE',  ( 0.000000000000000000, -1.000000000000000000, 0.000000000000000000 ) ) ;
#2221 = CARTESIAN_POINT ( 'NONE',  ( 10.65295200446612967, -80.26231955895572412, 1.664190318615631270 ) ) ;
#2222 = VECTOR ( 'NONE', #57565, 1000.000000000000000 ) ;
#2223 = FACE_OUTER_BOUND ( 'NONE', #45378, .T. ) ;
#2224 = CARTESIAN_POINT ( 'NONE',  ( 0.8397211166896187962, -78.41649201275657788, 0.9258721447709178376 ) ) ;
#2225 = B_SPLINE_CURVE_WITH_KNOTS ( 'NONE', 3,
 ( #47429, #38538, #51559, #11117, #15820, #33807, #20822, #51846, #11402, #29381, #6958, #24963, #42982, #20543, #4569, #21971, #57419, #45015 ),
 .UNSPECIFIED., .F., .F.,
 ( 4, 2, 2, 2, 2, 2, 2, 2, 4 ),
 ( 0.000000000000000000, 0.1249999999999999722, 0.2499999999999999445, 0.3749999999999998890, 0.4999999999999998890, 0.6249999999999998890, 0.7499999999999997780, 0.8749999999999998890, 1.000000000000000000 ),
 .UNSPECIFIED. ) ;
#2226 = CARTESIAN_POINT ( 'NONE',  ( 9.223408614079000145, -79.68658117083499803, -2.412288579557000379 ) ) ;
#2227 = CARTESIAN_POINT ( 'NONE',  ( 11.79660191402999914, -76.73268768631000114, 5.494707494196000575 ) ) ;
#2228 = CARTESIAN_POINT ( 'NONE',  ( 0.000000000000000000, 0.000000000000000000, 0.000000000000000000 ) ) ;
#2229 = CARTESIAN_POINT ( 'NONE',  ( 1.250000000000000000, -76.50000000000000000, -0.5000000000000000000 ) ) ;
#2230 = CARTESIAN_POINT ( 'NONE',  ( -0.8350018197176957147, -79.48137498126830280, 10.71907040161639735 ) ) ;
#2231 = AXIS2_PLACEMENT_3D ( 'NONE', #19491, #14471, #24792 ) ;
#2232 = DIRECTION ( 'NONE',  ( 0.000000000000000000, 1.000000000000000000, 0.000000000000000000 ) ) ;
#2233 = VECTOR ( 'NONE', #46759, 1000.000000000000000 ) ;
#2234 = CARTESIAN_POINT ( 'NONE',  ( -3.999289405514485196, -78.69999999999998863, -0.07539397150088360255 ) ) ;
#2235 = CARTESIAN_POINT ( 'NONE',  ( 10.67692985166999797, -77.60307432715698894, -2.420308236818999870 ) ) ;
#2236 = CARTESIAN_POINT ( 'NONE',  ( 9.706674989537999565, -76.85173030608999056, -5.242346328414999590 ) ) ;
#2237 = CARTESIAN_POINT ( 'NONE',  ( -8.918806285220000518, -78.11739514476064983, 3.872830773119999126 ) ) ;
#2238 = CARTESIAN_POINT ( 'NONE',  ( -2.117690490098999678, -77.91387044253798422, 9.172054377053999730 ) ) ;
#2240 = CARTESIAN_POINT ( 'NONE',  ( 1.997276839918466829, -2.822916666666666075, 2.598917237794090784 ) ) ;
#2239 = CARTESIAN_POINT ( 'NONE',  ( -3.497086053584999910, -84.30604218908899838, 1.371772379829000021 ) ) ;
#2241 = CARTESIAN_POINT ( 'NONE',  ( 0.000000000000000000, -80.99999999999998579, -7.000000000000000000 ) ) ;
#2242 = CARTESIAN_POINT ( 'NONE',  ( -0.1963495408493673156, -80.78541666666670551, 1.499999999999999556 ) ) ;
#2243 = CARTESIAN_POINT ( 'NONE',  ( 7.892561263457914755, -80.29061954989504102, -7.298914836821083441 ) ) ;
#2244 = EDGE_CURVE ( 'NONE', #1173, #5899, #7451, .T. ) ;
#2245 = CARTESIAN_POINT ( 'NONE',  ( 0.000000000000000000, -77.69999999999998863, 0.000000000000000000 ) ) ;
#2246 = CARTESIAN_POINT ( 'NONE',  ( 4.784380313523522332, -77.23333333333332007, 8.300970689365462007 ) ) ;
#2247 = CARTESIAN_POINT ( 'NONE',  ( -11.22206352833000054, -79.59542660325699615, -4.332716936452000844 ) ) ;
#2248 = CYLINDRICAL_SURFACE ( 'NONE', #10550, 0.5999999999999999778 ) ;
#2249 = VERTEX_POINT ( 'NONE', #43471 ) ;
#2250 = CARTESIAN_POINT ( 'NONE',  ( 10.42985624311000059, -77.41380270170699873, 5.801172517007000096 ) ) ;
#2251 = VERTEX_POINT ( 'NONE', #3027 ) ;
#2252 = VERTEX_POINT ( 'NONE', #24877 ) ;
#2253 = CARTESIAN_POINT ( 'NONE',  ( 9.393203674808260573, -78.79166666666665719, 5.413904038987188194 ) ) ;
#2254 = ORIENTED_EDGE ( 'NONE', *, *, #19076, .T. ) ;
#2255 = CONICAL_SURFACE ( 'NONE', #42789, 0.6999999997695000031, 0.7853981633972997312 ) ;
#2256 = CARTESIAN_POINT ( 'NONE',  ( 2.359935201127000060, -81.13242513063499928, 2.648634738920000231 ) ) ;
#2257 = CARTESIAN_POINT ( 'NONE',  ( 6.135231488085603146, -79.21900635011196812, 7.253197741126338194 ) ) ;
#2258 = ORIENTED_EDGE ( 'NONE', *, *, #54684, .F. ) ;
#2259 = CARTESIAN_POINT ( 'NONE',  ( 0.4467594448287516284, -82.75414052523781550, -1.167571400202662035 ) ) ;
#2260 = ORIENTED_EDGE ( 'NONE', *, *, #33418, .F. ) ;
#2261 = CARTESIAN_POINT ( 'NONE',  ( -7.653559502261000347, -55.50150862742999891, 10.01234990226999955 ) ) ;
#2263 = ORIENTED_EDGE ( 'NONE', *, *, #43832, .T. ) ;
#2262 = EDGE_CURVE ( 'NONE', #3901, #1043, #4923, .T. ) ;
#2264 = CARTESIAN_POINT ( 'NONE',  ( 0.6359740846337066378, -79.43277818229616116, 1.079437290100915048 ) ) ;
#2265 = CARTESIAN_POINT ( 'NONE',  ( -1.002309790681787716, -78.81711688494529255, -1.125562765835532497 ) ) ;
#2266 = CARTESIAN_POINT ( 'NONE',  ( -3.627345285118236173, -79.79999999999999716, -11.28297148844626641 ) ) ;
#2267 = CLOSED_SHELL ( 'NONE', ( #13427, #10694, #38626, #40692, #16760, #28341, #8235, #6042, #56094, #3598, #44706, #44437, #56570, #53806, #8409, #18427, #13506, #33732, #6776, #13616, #34124, #45071, #13215, #810, #51759, #14698 ) ) ;
#2268 = AXIS2_PLACEMENT_3D ( 'NONE', #57745, #35003, #12584 ) ;
#2269 = CARTESIAN_POINT ( 'NONE',  ( 0.000000000000000000, -81.99999999999998579, 7.000000000000000000 ) ) ;
#2270 = CARTESIAN_POINT ( 'NONE',  ( -5.531931755322890609, -79.03797283330507639, -10.94557777195214676 ) ) ;
#2271 = CARTESIAN_POINT ( 'NONE',  ( -1.412116703021428998, -86.12609999968209706, -3.092883188393197091 ) ) ;
#2272 = CARTESIAN_POINT ( 'NONE',  ( -10.99972769911000015, -76.38723109256000043, 2.019869862886000345 ) ) ;
#2273 = CARTESIAN_POINT ( 'NONE',  ( 9.145904359845623333, -76.30685081006325277, -5.699187237481845969 ) ) ;
#2274 = CARTESIAN_POINT ( 'NONE',  ( 0.9062719787061290777, -81.17322235724128632, 1.209793186763744366 ) ) ;
#2275 = CARTESIAN_POINT ( 'NONE',  ( -1.950974211964999983, -76.50209444038399909, -10.94135830880000171 ) ) ;
#2276 = EDGE_CURVE ( 'NONE', #22563, #51850, #43604, .T. ) ;
#2277 = CARTESIAN_POINT ( 'NONE',  ( -7.837416255276716370, -78.64473494204541737, -4.912785058267089333 ) ) ;
#2278 = CARTESIAN_POINT ( 'NONE',  ( -7.361960514518000487, -77.56153667140098662, -6.036001273387999966 ) ) ;
#2279 = CARTESIAN_POINT ( 'NONE',  ( -1.308081345731999967, -80.66250310536500479, 0.2599445073669000017 ) ) ;
#2280 = CARTESIAN_POINT ( 'NONE',  ( -3.321932689531000182, -80.44999999999998863, -10.22385755016999909 ) ) ;
#2281 = CARTESIAN_POINT ( 'NONE',  ( -12.50000000000000000, -49.87071424677999687, 0.000000000000000000 ) ) ;
#2282 = CARTESIAN_POINT ( 'NONE',  ( -2.650684130113999615, -81.20728455456799111, 2.661810600175999575 ) ) ;
#2283 = CARTESIAN_POINT ( 'NONE',  ( 2.757516338679999901, -79.71991147651499432, -11.76501219937000009 ) ) ;
#2284 = CARTESIAN_POINT ( 'NONE',  ( -8.197392310145165339, -78.04411871163161152, 6.956661028266359459 ) ) ;
#2285 = CARTESIAN_POINT ( 'NONE',  ( 0.2266372662724759901, -82.96071876721104843, 1.229146615866300696 ) ) ;
#2286 = DIRECTION ( 'NONE',  ( 0.000000000000000000, 0.000000000000000000, -1.000000000000000000 ) ) ;
#2287 = DIRECTION ( 'NONE',  ( 1.000000000000000000, 0.000000000000000000, 0.000000000000000000 ) ) ;
#2288 = CARTESIAN_POINT ( 'NONE',  ( 6.000000000000000000, -81.19999999999998863, 0.000000000000000000 ) ) ;
#2289 = CARTESIAN_POINT ( 'NONE',  ( -0.04193593611713257452, -25.01009741336690695, 12.50649570005664835 ) ) ;
#2290 = CARTESIAN_POINT ( 'NONE',  ( 8.909545442949999838, -57.79999999967000690, -7.919595949288999570 ) ) ;
#2291 = AXIS2_PLACEMENT_3D ( 'NONE', #47733, #33824, #24695 ) ;
#2292 = CARTESIAN_POINT ( 'NONE',  ( 1.500000000000000000, -77.75000000000000000, 0.000000000000000000 ) ) ;
#2293 = DIRECTION ( 'NONE',  ( 0.000000000000000000, 1.000000000000000000, 0.000000000000000000 ) ) ;
#2294 = LINE ( 'NONE', #15566, #45221 ) ;
#2295 = CARTESIAN_POINT ( 'NONE',  ( 10.75486844802039244, -77.71022976309595265, 1.335108088061891074 ) ) ;
#2296 = CARTESIAN_POINT ( 'NONE',  ( -5.915252869412679360, -78.28189657008987012, -10.26004535388594796 ) ) ;
#2297 = CARTESIAN_POINT ( 'NONE',  ( -3.673218652927999539, -79.25215584929806312, 10.34270183799000087 ) ) ;
#2298 = CARTESIAN_POINT ( 'NONE',  ( -6.510718906818000029, -75.83346457246000227, -9.669701809193998798 ) ) ;
#2299 = EDGE_LOOP ( 'NONE', ( #39171, #41298, #39758, #31302, #44069 ) ) ;
#2300 = CARTESIAN_POINT ( 'NONE',  ( 3.648112879021999877, -82.75482450217398878, 1.936488760383000107 ) ) ;
#2301 = CARTESIAN_POINT ( 'NONE',  ( 10.71017182930000011, -80.49865852947209532, -3.921716777206999627 ) ) ;
#2302 = CARTESIAN_POINT ( 'NONE',  ( 8.735034027244228838, -78.32339736695811894, -3.043218161446495706 ) ) ;
#2303 = DIRECTION ( 'NONE',  ( -1.000000000000000000, 0.000000000000000000, 0.000000000000000000 ) ) ;
#2304 = CARTESIAN_POINT ( 'NONE',  ( -10.93308570624999909, -78.41962113229800480, -2.507139558745000052 ) ) ;
#2305 = CARTESIAN_POINT ( 'NONE',  ( 12.72558083408000051, -55.59866855809999464, -1.930284430576000076 ) ) ;
#2306 = CARTESIAN_POINT ( 'NONE',  ( 9.084121021304000010, -77.60854790367199030, 3.512611703280999809 ) ) ;
#2307 = CARTESIAN_POINT ( 'NONE',  ( 3.685137227213000521, -82.58532103627599952, 1.956153376060999927 ) ) ;
#2308 = CARTESIAN_POINT ( 'NONE',  ( 12.56594317989000054, -23.24999999414999863, 1.750000000001000089 ) ) ;
#2309 = CIRCLE ( 'NONE', #46646, 12.50000000000000000 ) ;
#2310 = CYLINDRICAL_SURFACE ( 'NONE', #53783, 1.500000000000000000 ) ;
#2311 = ORIENTED_EDGE ( 'NONE', *, *, #32214, .T. ) ;
#2312 = EDGE_CURVE ( 'NONE', #6792, #52990, #25456, .T. ) ;
#2313 = DIRECTION ( 'NONE',  ( 0.000000000000000000, 0.000000000000000000, 1.000000000000000000 ) ) ;
#2314 = FACE_OUTER_BOUND ( 'NONE', #22185, .T. ) ;
#2315 = EDGE_LOOP ( 'NONE', ( #8172, #22576, #4098, #16468 ) ) ;
#2316 = EDGE_CURVE ( 'NONE', #21151, #28651, #53186, .T. ) ;
#2317 = CARTESIAN_POINT ( 'NONE',  ( -0.9151233253627000241, -78.24293362662599804, -0.9701162038759999495 ) ) ;
#2318 = CARTESIAN_POINT ( 'NONE',  ( 12.64500484464999808, -59.57152778012000027, 1.799490225533999732 ) ) ;
#2319 = FACE_OUTER_BOUND ( 'NONE', #35834, .T. ) ;
#2320 = ORIENTED_EDGE ( 'NONE', *, *, #58012, .F. ) ;
#2321 = CARTESIAN_POINT ( 'NONE',  ( 12.16237383090999913, -78.01045519273699824, 0.2432969017631999853 ) ) ;
#2322 = CARTESIAN_POINT ( 'NONE',  ( -6.206998376855000110, -77.97811096436200273, 9.469182112634999982 ) ) ;
#2323 = VERTEX_POINT ( 'NONE', #36045 ) ;
#2324 = ORIENTED_EDGE ( 'NONE', *, *, #52934, .F. ) ;
#2325 = CARTESIAN_POINT ( 'NONE',  ( -0.02507988100666198525, -80.47717407346517859, 1.249410415426445153 ) ) ;
#2326 = CARTESIAN_POINT ( 'NONE',  ( -1.570796326794938524, -79.68541666666668277, 11.99999999999999645 ) ) ;
#2327 = CARTESIAN_POINT ( 'NONE',  ( -0.6514213267380000172, -80.13032419407451812, 9.745581310452999801 ) ) ;
#2328 = CIRCLE ( 'NONE', #34322, 9.500000000000000000 ) ;
#2329 = ORIENTED_EDGE ( 'NONE', *, *, #876, .T. ) ;
#2330 = CARTESIAN_POINT ( 'NONE',  ( 12.66319948253000049, -53.61851729328000005, 0.1456213732515000137 ) ) ;
#2331 = CARTESIAN_POINT ( 'NONE',  ( 10.30613478042999986, -78.29666782993099616, -3.599856929194000354 ) ) ;
#2332 = ORIENTED_EDGE ( 'NONE', *, *, #19355, .T. ) ;
#2333 = CARTESIAN_POINT ( 'NONE',  ( 9.393794433358884532, -80.80838448933172913, -5.414110195013384974 ) ) ;
#2334 = CARTESIAN_POINT ( 'NONE',  ( 8.385799987677961198, -24.88809827229000504, 9.298537617329934335 ) ) ;
#2335 = CYLINDRICAL_SURFACE ( 'NONE', #12144, 1.750000000000001332 ) ;
#2336 = CARTESIAN_POINT ( 'NONE',  ( 8.610991514544377168, -16.82512235768486875, -9.355860133801421341 ) ) ;
#2337 = FACE_OUTER_BOUND ( 'NONE', #49503, .T. ) ;
#2338 = CARTESIAN_POINT ( 'NONE',  ( -5.506559303151407292, -78.62622913613842002, -8.015689466314336542 ) ) ;
#2339 = VECTOR ( 'NONE', #17547, 1000.000000000000000 ) ;
#2340 = CARTESIAN_POINT ( 'NONE',  ( -12.70255494774433558, -17.25391159035561728, -1.306413223700355397 ) ) ;
#2341 = CARTESIAN_POINT ( 'NONE',  ( -1.478853428237032475, -77.86561205178121270, -0.3007429780463568014 ) ) ;
#2342 = ADVANCED_FACE ( 'NONE', ( #58194 ), #8600, .F. ) ;
#2343 = CARTESIAN_POINT ( 'NONE',  ( -3.873114923184498348, -81.62916667827332162, 1.189743371674534256 ) ) ;
#2344 = CARTESIAN_POINT ( 'NONE',  ( 9.569482281372000188, -76.64386216769000271, -7.743360016082000641 ) ) ;
#2345 = EDGE_CURVE ( 'NONE', #55096, #24152, #22472, .T. ) ;
#2346 = CARTESIAN_POINT ( 'NONE',  ( -9.252740428349001789, -77.92083333333333428, -2.486604901413163926 ) ) ;
#2347 = CARTESIAN_POINT ( 'NONE',  ( 8.878335097443999402, -61.86963071710999884, -8.870344075662000449 ) ) ;
#2348 = CARTESIAN_POINT ( 'NONE',  ( 7.914613980750001332, -79.26568659574000719, 9.019916049260999102 ) ) ;
#2349 = CARTESIAN_POINT ( 'NONE',  ( 7.144724566336000393, -76.39169569806699656, 9.988770583665001368 ) ) ;
#2350 = CARTESIAN_POINT ( 'NONE',  ( -10.12290050126000196, -60.04999999958999979, -7.648026767103999646 ) ) ;
#2351 = CARTESIAN_POINT ( 'NONE',  ( 6.038193122641423827, -78.21661092667235948, -10.45819121534531959 ) ) ;
#2352 = CARTESIAN_POINT ( 'NONE',  ( 11.68767212001979594, -78.02916666666668277, -3.140974612311341563 ) ) ;
#2353 = ORIENTED_EDGE ( 'NONE', *, *, #23929, .T. ) ;
#2354 = CARTESIAN_POINT ( 'NONE',  ( 1.329440977735876661, -79.96045754634249647, -0.7203538468090995295 ) ) ;
#2355 = FACE_OUTER_BOUND ( 'NONE', #50391, .T. ) ;
#2356 = CARTESIAN_POINT ( 'NONE',  ( 1.798336774608999988, -23.19644498052000259, 12.61277771566000006 ) ) ;
#2357 = CARTESIAN_POINT ( 'NONE',  ( 1.704789469149671666, -23.70346161525050732, 12.53199752960681046 ) ) ;
#2358 = CARTESIAN_POINT ( 'NONE',  ( -3.234369484799000549, -2.340565377978999884, 1.825734147243999850 ) ) ;
#2359 = CARTESIAN_POINT ( 'NONE',  ( -9.022824479474000015, -77.88263333629100771, 8.159115699504999597 ) ) ;
#2360 = CARTESIAN_POINT ( 'NONE',  ( -6.496683922195000349, -78.20392319598897757, 7.256224481198000120 ) ) ;
#2361 = EDGE_CURVE ( 'NONE', #17717, #11974, #17560, .T. ) ;
#2363 = CARTESIAN_POINT ( 'NONE',  ( 4.741624722535068948, -77.03333333334457222, 8.228481285277691626 ) ) ;
#2362 = CARTESIAN_POINT ( 'NONE',  ( -7.782531694773533459, -76.13256886044052862, 8.804557435548110433 ) ) ;
#2364 = CARTESIAN_POINT ( 'NONE',  ( -0.2230286467304000153, -78.64998243216399487, -10.77282081049999896 ) ) ;
#2365 = CARTESIAN_POINT ( 'NONE',  ( -10.07999562765293255, -79.57180944839785752, 3.736692566665637205 ) ) ;
#2366 = ORIENTED_EDGE ( 'NONE', *, *, #17037, .F. ) ;
#2367 = CARTESIAN_POINT ( 'NONE',  ( 10.35453599130000057, -76.75783510652000530, -6.064947188958000446 ) ) ;
#2368 = CIRCLE ( 'NONE', #31531, 4.000000000000000000 ) ;
#2369 = CARTESIAN_POINT ( 'NONE',  ( 9.169855720791529663, -79.02165581492216972, 2.557895400793727347 ) ) ;
#2370 = CARTESIAN_POINT ( 'NONE',  ( 2.598917237794081014, -2.302083333333333481, 1.997276839918480373 ) ) ;
#2371 = CARTESIAN_POINT ( 'NONE',  ( -7.633501923173000137, -60.00104675737999571, 10.36289748054999826 ) ) ;
#2372 = VECTOR ( 'NONE', #47862, 1000.000000000000114 ) ;
#2373 = CARTESIAN_POINT ( 'NONE',  ( -10.47195525230314139, -80.07542197283444807, 3.366853175460504666 ) ) ;
#2374 = CARTESIAN_POINT ( 'NONE',  ( 8.860884805193000702, -78.80704449888298768, -2.531140219154000004 ) ) ;
#2375 = CARTESIAN_POINT ( 'NONE',  ( -1.259732728554407988, -79.32676086870174004, -0.4364646385938031337 ) ) ;
#2376 = CARTESIAN_POINT ( 'NONE',  ( -9.250000000000001776, -79.01041666666667140, -1.210822168571065616 ) ) ;
#2377 = VERTEX_POINT ( 'NONE', #4176 ) ;
#2378 = CARTESIAN_POINT ( 'NONE',  ( 8.680500415593000341, -78.58155805217599266, 7.175156920760000112 ) ) ;
#2379 = CARTESIAN_POINT ( 'NONE',  ( 12.99999999999509726, -6.000000000000000000, 2.526608922437675593E-09 ) ) ;
#2380 = DIRECTION ( 'NONE',  ( 0.9999999999999992228, 4.158397913305990963E-08, 7.906211578309984016E-12 ) ) ;
#2381 = CARTESIAN_POINT ( 'NONE',  ( -3.436577016645513627, -78.54828564506388489, -0.06478580652260451656 ) ) ;
#2382 = ADVANCED_FACE ( 'NONE', ( #17167 ), #55596, .F. ) ;
#2384 = CARTESIAN_POINT ( 'NONE',  ( 1.146081193082048033, -81.38292660934976652, 0.4986479518160068514 ) ) ;
#2383 = CONICAL_SURFACE ( 'NONE', #8984, 0.5999999993581000002, 0.7853981633972997312 ) ;
#2385 = CARTESIAN_POINT ( 'NONE',  ( 0.3718183191318770731, -79.00162595749708316, 1.218859363413805852 ) ) ;
#2386 = LINE ( 'NONE', #21813, #29769 ) ;
#2387 = CARTESIAN_POINT ( 'NONE',  ( 3.911994926767235370, -82.33721874605919311, -0.8315198071374734212 ) ) ;
#2388 = CARTESIAN_POINT ( 'NONE',  ( -1.980584515756000030, -18.73514849905999924, 12.76303204340999997 ) ) ;
#2389 = CARTESIAN_POINT ( 'NONE',  ( 6.605943070247981552, -78.42293208188651477, 8.595924706473319077 ) ) ;
#2390 = CARTESIAN_POINT ( 'NONE',  ( -7.919595949288999570, -59.94999999967000548, -9.050966799188000067 ) ) ;
#2391 = ORIENTED_EDGE ( 'NONE', *, *, #24170, .T. ) ;
#2392 = ORIENTED_EDGE ( 'NONE', *, *, #3092, .T. ) ;
#2393 = CARTESIAN_POINT ( 'NONE',  ( -12.36265669798000033, -76.74838446013099258, 1.637438600144999867 ) ) ;
#2394 = CARTESIAN_POINT ( 'NONE',  ( 0.5871605803710688853, -78.72939686299562823, -10.73511180301259671 ) ) ;
#2395 = EDGE_LOOP ( 'NONE', ( #43208, #30951, #22703, #57067 ) ) ;
#2396 = CARTESIAN_POINT ( 'NONE',  ( 9.966229686710001090, -18.33098097385000003, 7.657726530248999630 ) ) ;
#2397 = CARTESIAN_POINT ( 'NONE',  ( -0.5135400117351243132, -53.62131466101166666, 12.70453250094476516 ) ) ;
#2398 = CARTESIAN_POINT ( 'NONE',  ( -9.073214995490001655, -78.31691570303000560, -8.802385182600000135 ) ) ;
#2399 = CARTESIAN_POINT ( 'NONE',  ( -3.463687794021950150, -79.69898096214407701, -10.20052495849528995 ) ) ;
#2400 = CARTESIAN_POINT ( 'NONE',  ( 9.369164850722000892, -60.04999999966999980, 7.601397897754999633 ) ) ;
#2401 = CARTESIAN_POINT ( 'NONE',  ( 6.060638544127889382, -77.21786737044560311, -10.11814076704347443 ) ) ;
#2402 = CARTESIAN_POINT ( 'NONE',  ( 9.453938376997999882, -79.12911590622699975, 6.036651369377000087 ) ) ;
#2403 = AXIS2_PLACEMENT_3D ( 'NONE', #38804, #8601, #34361 ) ;
#2404 = ORIENTED_EDGE ( 'NONE', *, *, #30223, .T. ) ;
#2405 = LINE ( 'NONE', #47002, #2998 ) ;
#2406 = ORIENTED_EDGE ( 'NONE', *, *, #22775, .F. ) ;
#2407 = CARTESIAN_POINT ( 'NONE',  ( 3.850229173358457491, -77.25920432106504165, -8.419659690126449547 ) ) ;
#2408 = CARTESIAN_POINT ( 'NONE',  ( 0.7999999997951000585, -23.14999999072999870, 11.99999999979999821 ) ) ;
#2409 = CARTESIAN_POINT ( 'NONE',  ( 1.500000000000000000, -79.25000000000000000, 0.000000000000000000 ) ) ;
#2410 = CARTESIAN_POINT ( 'NONE',  ( 10.34084413924634305, -78.06824677350734021, -4.346096116244792640 ) ) ;
#2411 = UNCERTAINTY_MEASURE_WITH_UNIT (LENGTH_MEASURE( 1.000000000000000082E-05 ), #44948, 'distance_accuracy_value', 'NONE');
#2412 = CARTESIAN_POINT ( 'NONE',  ( 1.326698500471999997, -78.75709889550499554, -0.7340390780227000755 ) ) ;
#2413 = CARTESIAN_POINT ( 'NONE',  ( 0.000000000000000000, -51.86282895648000135, 0.000000000000000000 ) ) ;
#2414 = DIRECTION ( 'NONE',  ( 0.000000000000000000, -1.000000000000000000, 0.000000000000000000 ) ) ;
#2415 = CARTESIAN_POINT ( 'NONE',  ( 0.1742577344548000007, -77.75455890439999962, 1.489843697164999980 ) ) ;
#2416 = CARTESIAN_POINT ( 'NONE',  ( -7.627487606609999915, -23.29778595484999926, 10.35845616727999996 ) ) ;
#2417 = CARTESIAN_POINT ( 'NONE',  ( 9.088959790636000236, -78.19661130901299373, -6.010253266999000310 ) ) ;
#2418 = DIRECTION ( 'NONE',  ( 0.000000000000000000, -1.000000000000000000, 0.000000000000000000 ) ) ;
#2419 = SURFACE_STYLE_USAGE ( .BOTH. , #47885 ) ;
#2420 = CARTESIAN_POINT ( 'NONE',  ( -1.557310112275000158, -85.94606716926699619, 3.186928280003000324 ) ) ;
#2421 = ORIENTED_EDGE ( 'NONE', *, *, #5439, .F. ) ;
#2422 = CARTESIAN_POINT ( 'NONE',  ( -1.586699731716999962, -82.80045924015399805, 0.6182239771991999699 ) ) ;
#2423 = CARTESIAN_POINT ( 'NONE',  ( -1.639384890095999969, -80.35182505433999722, -0.4606887641594999971 ) ) ;
#2424 = CARTESIAN_POINT ( 'NONE',  ( -5.413876276891260275, -79.18349062226657509, -9.393307288579276104 ) ) ;
#2425 = CARTESIAN_POINT ( 'NONE',  ( 0.9627474882855999727, -78.12971924654898714, -11.94107121277999894 ) ) ;
#2426 = CARTESIAN_POINT ( 'NONE',  ( -7.606021555073000151, -18.57841460072999951, 10.52692944505000128 ) ) ;
#2427 = CARTESIAN_POINT ( 'NONE',  ( 9.329450859912574501, -78.89181274521322962, 5.387597712135250738 ) ) ;
#2428 = CARTESIAN_POINT ( 'NONE',  ( 0.006631491796348466111, -2.124900358190759064, 3.523059322413071737 ) ) ;
#2429 = CARTESIAN_POINT ( 'NONE',  ( 9.526733066210548273, -80.88851237995341137, 4.980266374315006850 ) ) ;
#2430 = CARTESIAN_POINT ( 'NONE',  ( -1.160011803644999784, -78.75834361351799373, -9.451177169703999681 ) ) ;
#2432 = EDGE_CURVE ( 'NONE', #9068, #28511, #35808, .T. ) ;
#2431 = CARTESIAN_POINT ( 'NONE',  ( -0.8302729325563608098, -81.16825566421603355, -0.9509483969845207163 ) ) ;
#2433 = CARTESIAN_POINT ( 'NONE',  ( -10.41264997627000000, -77.93207497455300370, 3.643961423121000021 ) ) ;
#2434 = CARTESIAN_POINT ( 'NONE',  ( 10.75000000000000000, -79.25000000000000000, 0.000000000000000000 ) ) ;
#2435 = CARTESIAN_POINT ( 'NONE',  ( 0.5212087151649998917, -80.89778770350477544, 10.89825343941999947 ) ) ;
#2436 = CARTESIAN_POINT ( 'NONE',  ( -0.8273849986450537708, -80.71898599761188109, -0.9695052011924152335 ) ) ;
#2437 = ORIENTED_EDGE ( 'NONE', *, *, #52656, .F. ) ;
#2438 = LINE ( 'NONE', #38724, #47230 ) ;
#2439 = CARTESIAN_POINT ( 'NONE',  ( -0.9820397338569999413, -80.70308451575900222, -0.7733679338621000099 ) ) ;
#2440 = CARTESIAN_POINT ( 'NONE',  ( 1.930009203933999995, -60.00099032284000344, -12.72537718780000127 ) ) ;
#2441 = CARTESIAN_POINT ( 'NONE',  ( -8.137215171344880815, -55.34844303569388302, 7.401770473313843191 ) ) ;
#2442 = CARTESIAN_POINT ( 'NONE',  ( 9.869466656387999137, -76.97669956165799476, -5.330266269891000164 ) ) ;
#2443 = CARTESIAN_POINT ( 'NONE',  ( -2.169167664939000151, -78.32098300445798600, 10.75912301088999889 ) ) ;
#2444 = DIRECTION ( 'NONE',  ( 1.000000000000000000, 0.000000000000000000, 0.000000000000000000 ) ) ;
#2445 = CARTESIAN_POINT ( 'NONE',  ( -2.729547995496241164, -86.00364585192558309, 2.940596197643096321 ) ) ;
#2446 = FACE_OUTER_BOUND ( 'NONE', #20407, .T. ) ;
#2447 = CARTESIAN_POINT ( 'NONE',  ( 10.52222799053675040, -78.48640825465236048, 5.259909153984513530 ) ) ;
#2448 = CARTESIAN_POINT ( 'NONE',  ( 4.044903269867999640, -79.05999999999998806, -8.595856998426999240 ) ) ;
#2449 = ORIENTED_EDGE ( 'NONE', *, *, #8622, .F. ) ;
#2450 = CARTESIAN_POINT ( 'NONE',  ( -1.250000000000000000, -77.64999999999999147, 0.000000000000000000 ) ) ;
#2451 = CARTESIAN_POINT ( 'NONE',  ( 9.009247259181913492, -78.22916666666667140, -2.421167930323368633 ) ) ;
#2452 = EDGE_CURVE ( 'NONE', #31055, #49519, #17758, .T. ) ;
#2453 = AXIS2_PLACEMENT_3D ( 'NONE', #33184, #1638, #41479 ) ;
#2454 = CARTESIAN_POINT ( 'NONE',  ( -10.13316084080999957, -79.64318977307699754, 4.924182635666999985 ) ) ;
#2455 = FACE_OUTER_BOUND ( 'NONE', #28665, .T. ) ;
#2456 = CARTESIAN_POINT ( 'NONE',  ( -5.917523019358107206, -77.71666666666666856, 10.26699006316250795 ) ) ;
#2457 = DIRECTION ( 'NONE',  ( 0.000000000000000000, 0.000000000000000000, -1.000000000000000000 ) ) ;
#2458 = CARTESIAN_POINT ( 'NONE',  ( -0.1835247799291997717, -82.96475420480349783, -1.500792295550013478 ) ) ;
#2459 = CARTESIAN_POINT ( 'NONE',  ( 0.000000000000000000, -87.20000000000000284, 0.000000000000000000 ) ) ;
#2460 = CIRCLE ( 'NONE', #38381, 1.750000000000001332 ) ;
#2461 = CARTESIAN_POINT ( 'NONE',  ( -10.42531124903999995, -55.53514851492000304, 7.624341765436000173 ) ) ;
#2462 = EDGE_CURVE ( 'NONE', #36137, #45005, #30194, .T. ) ;
#2463 = ORIENTED_EDGE ( 'NONE', *, *, #10305, .T. ) ;
#2464 = CARTESIAN_POINT ( 'NONE',  ( 8.061017305527000687, -55.64999999967000122, 8.909545442950999927 ) ) ;
#2465 = EDGE_CURVE ( 'NONE', #25083, #50457, #31895, .T. ) ;
#2466 = DIRECTION ( 'NONE',  ( 0.7071067811865475727, 0.000000000000000000, -0.7071067811865475727 ) ) ;
#2467 = ORIENTED_EDGE ( 'NONE', *, *, #16504, .T. ) ;
#2468 = ORIENTED_EDGE ( 'NONE', *, *, #26760, .T. ) ;
#2469 = CARTESIAN_POINT ( 'NONE',  ( -12.83836748059999877, -55.59372227128000077, -2.062147040909000140 ) ) ;
#2470 = EDGE_LOOP ( 'NONE', ( #31332, #13621, #31069, #19559 ) ) ;
#2471 = VERTEX_POINT ( 'NONE', #23922 ) ;
#2472 = CARTESIAN_POINT ( 'NONE',  ( -8.973625165401864834, -81.00000000000001421, -6.089121955489211757 ) ) ;
#2473 = CARTESIAN_POINT ( 'NONE',  ( -5.597547907814000467, -77.65556621773498591, -9.372450235129999641 ) ) ;
#2474 = CARTESIAN_POINT ( 'NONE',  ( 0.3926218265389220807, -78.14583333333335702, -1.460959015002473382 ) ) ;
#2475 = CARTESIAN_POINT ( 'NONE',  ( 1.936520525790000002, -78.61623667140099769, 9.719586767747999900 ) ) ;
#2476 = CARTESIAN_POINT ( 'NONE',  ( -9.250000000000000000, -79.49999999999998579, 1.813240672189999963E-14 ) ) ;
#2477 = ORIENTED_EDGE ( 'NONE', *, *, #1582, .F. ) ;
#2478 = ORIENTED_EDGE ( 'NONE', *, *, #43659, .F. ) ;
#2479 = CARTESIAN_POINT ( 'NONE',  ( -7.487847511170848236, -77.55006124278669688, 5.430885747604098590 ) ) ;
#2480 = LINE ( 'NONE', #38190, #24417 ) ;
#2481 = EDGE_CURVE ( 'NONE', #44663, #23438, #1379, .T. ) ;
#2482 = CARTESIAN_POINT ( 'NONE',  ( -12.57434559700999976, -60.51110719467000365, -1.760800161976000089 ) ) ;
#2483 = CARTESIAN_POINT ( 'NONE',  ( 6.983565664416999219, -78.51907550980999417, -6.737990796766999857 ) ) ;
#2484 = CARTESIAN_POINT ( 'NONE',  ( 4.614362421889810051, -86.12610001270964233, 0.5296543453898773235 ) ) ;
#2485 = CARTESIAN_POINT ( 'NONE',  ( -9.450266643504305009, -79.40799665456589196, -0.9830318362740778637 ) ) ;
#2486 = CARTESIAN_POINT ( 'NONE',  ( 1.407171709420440342, -76.63541666666665719, -10.74999999999999822 ) ) ;
#2487 = CARTESIAN_POINT ( 'NONE',  ( -12.00000000000000888, -76.88958333333333428, 1.570796326794847264 ) ) ;
#2488 = CARTESIAN_POINT ( 'NONE',  ( -0.9334586162929999764, -81.34442870581999330, -1.282259494539000011 ) ) ;
#2489 = CARTESIAN_POINT ( 'NONE',  ( -1.092232985442822102, -81.04166666666664298, -0.6295237254636245616 ) ) ;
#2490 = CARTESIAN_POINT ( 'NONE',  ( -10.07615509324000058, -54.07367739666999285, 7.986954869161998261 ) ) ;
#2491 = CARTESIAN_POINT ( 'NONE',  ( 8.546298008199000762, -78.65086332859900153, -5.018094164374000243 ) ) ;
#2492 = CARTESIAN_POINT ( 'NONE',  ( -1.570796326794937636, -77.28541666666664867, 11.99999999999999467 ) ) ;
#2493 = CARTESIAN_POINT ( 'NONE',  ( 2.062670899148999926, -18.69360374348000065, -12.83044039274999903 ) ) ;
#2494 = CIRCLE ( 'NONE', #39213, 9.000000000000000000 ) ;
#2496 = CARTESIAN_POINT ( 'NONE',  ( -0.5996107393304999089, -78.67777002545099663, 1.191235959310000148 ) ) ;
#2495 = CARTESIAN_POINT ( 'NONE',  ( -7.954951288349001004, -60.04999999966999980, -9.722718241315000398 ) ) ;
#2497 = CARTESIAN_POINT ( 'NONE',  ( 3.562066907208550237, -79.44390867633869391, 8.599352349090708003 ) ) ;
#2498 =( NAMED_UNIT ( * ) SI_UNIT ( $, .STERADIAN. ) SOLID_ANGLE_UNIT ( ) );
#2499 = FACE_OUTER_BOUND ( 'NONE', #12871, .T. ) ;
#2500 = CARTESIAN_POINT ( 'NONE',  ( 3.702420020526000055, -2.620613097741000264, 0.8821385418971999792 ) ) ;
#2501 = AXIS2_PLACEMENT_3D ( 'NONE', #15199, #10199, #28179 ) ;
#2502 = CARTESIAN_POINT ( 'NONE',  ( -1.720719981710890023, -0.8344193358160810758, -3.082755224493606949 ) ) ;
#2503 = AXIS2_PLACEMENT_3D ( 'NONE', #8887, #27462, #35737 ) ;
#2504 = EDGE_LOOP ( 'NONE', ( #26220, #44640, #7939, #2537, #53948 ) ) ;
#2505 = CARTESIAN_POINT ( 'NONE',  ( -3.250000000000000000, -3.500000000000000000, -1.188926645705999921E-13 ) ) ;
#2506 = DIRECTION ( 'NONE',  ( 0.000000000000000000, 1.000000000000000000, 0.000000000000000000 ) ) ;
#2507 = CARTESIAN_POINT ( 'NONE',  ( -2.065550207748000133, -55.37434920636000157, 12.82162303852000029 ) ) ;
#2508 = CARTESIAN_POINT ( 'NONE',  ( -8.479436900434727420, -77.15903440364206745, -3.916278883261680388 ) ) ;
#2509 = CARTESIAN_POINT ( 'NONE',  ( 7.742394642564000229, -79.65735851257699096, -5.562888445052999842 ) ) ;
#2510 = CARTESIAN_POINT ( 'NONE',  ( -9.329492144256546382, -77.05848916406876015, 5.387603188400559517 ) ) ;
#2511 = DIRECTION ( 'NONE',  ( 0.000000000000000000, 0.000000000000000000, -1.000000000000000000 ) ) ;
#2512 = CARTESIAN_POINT ( 'NONE',  ( 1.930628539543000066, -60.02124444054000207, 12.72375828107000117 ) ) ;
#2513 = FACE_OUTER_BOUND ( 'NONE', #36211, .T. ) ;
#2514 = CARTESIAN_POINT ( 'NONE',  ( -1.439896632895311113, -77.31458333333333144, -11.00000000000000355 ) ) ;
#2515 = EDGE_CURVE ( 'NONE', #44715, #45083, #42414, .T. ) ;
#2516 = CARTESIAN_POINT ( 'NONE',  ( 1.250000000000000000, -67.52659999995799467, 0.000000000000000000 ) ) ;
#2517 = CARTESIAN_POINT ( 'NONE',  ( -9.137594394056998581, -77.91723112247599659, -6.029850034859999930 ) ) ;
#2518 = EDGE_CURVE ( 'NONE', #9803, #34745, #14001, .T. ) ;
#2519 = CARTESIAN_POINT ( 'NONE',  ( -0.1560029832145526929, -76.32376738114049886, -11.74899260739961804 ) ) ;
#2520 = CARTESIAN_POINT ( 'NONE',  ( -2.172168385828000314, -77.81825668956298614, -10.93326506925000174 ) ) ;
#2521 = CARTESIAN_POINT ( 'NONE',  ( 8.384816012895999648, -78.85774514476065633, -4.923277454554000343 ) ) ;
#2522 = LINE ( 'NONE', #6942, #57537 ) ;
#2523 = CARTESIAN_POINT ( 'NONE',  ( -0.8405563561534999950, -76.88792425275799758, -9.635375415708001157 ) ) ;
#2524 = CARTESIAN_POINT ( 'NONE',  ( -1.310679582531389498, -78.95833333333335702, 0.7554284705563444335 ) ) ;
#2525 = CARTESIAN_POINT ( 'NONE',  ( 3.250000000000000000, -2.750000000000000000, 0.000000000000000000 ) ) ;
#2526 = CARTESIAN_POINT ( 'NONE',  ( 9.446529892197220946, -80.31034450011661363, -5.155174753762183926 ) ) ;
#2527 = DIRECTION ( 'NONE',  ( 1.000000000000000000, 0.000000000000000000, 0.000000000000000000 ) ) ;
#2528 = FACE_BOUND ( 'NONE', #24499, .T. ) ;
#2529 = CARTESIAN_POINT ( 'NONE',  ( -3.970056213021999625, -78.96787035545898448, 11.35542513096999961 ) ) ;
#2530 = CARTESIAN_POINT ( 'NONE',  ( -0.3271848554491046945, -81.89583333333330017, 1.217465845835393301 ) ) ;
#2531 = ADVANCED_FACE ( 'NONE', ( #7655 ), #43683, .T. ) ;
#2532 = CARTESIAN_POINT ( 'NONE',  ( 5.940599228801999379E-14, -5.950000000028880187, 0.000000000000000000 ) ) ;
#2533 = ORIENTED_EDGE ( 'NONE', *, *, #10356, .T. ) ;
#2534 = CARTESIAN_POINT ( 'NONE',  ( 1.779623408257821504, -24.13630869023482717, 12.71471627657148318 ) ) ;
#2535 = VERTEX_POINT ( 'NONE', #33649 ) ;
#2536 = AXIS2_PLACEMENT_3D ( 'NONE', #50585, #23701, #41714 ) ;
#2537 = ORIENTED_EDGE ( 'NONE', *, *, #24871, .T. ) ;
#2538 = CARTESIAN_POINT ( 'NONE',  ( -3.165411199172029288, -1.479166666666666075, 0.8506806241676482250 ) ) ;
#2539 = ORIENTED_EDGE ( 'NONE', *, *, #55559, .F. ) ;
#2540 = VECTOR ( 'NONE', #37179, 1000.000000000000114 ) ;
#2541 = CARTESIAN_POINT ( 'NONE',  ( -3.402914194239000434, -81.68874464050298911, 0.9925453996215999330 ) ) ;
#2542 = CARTESIAN_POINT ( 'NONE',  ( 4.369668091130538556, -79.23660998577489067, 8.435227713305813779 ) ) ;
#2543 = VERTEX_POINT ( 'NONE', #6502 ) ;
#2544 = CARTESIAN_POINT ( 'NONE',  ( 0.7945685312060931649, -82.78032265392057809, -0.9647621081858361869 ) ) ;
#2545 = ORIENTED_EDGE ( 'NONE', *, *, #17350, .T. ) ;
#2546 = CARTESIAN_POINT ( 'NONE',  ( -3.380225385341000255, -3.046741667230000061, 0.3787538185775999877 ) ) ;
#2547 = ORIENTED_EDGE ( 'NONE', *, *, #21590, .T. ) ;
#2548 = CARTESIAN_POINT ( 'NONE',  ( 0.8360307752442982521, -79.41690561761365075, 0.9295092197899607056 ) ) ;
#2549 = CARTESIAN_POINT ( 'NONE',  ( -0.9591330678447479441, -78.32136967069745026, -1.194087134926961946 ) ) ;
#2550 = CONICAL_SURFACE ( 'NONE', #34593, 9.099999999966000175, 0.7853981633972997312 ) ;
#2551 = CARTESIAN_POINT ( 'NONE',  ( -11.00477662459603501, -79.80000000000001137, -4.649775713267806587 ) ) ;
#2552 = EDGE_CURVE ( 'NONE', #2471, #47498, #21656, .T. ) ;
#2553 = CARTESIAN_POINT ( 'NONE',  ( -10.13847005927290468, -80.07308699731846957, 3.575929410332394642 ) ) ;
#2554 = CARTESIAN_POINT ( 'NONE',  ( -4.000000000000000000, -75.00000000000001421, 0.5999999999999999778 ) ) ;
#2555 = CARTESIAN_POINT ( 'NONE',  ( -4.101471859984844315, -86.36264282632896538, -0.3926127889848393115 ) ) ;
#2556 = CARTESIAN_POINT ( 'NONE',  ( 11.06808393496999976, -76.66313245443998881, 1.603559079323000125 ) ) ;
#2557 = CARTESIAN_POINT ( 'NONE',  ( -5.173679449032695388, -79.93013575167898921, -8.224241350002412076 ) ) ;
#2558 = CARTESIAN_POINT ( 'NONE',  ( -1.480668258985768482, -81.36553860590423426, -0.3070248522480592546 ) ) ;
#2559 = CARTESIAN_POINT ( 'NONE',  ( -7.811514047910000258, -76.82815968624299785, 7.905692513472000194 ) ) ;
#2560 = CARTESIAN_POINT ( 'NONE',  ( -7.779924306592839400, -78.64565599839535537, -5.003626092249043644 ) ) ;
#2561 = CARTESIAN_POINT ( 'NONE',  ( -1.185397549814999785, -80.21598949493500186, -0.6110718436566999756 ) ) ;
#2562 = DIRECTION ( 'NONE',  ( -0.7071067811865475727, 0.000000000000000000, 0.7071067811865475727 ) ) ;
#2563 = CARTESIAN_POINT ( 'NONE',  ( -5.838193839761721016, -77.22708333333332575, 7.596835002782687418 ) ) ;
#2564 = CARTESIAN_POINT ( 'NONE',  ( 2.817646679242999941, -80.60217549782598212, -2.223646712691999650 ) ) ;
#2566 = EDGE_CURVE ( 'NONE', #11618, #52988, #6796, .T. ) ;
#2565 = CARTESIAN_POINT ( 'NONE',  ( 9.045277090019000710, -79.20032221108399995, -8.187312926306001160 ) ) ;
#2567 = CARTESIAN_POINT ( 'NONE',  ( -10.56344111567097954, -78.08522265697479270, 1.994203520344934644 ) ) ;
#2568 = CARTESIAN_POINT ( 'NONE',  ( -11.00000000000000000, -74.64999999999999147, 0.000000000000000000 ) ) ;
#2569 = CARTESIAN_POINT ( 'NONE',  ( 2.949810794156999982, -82.38249735065198820, -1.686638855401999981 ) ) ;
#2570 = CARTESIAN_POINT ( 'NONE',  ( -10.86515771069091407, -76.23152734406622244, -4.589020684590622068 ) ) ;
#2571 = CARTESIAN_POINT ( 'NONE',  ( 10.53101998747000145, -23.30639625649999758, 7.613962827179999948 ) ) ;
#2572 = CARTESIAN_POINT ( 'NONE',  ( -9.414507962650999318, -62.06263135892999827, -8.652357372810001834 ) ) ;
#2573 = DIRECTION ( 'NONE',  ( -0.7071067811865475727, 0.000000000000000000, 0.7071067811865475727 ) ) ;
#2574 = CARTESIAN_POINT ( 'NONE',  ( 0.1963495408493638184, -77.63541666666668561, -1.499999999999999778 ) ) ;
#2575 = B_SPLINE_CURVE_WITH_KNOTS ( 'NONE', 3,
 ( #11940, #20789, #52668, #39377, #12504, #34924, #47969, #2221, #7213, #25504 ),
 .UNSPECIFIED., .F., .F.,
 ( 4, 2, 2, 2, 4 ),
 ( 0.000000000000000000, 0.2500000000000000000, 0.5000000000000000000, 0.7500000000000000000, 1.000000000000000000 ),
 .UNSPECIFIED. ) ;
#2576 = CARTESIAN_POINT ( 'NONE',  ( -1.500000000000000000, -78.00000000000000000, 0.000000000000000000 ) ) ;
#2577 = CARTESIAN_POINT ( 'NONE',  ( -9.692839446179998930, -78.50182691516999967, 7.074522137259999788 ) ) ;
#2578 = VECTOR ( 'NONE', #112, 1000.000000000000000 ) ;
#2579 = CARTESIAN_POINT ( 'NONE',  ( -0.3888001762888235735, -77.57257727438346251, -10.76536887735824877 ) ) ;
#2580 = CARTESIAN_POINT ( 'NONE',  ( 1.179538764136264906, -78.23344348886517707, -11.01565543437853734 ) ) ;
#2581 = CARTESIAN_POINT ( 'NONE',  ( 0.2678032735093955896, -25.21432775290392314, -12.70526550768988372 ) ) ;
#2582 = CARTESIAN_POINT ( 'NONE',  ( -5.751871349228999897, -76.75451366967000411, -10.77263286324999925 ) ) ;
#2583 = ORIENTED_EDGE ( 'NONE', *, *, #23290, .T. ) ;
#2584 = CONICAL_SURFACE ( 'NONE', #12912, 9.649999999909001147, 0.7853981633972997312 ) ;
#2585 = ADVANCED_FACE ( 'NONE', ( #20377 ), #10662, .F. ) ;
#2586 = DIRECTION ( 'NONE',  ( 0.000000000000000000, 1.000000000000000000, 0.000000000000000000 ) ) ;
#2587 = CARTESIAN_POINT ( 'NONE',  ( 3.308356911591999960, -85.80681307385599155, -1.472975398278999926 ) ) ;
#2588 = AXIS2_PLACEMENT_3D ( 'NONE', #52566, #57277, #38977 ) ;
#2589 = EDGE_CURVE ( 'NONE', #44855, #52059, #25295, .T. ) ;
#2590 = CARTESIAN_POINT ( 'NONE',  ( -0.4104034600731000237, -81.14228670038500013, 1.244744919973999941 ) ) ;
#2591 = CARTESIAN_POINT ( 'NONE',  ( 6.047694738970999850, -79.33324558444999752, -11.09599207243999963 ) ) ;
#2592 = CARTESIAN_POINT ( 'NONE',  ( 12.83677071375000089, -55.57261389723999656, -2.062839858856999609 ) ) ;
#2593 = CARTESIAN_POINT ( 'NONE',  ( -9.520207861471000399, -78.95852403778498285, -0.1897854149113999966 ) ) ;
#2594 = VECTOR ( 'NONE', #28469, 1000.000000000000000 ) ;
#2595 = CARTESIAN_POINT ( 'NONE',  ( -0.8762103189736000219, -81.41053970282000307, -1.416501064863000092 ) ) ;
#2596 = CARTESIAN_POINT ( 'NONE',  ( 4.230954068466677320, -79.94294377347027591, 9.882283910680856209 ) ) ;
#2597 = CARTESIAN_POINT ( 'NONE',  ( 0.6980205241115000625, -79.83136847860799890, 1.456015547280999911 ) ) ;
#2598 = VERTEX_POINT ( 'NONE', #46243 ) ;
#2599 = CARTESIAN_POINT ( 'NONE',  ( 10.69999999999999929, -81.79999999999998295, 0.000000000000000000 ) ) ;
#2600 = CARTESIAN_POINT ( 'NONE',  ( -7.000000000000000000, -81.19999999999998863, 0.000000000000000000 ) ) ;
#2601 = CARTESIAN_POINT ( 'NONE',  ( -0.5454189353424065967, -78.86967215500642681, -3.431877180009151651 ) ) ;
#2602 = ORIENTED_EDGE ( 'NONE', *, *, #53719, .T. ) ;
#2603 = CARTESIAN_POINT ( 'NONE',  ( 0.1299632413661999941, -79.18100181365798562, 11.04812215732000169 ) ) ;
#2604 = DIRECTION ( 'NONE',  ( 0.000000000000000000, -1.000000000000000000, 0.000000000000000000 ) ) ;
#2605 = EDGE_CURVE ( 'NONE', #6077, #44782, #26365, .T. ) ;
#2606 = DIRECTION ( 'NONE',  ( 0.7071067811865474617, 0.000000000000000000, -0.7071067811865474617 ) ) ;
#2607 = ORIENTED_EDGE ( 'NONE', *, *, #55721, .F. ) ;
#2608 = CARTESIAN_POINT ( 'NONE',  ( 4.442094508599000235, -77.41361025341399227, -11.32474889210000057 ) ) ;
#2609 = CARTESIAN_POINT ( 'NONE',  ( -4.690256031270999770, -77.64794858637398534, -10.30503454587000078 ) ) ;
#2610 = ORIENTED_EDGE ( 'NONE', *, *, #23773, .F. ) ;
#2611 = EDGE_LOOP ( 'NONE', ( #45072, #3068, #21608, #2789, #31112, #29819 ) ) ;
#2612 = CARTESIAN_POINT ( 'NONE',  ( -0.06320921880059908460, -80.47953876087936465, 1.248225759446036864 ) ) ;
#2613 = DIRECTION ( 'NONE',  ( 0.000000000000000000, -1.000000000000000000, 0.000000000000000000 ) ) ;
#2614 = CARTESIAN_POINT ( 'NONE',  ( -9.358268528169000788, -79.53341926633650871, -2.797054701638000296 ) ) ;
#2615 = VERTEX_POINT ( 'NONE', #33204 ) ;
#2616 = CARTESIAN_POINT ( 'NONE',  ( -6.040190233171999878, -79.49506692201099156, 9.093484917090998820 ) ) ;
#2617 = ORIENTED_EDGE ( 'NONE', *, *, #9555, .F. ) ;
#2618 = CARTESIAN_POINT ( 'NONE',  ( -0.5434382620641865502, -79.24014818529076365, -1.152742929317775777 ) ) ;
#2619 = CARTESIAN_POINT ( 'NONE',  ( 3.861138328465000047, -76.85095248368000398, 8.493887087553000370 ) ) ;
#2620 = AXIS2_PLACEMENT_3D ( 'NONE', #24627, #10470, #24038 ) ;
#2621 = CARTESIAN_POINT ( 'NONE',  ( 7.758899961864000439, -54.49918178063000340, 10.31442855571999928 ) ) ;
#2622 = CARTESIAN_POINT ( 'NONE',  ( 1.500000000000000000, -80.65000000000000568, 0.000000000000000000 ) ) ;
#2623 = CARTESIAN_POINT ( 'NONE',  ( 1.500000000000000000, -81.15000000000000568, 0.000000000000000000 ) ) ;
#2624 = CARTESIAN_POINT ( 'NONE',  ( -7.604857126344345630, -78.49557913613843141, 6.061321726079917482 ) ) ;
#2625 = CARTESIAN_POINT ( 'NONE',  ( 9.831723082683108572, -80.55996316945166313, -5.387191927894570576 ) ) ;
#2626 = CIRCLE ( 'NONE', #15812, 0.8000000000000011546 ) ;
#2627 = CARTESIAN_POINT ( 'NONE',  ( 11.88382656225999945, -78.38991971485397414, -1.513515996960000276 ) ) ;
#2628 = CARTESIAN_POINT ( 'NONE',  ( 0.06506789018937424174, -81.32083334150291876, 4.050171521248369544 ) ) ;
#2629 = CARTESIAN_POINT ( 'NONE',  ( -1.250000000000000000, -83.09999999999999432, 0.000000000000000000 ) ) ;
#2630 = CARTESIAN_POINT ( 'NONE',  ( -3.808791273250000220, -78.64482046129089099, 1.219936614250999973 ) ) ;
#2631 = EDGE_CURVE ( 'NONE', #49572, #20471, #39419, .T. ) ;
#2632 = CARTESIAN_POINT ( 'NONE',  ( -1.343382297838000047E-14, -80.79999999999999716, 0.000000000000000000 ) ) ;
#2633 = CARTESIAN_POINT ( 'NONE',  ( 10.36222489920000100, -60.02120223818999989, -7.631889817968999346 ) ) ;
#2634 = VECTOR ( 'NONE', #50400, 1000.000000000000114 ) ;
#2635 = B_SPLINE_CURVE_WITH_KNOTS ( 'NONE', 3,
 ( #33452, #42620, #51489, #11047, #38468, #2186, #38177, #56198, #15745, #33742, #11330, #47357, #6886, #21613, #57342, #13033, #40499, #17774, #57627, #26036, #12465, #53202, #26905, #30465, #8915, #48496, #39903, #39335, #25758, #18070, #44061, #44933, #44639, #48781, #35764, #58212, #31322, #3608, #39619, #35169, #22488, #17475, #48222, #49365 ),
 .UNSPECIFIED., .F., .F.,
 ( 4, 2, 2, 2, 2, 2, 2, 2, 2, 2, 2, 2, 2, 2, 2, 2, 2, 2, 2, 2, 2, 4 ),
 ( 1.714264432196704922E-08, 0.03125001607122906977, 0.06250001499981379383, 0.09375001392839851788, 0.1250000128569832558, 0.1562500117855679937, 0.1875000107141527039, 0.2187500096427374141, 0.2500000085713221520, 0.2812500074999068067, 0.3125000064284915724, 0.3281250058927839830, 0.3437500053570763381, 0.3593750048213686932, 0.3750000042856610483, 0.3906250037499534589, 0.4062500032142458140, 0.4218750026785381690, 0.4375000021428305241, 0.4687500010714153453, 0.4843750005357077004, 0.5000000000000000000 ),
 .UNSPECIFIED. ) ;
#2636 = CARTESIAN_POINT ( 'NONE',  ( -12.26143800982999998, -78.98420536356999833, -0.2371146996492999870 ) ) ;
#2637 = CARTESIAN_POINT ( 'NONE',  ( 11.61133755414000035, -76.77471726614500369, 3.999933378912999604 ) ) ;
#2638 = CARTESIAN_POINT ( 'NONE',  ( 13.94827576517086065, -33.10361340872000113, 0.001644113314434763381 ) ) ;
#2639 = EDGE_CURVE ( 'NONE', #51790, #14050, #28489, .T. ) ;
#2640 = CARTESIAN_POINT ( 'NONE',  ( -11.68767212001979061, -77.82083333333333997, -3.140974612311365988 ) ) ;
#2641 = ORIENTED_EDGE ( 'NONE', *, *, #31744, .F. ) ;
#2642 = CARTESIAN_POINT ( 'NONE',  ( 1.545086291967713299, -80.49690600801427820, -0.05127199417640600221 ) ) ;
#2643 = CARTESIAN_POINT ( 'NONE',  ( 12.49830695671999869, -60.00970582242000262, -1.666977511085999897 ) ) ;
#2644 = CARTESIAN_POINT ( 'NONE',  ( 2.065550207748000133, -23.42565079331000177, 12.82162303854000029 ) ) ;
#2645 = CARTESIAN_POINT ( 'NONE',  ( 12.70556836347999941, -16.77227722772000007, -1.774194455291999869E-09 ) ) ;
#2646 = CARTESIAN_POINT ( 'NONE',  ( 2.191379079411999609, -3.651279784235999859, -2.470611052852000000 ) ) ;
#2647 = B_SPLINE_SURFACE_WITH_KNOTS ( 'NONE', 3, 3, ( 
 ( #16906, #53793, #40201, #49069, #95, #36064, #8617, #54084, #8038, #30172, #7754, #3331, #21326, #52918, #26325, #44339, #3892, #21895, #53491, #26602, #14155, #13869, #15031, #5016, #33027, #28602, #41907, #54895, #49905, #23316, #27438, #46649, #36304, #51073, #1192 ),
 ( #50779, #9452, #5305, #18606, #10621, #6176, #5586, #24186, #50485, #41611, #10036, #28018, #27727, #32153, #10325, #46064, #23599, #41032, #45474, #28305, #45771, #623, #46356, #23020, #42204, #9739, #18312, #41323, #55484, #908, #36595, #19182, #54328, #18890, #54617 ),
 ( #50192, #31863, #36883, #14445, #37463, #32440, #37177, #55190, #14731, #32731, #5880, #23888, #1480, #19470, #10916, #16493, #25626, #7625, #34472, #29469, #11777, #15912, #2636, #38631, #47525, #7054, #28896, #2914, #52220, #47806, #20064, #7338, #33323, #25053, #47233 ),
 ( #51659, #1771, #6761, #38915, #24771, #42494, #20630, #48094, #11207, #46943, #43076, #12061, #25338, #29185, #56075, #2063, #52503, #30041, #38052, #56933, #19765, #37761, #43354, #20912, #15620, #56649, #55783, #42784, #15333, #51360, #6468, #16206, #33615, #24479, #2348 ) ),
 .UNSPECIFIED., .F., .F., .F.,
 ( 4, 4 ),
 ( 4, 1, 1, 1, 1, 1, 1, 1, 1, 1, 1, 1, 1, 1, 1, 1, 1, 1, 1, 1, 1, 1, 1, 1, 1, 1, 1, 1, 1, 1, 1, 1, 4 ),
 ( -0.02000000000005000209, 1.020000000000000018 ),
 ( -0.01035614953205000154, 0.006472593457530000441, 0.02330133644711000068, 0.04013007943667999677, 0.05695882242625999875, 0.07378756541584000073, 0.09061630840541000376, 0.1074450513949999908, 0.1242737943845999976, 0.1411025373741000011, 0.1579312803636999940, 0.1747600233533000147, 0.1915887663428999799, 0.2084175093325000006, 0.2252462523220000179, 0.2420749953115999831, 0.2589037383012000038, 0.2757324812907999689, 0.2925612242803000140, 0.3093899672698999792, 0.3262187102594999999, 0.3430474532491000206, 0.3598761962385999547, 0.3767049392282000309, 0.3935336822177999960, 0.4103624252073999612, 0.4271911681970000374, 0.4440199111864999715, 0.4608486541761000477, 0.4776773971657000128, 0.4945061401552999780, 0.5113348831447999121, 0.5281636261344000438 ),
 .UNSPECIFIED. ) ;
#2648 = CARTESIAN_POINT ( 'NONE',  ( -11.23155942826000064, -77.90976265171399007, 4.672751159098000429 ) ) ;
#2649 = CARTESIAN_POINT ( 'NONE',  ( -3.921497456393000292, -77.86283724644100346, -8.915242756422999904 ) ) ;
#2651 = CARTESIAN_POINT ( 'NONE',  ( -0.6498089757737999239, -78.15792523368020284, 1.148178518287000127 ) ) ;
#2650 = CARTESIAN_POINT ( 'NONE',  ( -9.690163305986116526, -76.15162990441653790, 6.645162696918485601 ) ) ;
#2652 = CARTESIAN_POINT ( 'NONE',  ( 0.6735630312197999903, -82.86657026302199824, -1.435516540950999786 ) ) ;
#2653 = CARTESIAN_POINT ( 'NONE',  ( -9.823574345946489927, -79.56680724124903747, 4.374665960120871944 ) ) ;
#2654 = ORIENTED_EDGE ( 'NONE', *, *, #15989, .T. ) ;
#2655 = CARTESIAN_POINT ( 'NONE',  ( 0.000000000000000000, -9.295797029142999435, 0.000000000000000000 ) ) ;
#2656 = CARTESIAN_POINT ( 'NONE',  ( -11.40016033654000083, -79.16505199243299273, 3.876673637571999897 ) ) ;
#2657 = CARTESIAN_POINT ( 'NONE',  ( 0.5334414343224818111, -79.12052801969377924, 9.504702743072071414 ) ) ;
#2658 = ADVANCED_FACE ( 'NONE', ( #5771 ), #36744, .F. ) ;
#2659 = DIRECTION ( 'NONE',  ( 0.000000000000000000, 0.000000000000000000, -1.000000000000000000 ) ) ;
#2660 = DIRECTION ( 'NONE',  ( 0.000000000000000000, 0.000000000000000000, -1.000000000000000000 ) ) ;
#2661 = FACE_OUTER_BOUND ( 'NONE', #36438, .T. ) ;
#2662 = CARTESIAN_POINT ( 'NONE',  ( -1.274026893842000074, -79.96482190487999731, 9.474508900323998617 ) ) ;
#2663 = CARTESIAN_POINT ( 'NONE',  ( -11.68767212001978706, -77.92083333333333428, -3.140974612311364655 ) ) ;
#2664 = CARTESIAN_POINT ( 'NONE',  ( -10.42531125072000009, -55.53514854654000032, -7.624341767124000135 ) ) ;
#2665 = ORIENTED_EDGE ( 'NONE', *, *, #47411, .F. ) ;
#2666 = DIRECTION ( 'NONE',  ( -1.000000000000000000, 0.000000000000000000, 0.000000000000000000 ) ) ;
#2667 = CARTESIAN_POINT ( 'NONE',  ( 3.970614904013836988, -79.39750627768901836, 11.12517343397338898 ) ) ;
#2668 = DIRECTION ( 'NONE',  ( -1.000000000000000000, 0.000000000000000000, 0.000000000000000000 ) ) ;
#2669 = B_SPLINE_SURFACE_WITH_KNOTS ( 'NONE', 3, 3, ( 
 ( #15754, #38763, #7476, #24326, #42342, #19902, #25473, #3053, #15469, #21048, #33749, #39050, #57065, #51498, #16625, #34610, #11055, #29037, #47076, #6604, #24616, #42629, #4498, #54093, #44067, #35772, #48787, #8332, #53800, #31628, #17482, #34894, #16914, #21902, #8046, #8921, #4200, #22496, #3337, #57351, #57925, #7763, #31038, #40507, #26911, #43786, #40209, #3616, #30753, #31330, #44646, #49374, #48501, #17782, #13334, #53497, #35469, #49074, #3898, #102, #52923, #26331, #39344, #12757, #25766, #39911, #39625 ),
 ( #44942, #13631, #21331, #18077, #13040, #26043, #36072, #12474, #30475, #8624, #21621, #57633, #22198, #17189, #26610, #35178, #53209, #44345, #58219, #391, #55248, #37522, #28076, #45535, #45829, #37231, #55540, #15091, #19529, #54953, #41671, #49670, #9215, #27493, #1536, #1252, #28367, #54671, #9506, #19239, #14794, #681, #50251, #4786, #27201, #22788, #45239, #46125, #14505, #40797, #32789, #5649, #5080, #10382, #18664, #46413, #9801, #18368, #5943, #36361, #54388, #27784, #23658, #13925, #14212, #31920, #41383 ),
 ( #966, #5365, #23947, #41963, #49965, #23075, #41090, #36652, #32209, #23372, #18949, #36942, #32496, #50543, #10096, #38399, #16264, #2972, #28664, #7394, #33960, #42265, #34243, #51712, #24828, #33385, #56419, #11262, #29243, #7111, #24249, #20119, #1831, #19827, #47290, #52278, #6818, #2695, #43414, #42843, #2402, #51421, #56987, #20971, #46713, #33086, #20403, #51997, #15968, #38109, #2120, #33675, #38976, #6233, #20689, #15678, #11552, #29530, #47586, #43137, #25112, #6527, #38687, #51130, #37819, #11833, #56707 ),
 ( #29813, #24539, #47865, #28957, #10978, #10684, #25397, #55840, #15391, #46999, #42552, #56129, #48430, #4123, #3266, #39837, #12403, #22123, #21257, #49298, #3832, #26262, #21831, #8550, #12966, #8850, #35104, #57852, #4422, #40133, #39263, #58146, #44568, #17409, #34822, #35391, #22422, #44275, #53422, #30965, #53138, #26541, #53727, #44868, #26840, #49002, #34531, #39553, #17713, #52850, #16549, #35698, #13266, #31257, #17119, #43995, #40434, #52564, #12116, #7972, #25969, #30101, #48152, #57558, #7683, #30394, #25684 ) ),
 .UNSPECIFIED., .F., .F., .F.,
 ( 4, 4 ),
 ( 4, 1, 1, 1, 1, 1, 1, 1, 1, 1, 1, 1, 1, 1, 1, 1, 1, 1, 1, 1, 1, 1, 1, 1, 1, 1, 1, 1, 1, 1, 1, 1, 1, 1, 1, 1, 1, 1, 1, 1, 1, 1, 1, 1, 1, 1, 1, 1, 1, 1, 1, 1, 1, 1, 1, 1, 1, 1, 1, 1, 1, 1, 1, 1, 4 ),
 ( -0.5168282991434000051, 1.516828299142999992 ),
 ( -0.02000000000000000042, -0.003749999999999999861, 0.01250000000000000069, 0.02875000000000000125, 0.04499999999999999833, 0.06124999999999999889, 0.07749999999999999944, 0.09375000000000000000, 0.1100000000000000006, 0.1262500000000000011, 0.1424999999999999878, 0.1587500000000000022, 0.1749999999999999889, 0.1912500000000000033, 0.2074999999999999900, 0.2237500000000000044, 0.2399999999999999911, 0.2562499999999999778, 0.2725000000000000200, 0.2887500000000000067, 0.3049999999999999933, 0.3212499999999999800, 0.3375000000000000222, 0.3537500000000000089, 0.3699999999999999956, 0.3862499999999999822, 0.4025000000000000244, 0.4187500000000000111, 0.4349999999999999978, 0.4512499999999999845, 0.4675000000000000266, 0.4837500000000000133, 0.5000000000000000000, 0.5162499999999999867, 0.5324999999999999734, 0.5487499999999999600, 0.5649999999999999467, 0.5812500000000000444, 0.5975000000000000311, 0.6137500000000000178, 0.6300000000000000044, 0.6462499999999999911, 0.6624999999999999778, 0.6787499999999999645, 0.6949999999999999512, 0.7112500000000000488, 0.7275000000000000355, 0.7437500000000000222, 0.7600000000000000089, 0.7762499999999999956, 0.7924999999999999822, 0.8087499999999999689, 0.8249999999999999556, 0.8412500000000000533, 0.8575000000000000400, 0.8737500000000000266, 0.8900000000000000133, 0.9062500000000000000, 0.9224999999999999867, 0.9387499999999999734, 0.9549999999999999600, 0.9712499999999999467, 0.9875000000000000444, 1.003749999999999920, 1.020000000000000018 ),
 .UNSPECIFIED. ) ;
#2670 = CARTESIAN_POINT ( 'NONE',  ( 0.6793202165550557003, -81.42948271688828754, 1.050371840538202539 ) ) ;
#2671 = EDGE_CURVE ( 'NONE', #5427, #13118, #49955, .T. ) ;
#2672 = ORIENTED_EDGE ( 'NONE', *, *, #23098, .F. ) ;
#2673 = CARTESIAN_POINT ( 'NONE',  ( 0.000000000000000000, -87.15000000002500258, 0.000000000000000000 ) ) ;
#2674 = DIRECTION ( 'NONE',  ( 0.000000000000000000, -1.000000000000000000, 0.000000000000000000 ) ) ;
#2675 = CARTESIAN_POINT ( 'NONE',  ( 1.667936697358999965, -56.03537109808000594, -12.53241208775000004 ) ) ;
#2676 = EDGE_CURVE ( 'NONE', #13401, #36778, #51252, .T. ) ;
#2677 = CARTESIAN_POINT ( 'NONE',  ( 9.375326036246072192, -76.27905215015013596, 5.420036776477389573 ) ) ;
#2678 = CARTESIAN_POINT ( 'NONE',  ( -6.606163316386915341, -78.52711955731416538, 8.596028648480132262 ) ) ;
#2679 = CARTESIAN_POINT ( 'NONE',  ( -4.465297566879000257, -79.62232954496899140, 8.686876450551999085 ) ) ;
#2680 = ORIENTED_EDGE ( 'NONE', *, *, #10718, .F. ) ;
#2681 = ORIENTED_EDGE ( 'NONE', *, *, #1428, .F. ) ;
#2682 = CARTESIAN_POINT ( 'NONE',  ( -6.722591978632999066, -76.33855707708200100, -10.50348591810000087 ) ) ;
#2683 = CARTESIAN_POINT ( 'NONE',  ( -4.872804940501344717, -78.68772107945071070, -9.582789324058202496 ) ) ;
#2684 = B_SPLINE_CURVE_WITH_KNOTS ( 'NONE', 3,
 ( #37567, #33128, #50876, #37271, #28407, #41712 ),
 .UNSPECIFIED., .F., .F.,
 ( 4, 1, 1, 4 ),
 ( 0.000000000000000000, 0.3333333333333000081, 0.6666666666667000474, 1.000000000000000000 ),
 .UNSPECIFIED. ) ;
#2685 = ORIENTED_EDGE ( 'NONE', *, *, #47049, .F. ) ;
#2686 = CARTESIAN_POINT ( 'NONE',  ( 7.618394506893999996, -18.77286435802000142, 10.53494428259999971 ) ) ;
#2687 = B_SPLINE_CURVE_WITH_KNOTS ( 'NONE', 3,
 ( #52094, #29913, #38787, #11652, #16651, #43815 ),
 .UNSPECIFIED., .F., .F.,
 ( 4, 1, 1, 4 ),
 ( 0.000000000000000000, 0.3333333333333000081, 0.6666666666667000474, 1.000000000000000000 ),
 .UNSPECIFIED. ) ;
#2688 = CARTESIAN_POINT ( 'NONE',  ( -2.879226727952121312, -77.59583333333331723, 10.71369944335146052 ) ) ;
#2689 = EDGE_CURVE ( 'NONE', #13177, #23377, #36586, .T. ) ;
#2690 = CARTESIAN_POINT ( 'NONE',  ( 1.782734487931668887, -54.67754631410036836, 12.71547286922865183 ) ) ;
#2691 = CARTESIAN_POINT ( 'NONE',  ( 11.69353635062999963, -78.45185341714999083, 5.202647212677000255 ) ) ;
#2692 = DIRECTION ( 'NONE',  ( 0.000000000000000000, -1.000000000000000000, 0.000000000000000000 ) ) ;
#2693 = DIRECTION ( 'NONE',  ( 0.000000000000000000, 1.000000000000000000, 0.000000000000000000 ) ) ;
#2694 = DIRECTION ( 'NONE',  ( 0.000000000000000000, -1.000000000000000000, 3.571217395878000445E-14 ) ) ;
#2695 = CARTESIAN_POINT ( 'NONE',  ( -0.2721098858049000313, -79.21082493523199730, 11.21356619464000026 ) ) ;
#2696 = CARTESIAN_POINT ( 'NONE',  ( 11.75000000000000000, -75.95000000000000284, 0.000000000000000000 ) ) ;
#2697 = ORIENTED_EDGE ( 'NONE', *, *, #42819, .F. ) ;
#2698 = CARTESIAN_POINT ( 'NONE',  ( 6.818082927312866026, -78.12593218097666181, 9.623674802968025688 ) ) ;
#2699 = ORIENTED_EDGE ( 'NONE', *, *, #1617, .T. ) ;
#2700 = CARTESIAN_POINT ( 'NONE',  ( 3.557252205646057597, -77.25651624396304840, -8.541931941478511092 ) ) ;
#2701 = CARTESIAN_POINT ( 'NONE',  ( -0.3164422402712000482, -79.69022655590600834, 1.381999876370000102 ) ) ;
#2702 = CARTESIAN_POINT ( 'NONE',  ( 10.79432616025544611, -77.57799259947435644, -3.050267481686816939 ) ) ;
#2704 = EDGE_CURVE ( 'NONE', #10810, #35609, #51353, .T. ) ;
#2703 = CARTESIAN_POINT ( 'NONE',  ( 1.391768007815999963, -77.76484642788379631, -0.6016011292324999760 ) ) ;
#2705 = FACE_OUTER_BOUND ( 'NONE', #2996, .T. ) ;
#2706 = DIRECTION ( 'NONE',  ( -1.000000000000000000, 0.000000000000000000, 0.000000000000000000 ) ) ;
#2707 = CARTESIAN_POINT ( 'NONE',  ( -1.566959183383000109, -78.36705617198001050, 0.4396611996733000294 ) ) ;
#2708 = EDGE_CURVE ( 'NONE', #53789, #24195, #958, .T. ) ;
#2709 = CARTESIAN_POINT ( 'NONE',  ( -3.697742159549999741, -79.39521842720699851, 10.41175280961999938 ) ) ;
#2710 = CARTESIAN_POINT ( 'NONE',  ( -12.80090744921000123, -59.56232687415000271, 1.980532734072999901 ) ) ;
#2711 = CARTESIAN_POINT ( 'NONE',  ( -3.288309003486036275, -1.962318126216331837, -0.5433950876430284627 ) ) ;
#2712 = ORIENTED_EDGE ( 'NONE', *, *, #5626, .F. ) ;
#2713 = CARTESIAN_POINT ( 'NONE',  ( 0.4046438523804999909, -81.47411572283999703, -1.654233492563000008 ) ) ;
#2714 = CARTESIAN_POINT ( 'NONE',  ( -0.7407245532275998912, -81.59442870581999330, -1.017507444502999903 ) ) ;
#2715 = CARTESIAN_POINT ( 'NONE',  ( 7.601397897754999633, -18.75000000310999937, -10.07627163191000008 ) ) ;
#2716 = CARTESIAN_POINT ( 'NONE',  ( 11.97742283006000186, -77.81769738389299107, 0.2395971301470000148 ) ) ;
#2717 = CARTESIAN_POINT ( 'NONE',  ( 4.411570631796044140, -76.99999999999998579, 8.157888388493256926 ) ) ;
#2718 = CARTESIAN_POINT ( 'NONE',  ( 1.309259533489598670, -78.51346957102681756, 0.2203786214735808102 ) ) ;
#2719 = CIRCLE ( 'NONE', #8341, 10.25000000000000000 ) ;
#2720 = CARTESIAN_POINT ( 'NONE',  ( 3.520922223394743256, -1.998246443813628703, -0.07578465938312391181 ) ) ;
#2721 = CARTESIAN_POINT ( 'NONE',  ( 9.345760913908002010, -78.40230194988500045, 2.683384691900000174 ) ) ;
#2722 = CARTESIAN_POINT ( 'NONE',  ( 2.813750093493999849, -77.79193342313199366, -9.096877851405000825 ) ) ;
#2723 = CARTESIAN_POINT ( 'NONE',  ( -3.106054555984679055, -86.10000000000019327, 1.382904586457923246 ) ) ;
#2724 = CARTESIAN_POINT ( 'NONE',  ( 10.06402303786000196, -78.24492912598299199, -4.229752508564000202 ) ) ;
#2725 = CARTESIAN_POINT ( 'NONE',  ( 8.596418555780450887, -79.19791666666667140, -6.606377239730321982 ) ) ;
#2726 = CARTESIAN_POINT ( 'NONE',  ( -10.51811773240999948, -81.00517844751929886, 2.900480251473000148 ) ) ;
#2727 = CARTESIAN_POINT ( 'NONE',  ( -0.9820397338569999413, -80.70308451575900222, -0.7733679338621000099 ) ) ;
#2728 = ORIENTED_EDGE ( 'NONE', *, *, #37415, .F. ) ;
#2729 = CARTESIAN_POINT ( 'NONE',  ( 10.98521938008762078, -18.65929923595093243, -0.5702549022801662870 ) ) ;
#2730 = CARTESIAN_POINT ( 'NONE',  ( -4.043785186575674651, -78.67389998729009903, -2.284879765406155006 ) ) ;
#2731 = CARTESIAN_POINT ( 'NONE',  ( -5.751434148371999733, -77.84826253771599625, -9.630115047516998317 ) ) ;
#2732 = CARTESIAN_POINT ( 'NONE',  ( -10.79326785783000098, -79.38437425209399123, -1.992331681952000055 ) ) ;
#2733 = CARTESIAN_POINT ( 'NONE',  ( -1.440962122118119471, -79.37367604318139058, -0.4505052090234867301 ) ) ;
#2734 = CARTESIAN_POINT ( 'NONE',  ( -3.903296333128821516, -84.63541667053057438, 1.088434527864090340 ) ) ;
#2735 = CARTESIAN_POINT ( 'NONE',  ( -11.14126686682999967, -76.54389604793398405, 4.853629488117999990 ) ) ;
#2736 = CARTESIAN_POINT ( 'NONE',  ( 11.75000000000000000, -78.45000000000000284, 0.000000000000000000 ) ) ;
#2737 = CARTESIAN_POINT ( 'NONE',  ( -8.838834764832000701, -23.25000000000000000, 8.838834764832000701 ) ) ;
#2738 = VERTEX_POINT ( 'NONE', #28784 ) ;
#2739 = CARTESIAN_POINT ( 'NONE',  ( -1.250000000000000000, -80.09999999999999432, 0.000000000000000000 ) ) ;
#2740 = DIRECTION ( 'NONE',  ( 0.000000000000000000, 1.000000000000000000, 0.000000000000000000 ) ) ;
#2741 = CARTESIAN_POINT ( 'NONE',  ( 10.45148855949000044, -78.02152425389999735, 3.906137931512999817 ) ) ;
#2742 = CARTESIAN_POINT ( 'NONE',  ( -9.522678871818975210, -79.15755207139983440, -7.317142126971875271 ) ) ;
#2743 = CARTESIAN_POINT ( 'NONE',  ( -1.164828128805999992E-14, -72.75000000040999737, 0.000000000000000000 ) ) ;
#2744 = CARTESIAN_POINT ( 'NONE',  ( -10.12290050122000018, -55.54999999974999980, 7.648026767069000087 ) ) ;
#2745 = CARTESIAN_POINT ( 'NONE',  ( 0.4264742922811849413, -82.70158460137095346, 1.451405935591948637 ) ) ;
#2746 = CARTESIAN_POINT ( 'NONE',  ( -0.9383909286133819139, -79.65811737660978054, -0.8288992896692728429 ) ) ;
#2747 = ORIENTED_EDGE ( 'NONE', *, *, #47978, .T. ) ;
#2748 = CARTESIAN_POINT ( 'NONE',  ( 2.062597299672999540, -19.21514526754999963, 12.87022657274000004 ) ) ;
#2749 = CARTESIAN_POINT ( 'NONE',  ( -12.49830695668999958, -23.20970582274999927, 1.666977511086999986 ) ) ;
#2750 = VERTEX_POINT ( 'NONE', #3102 ) ;
#2751 = ORIENTED_EDGE ( 'NONE', *, *, #16332, .T. ) ;
#2752 = CARTESIAN_POINT ( 'NONE',  ( -12.66319948253000049, -53.61851729328000005, -0.1456213732515000137 ) ) ;
#2753 = AXIS2_PLACEMENT_3D ( 'NONE', #26508, #35071, #17088 ) ;
#2754 = ORIENTED_EDGE ( 'NONE', *, *, #48627, .T. ) ;
#2755 = VERTEX_POINT ( 'NONE', #44119 ) ;
#2756 = CARTESIAN_POINT ( 'NONE',  ( -2.812084287824942574, -81.00000000000000000, -10.57161323837342159 ) ) ;
#2757 = CARTESIAN_POINT ( 'NONE',  ( -7.506332976489000330, -77.13807570069999997, -7.926558599818001483 ) ) ;
#2758 = VECTOR ( 'NONE', #47296, 1000.000000000000227 ) ;
#2759 = CONTEXT_DEPENDENT_SHAPE_REPRESENTATION ( #8045, #20199 ) ;
#2760 = EDGE_CURVE ( 'NONE', #2165, #27203, #12636, .T. ) ;
#2761 = B_SPLINE_CURVE_WITH_KNOTS ( 'NONE', 3,
 ( #32593, #11357, #47092, #6623, #46219, #24634, #10477, #15773, #1344, #33765, #5745, #51803, #23753, #55345, #24045, #46512, #14888, #32886, #50930, #28463, #6036, #1632 ),
 .UNSPECIFIED., .F., .F.,
 ( 4, 2, 2, 2, 2, 2, 2, 2, 2, 2, 4 ),
 ( 0.000000000000000000, 0.06249999999999995837, 0.1249999999999999167, 0.2500000000000000000, 0.3750000000000000000, 0.5000000000000001110, 0.6250000000000001110, 0.7500000000000001110, 0.8125000000000001110, 0.8750000000000001110, 1.000000000000000000 ),
 .UNSPECIFIED. ) ;
#2762 = CARTESIAN_POINT ( 'NONE',  ( 4.349579488465999511, -79.03151332859899014, 8.780633650160998727 ) ) ;
#2763 = EDGE_CURVE ( 'NONE', #13397, #16171, #42966, .T. ) ;
#2764 = CARTESIAN_POINT ( 'NONE',  ( -1.769489979047951467, -78.20976201800445438, -9.079134725190300514 ) ) ;
#2765 = CARTESIAN_POINT ( 'NONE',  ( 5.643184558664585460, -76.28046875019616380, -9.211581335339863230 ) ) ;
#2766 = ORIENTED_EDGE ( 'NONE', *, *, #22856, .F. ) ;
#2767 = ORIENTED_EDGE ( 'NONE', *, *, #15574, .F. ) ;
#2768 = CARTESIAN_POINT ( 'NONE',  ( -3.474029939969885739, -77.50579965437593444, 8.573561196712942589 ) ) ;
#2769 = CARTESIAN_POINT ( 'NONE',  ( -12.70305380112262661, -25.03154493769341116, 0.8725910145369886184 ) ) ;
#2770 = CARTESIAN_POINT ( 'NONE',  ( 0.000000000000000000, -33.10361340872000113, 0.000000000000000000 ) ) ;
#2771 = CARTESIAN_POINT ( 'NONE',  ( 3.248345031021000029, -78.17798956026199164, 9.144340540792999406 ) ) ;
#2772 = CARTESIAN_POINT ( 'NONE',  ( 7.635227771910129135, -60.56609606924865119, 10.36745004612414789 ) ) ;
#2773 = LINE ( 'NONE', #29614, #29892 ) ;
#2774 = CARTESIAN_POINT ( 'NONE',  ( 10.52776997023000050, -80.08830587811999635, 3.979665013433000720 ) ) ;
#2775 = ADVANCED_FACE ( 'NONE', ( #43538 ), #24489, .F. ) ;
#2776 = CARTESIAN_POINT ( 'NONE',  ( -1.526555281555000088, -80.22845843187998582, -0.4289821568622999570 ) ) ;
#2777 = DIRECTION ( 'NONE',  ( 0.000000000000000000, -1.000000000000000000, 0.000000000000000000 ) ) ;
#2778 = CARTESIAN_POINT ( 'NONE',  ( -1.492020074518721318, -79.73778082640328080, 0.2322189972777134459 ) ) ;
#2779 = CARTESIAN_POINT ( 'NONE',  ( 6.711318802534000483, -78.25891332859899308, 7.292371261484999145 ) ) ;
#2780 = DIRECTION ( 'NONE',  ( 0.000000000000000000, -1.000000000000000000, 0.000000000000000000 ) ) ;
#2781 = CARTESIAN_POINT ( 'NONE',  ( 12.50000000000000000, -26.93717104351999936, 1.868110276009999908E-13 ) ) ;
#2783 = CARTESIAN_POINT ( 'NONE',  ( -0.3862712429687000237, -82.25000000000000000, -1.188820645369000006 ) ) ;
#2782 = CARTESIAN_POINT ( 'NONE',  ( -1.210889911462935231, -78.48544186924020494, 9.249751145355588733 ) ) ;
#2784 = LINE ( 'NONE', #20784, #31718 ) ;
#2785 = CARTESIAN_POINT ( 'NONE',  ( 4.535769924631999572, -80.15130006555698117, -10.22046309969000077 ) ) ;
#2786 = EDGE_CURVE ( 'NONE', #49814, #47867, #21668, .T. ) ;
#2787 = CARTESIAN_POINT ( 'NONE',  ( 3.938458446976999205, -79.30999999999998806, -8.369650235310999165 ) ) ;
#2788 = CARTESIAN_POINT ( 'NONE',  ( -3.295646577751982331, -1.720822363418331502, 1.264561824618803509 ) ) ;
#2789 = ORIENTED_EDGE ( 'NONE', *, *, #23705, .F. ) ;
#2790 = CARTESIAN_POINT ( 'NONE',  ( 9.000000000000000000, -4.000000000000000000, 0.000000000000000000 ) ) ;
#2791 = DIRECTION ( 'NONE',  ( 0.000000000000000000, 1.000000000000000000, 0.000000000000000000 ) ) ;
#2792 = ADVANCED_FACE ( 'NONE', ( #12523 ), #11625, .F. ) ;
#2793 = CARTESIAN_POINT ( 'NONE',  ( 9.931063219240325424, -17.87724209358196958, -7.763994033417543683 ) ) ;
#2794 = CARTESIAN_POINT ( 'NONE',  ( -8.024068383896736378, -77.16415510318682891, -4.770143147090037949 ) ) ;
#2795 = CARTESIAN_POINT ( 'NONE',  ( -1.215810657191000121, -1.729405165122000154, -3.437332899015999921 ) ) ;
#2796 = B_SPLINE_CURVE_WITH_KNOTS ( 'NONE', 3,
 ( #22569, #49745, #9286, #40581, #8694, #50033, #26685, #58292, #17855, #27276, #35844, #45313, #5150, #55614, #51492, #20188, #45899, #24610, #37012 ),
 .UNSPECIFIED., .F., .F.,
 ( 4, 1, 1, 1, 1, 1, 1, 1, 1, 1, 1, 1, 1, 1, 1, 1, 4 ),
 ( 0.000000000000000000, 0.04500074405000878408, 0.1100006377635261434, 0.1750005314770704257, 0.2400004251906146802, 0.3050003189042128082, 0.3700002126177032169, 0.4350001063311936811, 0.5000000000446841453, 0.5649998937584436165, 0.6299997874719340807, 0.6949996811854246559, 0.7599995748989150091, 0.8249994686124054732, 0.8899993623258959374, 0.9549992560396556307, 1.000000000000000000 ),
 .UNSPECIFIED. ) ;
#2797 = CARTESIAN_POINT ( 'NONE',  ( 9.328744840303000885, -79.62270543005199386, -2.439838196641999524 ) ) ;
#2798 = AXIS2_PLACEMENT_3D ( 'NONE', #33784, #43246, #16954 ) ;
#2799 = CARTESIAN_POINT ( 'NONE',  ( -12.54715396797999993, -54.26815137240999576, 1.292200816717000045 ) ) ;
#2800 = CARTESIAN_POINT ( 'NONE',  ( -8.874863966699559015, -79.31646010331650132, 3.954991475770741172 ) ) ;
#2801 = CARTESIAN_POINT ( 'NONE',  ( -0.3926218265389190276, -80.10416666666667140, -1.460959015002473826 ) ) ;
#2802 = CARTESIAN_POINT ( 'NONE',  ( -0.8506806241676574398, -3.104166666666666963, -3.165411199172027068 ) ) ;
#2803 = AXIS2_PLACEMENT_3D ( 'NONE', #36723, #54737, #54161 ) ;
#2804 = FACE_OUTER_BOUND ( 'NONE', #5564, .T. ) ;
#2805 = CARTESIAN_POINT ( 'NONE',  ( 1.750000000000000000, -55.55000000209000177, -12.50000000000000000 ) ) ;
#2806 = CARTESIAN_POINT ( 'NONE',  ( -0.9683059680012998660, -77.42495975171298994, -11.01410536002000029 ) ) ;
#2807 = CARTESIAN_POINT ( 'NONE',  ( -0.4507512596549299033, -76.32183930805716443, -11.74168627474140969 ) ) ;
#2808 = CARTESIAN_POINT ( 'NONE',  ( -6.550114462690999950, -76.71554859108100288, -8.876808543633000426 ) ) ;
#2809 = CARTESIAN_POINT ( 'NONE',  ( 6.584508673715998128, -78.46579514476064787, 7.154582167228999090 ) ) ;
#2810 = CARTESIAN_POINT ( 'NONE',  ( 1.357547920874000003, -78.53098293213999170, -0.9615626969474000418 ) ) ;
#2811 = CARTESIAN_POINT ( 'NONE',  ( 10.12290050126000196, -60.04999999958999979, 7.648026767103999646 ) ) ;
#2812 = CARTESIAN_POINT ( 'NONE',  ( -1.500000000000000888, -78.98958333333331439, 0.1963495408493559080 ) ) ;
#2813 = CARTESIAN_POINT ( 'NONE',  ( -9.611650271896857944, -77.55833333333332291, 5.539808784079855997 ) ) ;
#2814 = CARTESIAN_POINT ( 'NONE',  ( 7.627621379903384735, -80.28777230127180076, -7.575081149988561080 ) ) ;
#2815 = CARTESIAN_POINT ( 'NONE',  ( -1.500000000000000000, -80.91769483858634260, -0.3335398494528040159 ) ) ;
#2816 = CARTESIAN_POINT ( 'NONE',  ( -10.41172548051528146, -18.47988211125538527, -7.610718780881579271 ) ) ;
#2817 = CARTESIAN_POINT ( 'NONE',  ( 6.536979956083999177, -79.16903447980999431, -10.09826910480999906 ) ) ;
#2818 = CARTESIAN_POINT ( 'NONE',  ( 0.9995835529977233902, -81.80208333333332860, 0.7681833999686461523 ) ) ;
#2819 = CARTESIAN_POINT ( 'NONE',  ( 10.97564558566000059, -79.09139468996799849, 2.523721168482999655 ) ) ;
#2820 = VERTEX_POINT ( 'NONE', #8379 ) ;
#2821 = CARTESIAN_POINT ( 'NONE',  ( -0.1380878923284744875, -25.22734402323948544, 12.70555840932578384 ) ) ;
#2822 = VERTEX_POINT ( 'NONE', #57977 ) ;
#2823 = ORIENTED_EDGE ( 'NONE', *, *, #41511, .T. ) ;
#2824 = LINE ( 'NONE', #53275, #12192 ) ;
#2825 = LINE ( 'NONE', #43856, #18308 ) ;
#2826 = CARTESIAN_POINT ( 'NONE',  ( -1.280865346364000068, -79.04323530191599900, -3.305193740963000337 ) ) ;
#2827 = CARTESIAN_POINT ( 'NONE',  ( 8.035977331916674515, -79.19462052551928366, 5.075416816263699005 ) ) ;
#2828 = ORIENTED_EDGE ( 'NONE', *, *, #38049, .T. ) ;
#2829 = DIRECTION ( 'NONE',  ( 0.000000000000000000, -1.000000000000000000, 0.000000000000000000 ) ) ;
#2830 = B_SPLINE_CURVE_WITH_KNOTS ( 'NONE', 3,
 ( #21725, #52455, #48325, #29423, #34425, #52174, #43598, #12013 ),
 .UNSPECIFIED., .F., .F.,
 ( 4, 2, 2, 4 ),
 ( 0.000000000000000000, 0.4999999999999971134, 0.7499999999999985567, 1.000000000000000000 ),
 .UNSPECIFIED. ) ;
#2831 = DIRECTION ( 'NONE',  ( 0.000000000000000000, 1.000000000000000000, 0.000000000000000000 ) ) ;
#2832 = VERTEX_POINT ( 'NONE', #26664 ) ;
#2833 = CARTESIAN_POINT ( 'NONE',  ( 1.861192509982939169, -79.69030282387936381, -9.372352437101028499 ) ) ;
#2834 = CARTESIAN_POINT ( 'NONE',  ( -0.2254326743809463296, -78.13651477724624783, 1.514863696781568736 ) ) ;
#2835 = AXIS2_PLACEMENT_3D ( 'NONE', #55220, #42238, #28637 ) ;
#2836 = CARTESIAN_POINT ( 'NONE',  ( 6.200214177871735899, -79.80000000000001137, 10.15137242043624966 ) ) ;
#2837 = CARTESIAN_POINT ( 'NONE',  ( -5.074860051582180454, -80.01429829952145667, 9.477187767418271847 ) ) ;
#2838 = CIRCLE ( 'NONE', #47153, 2.799999999999999822 ) ;
#2839 = CARTESIAN_POINT ( 'NONE',  ( -1.412116703021476960, -86.09999999999996589, -3.092883188393807270 ) ) ;
#2840 = CARTESIAN_POINT ( 'NONE',  ( -1.432420283025999996, -76.28690332460300283, 11.09153081809999897 ) ) ;
#2841 = CARTESIAN_POINT ( 'NONE',  ( -8.707837037439713157, -76.54997136955654469, 6.490898182015857110 ) ) ;
#2842 = EDGE_CURVE ( 'NONE', #11057, #27205, #1887, .T. ) ;
#2843 = CARTESIAN_POINT ( 'NONE',  ( 11.00000000000000000, -78.44999999999998863, 0.000000000000000000 ) ) ;
#2844 = CARTESIAN_POINT ( 'NONE',  ( 10.16646861257000012, -76.10830213011298895, 4.767248372777999954 ) ) ;
#2845 = FACE_OUTER_BOUND ( 'NONE', #49797, .T. ) ;
#2846 = CARTESIAN_POINT ( 'NONE',  ( 7.412894021246999365, -77.70291167140099731, -5.973338413043999928 ) ) ;
#2847 = CARTESIAN_POINT ( 'NONE',  ( -0.4872545538094000261, -79.27334965069501038, -1.241463230931000084 ) ) ;
#2848 = CARTESIAN_POINT ( 'NONE',  ( -10.90550475849158119, -80.11063224077452105, -1.438076737588118048 ) ) ;
#2849 = CARTESIAN_POINT ( 'NONE',  ( 2.187994190098494052, -2.916594878656368461, 2.403360964150264234 ) ) ;
#2850 = CARTESIAN_POINT ( 'NONE',  ( 3.779826922834999881, -82.16928455456799441, 0.3812749626282999627 ) ) ;
#2851 = CARTESIAN_POINT ( 'NONE',  ( -5.997359202501453268, -78.02227085838593723, 8.921436172744598991 ) ) ;
#2852 = CARTESIAN_POINT ( 'NONE',  ( 0.000000000000000000, -79.65000000003199432, 0.000000000000000000 ) ) ;
#2853 = FILL_AREA_STYLE ('',( #43298 ) ) ;
#2854 = CARTESIAN_POINT ( 'NONE',  ( 1.924356497468000082, -85.26849735065199809, -2.976880213510999962 ) ) ;
#2855 = CARTESIAN_POINT ( 'NONE',  ( -9.152251458167393494, -76.25350003968078738, -7.375437608540630130 ) ) ;
#2856 = CARTESIAN_POINT ( 'NONE',  ( 12.50000000000000000, -18.75000000240999753, 1.750000000000000000 ) ) ;
#2857 = CARTESIAN_POINT ( 'NONE',  ( -8.220407391966000787, -61.61950084198999633, -9.523310056136001123 ) ) ;
#2858 = EDGE_CURVE ( 'NONE', #28634, #6364, #35852, .T. ) ;
#2859 = CARTESIAN_POINT ( 'NONE',  ( 6.365665562422999635, -79.13050366622999832, 10.17242851768000023 ) ) ;
#2860 = CARTESIAN_POINT ( 'NONE',  ( 1.310679582531387943, -77.70833333333332860, -0.7554284705563468760 ) ) ;
#2861 = CIRCLE ( 'NONE', #24517, 1.749999999999997113 ) ;
#2862 = CARTESIAN_POINT ( 'NONE',  ( 1.199500263597271577, -80.59791666666667709, -0.9218200799623702535 ) ) ;
#2864 = CARTESIAN_POINT ( 'NONE',  ( 5.512103878356000131, -76.85752566061000834, 11.78783395355999986 ) ) ;
#2863 = B_SPLINE_CURVE_WITH_KNOTS ( 'NONE', 3,
 ( #16101, #25813, #3388, #43257, #8100, #38525, #21099, #56540, #29937, #16962, #34944, #43841 ),
 .UNSPECIFIED., .F., .F.,
 ( 4, 2, 2, 2, 2, 4 ),
 ( 0.000000000000000000, 0.1250000000000000000, 0.2500000000000000000, 0.5000000000000000000, 0.7500000000000000000, 1.000000000000000000 ),
 .UNSPECIFIED. ) ;
#2865 = CARTESIAN_POINT ( 'NONE',  ( 1.750000000001000089, -18.75000001325000198, 12.56594318051000059 ) ) ;
#2866 = DIRECTION ( 'NONE',  ( 0.000000000000000000, 1.000000000000000000, 0.000000000000000000 ) ) ;
#2867 = CARTESIAN_POINT ( 'NONE',  ( 10.98849124983000003, -76.88653068653000844, -4.660349322786999871 ) ) ;
#2868 = ORIENTED_EDGE ( 'NONE', *, *, #53910, .F. ) ;
#2869 = CARTESIAN_POINT ( 'NONE',  ( -6.711381441964999972, -80.17578567971679604, 9.048015653393999713 ) ) ;
#2870 = CARTESIAN_POINT ( 'NONE',  ( 3.106054555984999688, -86.09999999999999432, -1.382904586457999851 ) ) ;
#2871 = CARTESIAN_POINT ( 'NONE',  ( -1.034297989014000052, -81.18931145362199686, 0.8050146651342000581 ) ) ;
#2872 = CARTESIAN_POINT ( 'NONE',  ( -3.310367643023999662, -78.77244978676999665, -12.19650721378999947 ) ) ;
#2873 = DIRECTION ( 'NONE',  ( 0.000000000000000000, -1.000000000000000000, 0.000000000000000000 ) ) ;
#2874 = CARTESIAN_POINT ( 'NONE',  ( 8.381176496771999496, -78.18405256877699117, 4.744374615790000860 ) ) ;
#2875 = CARTESIAN_POINT ( 'NONE',  ( -4.136973154815000164, -84.74982851107797899, -0.5403780116516999632 ) ) ;
#2876 = DIRECTION ( 'NONE',  ( 0.000000000000000000, -1.000000000000000000, 0.000000000000000000 ) ) ;
#2877 = DIRECTION ( 'NONE',  ( -0.7071067811865475727, 0.000000000000000000, -0.7071067811865475727 ) ) ;
#2878 = EDGE_CURVE ( 'NONE', #28730, #12876, #9840, .T. ) ;
#2879 = VERTEX_POINT ( 'NONE', #42317 ) ;
#2880 = DIRECTION ( 'NONE',  ( 4.860620543616000107E-11, -1.000000000000000000, 3.762834028070999803E-10 ) ) ;
#2881 = CARTESIAN_POINT ( 'NONE',  ( -1.026216979225322623, -82.21744791666523611, 0.7875855714864156143 ) ) ;
#2882 = AXIS2_PLACEMENT_3D ( 'NONE', #53196, #12740, #12457 ) ;
#2883 = CARTESIAN_POINT ( 'NONE',  ( 2.936298172289618869, -78.99844905003692475, -2.194537220288346191 ) ) ;
#2884 = ORIENTED_EDGE ( 'NONE', *, *, #49299, .T. ) ;
#2885 = CARTESIAN_POINT ( 'NONE',  ( 9.274475910318999539, -79.07632342844499362, -5.802750462065000114 ) ) ;
#2886 = CARTESIAN_POINT ( 'NONE',  ( 12.58338334673999981, -57.05199022587000002, 1.667961445601999992 ) ) ;
#2887 = CARTESIAN_POINT ( 'NONE',  ( -10.56934456194000127, -80.33626512904898220, -4.081628045126000082 ) ) ;
#2888 = ORIENTED_EDGE ( 'NONE', *, *, #53523, .F. ) ;
#2889 = ORIENTED_EDGE ( 'NONE', *, *, #50634, .F. ) ;
#2890 = VERTEX_POINT ( 'NONE', #1885 ) ;
#2891 = CARTESIAN_POINT ( 'NONE',  ( -0.01891664938484899361, -80.47679111333721380, 1.249509389969930773 ) ) ;
#2892 = CARTESIAN_POINT ( 'NONE',  ( -1.250000000000000000, -67.52659999995799467, 0.000000000000000000 ) ) ;
#2893 = CARTESIAN_POINT ( 'NONE',  ( -9.699833017908000343, -79.62079945152900962, 1.146274062705999963 ) ) ;
#2894 = ORIENTED_EDGE ( 'NONE', *, *, #30754, .T. ) ;
#2895 = VECTOR ( 'NONE', #57044, 1000.000000000000000 ) ;
#2896 = ORIENTED_EDGE ( 'NONE', *, *, #26131, .T. ) ;
#2897 = CARTESIAN_POINT ( 'NONE',  ( 6.688645397968000950, -78.87909499590685414, 10.27915892414000076 ) ) ;
#2898 = CARTESIAN_POINT ( 'NONE',  ( -2.218416052576314801, -79.00321104920828930, -3.679255452198593179 ) ) ;
#2899 = CARTESIAN_POINT ( 'NONE',  ( 9.523369619434999933, -53.98054357652999613, 8.220347091585999522 ) ) ;
#2900 = CARTESIAN_POINT ( 'NONE',  ( 7.712209501881797102, -17.93822238229371635, -10.27335463211299960 ) ) ;
#2901 = FACE_OUTER_BOUND ( 'NONE', #7102, .T. ) ;
#2902 = CARTESIAN_POINT ( 'NONE',  ( -4.000000000000000000, -78.69999999915415856, 2.834003763004000336E-08 ) ) ;
#2903 = EDGE_CURVE ( 'NONE', #17089, #55354, #15444, .T. ) ;
#2904 = CARTESIAN_POINT ( 'NONE',  ( -11.19161167724979222, -80.34518168142261629, 0.6576043368013242407 ) ) ;
#2905 = CARTESIAN_POINT ( 'NONE',  ( -6.777984382448001277, -78.22714382231113461, -9.878005474088999094 ) ) ;
#2906 = FACE_OUTER_BOUND ( 'NONE', #17702, .T. ) ;
#2907 = EDGE_CURVE ( 'NONE', #54376, #12596, #51474, .T. ) ;
#2908 = CARTESIAN_POINT ( 'NONE',  ( -6.024415200221000077, -76.36369539903000714, 10.73507988388000101 ) ) ;
#2909 = VECTOR ( 'NONE', #648, 1000.000000000000227 ) ;
#2910 = CARTESIAN_POINT ( 'NONE',  ( -9.003040227835604981, -79.32727112472369413, -3.132519729896531935 ) ) ;
#2911 = VECTOR ( 'NONE', #51281, 1000.000000000000000 ) ;
#2912 = CARTESIAN_POINT ( 'NONE',  ( 2.166634614239063377E-07, -77.01246206852036380, -9.437473063691797392 ) ) ;
#2913 = DIRECTION ( 'NONE',  ( -0.7272727272724163194, -0.6863485850246158204, -6.703676216865156901E-07 ) ) ;
#2914 = CARTESIAN_POINT ( 'NONE',  ( 3.086017585447000222, -79.12790895394999779, -11.86910201801999953 ) ) ;
#2915 = CARTESIAN_POINT ( 'NONE',  ( 4.297951556683999641, -76.65176905123000495, -11.50435740523999861 ) ) ;
#2916 = CARTESIAN_POINT ( 'NONE',  ( -7.596835002782739821, -78.84791666666669130, 5.838193839761659731 ) ) ;
#2917 = CARTESIAN_POINT ( 'NONE',  ( 12.00000000000000000, -55.54999999966999980, 0.000000000000000000 ) ) ;
#2918 = EDGE_CURVE ( 'NONE', #44143, #27639, #11924, .T. ) ;
#2919 = CARTESIAN_POINT ( 'NONE',  ( 0.8074256036998892494, -79.91997086998991051, -1.276157013251583150 ) ) ;
#2920 = CARTESIAN_POINT ( 'NONE',  ( 5.114889623276000385, -77.12723231992129058, -7.994241842339000037 ) ) ;
#2921 = DIRECTION ( 'NONE',  ( 0.000000000000000000, 0.000000000000000000, -1.000000000000000000 ) ) ;
#2922 = CARTESIAN_POINT ( 'NONE',  ( 8.012523733906446566, -78.71708638852500428, 8.990154430766319038 ) ) ;
#2923 = CARTESIAN_POINT ( 'NONE',  ( -3.258626092852999534, -3.578756257025999865, -0.9749691283561999766 ) ) ;
#2924 = CARTESIAN_POINT ( 'NONE',  ( 6.129172116842999785, -77.77411607459599452, 10.50789130831999962 ) ) ;
#2925 = CARTESIAN_POINT ( 'NONE',  ( -1.966850719965000494, -77.37963215124798921, -9.538930191946999315 ) ) ;
#2927 = CARTESIAN_POINT ( 'NONE',  ( -7.648026768024999811, -18.75000001589999954, 10.12290050218000026 ) ) ;
#2926 = DIRECTION ( 'NONE',  ( 0.7071067811865475727, 0.000000000000000000, 0.7071067811865475727 ) ) ;
#2928 = CARTESIAN_POINT ( 'NONE',  ( 1.420454834158999979, -81.41375084182999444, 0.3724989704330000095 ) ) ;
#2929 = FACE_OUTER_BOUND ( 'NONE', #54276, .T. ) ;
#2930 = ORIENTED_EDGE ( 'NONE', *, *, #10786, .F. ) ;
#2931 = CARTESIAN_POINT ( 'NONE',  ( -10.35845616727999996, -23.29778595484999926, -7.627487606609999915 ) ) ;
#2932 = CARTESIAN_POINT ( 'NONE',  ( -6.394435847298999498, -79.27158651582300308, -10.20310948103000115 ) ) ;
#2933 = CARTESIAN_POINT ( 'NONE',  ( -0.7090885217563500653, -79.13093592298157830, 9.493073439722991225 ) ) ;
#2934 = B_SPLINE_CURVE_WITH_KNOTS ( 'NONE', 3,
 ( #13704, #26114, #3969, #35246 ),
 .UNSPECIFIED., .F., .F.,
 ( 4, 4 ),
 ( 0.000000000000000000, 1.000000000000000000 ),
 .UNSPECIFIED. ) ;
#2935 = CIRCLE ( 'NONE', #28370, 12.50000000000000000 ) ;
#2936 = CARTESIAN_POINT ( 'NONE',  ( -4.889775958634938746, -79.99999999999998579, -8.013494230838169585 ) ) ;
#2937 = CARTESIAN_POINT ( 'NONE',  ( -8.652376385632999600, -62.06264602932999708, 9.414489258850998965 ) ) ;
#2938 = CARTESIAN_POINT ( 'NONE',  ( -3.395341895239999630, -1.598905165122000094, 1.471171784242000014 ) ) ;
#2939 = CARTESIAN_POINT ( 'NONE',  ( -4.561872603918999403, -79.85766786116599292, -8.776383598921000839 ) ) ;
#2940 = DIRECTION ( 'NONE',  ( 0.000000000000000000, 1.000000000000000000, 0.000000000000000000 ) ) ;
#2941 = CARTESIAN_POINT ( 'NONE',  ( -9.611650271896833075, -78.64166666666667993, -5.539808784079895077 ) ) ;
#2942 = ORIENTED_EDGE ( 'NONE', *, *, #37152, .F. ) ;
#2943 = CARTESIAN_POINT ( 'NONE',  ( -5.279640230871068596, -76.43576352588647183, -9.859185912017370157 ) ) ;
#2944 = CARTESIAN_POINT ( 'NONE',  ( 8.047230821198958495, -79.23460565973853420, -8.591241732543773324 ) ) ;
#2945 = CARTESIAN_POINT ( 'NONE',  ( -3.012268937172999816, -79.85615333806700278, -9.005103130722002192 ) ) ;
#2946 = CARTESIAN_POINT ( 'NONE',  ( -10.59551070212999946, -58.55648180022999583, -7.678690995210999404 ) ) ;
#2947 = CARTESIAN_POINT ( 'NONE',  ( -0.8033051684372000123, -80.41456746453999926, -1.459438184619000101 ) ) ;
#2948 = ORIENTED_EDGE ( 'NONE', *, *, #19155, .T. ) ;
#2949 = CARTESIAN_POINT ( 'NONE',  ( -12.50679926046298363, -54.49581646307559879, 1.424414840068720212 ) ) ;
#2950 = VECTOR ( 'NONE', #33858, 1000.000000000000000 ) ;
#2951 = CARTESIAN_POINT ( 'NONE',  ( -0.6299849389810197042, -82.18398283962009998, -1.093434970869878287 ) ) ;
#2952 = CARTESIAN_POINT ( 'NONE',  ( 1.931043742978000077, -56.02204592290999585, -12.75763395696999858 ) ) ;
#2953 = EDGE_CURVE ( 'NONE', #7307, #45201, #24594, .T. ) ;
#2954 = CIRCLE ( 'NONE', #39731, 0.5000000000000004441 ) ;
#2955 = CARTESIAN_POINT ( 'NONE',  ( -12.83044027758000105, -55.49360215019999742, 2.062670899361999766 ) ) ;
#2956 = B_SPLINE_SURFACE_WITH_KNOTS ( 'NONE', 3, 3, ( 
 ( #9575, #13105, #44411, #53271, #457, #49137, #27559, #44712, #22261, #27271, #12819, #745, #40276, #58287, #4858, #3964, #40866, #45308, #18143, #54454, #13990, #36139, #35239, #54156, #31400, #17850, #22855, #36428, #30817, #35838, #23145, #53866, #48850, #8394, #26390 ),
 ( #21966, #8991, #22564, #169, #13698, #31692, #33151, #36719, #24606, #14570, #32563, #46779, #27849, #24316, #51196, #1600, #37884, #55906, #19592, #42618, #37591, #14859, #19014, #10751, #28727, #18725, #50612, #6303, #23436, #42331, #1899, #19891, #10161, #14276, #15460 ),
 ( #29027, #33449, #55314, #50319, #23724, #45894, #47066, #54733, #51487, #55609, #11045, #15157, #6595, #32274, #28138, #32854, #9868, #41448, #5426, #1032, #6008, #42032, #37007, #55024, #46482, #24015, #46192, #5716, #41736, #1315, #19309, #10449, #37298, #50901, #28434 ),
 ( #31604, #22470, #27764, #40482, #45807, #77, #9192, #14484, #31897, #4763, #944, #18926, #9486, #50520, #10073, #46102, #51397, #20664, #24224, #7088, #32768, #50815, #20379, #33934, #10952, #38086, #28342, #28933, #10358, #46393, #41943, #47266, #24514, #15067, #20097 ) ),
 .UNSPECIFIED., .F., .F., .F.,
 ( 4, 4 ),
 ( 4, 1, 1, 1, 1, 1, 1, 1, 1, 1, 1, 1, 1, 1, 1, 1, 1, 1, 1, 1, 1, 1, 1, 1, 1, 1, 1, 1, 1, 1, 1, 1, 4 ),
 ( -0.05371687727927999811, 1.053716877278999986 ),
 ( -0.02000000000000000042, 0.01250000000000000069, 0.04499999999999999833, 0.07749999999999999944, 0.1100000000000000006, 0.1424999999999999878, 0.1749999999999999889, 0.2074999999999999900, 0.2399999999999999911, 0.2725000000000000200, 0.3049999999999999933, 0.3375000000000000222, 0.3699999999999999956, 0.4025000000000000244, 0.4349999999999999978, 0.4675000000000000266, 0.5000000000000000000, 0.5324999999999999734, 0.5649999999999999467, 0.5975000000000000311, 0.6300000000000000044, 0.6624999999999999778, 0.6949999999999999512, 0.7275000000000000355, 0.7600000000000000089, 0.7924999999999999822, 0.8249999999999999556, 0.8575000000000000400, 0.8900000000000000133, 0.9224999999999999867, 0.9549999999999999600, 0.9875000000000000444, 1.020000000000000018 ),
 .UNSPECIFIED. ) ;
#2957 = CARTESIAN_POINT ( 'NONE',  ( 0.000000000000000000, -79.79999999999999716, 0.000000000000000000 ) ) ;
#2958 = CARTESIAN_POINT ( 'NONE',  ( -8.448510849392999233, -79.16771232935798253, 4.901364000006999788 ) ) ;
#2959 = ORIENTED_EDGE ( 'NONE', *, *, #5783, .F. ) ;
#2960 = VERTEX_POINT ( 'NONE', #5994 ) ;
#2961 = CARTESIAN_POINT ( 'NONE',  ( 5.596253190686999446, -76.48824961810498735, -11.27629867687000065 ) ) ;
#2962 = CARTESIAN_POINT ( 'NONE',  ( 4.129401235074444010, -78.75639348479435853, -9.925231067652177330 ) ) ;
#2963 = EDGE_LOOP ( 'NONE', ( #1974, #5440, #29962, #48704, #22807 ) ) ;
#2964 = CARTESIAN_POINT ( 'NONE',  ( 9.422860735135998311, -16.74048607655000254, 8.643926020477998406 ) ) ;
#2965 = DIRECTION ( 'NONE',  ( 9.386928511358000402E-11, -1.000000000000000000, -5.363054260619999949E-10 ) ) ;
#2966 = CARTESIAN_POINT ( 'NONE',  ( -0.9935076048178934638, -53.83183812217039588, 12.70250268212202371 ) ) ;
#2967 = CARTESIAN_POINT ( 'NONE',  ( -3.331828115504000376, -76.97715654337000046, 12.52045872913000046 ) ) ;
#2968 = CARTESIAN_POINT ( 'NONE',  ( 0.000000000000000000, -74.70999999999999375, 0.000000000000000000 ) ) ;
#2969 = FACE_OUTER_BOUND ( 'NONE', #53859, .T. ) ;
#2970 = B_SPLINE_CURVE_WITH_KNOTS ( 'NONE', 3,
 ( #52532, #3518, #43682, #44839, #21228, #52819, #16522, #53696, #39233, #12937, #39524, #17379, #35665, #8820, #30935, #13234 ),
 .UNSPECIFIED., .F., .F.,
 ( 4, 2, 2, 2, 2, 2, 2, 4 ),
 ( 0.000000000000000000, 0.2500000000000003886, 0.3750000000000005551, 0.5000000000000007772, 0.6250000000000009992, 0.6875000000000039968, 0.7500000000000069944, 1.000000000000000000 ),
 .UNSPECIFIED. ) ;
#2971 = CARTESIAN_POINT ( 'NONE',  ( 1.353569424327119686, -86.09999999999998010, 3.118950113985159867 ) ) ;
#2972 = CARTESIAN_POINT ( 'NONE',  ( -6.206245474241999460, -79.75555179526899963, 9.343480492029000217 ) ) ;
#2973 = CARTESIAN_POINT ( 'NONE',  ( -1.180921238786448946, -79.98531230651158808, 9.176345860435365154 ) ) ;
#2974 = ORIENTED_EDGE ( 'NONE', *, *, #24005, .F. ) ;
#2975 = CARTESIAN_POINT ( 'NONE',  ( 7.836763323982919083, -54.49488832206740341, -9.850488778787754640 ) ) ;
#2976 = MECHANICAL_DESIGN_GEOMETRIC_PRESENTATION_REPRESENTATION (  '', ( #53896 ), #30306 ) ;
#2977 = ORIENTED_EDGE ( 'NONE', *, *, #21236, .F. ) ;
#2978 = CARTESIAN_POINT ( 'NONE',  ( 10.99934742197999960, -79.88817051509798262, 2.437886521773999782 ) ) ;
#2979 = ADVANCED_FACE ( 'NONE', ( #42608, #27837 ), #24000, .F. ) ;
#2980 = CARTESIAN_POINT ( 'NONE',  ( 7.560074365901553683, -77.30122887067066983, -5.329858952455061250 ) ) ;
#2981 = CARTESIAN_POINT ( 'NONE',  ( -0.6438247211726000341, -80.38480328324099844, -1.263150469460000203 ) ) ;
#2982 = CARTESIAN_POINT ( 'NONE',  ( -9.722718241315000398, -55.54999999966999980, 7.247844507162001015 ) ) ;
#2983 = CARTESIAN_POINT ( 'NONE',  ( -14.00000000000000000, -80.70000000000000284, 0.000000000000000000 ) ) ;
#2984 = CARTESIAN_POINT ( 'NONE',  ( -1.071041487988000140, -79.10438725917299507, -0.9340865940840999970 ) ) ;
#2985 = DIRECTION ( 'NONE',  ( 0.000000000000000000, -1.000000000000000000, 0.000000000000000000 ) ) ;
#2986 = DIRECTION ( 'NONE',  ( 0.000000000000000000, 1.000000000000000000, 0.000000000000000000 ) ) ;
#2987 = DIRECTION ( 'NONE',  ( 1.000000000000000000, 0.000000000000000000, 0.000000000000000000 ) ) ;
#2988 = DIRECTION ( 'NONE',  ( 1.000000000000000000, 0.000000000000000000, 2.719057617949999588E-13 ) ) ;
#2989 = CARTESIAN_POINT ( 'NONE',  ( -7.654537165468999760, -23.28056535155999995, 10.01332852689000141 ) ) ;
#2990 = CARTESIAN_POINT ( 'NONE',  ( -10.61618518222999796, -78.53204647501199531, 3.433396544298999764 ) ) ;
#2991 = CARTESIAN_POINT ( 'NONE',  ( 9.500000000000000000, -91.89999999999999147, 0.000000000000000000 ) ) ;
#2992 = CARTESIAN_POINT ( 'NONE',  ( -1.417334032777999964, -79.42654225787899236, -0.4910847579886000736 ) ) ;
#2993 = DIRECTION ( 'NONE',  ( 0.000000000000000000, 1.000000000000000000, 0.000000000000000000 ) ) ;
#2994 = EDGE_CURVE ( 'NONE', #3745, #31953, #5640, .T. ) ;
#2995 = DIRECTION ( 'NONE',  ( 0.000000000000000000, -1.000000000000000000, 0.000000000000000000 ) ) ;
#2996 = EDGE_LOOP ( 'NONE', ( #7749, #43806, #51269, #17557 ) ) ;
#2997 = CARTESIAN_POINT ( 'NONE',  ( -1.544355253863999966, -83.34783910444198796, -0.3612495668209000366 ) ) ;
#2998 = VECTOR ( 'NONE', #29245, 1000.000000000000000 ) ;
#2999 = CARTESIAN_POINT ( 'NONE',  ( 1.446151133417000079, -79.72054785055999560, 0.2550274018384999786 ) ) ;
#3000 = CARTESIAN_POINT ( 'NONE',  ( -11.70000000000000107, -80.79999999999999716, 0.000000000000000000 ) ) ;
#3001 = EDGE_CURVE ( 'NONE', #43048, #19498, #15143, .T. ) ;
#3002 = CARTESIAN_POINT ( 'NONE',  ( -5.687706977064000746, -77.98047327643499216, 10.54353137130999940 ) ) ;
#3003 = CARTESIAN_POINT ( 'NONE',  ( -12.71758670598746122, -17.93493368773759400, 1.809547514117124667 ) ) ;
#3004 = CARTESIAN_POINT ( 'NONE',  ( 0.3719284678543265388, -79.10182967317921054, 1.219176263759028878 ) ) ;
#3005 = CARTESIAN_POINT ( 'NONE',  ( -0.5480261397617977037, -1.862545821266776924, -3.476873622539977671 ) ) ;
#3006 = CARTESIAN_POINT ( 'NONE',  ( -7.530775182571000315, -78.18455194988499102, -6.150709233331999037 ) ) ;
#3007 = CARTESIAN_POINT ( 'NONE',  ( 9.412698430168999764, -77.33012407454400261, 0.1109178415545999941 ) ) ;
#3008 = CARTESIAN_POINT ( 'NONE',  ( -0.2863152943028942077, -81.20653045236295497, -1.221378511987871951 ) ) ;
#3009 = CARTESIAN_POINT ( 'NONE',  ( -6.481772035086000194, -77.10100271990599197, -8.784189910979000260 ) ) ;
#3010 = DIRECTION ( 'NONE',  ( 0.000000000000000000, 1.000000000000000000, 0.000000000000000000 ) ) ;
#3011 = CARTESIAN_POINT ( 'NONE',  ( 0.7671735781280533129, -80.97340970725861098, 1.017801935282923287 ) ) ;
#3012 = VERTEX_POINT ( 'NONE', #46175 ) ;
#3013 = DIRECTION ( 'NONE',  ( 0.000000000000000000, -1.000000000000000000, 0.000000000000000000 ) ) ;
#3014 = DIRECTION ( 'NONE',  ( 0.000000000000000000, -1.000000000000000000, 0.000000000000000000 ) ) ;
#3015 = CARTESIAN_POINT ( 'NONE',  ( -7.421735313277000756, -79.75327784566698597, 9.772525563196001741 ) ) ;
#3016 = CARTESIAN_POINT ( 'NONE',  ( 12.00000000000000000, -77.04999999999999716, 0.000000000000000000 ) ) ;
#3017 = CARTESIAN_POINT ( 'NONE',  ( -10.57157196544999955, -79.85258015763899664, 2.324769239444999691 ) ) ;
#3018 = CARTESIAN_POINT ( 'NONE',  ( 12.00000000000000000, -18.75000000000000000, 0.000000000000000000 ) ) ;
#3019 = CARTESIAN_POINT ( 'NONE',  ( -1.980611416588530682, -18.47402268192283259, 12.74335092662909297 ) ) ;
#3020 = CARTESIAN_POINT ( 'NONE',  ( 11.82336703301000114, -76.80802521606899802, -2.809544199102999684 ) ) ;
#3021 = CARTESIAN_POINT ( 'NONE',  ( 3.202676180380386928, -78.55085330470771510, 11.30378351636584533 ) ) ;
#3022 = CARTESIAN_POINT ( 'NONE',  ( 9.369164850722000892, -23.25000000000000000, -7.601397897754999633 ) ) ;
#3023 = ORIENTED_EDGE ( 'NONE', *, *, #17197, .T. ) ;
#3024 = CARTESIAN_POINT ( 'NONE',  ( 7.679819846117000637, -78.82741272537499810, -7.919728626202000576 ) ) ;
#3025 = CARTESIAN_POINT ( 'NONE',  ( -1.190683053189752982, -80.07578141901581148, 0.3803500925840294089 ) ) ;
#3026 = EDGE_CURVE ( 'NONE', #8229, #8361, #4019, .T. ) ;
#3027 = CARTESIAN_POINT ( 'NONE',  ( 10.42531124905999995, -18.73514851523999880, -7.624341765453999997 ) ) ;
#3028 = B_SPLINE_CURVE_WITH_KNOTS ( 'NONE', 3,
 ( #36962, #32810, #19545, #32517, #55560, #1851, #2138, #50561, #55859, #10402, #51442, #15109, #33105, #51149, #10704, #28681, #15411, #6252, #10994, #28977, #47019, #38419, #38709, #17141, #29836, #7130, #56438, #16861, #11859, #25131, #39576, #21280, #7993, #34268, #47606, #57299, #34842, #56729, #11571, #57579, #7419, #15992, #47308, #52872, #29551, #25991 ),
 .UNSPECIFIED., .F., .F.,
 ( 4, 1, 1, 1, 1, 1, 2, 2, 1, 1, 1, 1, 1, 1, 2, 2, 1, 1, 1, 1, 2, 2, 1, 2, 2, 2, 2, 2, 2, 2, 4 ),
 ( 0.000000000000000000, 0.06249999999999175659, 0.09374999999998766265, 0.1093749999999855810, 0.1171874999999845679, 0.1210937499999840405, 0.1230468749999838324, 0.1249999999999835965, 0.1874999999999750477, 0.2187499999999706901, 0.2343749999999685807, 0.2421874999999675815, 0.2460937499999671374, 0.2480468749999668876, 0.2490234374999668598, 0.2499999999999668043, 0.3124999999999651945, 0.3437499999999644729, 0.3593749999999639733, 0.3671874999999638067, 0.3710937499999638067, 0.3749999999999638622, 0.4374999999999673594, 0.4687499999999691913, 0.4999999999999710232, 0.6249999999999783507, 0.6874999999999820144, 0.7499999999999856781, 0.8124999999999893419, 0.8749999999999928946, 1.000000000000000000 ),
 .UNSPECIFIED. ) ;
#3029 = CARTESIAN_POINT ( 'NONE',  ( -11.19646453606000058, -78.68804972576597834, -1.252244488204000028 ) ) ;
#3030 = FACE_OUTER_BOUND ( 'NONE', #39334, .T. ) ;
#3031 = CARTESIAN_POINT ( 'NONE',  ( 12.00000000000000888, -79.53958333333332575, -1.570796326794872577 ) ) ;
#3032 = DIRECTION ( 'NONE',  ( 1.000000000000000000, 0.000000000000000000, 0.000000000000000000 ) ) ;
#3033 = CARTESIAN_POINT ( 'NONE',  ( 1.270967135966797112, -82.05378250061171741, -0.8204115018237847501 ) ) ;
#3034 = CARTESIAN_POINT ( 'NONE',  ( 0.4820167300484242690, -79.75682355617291819, -1.153123235814610181 ) ) ;
#3035 = ADVANCED_FACE ( 'NONE', ( #38742 ), #27342, .F. ) ;
#3036 = VERTEX_POINT ( 'NONE', #39321 ) ;
#3037 = CYLINDRICAL_SURFACE ( 'NONE', #46262, 10.75000000000000000 ) ;
#3038 = EDGE_CURVE ( 'NONE', #22499, #1747, #34876, .T. ) ;
#3039 = LINE ( 'NONE', #30166, #27305 ) ;
#3040 = FILL_AREA_STYLE_COLOUR ( '', #28459 ) ;
#3041 = CARTESIAN_POINT ( 'NONE',  ( -12.72554383680000001, -23.20159311629000243, 1.930239506950999884 ) ) ;
#3042 = ORIENTED_EDGE ( 'NONE', *, *, #46991, .F. ) ;
#3043 = VERTEX_POINT ( 'NONE', #25454 ) ;
#3044 = CARTESIAN_POINT ( 'NONE',  ( -12.82202470518000048, -55.37373556845999900, -2.066041976111999467 ) ) ;
#3045 = CIRCLE ( 'NONE', #31280, 13.89999999999999858 ) ;
#3046 = ORIENTED_EDGE ( 'NONE', *, *, #17079, .F. ) ;
#3047 = EDGE_LOOP ( 'NONE', ( #11821, #26978, #6807, #19530, #9731, #11234 ) ) ;
#3048 = CARTESIAN_POINT ( 'NONE',  ( 3.399186938124000079, -81.00000000000000000, -10.46162167925000119 ) ) ;
#3049 = CARTESIAN_POINT ( 'NONE',  ( -3.535896000267000350, -76.97465764268899591, 10.32825277893000226 ) ) ;
#3050 = SHAPE_DEFINITION_REPRESENTATION ( #24909, #33899 ) ;
#3051 = CARTESIAN_POINT ( 'NONE',  ( -7.459109567305000077, -79.24926332859899958, -6.354485205484000865 ) ) ;
#3052 = AXIS2_PLACEMENT_3D ( 'NONE', #44830, #36259, #26502 ) ;
#3053 = CARTESIAN_POINT ( 'NONE',  ( 8.554126827399000987, -79.89233811873450009, -7.255689219360999864 ) ) ;
#3054 = ORIENTED_EDGE ( 'NONE', *, *, #21803, .T. ) ;
#3055 = VERTEX_POINT ( 'NONE', #8024 ) ;
#3056 = B_SPLINE_CURVE_WITH_KNOTS ( 'NONE', 3,
 ( #4437, #26856, #4142, #26556, #35410, #8864, #36816, #27948, #50417, #40149, #16857, #21847, #58161, #35122, #57294, #17727, #54834, #35715 ),
 .UNSPECIFIED., .F., .F.,
 ( 4, 2, 2, 2, 2, 2, 2, 2, 4 ),
 ( 0.000000000000000000, 0.1250000000000000000, 0.2499999999999999722, 0.3750000000000000000, 0.5000000000000000000, 0.6250000000000000000, 0.7500000000000000000, 0.8750000000000000000, 1.000000000000000000 ),
 .UNSPECIFIED. ) ;
#3057 = CARTESIAN_POINT ( 'NONE',  ( -6.737926365805661177, -77.54008088401030818, 6.337568593985769994 ) ) ;
#3058 = CARTESIAN_POINT ( 'NONE',  ( 1.160587285869999929, -77.67616457946799358, 10.97894289003999901 ) ) ;
#3059 = CARTESIAN_POINT ( 'NONE',  ( -12.77302471396000172, -61.52230123271999673, -1.481949986260999941 ) ) ;
#3060 = CARTESIAN_POINT ( 'NONE',  ( -9.139898499914998808, -77.24602254130299173, 2.826942883852999966 ) ) ;
#3061 = CARTESIAN_POINT ( 'NONE',  ( -1.000000000000000000, -81.19999999999998863, -7.000000000000000000 ) ) ;
#3062 = CARTESIAN_POINT ( 'NONE',  ( 9.073558136327573465, -62.02808769462804861, 8.894842552356555743 ) ) ;
#3063 = CARTESIAN_POINT ( 'NONE',  ( 1.750000000001000089, -23.25000000990999993, 12.56594317857000043 ) ) ;
#3064 = CARTESIAN_POINT ( 'NONE',  ( -8.254612054926999676, -79.87482240675299749, 6.886499823760000361 ) ) ;
#3065 = CARTESIAN_POINT ( 'NONE',  ( 1.291435174072999903, -79.40738863544999049, -0.9202965842325999679 ) ) ;
#3066 = CARTESIAN_POINT ( 'NONE',  ( -0.5959590523698999887, -82.22858541388899312, -1.119253685964999967 ) ) ;
#3067 = EDGE_CURVE ( 'NONE', #31891, #15380, #15330, .T. ) ;
#3068 = ORIENTED_EDGE ( 'NONE', *, *, #54755, .F. ) ;
#3069 = CARTESIAN_POINT ( 'NONE',  ( -7.981651535783000462, -54.08135615453999634, 10.08154952393999970 ) ) ;
#3071 = EDGE_CURVE ( 'NONE', #23838, #21348, #26020, .T. ) ;
#3070 = CARTESIAN_POINT ( 'NONE',  ( -9.706274203897999442, -78.01783667140099965, -1.344096209030999800 ) ) ;
#3072 = CARTESIAN_POINT ( 'NONE',  ( 8.770451247185000909, -79.01131779197200444, 8.160602927202999624 ) ) ;
#3073 = CARTESIAN_POINT ( 'NONE',  ( -10.47840693002000023, -18.21310507181999938, -7.622759963130000038 ) ) ;
#3075 = CARTESIAN_POINT ( 'NONE',  ( -7.958776490640000034, -61.27699850015999772, 9.723157983991999487 ) ) ;
#3074 = CARTESIAN_POINT ( 'NONE',  ( 7.654537085048000122, -60.08056692637000396, 10.01332844639000008 ) ) ;
#3076 = CARTESIAN_POINT ( 'NONE',  ( 4.784380313523556083, -78.96666666666669698, -8.300970689365444244 ) ) ;
#3077 = CARTESIAN_POINT ( 'NONE',  ( 5.389383425300000141, -80.26373015146698719, 9.671489469558000707 ) ) ;
#3078 = CARTESIAN_POINT ( 'NONE',  ( 0.000000000000000000, -76.00000000000000000, -11.04999999999995275 ) ) ;
#3079 = CARTESIAN_POINT ( 'NONE',  ( -0.8287201338969000242, -77.44254838670400432, -11.23152649900999833 ) ) ;
#3080 = CARTESIAN_POINT ( 'NONE',  ( 2.391208922872818832, -3.499999999999999556, 2.442030068879051719 ) ) ;
#3081 = CARTESIAN_POINT ( 'NONE',  ( -0.5774875637779700588, -1.362040185579431295, -3.482711565813724874 ) ) ;
#3082 = EDGE_LOOP ( 'NONE', ( #19165, #46778, #46668, #48073, #384 ) ) ;
#3083 = CARTESIAN_POINT ( 'NONE',  ( 0.000000000000000000, -87.29999999999999716, 0.000000000000000000 ) ) ;
#3084 = CARTESIAN_POINT ( 'NONE',  ( 0.000000000000000000, -0.2000000000000000111, 0.000000000000000000 ) ) ;
#3085 = CARTESIAN_POINT ( 'NONE',  ( -12.53239398062000198, -19.23513569609999863, 1.667936688463999895 ) ) ;
#3086 = CARTESIAN_POINT ( 'NONE',  ( -3.006336704280999861, -1.519671397434999793, 0.9646084678590001182 ) ) ;
#3087 = CARTESIAN_POINT ( 'NONE',  ( 9.002331482469001500, -79.25367172123299042, -1.969766031707999909 ) ) ;
#3088 = AXIS2_PLACEMENT_3D ( 'NONE', #8858, #40447, #22134 ) ;
#3089 = CARTESIAN_POINT ( 'NONE',  ( -12.49837451343999994, -55.59042109264999709, 1.667049596277000001 ) ) ;
#3090 = CARTESIAN_POINT ( 'NONE',  ( 0.1963495408493638184, -80.13541666666668561, -1.499999999999999778 ) ) ;
#3091 = DIRECTION ( 'NONE',  ( 0.000000000000000000, 1.000000000000000000, 0.000000000000000000 ) ) ;
#3092 = EDGE_CURVE ( 'NONE', #26509, #39544, #52050, .T. ) ;
#3093 = CARTESIAN_POINT ( 'NONE',  ( 11.79999999988000070, -18.85000000520999919, 0.5999999998848000171 ) ) ;
#3094 = CARTESIAN_POINT ( 'NONE',  ( 0.000000000000000000, -75.00000000000000000, 0.000000000000000000 ) ) ;
#3095 = ADVANCED_FACE ( 'NONE', ( #16321 ), #45280, .F. ) ;
#3096 = AXIS2_PLACEMENT_3D ( 'NONE', #8865, #40453, #9164 ) ;
#3097 = CARTESIAN_POINT ( 'NONE',  ( -10.93544969797999933, -77.37459665783399032, -0.5202540992781999885 ) ) ;
#3098 = CARTESIAN_POINT ( 'NONE',  ( 6.439298073612021334, -76.37065965127577272, -9.837794316883584855 ) ) ;
#3099 = CARTESIAN_POINT ( 'NONE',  ( 6.290530912463999869, -78.03614743357699979, 9.202381290206000486 ) ) ;
#3100 = CARTESIAN_POINT ( 'NONE',  ( 1.249653476780883121, -81.85243642884611859, 0.02917368571513033818 ) ) ;
#3101 = CARTESIAN_POINT ( 'NONE',  ( -10.07627163191000008, -23.24999999688999708, 7.601397897754999633 ) ) ;
#3102 = CARTESIAN_POINT ( 'NONE',  ( -11.65000000000000036, -76.00000000000000000, 0.000000000000000000 ) ) ;
#3103 = DIRECTION ( 'NONE',  ( -0.6489586447433819405, 0.04890182323493858646, 0.7592504784964787534 ) ) ;
#3104 = CARTESIAN_POINT ( 'NONE',  ( -0.8506806241676574398, -2.604166666666666519, -3.165411199172027068 ) ) ;
#3105 = CARTESIAN_POINT ( 'NONE',  ( -2.054101735612868129, -80.20991162323984724, -10.55179437476100013 ) ) ;
#3106 = B_SPLINE_CURVE_WITH_KNOTS ( 'NONE', 3,
 ( #44072, #3621, #22204, #40215, #21627, #39632, #57639, #12762, #35183, #8337, #9223, #36660, #5656, #54678, #14513, #22795, #50549, #19535 ),
 .UNSPECIFIED., .F., .F.,
 ( 4, 2, 2, 2, 2, 2, 2, 2, 4 ),
 ( 0.000000000000000000, 0.1250000000000000833, 0.2500000000000001665, 0.3750000000000001665, 0.5000000000000002220, 0.6250000000000002220, 0.7500000000000001110, 0.8750000000000001110, 1.000000000000000000 ),
 .UNSPECIFIED. ) ;
#3107 = DIRECTION ( 'NONE',  ( 0.000000000000000000, 0.000000000000000000, 1.000000000000000000 ) ) ;
#3108 = CARTESIAN_POINT ( 'NONE',  ( -10.39774148753954641, -79.88051113478326215, -4.208156475417354159 ) ) ;
#3109 = AXIS2_PLACEMENT_3D ( 'NONE', #43235, #2791, #6342 ) ;
#3110 = ADVANCED_FACE ( 'NONE', ( #34304 ), #52335, .T. ) ;
#3111 = CIRCLE ( 'NONE', #37946, 0.5000000000000006661 ) ;
#3112 = CARTESIAN_POINT ( 'NONE',  ( 7.652056849482000267, -79.31845263404798629, 9.281873293285000770 ) ) ;
#3113 = DIRECTION ( 'NONE',  ( 0.000000000000000000, 1.000000000000000000, 0.000000000000000000 ) ) ;
#3114 = CARTESIAN_POINT ( 'NONE',  ( 0.9616906432773000279, -78.95521297495899660, -11.22092312000000014 ) ) ;
#3115 = CARTESIAN_POINT ( 'NONE',  ( 9.393509054760620813, -77.39172388621676646, 5.413909507467279170 ) ) ;
#3116 = ORIENTED_EDGE ( 'NONE', *, *, #36821, .F. ) ;
#3117 = DIRECTION ( 'NONE',  ( 0.000000000000000000, 0.000000000000000000, 1.000000000000000000 ) ) ;
#3118 = ORIENTED_EDGE ( 'NONE', *, *, #22608, .T. ) ;
#3119 = ORIENTED_EDGE ( 'NONE', *, *, #17784, .F. ) ;
#3120 = CARTESIAN_POINT ( 'NONE',  ( 2.933193322904608991, -3.500000000000000000, -1.912021129721755530 ) ) ;
#3121 =( LENGTH_UNIT ( ) NAMED_UNIT ( * ) SI_UNIT ( .MILLI., .METRE. ) );
#3122 = ORIENTED_EDGE ( 'NONE', *, *, #51295, .F. ) ;
#3123 = CARTESIAN_POINT ( 'NONE',  ( -0.3706195565557000027, -80.60649082017198452, -3.525281893971000002 ) ) ;
#3124 = CARTESIAN_POINT ( 'NONE',  ( -3.112989155534594321, -79.30136502081413141, 8.977538257521471721 ) ) ;
#3125 = ADVANCED_FACE ( 'NONE', ( #57045 ), #28857, .T. ) ;
#3126 = ORIENTED_EDGE ( 'NONE', *, *, #57860, .F. ) ;
#3127 = CARTESIAN_POINT ( 'NONE',  ( 0.3860122406418020624, -82.75015049869273298, -1.188808172101050165 ) ) ;
#3128 = CARTESIAN_POINT ( 'NONE',  ( 7.345153731672205311, -55.57158755757197355, -8.188331488387625257 ) ) ;
#3129 = ORIENTED_EDGE ( 'NONE', *, *, #50351, .F. ) ;
#3130 = CARTESIAN_POINT ( 'NONE',  ( 7.217860716171294655, -79.49333333333333940, -6.227832364471528770 ) ) ;
#3131 = AXIS2_PLACEMENT_3D ( 'NONE', #44299, #4148, #22444 ) ;
#3132 = DIRECTION ( 'NONE',  ( -0.9903465037206092836, -0.1386138613861012392, 0.000000000000000000 ) ) ;
#3133 = CARTESIAN_POINT ( 'NONE',  ( -8.667213820335565089, -80.04983638533551016, 6.359185785815872016 ) ) ;
#3134 = CARTESIAN_POINT ( 'NONE',  ( 9.723199429438999175, -17.52306056078000296, -7.958735708418001487 ) ) ;
#3135 = CARTESIAN_POINT ( 'NONE',  ( -9.939389728518001732, -76.79599943707599152, 5.126617716248000001 ) ) ;
#3136 = B_SPLINE_CURVE_WITH_KNOTS ( 'NONE', 3,
 ( #20333, #25043, #11488, #38328, #56351, #29460, #7044, #38621, #17933, #17633, #34753, #35622, #58073, #12899, #58371, #48648, #44795, #52780, #39191, #48085, #53650, #13190, #31184, #26471, #7901, #40057 ),
 .UNSPECIFIED., .F., .F.,
 ( 4, 2, 2, 2, 2, 2, 2, 2, 2, 2, 2, 2, 4 ),
 ( 0.000000000000000000, 0.06249999999999995837, 0.1249999999999999167, 0.2499999999999998335, 0.3749999999999998335, 0.4374999999999998890, 0.4999999999999998890, 0.6249999999999998890, 0.6874999999999998890, 0.7499999999999997780, 0.8749999999999998890, 0.9374999999999998890, 1.000000000000000000 ),
 .UNSPECIFIED. ) ;
#3137 = CARTESIAN_POINT ( 'NONE',  ( 2.468869335794306785, -79.03645833334485360, 11.59083142015582624 ) ) ;
#3138 = CARTESIAN_POINT ( 'NONE',  ( -1.260603054430202263, -81.39590432937541209, -0.8352852932649793560 ) ) ;
#3139 = AXIS2_PLACEMENT_3D ( 'NONE', #27654, #5235, #1408 ) ;
#3140 = CARTESIAN_POINT ( 'NONE',  ( -4.770269334038999887, -76.30143890447099864, 10.03813491106999933 ) ) ;
#3141 = CARTESIAN_POINT ( 'NONE',  ( -10.12290050124000018, -18.75000000007999645, 7.648026767085999822 ) ) ;
#3142 = CARTESIAN_POINT ( 'NONE',  ( -9.001945887299001470, -77.53326167140099301, -3.097861235667999757 ) ) ;
#3143 = FACE_OUTER_BOUND ( 'NONE', #47788, .T. ) ;
#3144 = CARTESIAN_POINT ( 'NONE',  ( 1.506700327918974347, -2.937474389527924945, 2.893236496711840910 ) ) ;
#3145 = CARTESIAN_POINT ( 'NONE',  ( -3.236022287149000309, -78.56950264934789629, 1.036481599910999973 ) ) ;
#3146 = AXIS2_PLACEMENT_3D ( 'NONE', #850, #10562, #24125 ) ;
#3147 = CARTESIAN_POINT ( 'NONE',  ( -2.206042088423531222, -77.99158609026490296, 10.52113899700466781 ) ) ;
#3148 = CARTESIAN_POINT ( 'NONE',  ( 1.251003419626117052, -82.85390030615222656, 0.05208032629560303828 ) ) ;
#3149 = CARTESIAN_POINT ( 'NONE',  ( -1.557146760448999911, -85.92094503318799070, 3.187006944544999776 ) ) ;
#3150 = CARTESIAN_POINT ( 'NONE',  ( -3.268529449828999844, -2.290807261823000207, -1.950076325099000085 ) ) ;
#3151 = CARTESIAN_POINT ( 'NONE',  ( 10.53003223724000037, -18.67547470641000018, 7.612971414716000140 ) ) ;
#3152 = VECTOR ( 'NONE', #49791, 1000.000000000000000 ) ;
#3153 = CARTESIAN_POINT ( 'NONE',  ( -8.588902834722000890, -61.93240111547999760, -9.317946123669999636 ) ) ;
#3154 = DIRECTION ( 'NONE',  ( 0.000000000000000000, 1.000000000000000000, 0.000000000000000000 ) ) ;
#3155 = CARTESIAN_POINT ( 'NONE',  ( -1.297058042903999953, -81.19679289562199642, -0.3101879797029999941 ) ) ;
#3156 = CARTESIAN_POINT ( 'NONE',  ( 14.00000000000000000, -72.89999999999999147, -1.714505518806294638E-15 ) ) ;
#3157 = CARTESIAN_POINT ( 'NONE',  ( 5.865988621150640190E-14, -72.89999999999999147, 14.00000000000097877 ) ) ;
#3158 = LINE ( 'NONE', #30285, #23867 ) ;
#3159 = EDGE_CURVE ( 'NONE', #57766, #22110, #11891, .T. ) ;
#3160 = CARTESIAN_POINT ( 'NONE',  ( 13.49939038839240979, -32.88214388149999934, 0.1282931867975413143 ) ) ;
#3161 = CARTESIAN_POINT ( 'NONE',  ( 6.640280624951000021, -75.91133535973999358, 10.42739536823000002 ) ) ;
#3162 = ORIENTED_EDGE ( 'NONE', *, *, #13222, .F. ) ;
#3163 = CARTESIAN_POINT ( 'NONE',  ( -11.09105850093000001, -80.23598105172408168, 1.974238845993000258 ) ) ;
#3164 = CARTESIAN_POINT ( 'NONE',  ( 0.000000000000000000, -32.88214388149999934, 0.000000000000000000 ) ) ;
#3165 = CARTESIAN_POINT ( 'NONE',  ( 12.68703394093999925, -60.55066116444000102, 1.889962945498999902 ) ) ;
#3166 = CARTESIAN_POINT ( 'NONE',  ( -12.50000327350000084, -79.18030127599000423, -1.860978320792999963 ) ) ;
#3167 = DIRECTION ( 'NONE',  ( 0.000000000000000000, 1.000000000000000000, 0.000000000000000000 ) ) ;
#3168 = CARTESIAN_POINT ( 'NONE',  ( 8.731705537153999330, -78.67428574649498785, -3.798380529179000042 ) ) ;
#3169 = CARTESIAN_POINT ( 'NONE',  ( 2.265106641207000227, -85.23083017214499080, -3.503690498526999875 ) ) ;
#3170 = CARTESIAN_POINT ( 'NONE',  ( -0.4597697825790413861, -79.97871958790278768, 10.74439705486481067 ) ) ;
#3171 = CARTESIAN_POINT ( 'NONE',  ( -1.606812318740999945, -79.48408011494099412, 0.1592736582230999953 ) ) ;
#3172 = ORIENTED_EDGE ( 'NONE', *, *, #20214, .T. ) ;
#3173 = CARTESIAN_POINT ( 'NONE',  ( -1.750000000000000000, -55.55000000278000272, -12.50000000000000000 ) ) ;
#3174 = CARTESIAN_POINT ( 'NONE',  ( 5.628103047462848174, -78.92394918533045711, 7.438029003534223804 ) ) ;
#3175 = CARTESIAN_POINT ( 'NONE',  ( -1.507301607646650332, -78.84234659871619044, -3.678386913577406769 ) ) ;
#3176 = ORIENTED_EDGE ( 'NONE', *, *, #12093, .F. ) ;
#3177 = EDGE_CURVE ( 'NONE', #41516, #19523, #44190, .T. ) ;
#3178 = CARTESIAN_POINT ( 'NONE',  ( -4.428614322242999890, -79.71475654597799121, 10.12250943391000035 ) ) ;
#3179 = AXIS2_PLACEMENT_3D ( 'NONE', #19689, #45696, #37390 ) ;
#3180 = CARTESIAN_POINT ( 'NONE',  ( 12.82904109059999875, -55.47547726255000100, 2.062673488410000200 ) ) ;
#3181 = CARTESIAN_POINT ( 'NONE',  ( 7.235133928286000327, -80.06358356157298317, 8.863387837910000400 ) ) ;
#3182 = ORIENTED_EDGE ( 'NONE', *, *, #23349, .F. ) ;
#3183 = CARTESIAN_POINT ( 'NONE',  ( -0.7974440169908999509, -78.81086622188499291, -12.02330465019000094 ) ) ;
#3184 = ORIENTED_EDGE ( 'NONE', *, *, #42622, .T. ) ;
#3185 = ORIENTED_EDGE ( 'NONE', *, *, #8365, .T. ) ;
#3186 = TOROIDAL_SURFACE ( 'NONE', #6970, 13.50000000000000000, 0.5000000000000000000 ) ;
#3187 = ADVANCED_FACE ( 'NONE', ( #38453 ), #56470, .F. ) ;
#3188 = CARTESIAN_POINT ( 'NONE',  ( 0.3239878837106308085, -80.45445633517968531, 1.207198879959141102 ) ) ;
#3189 = CARTESIAN_POINT ( 'NONE',  ( 1.704789469356775555, -60.50346161385093069, 12.53199752969997682 ) ) ;
#3190 = CARTESIAN_POINT ( 'NONE',  ( -4.373213035511999358, -79.71821742630301344, -8.733596771889999388 ) ) ;
#3191 = EDGE_CURVE ( 'NONE', #46715, #42403, #24151, .T. ) ;
#3192 = VERTEX_POINT ( 'NONE', #49648 ) ;
#3193 = ORIENTED_EDGE ( 'NONE', *, *, #24448, .T. ) ;
#3194 = CARTESIAN_POINT ( 'NONE',  ( -5.950798862880000151, -78.96531715013686892, 10.72320280238000123 ) ) ;
#3195 = CARTESIAN_POINT ( 'NONE',  ( 3.437187628289000152, -78.85171435493610659, -2.028536691635913325 ) ) ;
#3196 = CARTESIAN_POINT ( 'NONE',  ( 9.966229686695001533, -55.13098097352000337, 7.657726530227999540 ) ) ;
#3197 = CARTESIAN_POINT ( 'NONE',  ( 10.12290050255000118, -55.55000002206000431, 7.648026768392999664 ) ) ;
#3198 = DIRECTION ( 'NONE',  ( 0.000000000000000000, 1.000000000000000000, 0.000000000000000000 ) ) ;
#3199 = FACE_BOUND ( 'NONE', #5719, .T. ) ;
#3200 = CARTESIAN_POINT ( 'NONE',  ( 4.212091869424105184, -80.69420159946982096, 10.38955714771617522 ) ) ;
#3201 = CARTESIAN_POINT ( 'NONE',  ( -11.86109855474000163, -78.66121286909155685, -1.682380905047000219 ) ) ;
#3202 = CARTESIAN_POINT ( 'NONE',  ( 8.582624075744034187, -78.81972267989517889, -3.449750442334098555 ) ) ;
#3203 = CARTESIAN_POINT ( 'NONE',  ( -3.151328970204000157, -76.05239898940999410, -11.89977497056000111 ) ) ;
#3204 = EDGE_CURVE ( 'NONE', #44781, #13102, #48768, .T. ) ;
#3205 = CARTESIAN_POINT ( 'NONE',  ( -9.500350562740681681, -79.30722730559423894, -0.7959580027764865395 ) ) ;
#3206 = CARTESIAN_POINT ( 'NONE',  ( 2.486604901413172808, -78.04583333333330586, -9.252740428348992907 ) ) ;
#3207 = CARTESIAN_POINT ( 'NONE',  ( -1.092232985442824100, -83.45833333333328596, 0.6295237254636200097 ) ) ;
#3208 = DIRECTION ( 'NONE',  ( 0.000000000000000000, 0.000000000000000000, -1.000000000000000000 ) ) ;
#3209 = CARTESIAN_POINT ( 'NONE',  ( -3.699256142337000064, -76.89766548106000243, 11.71059914860999918 ) ) ;
#3210 = CARTESIAN_POINT ( 'NONE',  ( -7.553727747500123435, -60.48581381149021752, -7.997114030232342685 ) ) ;
#3211 = CARTESIAN_POINT ( 'NONE',  ( 4.299999999999999822, -74.99999999999998579, 0.000000000000000000 ) ) ;
#3212 = DIRECTION ( 'NONE',  ( -1.000000000000000000, 0.000000000000000000, 0.000000000000000000 ) ) ;
#3213 = CIRCLE ( 'NONE', #6031, 12.80000000000000071 ) ;
#3214 = CARTESIAN_POINT ( 'NONE',  ( 1.348353453518538192, -80.96250278606902384, -0.6851815357594489564 ) ) ;
#3215 = CARTESIAN_POINT ( 'NONE',  ( 2.583569908777999746, -77.30999788869900158, 9.132097282893997914 ) ) ;
#3216 = LINE ( 'NONE', #11785, #35157 ) ;
#3217 = DIRECTION ( 'NONE',  ( 0.000000000000000000, 1.000000000000000000, 0.000000000000000000 ) ) ;
#3218 = CLOSED_SHELL ( 'NONE', ( #8338, #40918, #18041, #43680, #15503, #48520, #15837, #43302, #5850, #23792, #36669, #13142, #53101, #45053, #3292, #4458, #3125, #12505, #11156, #53920, #48834, #529, #4367, #48637, #10478, #44201, #20250, #22544, #23612, #55524, #14497, #22097, #40205, #6910, #26633, #45845, #55223, #32970, #5936, #17479, #54884, #25957, #53064, #23359, #20414, #14717, #10200, #34037, #4557, #13972, #11603, #5920, #32233, #55487, #36421, #21309, #55816, #17575, #57832, #5765, #20027, #23374, #51918, #11364, #35979, #16319, #26875, #24105, #48964, #16030, #55403, #6379, #44115, #16915, #17400, #12301, #45690, #57367, #39943, #47183, #5732, #49551, #24219, #14028, #21451, #38622, #16932, #9387, #25711, #35017, #3110, #22286, #39114, #40170, #54572, #4210, #14617, #33146, #28674, #14531, #41565, #54667, #26515, #53296, #47340, #14802, #38501, #34398, #9443, #23619, #34283, #5043, #21299, #3488, #24657, #40909, #16496, #50052, #46342, #31475, #49610, #19966, #20041, #44427, #19917, #45559, #43172, #56061, #6172, #34971, #56880, #4493, #704, #27577, #56678, #56236, #16762, #9524, #29584, #12397, #43910, #47705, #38748, #12469, #28572, #48984, #38225, #57923, #46201, #10248, #6593, #52537, #37276, #24351, #30854, #28816, #12799, #3833, #9251, #33556, #16417, #31589, #29512, #36010, #42726, #13174, #50139, #22479, #22366, #31327, #34072, #29550, #37015, #27182, #54613, #31761, #32022, #53354, #58332, #18641, #976, #57921, #38911, #37941, #4494, #7921, #10905, #22196, #21380, #25950, #31508, #41828, #26727, #10290, #39613, #37678, #9156, #50171, #17354, #43984, #52338, #32561, #43187, #6703, #8680, #5711, #23597, #26063, #21737, #21375, #45256, #7096, #41901, #42026, #18199, #48703, #20008, #57471, #15039, #34434, #17220, #37299, #29784, #20577, #4795, #33162, #52970, #43972, #6515, #55747, #2531, #56383, #34149, #13300, #34327, #12366, #42712, #7828, #40016, #7506, #1636, #7030, #56631, #9458, #34880, #29760, #32486, #32352, #57205, #39530, #57220, #11434, #13277, #17754, #15007, #677, #8818, #44149, #57296, #49376, #22836, #55436, #56300, #24366, #47504, #16791, #46220, #5696, #49282, #13404, #41914, #49111, #4984, #11670, #40943, #16398, #29948, #17303, #249, #7904, #42844, #46376, #33520, #17463, #32716, #6066, #38165, #35114, #52022, #39032, #10731, #21529, #50550, #12054, #18411, #2658, #55826, #8749, #28300, #56772, #3035, #30120, #32437, #39476, #10619, #6117, #5226, #48559, #21635, #30835, #41288, #20955, #33294, #57614, #24969, #52698, #47370, #12776, #52294, #31903, #17772, #32316, #8908, #49931, #28074, #10529, #20961, #46185, #46754, #46603, #14787, #36338, #43342, #32522, #25499, #14428, #9317, #10565, #43713, #41666, #44030, #54470, #47584, #6237, #49721, #930, #40642, #32630, #40426, #30725, #28641, #20095, #36507, #33215, #19504, #42534, #33486, #29493, #55353, #42691, #41039, #56966, #16986, #43793, #31487, #3900, #8530, #47067, #21152, #42762, #38068, #40623, #51827, #38884, #54738, #57959, #33949, #10606, #4159, #16066, #12635, #19120, #7452, #48127, #55578, #50908, #56659, #27421, #36784, #15917, #37451, #25706, #30617, #32857, #15239, #5434, #2382, #56781, #34369, #54620, #7974, #14285, #53499, #44730, #27643, #8568, #20114, #34730, #50697, #4301, #36166, #56803, #12298, #44576, #52372, #9303, #285, #6802, #6857, #22319, #5611, #52559, #32027, #52484, #29721, #14752, #1722, #1973, #2775, #28026, #8446, #22193, #20810, #16813, #54295, #3187, #37516, #43760, #10132, #9131, #40588, #15294, #21249, #34612, #33321, #8035, #32651, #15623, #51382, #18860, #9650, #26542, #52741, #50327, #13348, #41608, #11592, #18385, #56475, #23395, #2585, #13071, #10406, #46236, #47326, #23915, #53266, #54039, #31255, #13773, #40707, #27571, #13549, #41088, #44915, #19057, #28215, #5877, #9531, #3499, #5088, #32227, #35229, #24240, #40437, #39920, #55919, #7414, #52129, #24574, #57275, #46884, #38669, #19441 ) ) ;
#3219 = CARTESIAN_POINT ( 'NONE',  ( 2.847026051941000002, -3.259547503149000214, -1.861134274785000153 ) ) ;
#3220 = CARTESIAN_POINT ( 'NONE',  ( 9.940990682305997694, -78.64225416815600056, -7.011364793726000855 ) ) ;
#3221 = CARTESIAN_POINT ( 'NONE',  ( -1.460959015002474937, -80.97916666666665719, 0.3926218265389144757 ) ) ;
#3223 = CARTESIAN_POINT ( 'NONE',  ( -7.644092900773785004, -18.47619833611051021, 10.09634159701094447 ) ) ;
#3222 = CARTESIAN_POINT ( 'NONE',  ( -11.50186437804589090, -76.18325783269531826, 2.401250034516278831 ) ) ;
#3224 = CARTESIAN_POINT ( 'NONE',  ( -0.6256353049379000941, -82.61393340258099727, 1.457043991488000012 ) ) ;
#3225 = CARTESIAN_POINT ( 'NONE',  ( -6.312747718300130373, -79.52497251010836976, 8.701216629874789277 ) ) ;
#3226 = ORIENTED_EDGE ( 'NONE', *, *, #981, .T. ) ;
#3227 = CARTESIAN_POINT ( 'NONE',  ( -1.249999999999999778, -82.01041666666662877, -0.1636246173744686228 ) ) ;
#3228 = CARTESIAN_POINT ( 'NONE',  ( -11.00710520982000062, -79.72435824023099826, -4.882200574570999763 ) ) ;
#3229 = CARTESIAN_POINT ( 'NONE',  ( -9.499162930933517046, -79.25065129256583418, -0.07774627389065781602 ) ) ;
#3230 = CARTESIAN_POINT ( 'NONE',  ( -6.855033324489887114, -79.99999999999998579, -6.359874399135010847 ) ) ;
#3231 = FACE_OUTER_BOUND ( 'NONE', #52360, .T. ) ;
#3232 = DIRECTION ( 'NONE',  ( 1.000000000000000000, 0.000000000000000000, 0.000000000000000000 ) ) ;
#3233 = CARTESIAN_POINT ( 'NONE',  ( 8.763152011282000942, -79.42031553780299191, -4.343982967351999847 ) ) ;
#3234 = FACE_OUTER_BOUND ( 'NONE', #57758, .T. ) ;
#3235 = CARTESIAN_POINT ( 'NONE',  ( 9.250000000000001776, -79.23958333333332860, -1.210822168571047186 ) ) ;
#3236 = VERTEX_POINT ( 'NONE', #36341 ) ;
#3237 = CARTESIAN_POINT ( 'NONE',  ( 0.000000000000000000, -87.20000000000000284, 0.000000000000000000 ) ) ;
#3238 = CARTESIAN_POINT ( 'NONE',  ( 2.028166799595999770, -0.9844610208691998432, -3.466423845304999585 ) ) ;
#3239 = CARTESIAN_POINT ( 'NONE',  ( 5.875583596582999668, -79.57968667140100649, 7.634009735705999944 ) ) ;
#3240 = DIRECTION ( 'NONE',  ( -1.000000000000000000, 0.000000000000000000, 0.000000000000000000 ) ) ;
#3241 = EDGE_CURVE ( 'NONE', #12329, #353, #49848, .T. ) ;
#3242 = CARTESIAN_POINT ( 'NONE',  ( 4.000000000000000000, -78.69999999999998863, 0.000000000000000000 ) ) ;
#3243 = CARTESIAN_POINT ( 'NONE',  ( 0.8512149552595998925, -80.16193060409999305, 1.432023780608000063 ) ) ;
#3244 = ORIENTED_EDGE ( 'NONE', *, *, #18460, .T. ) ;
#3245 = EDGE_CURVE ( 'NONE', #41301, #16006, #14699, .T. ) ;
#3246 = CARTESIAN_POINT ( 'NONE',  ( 0.3759584291129999811, -77.55688181347299803, -11.09523831386000126 ) ) ;
#3247 = CARTESIAN_POINT ( 'NONE',  ( 10.12290050122000018, -55.54999999974999980, -7.648026767069000087 ) ) ;
#3248 = CARTESIAN_POINT ( 'NONE',  ( 1.667961445601999992, -57.05199022587000002, -12.58338334673999981 ) ) ;
#3249 = CARTESIAN_POINT ( 'NONE',  ( -12.87024489159000140, -59.58461666436000570, 2.062597265787999845 ) ) ;
#3250 = FACE_BOUND ( 'NONE', #48402, .T. ) ;
#3251 = AXIS2_PLACEMENT_3D ( 'NONE', #19727, #37724, #24446 ) ;
#3252 = CARTESIAN_POINT ( 'NONE',  ( 3.269429986698999979, -79.55738422845298885, 9.203886808668999109 ) ) ;
#3253 = EDGE_LOOP ( 'NONE', ( #38606, #33928, #36721, #13284 ) ) ;
#3254 = EDGE_CURVE ( 'NONE', #48866, #46129, #37337, .T. ) ;
#3255 = VERTEX_POINT ( 'NONE', #8313 ) ;
#3256 = CARTESIAN_POINT ( 'NONE',  ( 9.642431301336001681, -77.02102521606900609, -8.092989473023999736 ) ) ;
#3257 = CARTESIAN_POINT ( 'NONE',  ( 2.342876876834760758, -78.74262638912878742, -10.49166047009287261 ) ) ;
#3258 = ORIENTED_EDGE ( 'NONE', *, *, #2878, .T. ) ;
#3259 = CARTESIAN_POINT ( 'NONE',  ( -0.7479529023060000892, -77.80888084965400253, -9.465622776916999825 ) ) ;
#3260 = CARTESIAN_POINT ( 'NONE',  ( 6.760013919724038978, -77.52291666666664582, 8.796335266380001627 ) ) ;
#3261 = CARTESIAN_POINT ( 'NONE',  ( 0.5222397222179528953, -53.63701780570490740, 12.70447686579673352 ) ) ;
#3262 = CARTESIAN_POINT ( 'NONE',  ( 5.552077009241000560, -78.59443890784000075, 11.35743496097000005 ) ) ;
#3263 = CARTESIAN_POINT ( 'NONE',  ( 14.00000000000000000, -32.90763690531000663, 1.352038286454999952E-05 ) ) ;
#3264 = CARTESIAN_POINT ( 'NONE',  ( -11.79999999999999893, -23.15000000000000213, -0.5999999999999999778 ) ) ;
#3265 = CARTESIAN_POINT ( 'NONE',  ( 10.14950121160999963, -22.75077027493999893, 7.674627477456000157 ) ) ;
#3266 = CARTESIAN_POINT ( 'NONE',  ( -11.20683111097000051, -79.90504937755049752, -0.4743912329535999728 ) ) ;
#3267 = CARTESIAN_POINT ( 'NONE',  ( 1.443912542026016155, -79.96302067931829072, 9.136300447085167420 ) ) ;
#3268 = ORIENTED_EDGE ( 'NONE', *, *, #49091, .T. ) ;
#3269 = CARTESIAN_POINT ( 'NONE',  ( -10.82575263932852572, -79.93590035623954293, 1.999893313492130620 ) ) ;
#3270 = EDGE_LOOP ( 'NONE', ( #3974, #51258, #19150 ) ) ;
#3271 = CARTESIAN_POINT ( 'NONE',  ( 7.994753734545000157, -78.93303046778699184, 7.938063182512999916 ) ) ;
#3272 = CARTESIAN_POINT ( 'NONE',  ( 7.757711236729307736, -77.30428715488800151, -5.039461175929132786 ) ) ;
#3273 = CARTESIAN_POINT ( 'NONE',  ( 0.1998609718125000101, -80.37904421889498963, -1.304078681214000168 ) ) ;
#3274 = CARTESIAN_POINT ( 'NONE',  ( 1.092232985442823212, -83.20833333333330017, -0.6295237254636224522 ) ) ;
#3275 = CARTESIAN_POINT ( 'NONE',  ( 0.1534498121882000021, -77.96905598575500562, 1.409436946036999760 ) ) ;
#3276 = CARTESIAN_POINT ( 'NONE',  ( -8.838834764832000701, -55.54999999966999980, -8.838834764832000701 ) ) ;
#3277 = CARTESIAN_POINT ( 'NONE',  ( -7.610717068332717439, -18.47984996834297888, 10.41172376763008245 ) ) ;
#3278 = CARTESIAN_POINT ( 'NONE',  ( 10.71369944335146762, -78.37083333333333712, 2.879226727952103548 ) ) ;
#3279 = CARTESIAN_POINT ( 'NONE',  ( -12.83044039274999903, -18.69360374348000065, -2.062670899148999926 ) ) ;
#3280 = CARTESIAN_POINT ( 'NONE',  ( -1.250000000000000000, -79.10000000000000853, 0.000000000000000000 ) ) ;
#3281 = CARTESIAN_POINT ( 'NONE',  ( 10.14733453800999996, -78.84106237267099004, 4.639310447764000145 ) ) ;
#3282 = CARTESIAN_POINT ( 'NONE',  ( 0.000000000000000000, -91.89999999999999147, 0.000000000000000000 ) ) ;
#3283 = CARTESIAN_POINT ( 'NONE',  ( -8.734850699938000673, -79.58966986058341320, 8.271005326623001253 ) ) ;
#3284 = CARTESIAN_POINT ( 'NONE',  ( 0.6655869891369000646, -82.09442852648498956, -4.118674637652000037 ) ) ;
#3285 = DIRECTION ( 'NONE',  ( 0.000000000000000000, -1.000000000000000000, 0.000000000000000000 ) ) ;
#3286 = VERTEX_POINT ( 'NONE', #54073 ) ;
#3287 = CARTESIAN_POINT ( 'NONE',  ( -1.438065998794000100, -83.41115579321099460, -0.3363867981957999742 ) ) ;
#3288 = CARTESIAN_POINT ( 'NONE',  ( 0.4542139134408000323, -80.54146017332999463, -1.519238769708999959 ) ) ;
#3289 = LINE ( 'NONE', #43440, #55934 ) ;
#3290 = CARTESIAN_POINT ( 'NONE',  ( 11.53501176087999980, -78.72656418587199312, -3.234124663588000104 ) ) ;
#3291 = CARTESIAN_POINT ( 'NONE',  ( -12.70451544424564361, -17.44534321915444863, 1.498804046748215546 ) ) ;
#3292 = ADVANCED_FACE ( 'NONE', ( #12736 ), #42070, .F. ) ;
#3293 = CARTESIAN_POINT ( 'NONE',  ( 1.224548907347106752, -79.02232155126675650, 0.3527677417113336267 ) ) ;
#3294 = CARTESIAN_POINT ( 'NONE',  ( -8.968518105033201238, -76.34128233971088662, 8.069401009964305871 ) ) ;
#3295 = CARTESIAN_POINT ( 'NONE',  ( -3.039602602086000083, -79.16964805011500061, -9.236151215514999180 ) ) ;
#3296 = CARTESIAN_POINT ( 'NONE',  ( 7.742244746672000133, -78.84361510090498371, -5.543281135378999913 ) ) ;
#3297 = CARTESIAN_POINT ( 'NONE',  ( -1.933504092460999857, -55.39593152692000189, -12.70940235704999921 ) ) ;
#3298 = CARTESIAN_POINT ( 'NONE',  ( 9.798996500078068550, -75.99648035482640296, 6.483966265465372913 ) ) ;
#3299 = CARTESIAN_POINT ( 'NONE',  ( -1.122584031195864362, -81.68897639063932559, -0.6023342644404590107 ) ) ;
#3300 = VERTEX_POINT ( 'NONE', #21601 ) ;
#3301 = CARTESIAN_POINT ( 'NONE',  ( 11.00000000000000000, -18.25000000000000000, 1.016729233725000008E-14 ) ) ;
#3302 = CARTESIAN_POINT ( 'NONE',  ( -0.3926218265389256890, -79.29583333333334849, 1.460959015002472050 ) ) ;
#3303 = CARTESIAN_POINT ( 'NONE',  ( -3.799897982867999957, -79.72664421481898955, 11.66812693903999865 ) ) ;
#3304 = DIRECTION ( 'NONE',  ( -1.000000000000000000, 0.000000000000000000, 0.000000000000000000 ) ) ;
#3305 = CARTESIAN_POINT ( 'NONE',  ( 1.496210884224999926, -83.11583851079198837, 0.7325374182646999799 ) ) ;
#3306 = CARTESIAN_POINT ( 'NONE',  ( 10.31626776183999894, -78.15242887846198983, -3.746764721243999841 ) ) ;
#3307 = DIRECTION ( 'NONE',  ( 1.000000000000000000, 0.000000000000000000, 0.000000000000000000 ) ) ;
#3308 = CARTESIAN_POINT ( 'NONE',  ( -10.53979166895999953, -76.55163446013099815, -6.281747244366999716 ) ) ;
#3309 = CARTESIAN_POINT ( 'NONE',  ( 5.947890417171738164, -78.53226363305368807, 10.13299647784000257 ) ) ;
#3310 = DIRECTION ( 'NONE',  ( 0.000000000000000000, 1.000000000000000000, 0.000000000000000000 ) ) ;
#3311 = ORIENTED_EDGE ( 'NONE', *, *, #26106, .F. ) ;
#3312 = CARTESIAN_POINT ( 'NONE',  ( 5.587778422887999419, -79.87564813785350282, -9.645275144704999803 ) ) ;
#3313 = CARTESIAN_POINT ( 'NONE',  ( 1.105138191744446718, -79.88914713198865059, 0.5837908578609295462 ) ) ;
#3314 = CARTESIAN_POINT ( 'NONE',  ( -5.684557159767971157, -78.07291666666667140, -7.396918292183161547 ) ) ;
#3315 = CARTESIAN_POINT ( 'NONE',  ( -10.61618518222999796, -78.21817073422899114, 3.433396544298999764 ) ) ;
#3316 = ADVANCED_FACE ( 'NONE', ( #53478 ), #370, .F. ) ;
#3317 = CARTESIAN_POINT ( 'NONE',  ( 10.26699006316251683, -77.59166666666666856, 5.917523019358090330 ) ) ;
#3318 = CARTESIAN_POINT ( 'NONE',  ( -0.3273215601811345077, -78.99604344152334079, 1.250887209240275633 ) ) ;
#3319 = CARTESIAN_POINT ( 'NONE',  ( 1.520202006809699524, -82.11451394755752631, 0.3017852963696689428 ) ) ;
#3320 = CARTESIAN_POINT ( 'NONE',  ( 0.01229450786555221289, -79.72617763684984027, -1.249719495759485710 ) ) ;
#3321 = CARTESIAN_POINT ( 'NONE',  ( 8.696932689530999738, -76.29999999999999716, -6.318691462144000681 ) ) ;
#3322 = DIRECTION ( 'NONE',  ( 0.000000000000000000, -1.000000000000000000, 0.000000000000000000 ) ) ;
#3323 = CIRCLE ( 'NONE', #36310, 8.800000000000000711 ) ;
#3324 = DIRECTION ( 'NONE',  ( -0.7071067811865474617, 0.000000000000000000, 0.7071067811865474617 ) ) ;
#3325 = VERTEX_POINT ( 'NONE', #27474 ) ;
#3326 = EDGE_CURVE ( 'NONE', #6234, #23510, #39605, .T. ) ;
#3327 = ORIENTED_EDGE ( 'NONE', *, *, #33623, .T. ) ;
#3328 = CARTESIAN_POINT ( 'NONE',  ( -12.66313295592999921, -53.62196533848999991, 0.06049275240488000138 ) ) ;
#3329 = VECTOR ( 'NONE', #58150, 1000.000000000000114 ) ;
#3330 = ORIENTED_EDGE ( 'NONE', *, *, #34450, .F. ) ;
#3331 = CARTESIAN_POINT ( 'NONE',  ( 8.438902753042999194, -78.73739079806000518, -8.898539530003999332 ) ) ;
#3332 = VERTEX_POINT ( 'NONE', #26312 ) ;
#3333 = CARTESIAN_POINT ( 'NONE',  ( 1.500000000000000000, -81.75000000000000000, 0.000000000000000000 ) ) ;
#3334 = CARTESIAN_POINT ( 'NONE',  ( -4.522750724863999316, -77.98240233375699404, 9.935798501838000618 ) ) ;
#3335 = VECTOR ( 'NONE', #54267, 1000.000000000000114 ) ;
#3336 = CARTESIAN_POINT ( 'NONE',  ( -7.675809325333999844, -78.31138667140099585, -6.269164879585000349 ) ) ;
#3337 = CARTESIAN_POINT ( 'NONE',  ( 3.507155896972999898, -79.04801148567800340, 10.65448112794999957 ) ) ;
#3338 = VERTEX_POINT ( 'NONE', #4474 ) ;
#3339 = ORIENTED_EDGE ( 'NONE', *, *, #26131, .F. ) ;
#3340 = CARTESIAN_POINT ( 'NONE',  ( -5.503123143393462868, -77.52574563389143236, 7.434945069734956391 ) ) ;
#3341 = CARTESIAN_POINT ( 'NONE',  ( -5.876696946710000091, -77.45018012715098621, -9.346046374399000101 ) ) ;
#3342 = CARTESIAN_POINT ( 'NONE',  ( 9.000000000000000000, -0.5000000000000000000, 0.000000000000000000 ) ) ;
#3343 = CARTESIAN_POINT ( 'NONE',  ( -12.59682790095999927, -60.18734115192999923, -1.801645751184999922 ) ) ;
#3344 = CARTESIAN_POINT ( 'NONE',  ( -9.669247687117000112, -77.83690361071398911, -0.8224101967608999919 ) ) ;
#3345 = CARTESIAN_POINT ( 'NONE',  ( 7.642147947518999729, -22.78485473281999774, 10.55910102242999926 ) ) ;
#3346 = CARTESIAN_POINT ( 'NONE',  ( -12.57042253521000141, -15.89905023022000030, 0.000000000000000000 ) ) ;
#3347 = CARTESIAN_POINT ( 'NONE',  ( 10.42531125072000009, -55.53514854654000032, 7.624341767124000135 ) ) ;
#3348 = CARTESIAN_POINT ( 'NONE',  ( -10.55592303174000079, -79.95834473742999648, -3.904632140253000205 ) ) ;
#3349 = CARTESIAN_POINT ( 'NONE',  ( 12.43570956085999946, -17.12016029981999665, -0.4384071701242000518 ) ) ;
#3350 = FACE_OUTER_BOUND ( 'NONE', #46619, .T. ) ;
#3351 = VERTEX_POINT ( 'NONE', #44326 ) ;
#3352 = CARTESIAN_POINT ( 'NONE',  ( -9.101506735319000896, -53.91932813864999474, 8.485532457216999447 ) ) ;
#3353 = CARTESIAN_POINT ( 'NONE',  ( 11.88382656225999945, -78.44160216807300401, -1.513515996960000054 ) ) ;
#3354 = CARTESIAN_POINT ( 'NONE',  ( -9.395773752832997872, -17.29509747843999889, -8.188237371225000061 ) ) ;
#3355 = EDGE_CURVE ( 'NONE', #37074, #8174, #57905, .T. ) ;
#3357 = CARTESIAN_POINT ( 'NONE',  ( -4.000000000000000000, -5.200000000000000178, 0.5999999999999999778 ) ) ;
#3356 = CARTESIAN_POINT ( 'NONE',  ( -5.684148906237979304, -78.52710219421626903, 7.396423488596521878 ) ) ;
#3358 = CARTESIAN_POINT ( 'NONE',  ( 7.601397897754999633, -55.55000000209000177, 10.07627163191000008 ) ) ;
#3359 = CARTESIAN_POINT ( 'NONE',  ( -0.2870568347697000089, -80.17991464100198584, -11.28808005806000025 ) ) ;
#3360 = CARTESIAN_POINT ( 'NONE',  ( 13.49939038839240979, -9.295797029142999435, 0.1282931867975413143 ) ) ;
#3361 = CARTESIAN_POINT ( 'NONE',  ( 6.459716167540999976, -77.49702107270799445, -9.225293035625000471 ) ) ;
#3362 = CARTESIAN_POINT ( 'NONE',  ( 1.738970389193763122, -3.500000000000001332, 2.879943715822681494 ) ) ;
#3363 = CARTESIAN_POINT ( 'NONE',  ( 0.5376952571279000059, -80.69460651026599862, 11.24298004781999971 ) ) ;
#3364 = EDGE_CURVE ( 'NONE', #17621, #47646, #32872, .T. ) ;
#3365 = ORIENTED_EDGE ( 'NONE', *, *, #5634, .T. ) ;
#3366 = DIRECTION ( 'NONE',  ( 0.000000000000000000, 1.000000000000000000, 0.000000000000000000 ) ) ;
#3367 = LINE ( 'NONE', #52387, #6067 ) ;
#3368 = AXIS2_PLACEMENT_3D ( 'NONE', #46810, #1934, #42068 ) ;
#3369 = CARTESIAN_POINT ( 'NONE',  ( -12.83044039274999903, -23.30639625649999758, 2.062670899148999926 ) ) ;
#3370 = CARTESIAN_POINT ( 'NONE',  ( 3.754188153876000467, -2.981688735460999773, 0.6259984742306999861 ) ) ;
#3371 = B_SPLINE_CURVE_WITH_KNOTS ( 'NONE', 3,
 ( #42656, #12222, #29635, #2793, #33776, #56813 ),
 .UNSPECIFIED., .F., .F.,
 ( 4, 2, 4 ),
 ( 0.000000000000000000, 0.5000000000000000000, 1.000000000000000000 ),
 .UNSPECIFIED. ) ;
#3372 = CARTESIAN_POINT ( 'NONE',  ( 9.243445784771999740, -79.26341260731899752, -0.8678123785519999966 ) ) ;
#3374 = CARTESIAN_POINT ( 'NONE',  ( -12.77302454164000167, -54.07764858523999862, 1.481891240072999993 ) ) ;
#3373 = B_SPLINE_CURVE_WITH_KNOTS ( 'NONE', 3,
 ( #3872, #3019, #52325, #57893, #34577, #13007, #4168, #26579, #21589, #11879, #57319, #3586, #52610, #8013, #31007, #7444, #39596, #57034, #17450, #8302, #29857, #26010, #34864, #39880, #49045, #12727, #30720, #8591, #48755, #16593 ),
 .UNSPECIFIED., .F., .F.,
 ( 4, 2, 2, 2, 2, 2, 2, 2, 2, 2, 2, 2, 2, 2, 4 ),
 ( 0.000000000000000000, 0.1250000000000009714, 0.1875000000000014155, 0.2500000000000018874, 0.3125000000000023315, 0.3750000000000027200, 0.5000000000000035527, 0.5625000000000039968, 0.6250000000000045519, 0.6875000000000049960, 0.7500000000000054401, 0.8125000000000059952, 0.8437500000000055511, 0.8750000000000051070, 1.000000000000000000 ),
 .UNSPECIFIED. ) ;
#3375 = CARTESIAN_POINT ( 'NONE',  ( 7.803382786781845049, -77.28749999999999432, -7.800872125332472429 ) ) ;
#3376 = DIRECTION ( 'NONE',  ( 0.4045849535018030685, -0.8201353734597037759, -0.4045849535018030685 ) ) ;
#3377 = CARTESIAN_POINT ( 'NONE',  ( -1.250000000001000089, -82.24999999999900524, 4.142826023433999917E-11 ) ) ;
#3378 = CARTESIAN_POINT ( 'NONE',  ( -4.139728944602000027, -84.78749735065200355, -0.5405960093036000780 ) ) ;
#3379 = FACE_OUTER_BOUND ( 'NONE', #15527, .T. ) ;
#3380 = B_SPLINE_SURFACE_WITH_KNOTS ( 'NONE', 3, 3, ( 
 ( #20504, #38500, #16076, #34056 ),
 ( #58251, #13067, #31065, #8953 ),
 ( #21928, #44094, #3643, #49103 ),
 ( #36102, #12500, #26937, #12782 ) ),
 .UNSPECIFIED., .F., .F., .F.,
 ( 4, 4 ),
 ( 4, 4 ),
 ( -0.1566102636784000024, 0.3603425273004000062 ),
 ( -0.0006517983049530999724, 0.01399779397395000020 ),
 .UNSPECIFIED. ) ;
#3381 = CARTESIAN_POINT ( 'NONE',  ( 3.719372377260759421, -76.80315702122973676, 11.49187281106599201 ) ) ;
#3382 = CARTESIAN_POINT ( 'NONE',  ( 10.84983825364951748, -76.41841306282870505, -4.509958312123425905 ) ) ;
#3383 = CARTESIAN_POINT ( 'NONE',  ( -3.190971086128000067, -76.74278493408199608, -10.56027646911999973 ) ) ;
#3384 = EDGE_CURVE ( 'NONE', #25767, #48350, #8947, .T. ) ;
#3385 = CARTESIAN_POINT ( 'NONE',  ( 1.181146588278086940, -81.87666702745578107, 0.4112698556210559464 ) ) ;
#3386 = CARTESIAN_POINT ( 'NONE',  ( -0.8405563561534999950, -76.82762132708718639, -9.635375415708001157 ) ) ;
#3387 = CARTESIAN_POINT ( 'NONE',  ( 9.539544502573999551, -79.32444805011499511, 0.5400218831816999687 ) ) ;
#3388 = CARTESIAN_POINT ( 'NONE',  ( -0.5095438350929912819, -3.488646560560789922, 3.221021376419205939 ) ) ;
#3389 = CARTESIAN_POINT ( 'NONE',  ( -5.498018440344079494, -80.18236152930400351, -9.239502841344624073 ) ) ;
#3390 = CARTESIAN_POINT ( 'NONE',  ( -5.930212039233577315, -76.09166666665643675, 10.26675032132114040 ) ) ;
#3391 = CARTESIAN_POINT ( 'NONE',  ( 4.782544914675210812, -79.68985673377078172, 10.14637241100733434 ) ) ;
#3392 = CARTESIAN_POINT ( 'NONE',  ( -8.734850699938000673, -79.43798715743798766, 8.271005326623001253 ) ) ;
#3393 = DIRECTION ( 'NONE',  ( 0.000000000000000000, -1.000000000000000000, 0.000000000000000000 ) ) ;
#3394 = CARTESIAN_POINT ( 'NONE',  ( 0.000000000000000000, -74.70999999999999375, 0.000000000000000000 ) ) ;
#3395 = CARTESIAN_POINT ( 'NONE',  ( 5.414072109562871660, -77.43337924860836097, 9.393465288415251635 ) ) ;
#3396 = ORIENTED_EDGE ( 'NONE', *, *, #15670, .F. ) ;
#3397 = EDGE_CURVE ( 'NONE', #28402, #27979, #26025, .T. ) ;
#3398 = CARTESIAN_POINT ( 'NONE',  ( -1.689459950960819912, -24.29188253903401318, 12.71013585610284302 ) ) ;
#3399 = EDGE_CURVE ( 'NONE', #27850, #17621, #55481, .T. ) ;
#3400 = ORIENTED_EDGE ( 'NONE', *, *, #47283, .T. ) ;
#3401 = ORIENTED_EDGE ( 'NONE', *, *, #32773, .T. ) ;
#3402 = CARTESIAN_POINT ( 'NONE',  ( -10.75000000000000000, -78.50000000000000000, 0.000000000000000000 ) ) ;
#3403 =( NAMED_UNIT ( * ) PLANE_ANGLE_UNIT ( ) SI_UNIT ( $, .RADIAN. ) );
#3404 = ORIENTED_EDGE ( 'NONE', *, *, #821, .T. ) ;
#3405 = CARTESIAN_POINT ( 'NONE',  ( 3.380803704886000016, -82.53049761187099875, 0.3410288241623999905 ) ) ;
#3406 = CARTESIAN_POINT ( 'NONE',  ( -1.469979871250949310, -79.28716761129145141, 9.385467292518239191 ) ) ;
#3407 = ORIENTED_EDGE ( 'NONE', *, *, #19575, .F. ) ;
#3408 = CARTESIAN_POINT ( 'NONE',  ( -9.428374488006999954, -78.94967853533998436, 7.989839463457000690 ) ) ;
#3409 = EDGE_LOOP ( 'NONE', ( #34555, #30308, #2392, #27625 ) ) ;
#3410 = ORIENTED_EDGE ( 'NONE', *, *, #33798, .F. ) ;
#3411 = CARTESIAN_POINT ( 'NONE',  ( 0.000000000000000000, -75.15999999999999659, 0.000000000000000000 ) ) ;
#3412 = CARTESIAN_POINT ( 'NONE',  ( -7.601397897754999633, -60.04999999966999980, -9.369164850722000892 ) ) ;
#3413 = CIRCLE ( 'NONE', #16609, 12.90000000000000036 ) ;
#3414 = CARTESIAN_POINT ( 'NONE',  ( -4.824611332692330556, -80.01213778624108386, 9.606459940033937883 ) ) ;
#3415 = PLANE ( 'NONE',  #11724 ) ;
#3416 = EDGE_CURVE ( 'NONE', #34022, #43554, #16610, .T. ) ;
#3417 = CARTESIAN_POINT ( 'NONE',  ( -3.272863771658545584, -86.25171435493597016, -2.284202767185578242 ) ) ;
#3418 = FACE_BOUND ( 'NONE', #15827, .T. ) ;
#3419 = VECTOR ( 'NONE', #39889, 1000.000000000000000 ) ;
#3420 = CARTESIAN_POINT ( 'NONE',  ( -3.226165562315000290, -77.90040178014000105, 12.71052925661000010 ) ) ;
#3421 = CARTESIAN_POINT ( 'NONE',  ( 0.3870708775265000456, -80.22814348455999323, -1.294661097694999929 ) ) ;
#3422 = CARTESIAN_POINT ( 'NONE',  ( 9.860379324123998757, -76.74539509872099075, 4.873887145968000212 ) ) ;
#3423 = CARTESIAN_POINT ( 'NONE',  ( -9.122985626357428046, -78.61336444762311260, -1.527181035531375297 ) ) ;
#3424 = CARTESIAN_POINT ( 'NONE',  ( -3.964978550598999618, -81.82057179202399766, 1.156485587164000295 ) ) ;
#3425 = CARTESIAN_POINT ( 'NONE',  ( -10.30336598198321951, -80.12884657563031965, -3.851716267939166549 ) ) ;
#3426 = CARTESIAN_POINT ( 'NONE',  ( -2.327681217703248873, -3.038872842925070650, 2.267910747349583200 ) ) ;
#3427 = CARTESIAN_POINT ( 'NONE',  ( 3.225105726725999933, -79.36005496681158888, -1.476568833565000238 ) ) ;
#3428 = CARTESIAN_POINT ( 'NONE',  ( 0.8338927958961740439, -24.80053577746324223, -12.50366901602911796 ) ) ;
#3429 = CARTESIAN_POINT ( 'NONE',  ( 3.546855337703000544, -85.43994503318799616, 0.03714407394458000417 ) ) ;
#3430 = CARTESIAN_POINT ( 'NONE',  ( -1.568660613942000071, -1.873862256653000102, -3.467930652269000102 ) ) ;
#3431 = CARTESIAN_POINT ( 'NONE',  ( -0.9315676299678438133, -79.69017609249064549, 0.8708394447951318673 ) ) ;
#3432 = EDGE_CURVE ( 'NONE', #44710, #32490, #947, .T. ) ;
#3433 = CARTESIAN_POINT ( 'NONE',  ( 10.42531124905999995, -23.26485148473999942, 7.624341765453999997 ) ) ;
#3434 = CARTESIAN_POINT ( 'NONE',  ( 12.50000000000000000, -55.55000000278000272, -1.750000000000000000 ) ) ;
#3435 = CARTESIAN_POINT ( 'NONE',  ( 0.8962411872155999770, -81.49446863590900136, 0.9875868993909000526 ) ) ;
#3436 = CARTESIAN_POINT ( 'NONE',  ( -12.66235371498999918, -16.86260492134000089, -0.4957155363045999685 ) ) ;
#3437 = DIRECTION ( 'NONE',  ( 0.000000000000000000, 0.000000000000000000, 1.000000000000000000 ) ) ;
#3438 = CARTESIAN_POINT ( 'NONE',  ( 0.9186508726441414696, -79.57551408595966791, -1.236643120628077241 ) ) ;
#3439 = CARTESIAN_POINT ( 'NONE',  ( 1.931736162947051527, -23.76670395715774120, -12.72978979890034523 ) ) ;
#3440 = CARTESIAN_POINT ( 'NONE',  ( -10.36185853650999888, -76.12736320551000802, -6.742090815642000301 ) ) ;
#3441 = ORIENTED_EDGE ( 'NONE', *, *, #3177, .F. ) ;
#3442 = CARTESIAN_POINT ( 'NONE',  ( 8.735587516832000077, -80.07898629742850005, 6.757696599697999851 ) ) ;
#3443 = CARTESIAN_POINT ( 'NONE',  ( 12.46165725309000116, -60.47155322489999918, 1.631637378451999965 ) ) ;
#3444 = CARTESIAN_POINT ( 'NONE',  ( -1.667917367065999912, -23.28056535155999995, -12.49306764015999960 ) ) ;
#3445 = CARTESIAN_POINT ( 'NONE',  ( -8.527407416480999203, -78.35459554355099954, 4.476218573567000369 ) ) ;
#3446 = CARTESIAN_POINT ( 'NONE',  ( -3.362678705222999831, -84.86381343186599224, -2.470316658220000239 ) ) ;
#3447 = CARTESIAN_POINT ( 'NONE',  ( -2.935164356122387908, -79.99732793198559477, 10.34225144355774617 ) ) ;
#3448 = CARTESIAN_POINT ( 'NONE',  ( 1.275615568647000098, -80.38862546449399815, 0.6187600927687999519 ) ) ;
#3449 = ORIENTED_EDGE ( 'NONE', *, *, #21568, .F. ) ;
#3450 = AXIS2_PLACEMENT_3D ( 'NONE', #57488, #3198, #29175 ) ;
#3451 = CARTESIAN_POINT ( 'NONE',  ( -11.00000000000000000, -78.71041666666667425, -1.439896632895320217 ) ) ;
#3452 = CARTESIAN_POINT ( 'NONE',  ( 3.399999999999689937, -78.72609999968184979, -4.163799117100620920E-16 ) ) ;
#3453 = ORIENTED_EDGE ( 'NONE', *, *, #38507, .F. ) ;
#3454 = CIRCLE ( 'NONE', #47809, 9.199999999999999289 ) ;
#3455 = CARTESIAN_POINT ( 'NONE',  ( -6.384381598444999639, -78.79539988511800175, 8.884114358872000849 ) ) ;
#3456 = CARTESIAN_POINT ( 'NONE',  ( 12.92177931905999877, -58.55736537918999574, 2.062503053667999797 ) ) ;
#3457 = FACE_OUTER_BOUND ( 'NONE', #8183, .T. ) ;
#3458 = AXIS2_PLACEMENT_3D ( 'NONE', #15490, #47098, #28759 ) ;
#3459 = ORIENTED_EDGE ( 'NONE', *, *, #1178, .F. ) ;
#3460 = AXIS2_PLACEMENT_3D ( 'NONE', #18296, #31549, #3827 ) ;
#3461 = ORIENTED_EDGE ( 'NONE', *, *, #48168, .F. ) ;
#3462 = VERTEX_POINT ( 'NONE', #55522 ) ;
#3463 = CARTESIAN_POINT ( 'NONE',  ( -2.061613410425999771, -18.79429985524000202, 12.83797036855999885 ) ) ;
#3464 = DIRECTION ( 'NONE',  ( -1.000000000000000000, 0.000000000000000000, 0.000000000000000000 ) ) ;
#3465 = CARTESIAN_POINT ( 'NONE',  ( -0.5483576180056000116, -79.87054292801151689, -9.751923335751000010 ) ) ;
#3466 = EDGE_LOOP ( 'NONE', ( #43905, #24684, #12476, #4857, #49366, #30018, #49439 ) ) ;
#3467 = CARTESIAN_POINT ( 'NONE',  ( 10.98964036629034347, -18.48475764895797724, 0.4777763868204561448 ) ) ;
#3468 = ORIENTED_EDGE ( 'NONE', *, *, #12887, .F. ) ;
#3469 = CARTESIAN_POINT ( 'NONE',  ( 1.058112158932194902, -79.44686744937848744, 0.7105453803691499370 ) ) ;
#3470 = B_SPLINE_CURVE_WITH_KNOTS ( 'NONE', 3,
 ( #5061, #50819, #1812, #10362, #5345, #37504 ),
 .UNSPECIFIED., .F., .F.,
 ( 4, 1, 1, 4 ),
 ( 0.000000000000000000, 0.3333333311575783497, 0.6666666623152567306, 0.9999999934728349693 ),
 .UNSPECIFIED. ) ;
#3471 = CARTESIAN_POINT ( 'NONE',  ( -0.03630073495416798190, -78.96264283715740362, -3.851479002382501182 ) ) ;
#3472 = FACE_OUTER_BOUND ( 'NONE', #5779, .T. ) ;
#3473 = EDGE_CURVE ( 'NONE', #22042, #6883, #33066, .T. ) ;
#3474 = CARTESIAN_POINT ( 'NONE',  ( -1.500000000000000444, -78.38958333333333428, 0.1963495408493560745 ) ) ;
#3475 = CARTESIAN_POINT ( 'NONE',  ( 0.000000000000000000, -82.00000000000000000, 0.000000000000000000 ) ) ;
#3476 = CARTESIAN_POINT ( 'NONE',  ( 12.70395504303439260, -61.40679290091602383, -1.447100708809422986 ) ) ;
#3477 = CARTESIAN_POINT ( 'NONE',  ( -9.690626710582000314, -78.20001450688755540, -7.043281791253000357 ) ) ;
#3478 = CARTESIAN_POINT ( 'NONE',  ( -10.14950121160999963, -22.75077027493999893, -7.674627477456000157 ) ) ;
#3479 = CARTESIAN_POINT ( 'NONE',  ( -8.596763593952999827, -25.13532396123000012, 9.310159863706001460 ) ) ;
#3480 = AXIS2_PLACEMENT_3D ( 'NONE', #7195, #33469, #55927 ) ;
#3481 = CARTESIAN_POINT ( 'NONE',  ( 3.496576729809000028, -79.53150264934789959, 2.281129299029000190 ) ) ;
#3482 = CARTESIAN_POINT ( 'NONE',  ( -7.898810015907999471, -77.87186001420199943, -5.922837236108999370 ) ) ;
#3483 = CARTESIAN_POINT ( 'NONE',  ( -12.77302454167999990, -17.27764858556999883, 1.481891240072999993 ) ) ;
#3484 = CARTESIAN_POINT ( 'NONE',  ( 0.5999999999999999778, -5.000000000000000000, -0.5999999999999999778 ) ) ;
#3485 = CARTESIAN_POINT ( 'NONE',  ( 6.725657209017000149, -77.17088373642599208, -9.843613558058999402 ) ) ;
#3486 = CARTESIAN_POINT ( 'NONE',  ( -8.190817883596533733, -60.03019609282340951, -7.342377162853142458 ) ) ;
#3487 = AXIS2_PLACEMENT_3D ( 'NONE', #5752, #19053, #37042 ) ;
#3488 = ADVANCED_FACE ( 'NONE', ( #51112 ), #15374, .T. ) ;
#3489 = CARTESIAN_POINT ( 'NONE',  ( 4.117077995765999532, -1.540283069271000116, -0.2120472831400999902 ) ) ;
#3490 = CARTESIAN_POINT ( 'NONE',  ( 0.7681833999686451531, -78.67708333333332860, -0.9995835529977240563 ) ) ;
#3491 = AXIS2_PLACEMENT_3D ( 'NONE', #28886, #10613, #55775 ) ;
#3492 = CARTESIAN_POINT ( 'NONE',  ( -0.6245939647354400437, -80.65885271342463625, 1.376621695022554936 ) ) ;
#3493 = CARTESIAN_POINT ( 'NONE',  ( -0.4970193761121000087, -77.33610725566698818, 9.477499788518001012 ) ) ;
#3494 = CARTESIAN_POINT ( 'NONE',  ( 1.980532758766000212, -59.56256650660999696, -12.80088938804999898 ) ) ;
#3495 = CARTESIAN_POINT ( 'NONE',  ( -7.954951288349001004, -23.44678171330999916, -9.722718241315000398 ) ) ;
#3496 = CARTESIAN_POINT ( 'NONE',  ( -3.535607672357000020, -2.959660817501999830, 0.3961643838024999642 ) ) ;
#3497 = CARTESIAN_POINT ( 'NONE',  ( 0.4919088493939999807, -77.31291771239200727, 12.15485731165999894 ) ) ;
#3498 = CARTESIAN_POINT ( 'NONE',  ( -0.7554284705563544255, -80.91666666666667140, 1.310679582531384169 ) ) ;
#3499 = ADVANCED_FACE ( 'NONE', ( #36635 ), #15672, .F. ) ;
#3501 = CARTESIAN_POINT ( 'NONE',  ( 1.301001062148999798, -78.50521359734798921, 0.2190019327816999928 ) ) ;
#3500 = CARTESIAN_POINT ( 'NONE',  ( -7.719682335140538143, -75.80000000000002558, 9.059469227681002934 ) ) ;
#3502 = CARTESIAN_POINT ( 'NONE',  ( 0.3489451476548999787, -81.28743241160998423, -1.426530384489999914 ) ) ;
#3503 = CARTESIAN_POINT ( 'NONE',  ( -7.608827018420656785, -79.53773796140059460, 7.593810091919143801 ) ) ;
#3504 = ORIENTED_EDGE ( 'NONE', *, *, #19789, .T. ) ;
#3505 = CARTESIAN_POINT ( 'NONE',  ( -10.18589234708000113, -23.28917565320000094, -7.641012386039999882 ) ) ;
#3506 = CARTESIAN_POINT ( 'NONE',  ( -5.548968227290999700, -79.70989843751300441, -10.55673919551000139 ) ) ;
#3507 = EDGE_CURVE ( 'NONE', #40288, #25723, #28706, .T. ) ;
#3508 = CARTESIAN_POINT ( 'NONE',  ( 8.495067938628560356, -79.03726686963507575, 4.296429619035287750 ) ) ;
#3509 = B_SPLINE_CURVE_WITH_KNOTS ( 'NONE', 3,
 ( #32368, #37689, #22948, #6103, #14084, #54542 ),
 .UNSPECIFIED., .F., .F.,
 ( 4, 1, 1, 4 ),
 ( 0.000000000000000000, 0.3333333333333000081, 0.6666666666667000474, 1.000000000000000000 ),
 .UNSPECIFIED. ) ;
#3510 = DIRECTION ( 'NONE',  ( 0.000000000000000000, -1.000000000000000000, 0.000000000000000000 ) ) ;
#3511 = CARTESIAN_POINT ( 'NONE',  ( -6.760013919724099374, -79.02708333333332291, 8.796335266379958995 ) ) ;
#3512 = CARTESIAN_POINT ( 'NONE',  ( 0.5847238537393000257, -1.182588905188999950, -3.489934961497000110 ) ) ;
#3513 = CARTESIAN_POINT ( 'NONE',  ( -7.959955112152999668, -79.09500618921398996, 5.491262329125000008 ) ) ;
#3514 = CARTESIAN_POINT ( 'NONE',  ( 12.43646324844999995, -24.92048514568000073, -0.1256879863178999857 ) ) ;
#3515 = CARTESIAN_POINT ( 'NONE',  ( -0.5999999999999999778, -5.200000000000000178, 4.000000000000000000 ) ) ;
#3516 = ORIENTED_EDGE ( 'NONE', *, *, #38191, .F. ) ;
#3517 = B_SPLINE_CURVE_WITH_KNOTS ( 'NONE', 3,
 ( #51296, #47461, #43295, #32958, #38565, #6698, #19695, #43009, #2567, #19404, #11146, #42135, #20567, #33835, #56580, #20280, #55413, #52160, #56006, #6109, #24117, #16140, #1701, #42719, #33254, #33549, #51588, #37695, #14961, #34116, #10852, #51873, #28825, #55714, #10552, #11716, #29120, #11427, #29693, #29408, #24416, #46874, #6401, #42432, #2001, #47166, #19996, #24707, #2284, #38274, #8944, #54112, #49986, #9530, #39930, #13946, #13653, #40821, #8646, #21134, #31648, #44962, #57946, #49395, #27515, #31354, #26931, #13356, #40228, #49691, #413, #31942, #54408, #4517, #20848, #26631, #22518, #17500, #2851, #40528, #18391, #4220, #35789, #35488, #22217, #122, #53820, #58240, #9237, #36382, #18099, #36095, #38852, #27223, #43584, #16429, #56871, #45262, #34412, #4810, #52441, #12001, #53518, #22810, #44666, #17803, #29979, #48033, #7564, #25564, #3147, #13059, #31058, #49095, #41987, #1853, #41111, #36676, #37255, #45556, #10404, #23681, #15111, #55861, #5671, #41694, #45853, #10996, #15413, #702, #5102, #1272, #46436, #19263, #50563, #14526, #46146, #33406, #18684, #33108, #28097, #23101, #55267, #18973, #14815, #19547, #54692, #32812, #51151, #10706, #5386, #14234, #51444, #32232, #50274, #50859, #5965, #28389, #10117, #32519, #23968, #9822, #1556, #27806, #37545, #23393, #55562, #36964, #28683, #46735, #41405, #6254, #24269, #42285 ),
 .UNSPECIFIED., .F., .F.,
 ( 4, 2, 2, 2, 1, 1, 1, 2, 2, 2, 2, 1, 1, 1, 1, 1, 2, 2, 2, 2, 2, 1, 1, 1, 1, 2, 2, 2, 1, 2, 2, 1, 1, 1, 1, 1, 1, 2, 2, 2, 2, 2, 1, 1, 1, 2, 2, 2, 2, 1, 1, 1, 2, 2, 2, 2, 1, 1, 1, 2, 2, 2, 1, 1, 1, 1, 1, 2, 2, 2, 2, 2, 1, 1, 1, 1, 2, 2, 2, 2, 2, 2, 2, 2, 2, 2, 2, 2, 1, 1, 1, 2, 2, 2, 1, 1, 2, 2, 1, 1, 2, 2, 2, 2, 1, 2, 2, 1, 2, 4 ),
 ( 0.000000000000000000, 0.03125000000004676121, 0.04687500000007015916, 0.05468750000008183038, 0.05859375000008768680, 0.06054687500009063583, 0.06152343750009210688, 0.06201171875009282852, 0.06250000000009355017, 0.09375000000013758439, 0.1093750000001596362, 0.1171875000001706552, 0.1210937500001761785, 0.1230468750001789263, 0.1240234375001803419, 0.1245117187501810357, 0.1247558593751813966, 0.1250000000001817435, 0.1562500000002016165, 0.1718750000002115252, 0.1796875000002164657, 0.1835937500002188805, 0.1855468750002200740, 0.1865234375002206846, 0.1870117187502209621, 0.1872558593752211009, 0.1875000000002212397, 0.2031250000002264577, 0.2109375000002290113, 0.2148437500002303435, 0.2187500000002316480, 0.2343750000002371714, 0.2421875000002399470, 0.2460937500002412792, 0.2480468750002420286, 0.2490234375002424450, 0.2495117187502426670, 0.2497558593752427503, 0.2500000000002428058, 0.2656250000002447487, 0.2734375000002456924, 0.2773437500002461920, 0.2792968750002464140, 0.2802734375002465250, 0.2807617187502465805, 0.2810058593752466360, 0.2812500000002466360, 0.2968750000002501888, 0.3046875000002519096, 0.3085937500002527978, 0.3105468750002532419, 0.3115234375002534639, 0.3120117187502535749, 0.3125000000002536304, 0.3281250000002541301, 0.3359375000002544076, 0.3398437500002545186, 0.3417968750002544631, 0.3427734375002545186, 0.3432617187502545741, 0.3437500000002546297, 0.3593750000002553513, 0.3671875000002556844, 0.3710937500002557954, 0.3730468750002559064, 0.3740234375002558509, 0.3745117187502558509, 0.3747558593752558509, 0.3750000000002557954, 0.4062500000002492451, 0.4218750000002459699, 0.4296875000002443601, 0.4335937500002434719, 0.4355468750002430278, 0.4365234375002428058, 0.4370117187502426948, 0.4372558593752426392, 0.4375000000002425282, 0.4687500000002331468, 0.4843750000002284284, 0.4921875000002260414, 0.4960937500002248757, 0.5000000000002235989, 0.5625000000002046141, 0.6250000000001857403, 0.6406250000001809664, 0.6425781250001804112, 0.6435546875001800782, 0.6445312500001797451, 0.6484375000001786349, 0.6562500000001763034, 0.6875000000001670886, 0.7500000000001487699, 0.8125000000001304512, 0.8437500000001213474, 0.8476562500001202372, 0.8496093750001195710, 0.8500976562501194600, 0.8505859375001192380, 0.8515625000001189049, 0.8593750000001161293, 0.8750000000001104672, 0.9062500000000992539, 0.9218750000000937028, 0.9238281250000927036, 0.9248046875000915934, 0.9257812500000903722, 0.9296875000000855982, 0.9375000000000761613, 1.000000000000000000 ),
 .UNSPECIFIED. ) ;
#3518 = CARTESIAN_POINT ( 'NONE',  ( -12.70556836324529293, -53.57227722633783173, 0.2641978056810228570 ) ) ;
#3519 = CARTESIAN_POINT ( 'NONE',  ( -5.199237357848000229, -79.90086001420199580, -8.238468209311999857 ) ) ;
#3520 = CARTESIAN_POINT ( 'NONE',  ( 0.6679678761999167103, -1.742764817395623389, -3.205531000182274770 ) ) ;
#3521 = CARTESIAN_POINT ( 'NONE',  ( -0.1963495408493606265, -78.51458333333334849, -1.500000000000000222 ) ) ;
#3522 = CARTESIAN_POINT ( 'NONE',  ( 3.433232437268999959, -83.87042953870898998, -0.8930104441242000535 ) ) ;
#3523 = ORIENTED_EDGE ( 'NONE', *, *, #28250, .F. ) ;
#3524 = FACE_OUTER_BOUND ( 'NONE', #15954, .T. ) ;
#3525 = CARTESIAN_POINT ( 'NONE',  ( 8.583677311528019160, -61.77185920727337276, -9.102132575249884283 ) ) ;
#3526 = CARTESIAN_POINT ( 'NONE',  ( -8.485281374238999419, -55.64999999967000122, 8.485281374238999419 ) ) ;
#3527 = VECTOR ( 'NONE', #6675, 999.9999999999998863 ) ;
#3528 = CARTESIAN_POINT ( 'NONE',  ( -12.49306764019000049, -60.08056535122999975, 1.667917367065999912 ) ) ;
#3529 = CARTESIAN_POINT ( 'NONE',  ( -7.646966891740999195, -55.60358255701000019, -10.19019756604999927 ) ) ;
#3530 = CARTESIAN_POINT ( 'NONE',  ( -9.358268528169000788, -79.35326349721498218, -2.797054701638000296 ) ) ;
#3531 = VERTEX_POINT ( 'NONE', #20100 ) ;
#3532 = CONICAL_SURFACE ( 'NONE', #5437, 0.6999999997695030007, 0.7853981633972997312 ) ;
#3533 = ORIENTED_EDGE ( 'NONE', *, *, #47407, .F. ) ;
#3534 = CARTESIAN_POINT ( 'NONE',  ( 12.43062359974000053, -76.50248803030198985, -0.9980395665033999775 ) ) ;
#3535 = CARTESIAN_POINT ( 'NONE',  ( -10.07627163191000008, -55.55000000209000177, 7.601397897754999633 ) ) ;
#3536 = AXIS2_PLACEMENT_3D ( 'NONE', #38996, #20421, #38704 ) ;
#3537 = ORIENTED_EDGE ( 'NONE', *, *, #6365, .T. ) ;
#3538 = CARTESIAN_POINT ( 'NONE',  ( 1.009320482739999969, -77.55668084965400055, 9.441330439200999791 ) ) ;
#3539 = CARTESIAN_POINT ( 'NONE',  ( -2.099388381696000023E-14, -0.04999999937965000224, -12.74999999937999995 ) ) ;
#3540 = AXIS2_PLACEMENT_3D ( 'NONE', #26513, #31527, #39809 ) ;
#3541 = DIRECTION ( 'NONE',  ( -4.025425605489000457E-14, 1.534883903844000000E-11, -1.000000000000000000 ) ) ;
#3542 = CARTESIAN_POINT ( 'NONE',  ( 12.30436613475999863, -78.39634877618999553, -3.523071432600000108 ) ) ;
#3543 = CARTESIAN_POINT ( 'NONE',  ( 3.895497176767999559, -77.09677593747389324, 10.51870773133999926 ) ) ;
#3544 = CARTESIAN_POINT ( 'NONE',  ( -7.714303428875997959, -26.30294702886003222, 12.53545825868000385 ) ) ;
#3545 = CARTESIAN_POINT ( 'NONE',  ( 3.549939863155374464, -86.39318692756700102, 2.578428034955390746 ) ) ;
#3546 = CARTESIAN_POINT ( 'NONE',  ( 8.838834764832000701, -60.04999999966999980, -8.838834764832000701 ) ) ;
#3547 = CARTESIAN_POINT ( 'NONE',  ( 1.444432371921226865, -79.96301603591265916, 9.136218687011998796 ) ) ;
#3548 = CARTESIAN_POINT ( 'NONE',  ( -9.813001901106970237, -79.91600936110660314, 4.522963347059401507 ) ) ;
#3549 = VERTEX_POINT ( 'NONE', #25662 ) ;
#3550 = CARTESIAN_POINT ( 'NONE',  ( -9.332307860560000279, -79.07349223945099936, 6.311653060910999535 ) ) ;
#3551 = CARTESIAN_POINT ( 'NONE',  ( 5.130170376780485597, -77.27182112023126592, -7.706256298038600683 ) ) ;
#3552 = CARTESIAN_POINT ( 'NONE',  ( -0.1680659145979999936, -80.62710733580000522, 1.308557476745999981 ) ) ;
#3553 = DIRECTION ( 'NONE',  ( 0.000000000000000000, 0.000000000000000000, -1.000000000000000000 ) ) ;
#3554 = DIRECTION ( 'NONE',  ( -1.000000000000000000, 0.000000000000000000, 0.000000000000000000 ) ) ;
#3555 = CARTESIAN_POINT ( 'NONE',  ( -1.305945605467999870, -78.66939177743699929, -0.1872743590209999809 ) ) ;
#3556 = CARTESIAN_POINT ( 'NONE',  ( -0.09454008427527169078, -3.226439081450838131, 3.519011153166962114 ) ) ;
#3557 = CARTESIAN_POINT ( 'NONE',  ( -7.770365054039128694, -17.76417299472041122, 10.20675369723943859 ) ) ;
#3558 = DIRECTION ( 'NONE',  ( 0.7071067811865475727, 0.000000000000000000, 0.7071067811865475727 ) ) ;
#3559 = LINE ( 'NONE', #26552, #51524 ) ;
#3560 = CARTESIAN_POINT ( 'NONE',  ( 4.105747930350998942, -79.71192535698398274, -10.37470161445000016 ) ) ;
#3561 = EDGE_CURVE ( 'NONE', #38384, #40940, #53340, .T. ) ;
#3562 = CARTESIAN_POINT ( 'NONE',  ( 10.18589226631999978, -23.28917723430000208, -7.641012305222999679 ) ) ;
#3563 = CARTESIAN_POINT ( 'NONE',  ( -0.8845133210371012300, -83.03823067849943129, 0.8826922710338861444 ) ) ;
#3564 = CARTESIAN_POINT ( 'NONE',  ( 0.000000000000000000, -74.64999999999999147, 0.000000000000000000 ) ) ;
#3565 = B_SPLINE_CURVE_WITH_KNOTS ( 'NONE', 3,
 ( #40388, #54844, #50432, #14390, #27385, #40082, #45127, #49851, #53976, #31809, #32388, #13216, #45421, #13515, #23261, #40688, #35648, #4963 ),
 .UNSPECIFIED., .F., .F.,
 ( 4, 2, 2, 2, 2, 2, 2, 2, 4 ),
 ( 0.000000000000000000, 0.1249999999999999722, 0.2499999999999999445, 0.3749999999999998890, 0.4999999999999998890, 0.6249999999999998890, 0.7499999999999997780, 0.8749999999999998890, 1.000000000000000000 ),
 .UNSPECIFIED. ) ;
#3566 = ORIENTED_EDGE ( 'NONE', *, *, #40614, .T. ) ;
#3567 = CARTESIAN_POINT ( 'NONE',  ( -0.5667803598935999831, -82.23202630415998726, 1.605794812195000087 ) ) ;
#3568 = CARTESIAN_POINT ( 'NONE',  ( -1.413725673013999984, -80.47845843187998582, -0.3972755495651000279 ) ) ;
#3569 = CARTESIAN_POINT ( 'NONE',  ( 7.648026766753000416, -60.05000000550000294, -10.12290050090999927 ) ) ;
#3570 = CARTESIAN_POINT ( 'NONE',  ( 7.483561698776000526, -78.31962445451600274, 9.354804580292000793 ) ) ;
#3571 = CARTESIAN_POINT ( 'NONE',  ( 3.574993757284770979, -77.00000000000001421, 8.552566962383416183 ) ) ;
#3572 = CARTESIAN_POINT ( 'NONE',  ( 0.5021253177900999454, -81.86053999106999868, -1.588436081161999969 ) ) ;
#3573 = CARTESIAN_POINT ( 'NONE',  ( 2.687462146607000335, -77.71966499545499119, -11.62811462177000088 ) ) ;
#3574 = CARTESIAN_POINT ( 'NONE',  ( -5.764562846862999912, -78.99544805011498738, 7.830301022820999712 ) ) ;
#3575 = CARTESIAN_POINT ( 'NONE',  ( 5.376158796547000129, -78.87906701255899122, -7.990628517496999983 ) ) ;
#3576 = CARTESIAN_POINT ( 'NONE',  ( -0.9887300587134000285, -53.86589942198000358, -12.65963207085999898 ) ) ;
#3577 = CARTESIAN_POINT ( 'NONE',  ( 9.282381572011505710, -76.00223643008524732, 7.204816828411842344 ) ) ;
#3578 = CARTESIAN_POINT ( 'NONE',  ( 4.614362421890620070, -86.07389998728977787, 0.5296543453901456644 ) ) ;
#3579 = ORIENTED_EDGE ( 'NONE', *, *, #2518, .T. ) ;
#3580 = CARTESIAN_POINT ( 'NONE',  ( 13.99999999996999911, -5.900000000026970781, -3.874887541704999824E-10 ) ) ;
#3581 = CARTESIAN_POINT ( 'NONE',  ( 1.499999999999999778, -79.16041666666667709, 0.1963495408493654004 ) ) ;
#3582 = CARTESIAN_POINT ( 'NONE',  ( -9.570476163416000048, -79.38040701380199948, -7.680520617063000266 ) ) ;
#3583 = EDGE_CURVE ( 'NONE', #49218, #13366, #20951, .T. ) ;
#3584 = CARTESIAN_POINT ( 'NONE',  ( 2.301294140410000022, -78.54828561723799396, -3.984678389768961271 ) ) ;
#3585 = CARTESIAN_POINT ( 'NONE',  ( 9.694840914897000062, -79.64132365809399516, -5.145296513660000848 ) ) ;
#3586 = CARTESIAN_POINT ( 'NONE',  ( -0.5135400119346991143, -16.82131466139585640, 12.70453250098583986 ) ) ;
#3587 = CARTESIAN_POINT ( 'NONE',  ( -11.96958589357000058, -75.93049390057900894, 1.626211782151000040 ) ) ;
#3588 = DIRECTION ( 'NONE',  ( -0.7071067811865475727, 0.000000000000000000, 0.7071067811865475727 ) ) ;
#3589 = CARTESIAN_POINT ( 'NONE',  ( 0.0004189892803136687979, -77.98437500001877254, 1.281334813302893005 ) ) ;
#3590 = ORIENTED_EDGE ( 'NONE', *, *, #46709, .T. ) ;
#3591 = CARTESIAN_POINT ( 'NONE',  ( -0.2676215762113999808, -79.01806712638799013, 11.02860431212999970 ) ) ;
#3592 = CARTESIAN_POINT ( 'NONE',  ( 1.072822471686033063, -79.89348443873119265, 0.6422160631042705958 ) ) ;
#3593 = CARTESIAN_POINT ( 'NONE',  ( 5.539808784079905735, -77.76666666666665151, -9.611650271896829523 ) ) ;
#3594 = CARTESIAN_POINT ( 'NONE',  ( 9.791822688510999129, -79.03284900987598860, 5.349000663092000174 ) ) ;
#3595 = CARTESIAN_POINT ( 'NONE',  ( -11.75000000000000000, -77.79999999999999716, 1.702919296826999607E-14 ) ) ;
#3596 = CARTESIAN_POINT ( 'NONE',  ( 10.69999999999999929, -77.19999999999998863, 0.000000000000000000 ) ) ;
#3597 = CARTESIAN_POINT ( 'NONE',  ( 12.76303204525000012, -60.06485147653999945, 1.980584515753000208 ) ) ;
#3598 = ADVANCED_FACE ( 'NONE', ( #47845 ), #29790, .F. ) ;
#3599 = B_SPLINE_SURFACE_WITH_KNOTS ( 'NONE', 3, 3, ( 
 ( #35579, #34708, #27317, #31736 ),
 ( #14032, #45349, #55064, #9326 ),
 ( #54495, #10492, #9616, #41781 ),
 ( #4899, #5470, #50944, #32030 ),
 ( #22606, #32312, #37343, #36184 ),
 ( #22897, #19349, #55359, #40910 ),
 ( #4608, #1354, #50655, #46233 ),
 ( #9910, #214, #45646, #14902 ) ),
 .UNSPECIFIED., .F., .F., .F.,
 ( 4, 1, 1, 1, 1, 4 ),
 ( 4, 4 ),
 ( -0.01200407345746999990, 0.000000000000000000, 0.3333333333333000081, 0.6666666666667000474, 1.000000000000000000, 1.011997855551999947 ),
 ( -0.3559705542741999906, 1.355970554273999928 ),
 .UNSPECIFIED. ) ;
#3600 = CARTESIAN_POINT ( 'NONE',  ( -1.881092013513000039, -78.21382883426899468, 12.13496073407999987 ) ) ;
#3601 = CARTESIAN_POINT ( 'NONE',  ( -12.50000000000000000, -60.04999999966999980, 0.000000000000000000 ) ) ;
#3602 = CARTESIAN_POINT ( 'NONE',  ( -12.70556836352000118, -62.02772277195000328, -2.424224025342999716E-09 ) ) ;
#3603 = CARTESIAN_POINT ( 'NONE',  ( 10.26699006316251683, -76.09166666666665435, 5.917523019358090330 ) ) ;
#3604 = ORIENTED_EDGE ( 'NONE', *, *, #54172, .F. ) ;
#3605 = ORIENTED_EDGE ( 'NONE', *, *, #6294, .F. ) ;
#3606 = CARTESIAN_POINT ( 'NONE',  ( -1.243547092045951263, -78.51458333333333428, -9.500000000000003553 ) ) ;
#3607 = VERTEX_POINT ( 'NONE', #16531 ) ;
#3608 = CARTESIAN_POINT ( 'NONE',  ( 6.152927464707564020, -79.56974109780976789, 7.410766869306328886 ) ) ;
#3610 = EDGE_CURVE ( 'NONE', #7212, #44932, #20964, .T. ) ;
#3609 = EDGE_LOOP ( 'NONE', ( #5179, #30253, #35549, #13398 ) ) ;
#3611 = CARTESIAN_POINT ( 'NONE',  ( 1.460959015002472494, -81.77083333333453652, 0.3926218265389233020 ) ) ;
#3612 = CARTESIAN_POINT ( 'NONE',  ( 3.791268666074999683, -76.92018495668600053, 10.23726759892000082 ) ) ;
#3613 = CARTESIAN_POINT ( 'NONE',  ( -9.565996717342001077, -79.14193998579798972, -1.527434585433000036 ) ) ;
#3614 = CARTESIAN_POINT ( 'NONE',  ( -6.538910319532891258, -78.16269370453200338, -6.542411771513464203 ) ) ;
#3615 = B_SPLINE_CURVE_WITH_KNOTS ( 'NONE', 3,
 ( #7457, #38161, #25167, #16893, #3318, #25455, #34875, #57046, #20173, #56184, #56471, #56763, #11315, #6872 ),
 .UNSPECIFIED., .F., .F.,
 ( 4, 2, 2, 2, 2, 2, 4 ),
 ( 0.000000000000000000, 0.2500000000000000000, 0.5000000000000000000, 0.6250000000000000000, 0.7500000000000000000, 0.8750000000000000000, 1.000000000000000000 ),
 .UNSPECIFIED. ) ;
#3616 = CARTESIAN_POINT ( 'NONE',  ( -2.848564863371000122, -78.80288439866200179, -10.84913769893999991 ) ) ;
#3617 = ORIENTED_EDGE ( 'NONE', *, *, #38962, .F. ) ;
#3618 = ORIENTED_EDGE ( 'NONE', *, *, #47736, .F. ) ;
#3619 = CARTESIAN_POINT ( 'NONE',  ( -5.441782793747363733, -77.52508094701889263, 7.479905722084790654 ) ) ;
#3620 = CARTESIAN_POINT ( 'NONE',  ( 10.77519778174000109, -77.05057364238318485, -1.228540277667999892 ) ) ;
#3621 = CARTESIAN_POINT ( 'NONE',  ( -1.500000000000000888, -77.98958333333332860, 0.1963495408493559080 ) ) ;
#3622 = CARTESIAN_POINT ( 'NONE',  ( 9.662203867310999783, -79.08755209238998418, 0.9012207007054000574 ) ) ;
#3623 = CARTESIAN_POINT ( 'NONE',  ( -0.5731199659188802586, -86.12610001270964233, 4.609165628484651833 ) ) ;
#3624 = CIRCLE ( 'NONE', #44175, 0.6000000000000008660 ) ;
#3625 = CARTESIAN_POINT ( 'NONE',  ( -6.673815826044733335, -79.46282625145217082, -6.760806027906673954 ) ) ;
#3626 = CARTESIAN_POINT ( 'NONE',  ( 0.4326115402657000342, -78.85758603771999731, -1.568920109259999807 ) ) ;
#3627 = B_SPLINE_CURVE_WITH_KNOTS ( 'NONE', 3,
 ( #43968, #12938, #30936, #57822, #39808, #8231, #48124, #21805, #26511, #11809 ),
 .UNSPECIFIED., .F., .F.,
 ( 4, 2, 2, 2, 4 ),
 ( 0.000000000000000000, 0.2500000000000000000, 0.5000000000000000000, 0.7500000000000000000, 1.000000000000000000 ),
 .UNSPECIFIED. ) ;
#3628 = CARTESIAN_POINT ( 'NONE',  ( -11.09141466634999951, -79.85628064642098423, 1.909950515085000022 ) ) ;
#3629 = CARTESIAN_POINT ( 'NONE',  ( 12.43421868118999818, -17.56340276631999942, -1.197355605037999871 ) ) ;
#3630 = EDGE_CURVE ( 'NONE', #43983, #23504, #20253, .T. ) ;
#3631 = FACE_OUTER_BOUND ( 'NONE', #54569, .T. ) ;
#3632 = CARTESIAN_POINT ( 'NONE',  ( -8.082524092276882399, -78.54166666666665719, -4.658475568430820779 ) ) ;
#3633 = ORIENTED_EDGE ( 'NONE', *, *, #2452, .T. ) ;
#3634 = EDGE_CURVE ( 'NONE', #55158, #3325, #7092, .T. ) ;
#3635 = CARTESIAN_POINT ( 'NONE',  ( -6.506018757879999725, -79.93025345888189293, 9.866615368227002136 ) ) ;
#3636 = DIRECTION ( 'NONE',  ( 0.000000000000000000, 1.000000000000000000, 0.000000000000000000 ) ) ;
#3637 = CARTESIAN_POINT ( 'NONE',  ( 0.9627474882855999727, -78.33308490637799082, -11.94107121277999894 ) ) ;
#3638 = CARTESIAN_POINT ( 'NONE',  ( -8.227509542990000924, -17.17460508872999725, -9.516261809269000338 ) ) ;
#3640 = CARTESIAN_POINT ( 'NONE',  ( -1.200170490671999879, -17.56594298002000087, -12.43444080551000042 ) ) ;
#3639 = CARTESIAN_POINT ( 'NONE',  ( 7.627487525433000570, -60.09778754156999980, 10.35845608626999947 ) ) ;
#3641 = CARTESIAN_POINT ( 'NONE',  ( -8.300970689365446020, -78.84166666666665435, -4.784380313523547201 ) ) ;
#3642 = CARTESIAN_POINT ( 'NONE',  ( 10.42272502862000039, -58.55453807205000061, -7.691893942725999800 ) ) ;
#3643 = CARTESIAN_POINT ( 'NONE',  ( -0.4831833036036000117, -82.26234308346199953, -1.158768654956999988 ) ) ;
#3644 = CARTESIAN_POINT ( 'NONE',  ( -10.91036644271999911, -76.84334884066400662, -2.792455208340000272 ) ) ;
#3645 = CARTESIAN_POINT ( 'NONE',  ( 2.598917237794080570, -1.802083333333333259, 1.997276839918479485 ) ) ;
#3646 = CARTESIAN_POINT ( 'NONE',  ( -6.760013919724102038, -80.12708333335245925, 8.796335266379953666 ) ) ;
#3647 = ORIENTED_EDGE ( 'NONE', *, *, #40726, .T. ) ;
#3648 = LINE ( 'NONE', #58256, #35752 ) ;
#3649 = CARTESIAN_POINT ( 'NONE',  ( 1.484804496640999893, -54.08130846584000295, 12.77261165604999960 ) ) ;
#3650 = CARTESIAN_POINT ( 'NONE',  ( -12.49306752634999995, -18.71943307332999851, 1.667917367010000040 ) ) ;
#3651 = EDGE_CURVE ( 'NONE', #50383, #32447, #39253, .T. ) ;
#3652 = CARTESIAN_POINT ( 'NONE',  ( -0.9552977345487000393, -2.613729981583999606, 3.684183631831999595 ) ) ;
#3653 = CARTESIAN_POINT ( 'NONE',  ( 4.297451186800683942, -78.10789250826600494, -9.948289673926124621 ) ) ;
#3654 = CARTESIAN_POINT ( 'NONE',  ( -7.313922093392000612, -79.57512096206998820, -5.944137246278000219 ) ) ;
#3655 = DIRECTION ( 'NONE',  ( 0.000000000000000000, -1.000000000000000000, 0.000000000000000000 ) ) ;
#3656 = CARTESIAN_POINT ( 'NONE',  ( 0.000000000000000000, -3.749999999256000027, 0.000000000000000000 ) ) ;
#3657 = CARTESIAN_POINT ( 'NONE',  ( -1.933504092458000034, -60.20406847242999504, 12.70940235709999833 ) ) ;
#3658 = DIRECTION ( 'NONE',  ( 1.000000000000000000, 0.000000000000000000, 0.000000000000000000 ) ) ;
#3659 = CARTESIAN_POINT ( 'NONE',  ( -3.844914979824000323, -84.79907450217399401, 1.508354171302999980 ) ) ;
#3660 = CIRCLE ( 'NONE', #29108, 11.05000000000000071 ) ;
#3661 = DIRECTION ( 'NONE',  ( 0.000000000000000000, 0.000000000000000000, -1.000000000000000000 ) ) ;
#3662 = CARTESIAN_POINT ( 'NONE',  ( -1.206665456719130836, -77.07001001640816185, -11.96363559127014398 ) ) ;
#3663 = B_SPLINE_CURVE_WITH_KNOTS ( 'NONE', 3,
 ( #11805, #3235, #52817, #16808, #29779, #42523, #47555, #52248, #42812, #24507, #25366, #21226, #43382, #43106, #51966, #30069, #2376, #7366 ),
 .UNSPECIFIED., .F., .F.,
 ( 4, 2, 2, 2, 2, 2, 2, 2, 4 ),
 ( 0.000000000000000000, 0.1250000000000000278, 0.2500000000000000555, 0.3750000000000001665, 0.5000000000000001110, 0.6250000000000001110, 0.7500000000000002220, 0.8750000000000001110, 1.000000000000000000 ),
 .UNSPECIFIED. ) ;
#3664 = B_SPLINE_CURVE_WITH_KNOTS ( 'NONE', 3,
 ( #5749, #33183, #15777, #29057, #24352, #23757, #10781, #41770, #1346, #19339, #34343, #11650, #2497, #21354, #16363, #29627, #44092, #25786, #12498, #38785, #52092 ),
 .UNSPECIFIED., .F., .F.,
 ( 4, 2, 2, 2, 2, 2, 1, 2, 2, 2, 4 ),
 ( 0.000000000000000000, 0.1249999999999999167, 0.2499999999999998335, 0.3749999999999997780, 0.4999999999999996669, 0.5624999999999996669, 0.6249999999999995559, 0.6874999999999996669, 0.7499999999999996669, 0.8749999999999998890, 1.000000000000000000 ),
 .UNSPECIFIED. ) ;
#3665 = CARTESIAN_POINT ( 'NONE',  ( -10.09586848912000079, -78.24005621299899360, 4.990731814912999553 ) ) ;
#3666 = CARTESIAN_POINT ( 'NONE',  ( 1.036471533130701506, -81.89769297308482976, 0.7000341817469545314 ) ) ;
#3667 = CARTESIAN_POINT ( 'NONE',  ( 1.541711259781999743, -79.15111531869999340, 0.1510856428486999914 ) ) ;
#3668 = CARTESIAN_POINT ( 'NONE',  ( 10.12290050255000118, -55.55000002206000431, 7.648026768392999664 ) ) ;
#3669 = CARTESIAN_POINT ( 'NONE',  ( -2.317989000404999889, -79.61534415034599022, -9.269382932261999386 ) ) ;
#3670 = CARTESIAN_POINT ( 'NONE',  ( 2.598917237794088564, -2.697916666666666519, -1.997276839918468605 ) ) ;
#3671 = CARTESIAN_POINT ( 'NONE',  ( -1.794921875279598122, -80.21179327765182165, -10.59966322526386229 ) ) ;
#3672 = CARTESIAN_POINT ( 'NONE',  ( 2.813789756862274505, -77.14583333333334281, -10.47020627418438821 ) ) ;
#3673 = CARTESIAN_POINT ( 'NONE',  ( -9.355955347629251406, -16.82516908807116351, -8.610895743724782392 ) ) ;
#3674 = CARTESIAN_POINT ( 'NONE',  ( -7.858171174022000827, -78.92996543302999157, 9.108036400545000077 ) ) ;
#3675 = CARTESIAN_POINT ( 'NONE',  ( -1.250000000000001332, -81.98958333333334281, 0.1636246173744632659 ) ) ;
#3676 = CARTESIAN_POINT ( 'NONE',  ( 1.104250457816000175, -79.69059423600799619, 11.20779173096999948 ) ) ;
#3677 = CARTESIAN_POINT ( 'NONE',  ( -10.98362417419999915, -23.15000000000000213, -0.5999999999999999778 ) ) ;
#3678 = ORIENTED_EDGE ( 'NONE', *, *, #787, .T. ) ;
#3679 = DIRECTION ( 'NONE',  ( 0.000000000000000000, 0.000000000000000000, 1.000000000000000000 ) ) ;
#3680 = ORIENTED_EDGE ( 'NONE', *, *, #26432, .F. ) ;
#3681 = DIRECTION ( 'NONE',  ( -1.000000000000000000, 0.000000000000000000, 0.000000000000000000 ) ) ;
#3683 = EDGE_CURVE ( 'NONE', #48012, #44548, #2386, .T. ) ;
#3682 = VERTEX_POINT ( 'NONE', #6800 ) ;
#3684 = FACE_OUTER_BOUND ( 'NONE', #58058, .T. ) ;
#3685 = CARTESIAN_POINT ( 'NONE',  ( -10.76888293467999880, -79.08652177698400010, -1.790677617362999907 ) ) ;
#3686 = CARTESIAN_POINT ( 'NONE',  ( 3.534928549350000004, -79.52423699984079519, 0.2631568632097999738 ) ) ;
#3687 = CARTESIAN_POINT ( 'NONE',  ( 1.484863747559565628, -79.26247634984721913, 9.383218303840022756 ) ) ;
#3688 = VERTEX_POINT ( 'NONE', #35977 ) ;
#3689 = CARTESIAN_POINT ( 'NONE',  ( 10.22358047590571317, -78.07468344508760083, -3.366618272953084468 ) ) ;
#3690 = CARTESIAN_POINT ( 'NONE',  ( -10.34744176347000000, -78.37400547832000086, 6.482158579691000178 ) ) ;
#3691 = ORIENTED_EDGE ( 'NONE', *, *, #16360, .F. ) ;
#3692 = ORIENTED_EDGE ( 'NONE', *, *, #12384, .F. ) ;
#3693 = FACE_OUTER_BOUND ( 'NONE', #2016, .T. ) ;
#3694 = DIRECTION ( 'NONE',  ( 1.000000000000000000, 0.000000000000000000, 0.000000000000000000 ) ) ;
#3695 = DIRECTION ( 'NONE',  ( 1.000000000000000000, 0.000000000000000000, 0.000000000000000000 ) ) ;
#3696 = CARTESIAN_POINT ( 'NONE',  ( -1.327128730425999992, -79.71402465532199244, 0.1315503032697999675 ) ) ;
#3697 = DIRECTION ( 'NONE',  ( 0.7026410690473250398, 0.1122098755728047209, 0.7026410690473250398 ) ) ;
#3698 = VECTOR ( 'NONE', #44379, 1000.000000000000000 ) ;
#3699 = CARTESIAN_POINT ( 'NONE',  ( -1.599699822274783134, -86.36264283715696877, -3.503736395301632722 ) ) ;
#3700 = CARTESIAN_POINT ( 'NONE',  ( 3.266119435496772194, -85.82533526675824476, 1.464745090892502155 ) ) ;
#3701 = CARTESIAN_POINT ( 'NONE',  ( -9.359366689070000689, -77.56737393437001060, -9.185202947203000790 ) ) ;
#3702 = CARTESIAN_POINT ( 'NONE',  ( 11.52003294054999927, -77.52814994903998524, 5.205193576094000463 ) ) ;
#3703 = CARTESIAN_POINT ( 'NONE',  ( -10.78744351475000052, -76.53722080125399430, -1.449653075750000131 ) ) ;
#3704 = CARTESIAN_POINT ( 'NONE',  ( -8.329046064005918737, -78.63589279464400761, -4.024567744346438936 ) ) ;
#3705 = ADVANCED_FACE ( 'NONE', ( #39815 ), #12666, .F. ) ;
#3706 = AXIS2_PLACEMENT_3D ( 'NONE', #9262, #26954, #35817 ) ;
#3707 = CARTESIAN_POINT ( 'NONE',  ( -10.35747158360999975, -55.48415522678000400, 7.626500902197000720 ) ) ;
#3708 = CARTESIAN_POINT ( 'NONE',  ( -0.3986185775606674309, -2.985056446498978833, 3.227758659026054300 ) ) ;
#3709 = CARTESIAN_POINT ( 'NONE',  ( 0.7877379977805000211, -81.21500264934797997, 3.456071849709000166 ) ) ;
#3710 = CIRCLE ( 'NONE', #17882, 10.69999999999999929 ) ;
#3711 = CARTESIAN_POINT ( 'NONE',  ( -0.9356112518355850227, -24.74107830238661876, -12.50329130247234133 ) ) ;
#3712 = CARTESIAN_POINT ( 'NONE',  ( 2.575494480515000184, -83.75644503318798684, -2.438932253181000043 ) ) ;
#3713 = CARTESIAN_POINT ( 'NONE',  ( 2.113064247614999669, -3.454503108079999940, -3.165785623842000351 ) ) ;
#3714 = CARTESIAN_POINT ( 'NONE',  ( -1.136758720370837805, -80.78738817488307689, -0.5771817327056680824 ) ) ;
#3715 = VERTEX_POINT ( 'NONE', #3810 ) ;
#3716 = CARTESIAN_POINT ( 'NONE',  ( -8.643979526187999696, -62.05953772878000052, -9.422807787405000468 ) ) ;
#3717 = CARTESIAN_POINT ( 'NONE',  ( 11.00000000000000711, -79.43958333333333144, -1.439896632895300010 ) ) ;
#3718 = EDGE_CURVE ( 'NONE', #24905, #21333, #5308, .T. ) ;
#3719 = CARTESIAN_POINT ( 'NONE',  ( 0.08638142328466999476, -81.09172904305800955, 1.330832257483999914 ) ) ;
#3721 = EDGE_CURVE ( 'NONE', #3462, #50691, #23060, .T. ) ;
#3720 = CARTESIAN_POINT ( 'NONE',  ( -12.54983130239999944, -16.94901607458999848, -0.1356732392833999989 ) ) ;
#3722 = CARTESIAN_POINT ( 'NONE',  ( -10.59876350475000173, -77.50274337785998569, 7.550195564144000393 ) ) ;
#3723 = DIRECTION ( 'NONE',  ( 0.9999999999999694689, -2.469236814435925861E-07, -1.232399280382962518E-12 ) ) ;
#3724 = CARTESIAN_POINT ( 'NONE',  ( 1.318114156690387784, -24.73572477191089902, -12.70261578162881655 ) ) ;
#3725 = CARTESIAN_POINT ( 'NONE',  ( 0.7846939639768999442, -76.45140497417000347, 12.33726696821999802 ) ) ;
#3726 = ORIENTED_EDGE ( 'NONE', *, *, #52233, .F. ) ;
#3727 = CARTESIAN_POINT ( 'NONE',  ( -10.34138800174999950, -80.71754402778218207, 4.468208825537999473 ) ) ;
#3728 = CARTESIAN_POINT ( 'NONE',  ( 8.485281374238999419, -18.75000000000000000, 8.485281374238999419 ) ) ;
#3729 = CARTESIAN_POINT ( 'NONE',  ( -10.98964036629029195, -18.48475764895765039, -0.4777763868216057808 ) ) ;
#3730 = CARTESIAN_POINT ( 'NONE',  ( 10.50000000000000000, -81.99999999999998579, 0.000000000000000000 ) ) ;
#3731 = CARTESIAN_POINT ( 'NONE',  ( 6.193386186315999353, -78.21247639790598782, 7.375308638433999420 ) ) ;
#3732 = CARTESIAN_POINT ( 'NONE',  ( -4.137391094169000638, -84.74356301659899771, -0.5404326035545999884 ) ) ;
#3733 = CARTESIAN_POINT ( 'NONE',  ( -3.202240918582688334, -79.99931087886648129, 10.26207580309217349 ) ) ;
#3734 = CARTESIAN_POINT ( 'NONE',  ( -1.016909733597999965, -80.04133710082599862, 0.9879038282509999824 ) ) ;
#3735 = ORIENTED_EDGE ( 'NONE', *, *, #12317, .F. ) ;
#3736 = LINE ( 'NONE', #52187, #48479 ) ;
#3737 = CARTESIAN_POINT ( 'NONE',  ( -6.983600593180121052, -79.04328884231583174, 6.095355805603315247 ) ) ;
#3738 = EDGE_CURVE ( 'NONE', #21348, #27676, #1532, .T. ) ;
#3739 = CARTESIAN_POINT ( 'NONE',  ( 0.8501357521078367618, -78.91365707727138101, -3.816953471012215715 ) ) ;
#3740 = ORIENTED_EDGE ( 'NONE', *, *, #55612, .T. ) ;
#3741 = ORIENTED_EDGE ( 'NONE', *, *, #17449, .F. ) ;
#3742 = CARTESIAN_POINT ( 'NONE',  ( 10.70874647057999951, -79.10441578277699648, -2.238429218213000116 ) ) ;
#3743 = CARTESIAN_POINT ( 'NONE',  ( -7.997114030203776203, -55.11418618783218903, -7.553727747530986747 ) ) ;
#3744 = DIRECTION ( 'NONE',  ( 0.000000000000000000, 1.000000000000000000, 0.000000000000000000 ) ) ;
#3745 = VERTEX_POINT ( 'NONE', #48982 ) ;
#3746 = CIRCLE ( 'NONE', #19776, 0.5000000000000006661 ) ;
#3747 = ORIENTED_EDGE ( 'NONE', *, *, #22853, .F. ) ;
#3749 = EDGE_CURVE ( 'NONE', #52954, #37470, #40635, .T. ) ;
#3748 = EDGE_LOOP ( 'NONE', ( #37219, #7609 ) ) ;
#3750 = AXIS2_PLACEMENT_3D ( 'NONE', #2464, #29587, #47929 ) ;
#3751 = EDGE_CURVE ( 'NONE', #41331, #18799, #13852, .T. ) ;
#3752 = DIRECTION ( 'NONE',  ( -1.000000000000000000, 0.000000000000000000, 0.000000000000000000 ) ) ;
#3753 = CARTESIAN_POINT ( 'NONE',  ( 9.630577183392999174, -79.51334368717353129, 1.628483183780000010 ) ) ;
#3754 = ORIENTED_EDGE ( 'NONE', *, *, #55399, .F. ) ;
#3755 = CARTESIAN_POINT ( 'NONE',  ( 10.98362417419999915, -18.84999999999999787, 0.5999999999999999778 ) ) ;
#3756 = ORIENTED_EDGE ( 'NONE', *, *, #55347, .T. ) ;
#3757 = CARTESIAN_POINT ( 'NONE',  ( 0.8974734542577849084, -80.33735043314219126, -0.9053192546341672919 ) ) ;
#3758 = CARTESIAN_POINT ( 'NONE',  ( -2.347024683480479545, -78.91452044229970397, -3.892553587101836410 ) ) ;
#3759 = CARTESIAN_POINT ( 'NONE',  ( 7.986982684638000762, -54.07364722701999682, 10.07612755991999975 ) ) ;
#3760 = CARTESIAN_POINT ( 'NONE',  ( -0.5392637480170889841, -18.58467666638265925, 10.98678411023718482 ) ) ;
#3761 = CARTESIAN_POINT ( 'NONE',  ( 9.499178638196321245, -79.00092112126561972, 0.1004274591880019996 ) ) ;
#3762 = CARTESIAN_POINT ( 'NONE',  ( 1.283537837596413045, -80.98401907456398874, -11.03296757967288677 ) ) ;
#3763 = CARTESIAN_POINT ( 'NONE',  ( 7.718368845781999887, -58.54800977479000323, -10.07722254367000048 ) ) ;
#3764 = CARTESIAN_POINT ( 'NONE',  ( 4.100000000000000533, -81.79999999999998295, 0.000000000000000000 ) ) ;
#3765 = VECTOR ( 'NONE', #24119, 1000.000000000000000 ) ;
#3766 = CARTESIAN_POINT ( 'NONE',  ( 0.000000000000000000, -81.19999999999998863, 7.000000000000000000 ) ) ;
#3767 = CARTESIAN_POINT ( 'NONE',  ( 3.981833447626999423, -82.41750264934799475, 0.4016515649867999915 ) ) ;
#3768 = CARTESIAN_POINT ( 'NONE',  ( 9.685708259213999582, -77.51688667140099653, 1.223589504196999966 ) ) ;
#3769 = CARTESIAN_POINT ( 'NONE',  ( 0.9995835529977233902, -83.30208333333332860, 0.7681833999686461523 ) ) ;
#3770 = CARTESIAN_POINT ( 'NONE',  ( 10.48774103546000092, -20.24527981753999839, -7.686941364807000632 ) ) ;
#3771 = CARTESIAN_POINT ( 'NONE',  ( -8.987350104473000201, -76.93864821936499254, 8.369597699504998545 ) ) ;
#3772 = CARTESIAN_POINT ( 'NONE',  ( -1.149697912616226558, -81.29158079410925097, -0.6590062889063229568 ) ) ;
#3773 = CARTESIAN_POINT ( 'NONE',  ( 3.042547531669000271, -78.24783470746899638, -10.31045122763999977 ) ) ;
#3774 = CARTESIAN_POINT ( 'NONE',  ( 1.082313248930284022, -80.53554216430265456, -1.106039928096046898 ) ) ;
#3775 = CARTESIAN_POINT ( 'NONE',  ( -2.826502466506999767, -77.05760734133949086, -8.941232880334000654 ) ) ;
#3776 = CARTESIAN_POINT ( 'NONE',  ( -0.1356420093736999954, -78.02636455657749082, -1.608970710047999964 ) ) ;
#3777 = CARTESIAN_POINT ( 'NONE',  ( 7.714303428875997959, -15.69705297113999443, -12.53545825868000385 ) ) ;
#3778 = ADVANCED_FACE ( 'NONE', ( #29700 ), #29807, .T. ) ;
#3779 = AXIS2_PLACEMENT_3D ( 'NONE', #2104, #29513, #47568 ) ;
#3780 = CIRCLE ( 'NONE', #19821, 0.5000000000000006661 ) ;
#3781 = CARTESIAN_POINT ( 'NONE',  ( -0.8126767071385999630, -78.49313915747200099, -12.25297252704000073 ) ) ;
#3782 = CARTESIAN_POINT ( 'NONE',  ( -1.513302041219688123E-14, -80.75000000002938805, 13.94999999997000018 ) ) ;
#3783 = VECTOR ( 'NONE', #20875, 1000.000000000000000 ) ;
#3784 = CARTESIAN_POINT ( 'NONE',  ( -1.407171709420418138, -79.11458333333331439, -10.75000000000000000 ) ) ;
#3786 = CARTESIAN_POINT ( 'NONE',  ( 8.000000000000000000, -81.19999999999998863, 0.000000000000000000 ) ) ;
#3785 = CARTESIAN_POINT ( 'NONE',  ( 0.000000000000000000, -65.72928575305999743, 0.000000000000000000 ) ) ;
#3787 = CARTESIAN_POINT ( 'NONE',  ( 1.392666586335999934, -81.91902456270999267, 0.4657552147452999614 ) ) ;
#3788 = CARTESIAN_POINT ( 'NONE',  ( -5.583693648563480494, -79.51845993124416623, 9.199230099472547550 ) ) ;
#3789 = ORIENTED_EDGE ( 'NONE', *, *, #43267, .T. ) ;
#3790 = CARTESIAN_POINT ( 'NONE',  ( -6.745911349169845472, -78.82231418035541992, 9.981325353439961745 ) ) ;
#3791 = CARTESIAN_POINT ( 'NONE',  ( -11.34557120194999946, -79.21831925412799080, -4.033641907284000183 ) ) ;
#3792 = CARTESIAN_POINT ( 'NONE',  ( -3.008550086500999754, -80.47034076625139676, 10.63866553953000071 ) ) ;
#3793 = DIRECTION ( 'NONE',  ( -0.7071067811865475727, 0.000000000000000000, -0.7071067811865475727 ) ) ;
#3794 = CARTESIAN_POINT ( 'NONE',  ( -2.047671225339077468E-06, -76.25353340279926329, -10.79679441329301959 ) ) ;
#3795 = CARTESIAN_POINT ( 'NONE',  ( -2.173628335086999819, -1.116741823149000057, -2.792292937636999817 ) ) ;
#3796 = CARTESIAN_POINT ( 'NONE',  ( -0.2732314027492999675, -79.02031087269799059, 9.666450061188999854 ) ) ;
#3797 = DIRECTION ( 'NONE',  ( -1.000000000000000000, 0.000000000000000000, 0.000000000000000000 ) ) ;
#3798 = CARTESIAN_POINT ( 'NONE',  ( -1.799490225533999732, -59.57152778012000027, 12.64500484464999808 ) ) ;
#3799 = ORIENTED_EDGE ( 'NONE', *, *, #26920, .T. ) ;
#3800 = DIRECTION ( 'NONE',  ( 0.000000000000000000, -1.000000000000000000, 0.000000000000000000 ) ) ;
#3801 = DIRECTION ( 'NONE',  ( 0.000000000000000000, 0.000000000000000000, -1.000000000000000000 ) ) ;
#3802 = ADVANCED_FACE ( 'NONE', ( #42725 ), #11435, .T. ) ;
#3803 = CARTESIAN_POINT ( 'NONE',  ( -12.50679926050217006, -17.69581646372544981, 1.424414840279750072 ) ) ;
#3804 = CARTESIAN_POINT ( 'NONE',  ( -10.53003223722000037, -55.47547470607999998, -7.612971414697999428 ) ) ;
#3805 = EDGE_CURVE ( 'NONE', #41659, #29156, #12575, .T. ) ;
#3806 = CARTESIAN_POINT ( 'NONE',  ( -1.445929428138999828, -80.34746535818999291, 0.8273736140038000508 ) ) ;
#3807 = ORIENTED_EDGE ( 'NONE', *, *, #12414, .T. ) ;
#3808 = CONICAL_SURFACE ( 'NONE', #12328, 9.649999999909001147, 0.7853981633972997312 ) ;
#3809 = CARTESIAN_POINT ( 'NONE',  ( 0.000000000000000000, -82.50000000000000000, 0.000000000000000000 ) ) ;
#3810 = CARTESIAN_POINT ( 'NONE',  ( 3.042547531669000271, -78.24783470746899638, -10.31045122763999977 ) ) ;
#3811 = PLANE ( 'NONE',  #19518 ) ;
#3813 = EDGE_LOOP ( 'NONE', ( #29288, #38677, #38533, #27172 ) ) ;
#3812 = B_SPLINE_CURVE_WITH_KNOTS ( 'NONE', 3,
 ( #14647, #1684, #50694, #19674, #37674, #55692, #38255, #57926, #24688, #11699, #4201, #49075, #7547, #52140, #53498, #25547, #56278, #31039, #21903, #17483, #16411, #34100, #56561, #29675, #47148, #16122, #43565, #47725, #52426, #2264, #29963, #58220, #11985, #2548, #35470, #17783, #48013, #3899, #22199, #13041, #44647, #40210, #38837, #8625, #35773, #39912, #53801, #26611, #20551 ),
 .UNSPECIFIED., .F., .F.,
 ( 4, 2, 2, 2, 2, 2, 2, 2, 2, 2, 2, 2, 1, 2, 2, 2, 2, 1, 2, 2, 2, 2, 1, 2, 2, 4 ),
 ( 0.000000000000000000, 0.06250000000000033307, 0.09375000000000018041, 0.1093750000000004441, 0.1250000000000006939, 0.1875000000000002498, 0.2499999999999998057, 0.3124999999999993894, 0.3749999999999989453, 0.4374999999999985012, 0.4999999999999981126, 0.5624999999999976685, 0.5937499999999973355, 0.6093749999999968914, 0.6249999999999964473, 0.6874999999999957812, 0.7187499999999953371, 0.7343749999999952260, 0.7421874999999952260, 0.7499999999999951150, 0.8124999999999962252, 0.8437499999999966693, 0.8593749999999966693, 0.8671874999999966693, 0.8749999999999965583, 1.000000000000000000 ),
 .UNSPECIFIED. ) ;
#3814 = CARTESIAN_POINT ( 'NONE',  ( -12.69619287811999797, -58.55083378327000077, 1.799475295154000065 ) ) ;
#3815 = CARTESIAN_POINT ( 'NONE',  ( -9.395773752806999113, -54.09509747810999869, -8.188237371196001035 ) ) ;
#3816 = EDGE_CURVE ( 'NONE', #39245, #23213, #25284, .T. ) ;
#3817 = CARTESIAN_POINT ( 'NONE',  ( -2.217000330786000450, -79.16306993851199536, 9.512392227823999846 ) ) ;
#3818 = EDGE_LOOP ( 'NONE', ( #44014, #30984, #21174, #55691, #31758 ) ) ;
#3819 = VERTEX_POINT ( 'NONE', #57450 ) ;
#3820 = CARTESIAN_POINT ( 'NONE',  ( -9.039790932574998550, -77.13146751707299131, 8.418433967051999645 ) ) ;
#3821 = CARTESIAN_POINT ( 'NONE',  ( -10.53015523610255144, -78.61621378903457469, -2.164481121597691349 ) ) ;
#3822 = VECTOR ( 'NONE', #39882, 1000.000000000000000 ) ;
#3823 = ORIENTED_EDGE ( 'NONE', *, *, #25570, .F. ) ;
#3824 = CARTESIAN_POINT ( 'NONE',  ( 4.001451577097999923, -78.02955584965400249, 8.339717337904000161 ) ) ;
#3825 = AXIS2_PLACEMENT_3D ( 'NONE', #22605, #40616, #213 ) ;
#3826 = CARTESIAN_POINT ( 'NONE',  ( -9.669407782331445489, -77.85665777210621741, -0.8224238135324427601 ) ) ;
#3827 = DIRECTION ( 'NONE',  ( 0.000000000000000000, -1.000000000000000000, 0.000000000000000000 ) ) ;
#3828 = CARTESIAN_POINT ( 'NONE',  ( -9.650487694675000228, -78.53128649030999497, 7.043610823269999877 ) ) ;
#3829 = CARTESIAN_POINT ( 'NONE',  ( -6.884807209879997281, -78.32241137255587660, -8.855368954042999619 ) ) ;
#3830 = CARTESIAN_POINT ( 'NONE',  ( 13.13047446164998711, -19.21421830981000767, -0.8260994316375004365 ) ) ;
#3831 = CARTESIAN_POINT ( 'NONE',  ( -0.5518643889783007017, -86.36264283715698298, 4.438223277016744461 ) ) ;
#3832 = CARTESIAN_POINT ( 'NONE',  ( 4.782478426736999744, -79.74163131954000505, 10.14623135401999932 ) ) ;
#3833 = ADVANCED_FACE ( 'NONE', ( #6991 ), #43303, .F. ) ;
#3834 = B_SPLINE_CURVE_WITH_KNOTS ( 'NONE', 3,
 ( #38076, #37785, #55211, #14757, #32755, #55509, #51096, #6198, #50802, #10347, #33350, #7075, #8223, #17083, #7647, #34787, #35358, #35065 ),
 .UNSPECIFIED., .F., .F.,
 ( 4, 2, 2, 2, 2, 2, 2, 2, 4 ),
 ( 0.000000000000000000, 0.1249999999999999722, 0.2499999999999999445, 0.3749999999999998890, 0.4999999999999998890, 0.6249999999999998890, 0.7499999999999997780, 0.8749999999999998890, 1.000000000000000000 ),
 .UNSPECIFIED. ) ;
#3835 = CARTESIAN_POINT ( 'NONE',  ( 3.242578276031594875, -79.94660715946710638, 8.663862471309647262 ) ) ;
#3836 = CARTESIAN_POINT ( 'NONE',  ( 9.697390092220967261, -17.02767731352027525, 8.266602378556456188 ) ) ;
#3837 = ORIENTED_EDGE ( 'NONE', *, *, #36437, .T. ) ;
#3838 = CARTESIAN_POINT ( 'NONE',  ( -10.40633193566000081, -78.65210692446099472, -4.317081191017999586 ) ) ;
#3839 = CARTESIAN_POINT ( 'NONE',  ( 12.02702378446000075, -75.75855317818999879, -1.341316611471999876 ) ) ;
#3840 = CARTESIAN_POINT ( 'NONE',  ( 0.6275421466603999798, -80.57749471241899641, 1.160498354042999836 ) ) ;
#3841 = CARTESIAN_POINT ( 'NONE',  ( -0.5351185351402000245, -79.06629276448599342, 1.205899990410000067 ) ) ;
#3842 = CARTESIAN_POINT ( 'NONE',  ( -1.820508558488653783, -3.431062509705810726, -3.014547121651218298 ) ) ;
#3843 = CARTESIAN_POINT ( 'NONE',  ( -9.073547343531414455, -16.77191135192954619, 8.894853367293087842 ) ) ;
#3844 = DIRECTION ( 'NONE',  ( 0.000000000000000000, -0.7071067811866525998, -0.7071067811864425456 ) ) ;
#3845 = LINE ( 'NONE', #27142, #31714 ) ;
#3846 = CARTESIAN_POINT ( 'NONE',  ( -8.192247052095000370, -78.61632353800997919, -7.574872137178000564 ) ) ;
#3847 = DIRECTION ( 'NONE',  ( 0.000000000000000000, 1.000000000000000000, 0.000000000000000000 ) ) ;
#3848 = CARTESIAN_POINT ( 'NONE',  ( -0.8853410819279036170, -83.03830652476008822, 0.8818642663556593986 ) ) ;
#3849 = CARTESIAN_POINT ( 'NONE',  ( -4.071647054251999798, -81.73367725304099451, -0.9100801767057999925 ) ) ;
#3850 =( GEOMETRIC_REPRESENTATION_CONTEXT ( 3 ) GLOBAL_UNCERTAINTY_ASSIGNED_CONTEXT ( ( #34253 ) ) GLOBAL_UNIT_ASSIGNED_CONTEXT ( ( #26747, #50387, #27627 ) ) REPRESENTATION_CONTEXT ( 'NONE', 'WORKASPACE' ) );
#3851 = ORIENTED_EDGE ( 'NONE', *, *, #7318, .T. ) ;
#3852 = CARTESIAN_POINT ( 'NONE',  ( -1.388458563311000038, -81.85322848715999555, 0.7658850185041000680 ) ) ;
#3853 = CARTESIAN_POINT ( 'NONE',  ( -0.7917463127232000630, -80.03634392611000692, -1.236764296276999797 ) ) ;
#3854 = DIRECTION ( 'NONE',  ( 1.205798306211979422E-11, 1.868136817095964273E-07, -0.9999999999999824585 ) ) ;
#3855 = LINE ( 'NONE', #4444, #25802 ) ;
#3856 = EDGE_CURVE ( 'NONE', #55505, #22441, #47773, .T. ) ;
#3857 = LINE ( 'NONE', #30990, #48551 ) ;
#3858 = CARTESIAN_POINT ( 'NONE',  ( 0.6062141276560999437, -82.36581371194999690, -1.551696954864999922 ) ) ;
#3859 = CARTESIAN_POINT ( 'NONE',  ( -11.01904509677000021, -78.04521678053998812, 4.584337204197000304 ) ) ;
#3860 = CARTESIAN_POINT ( 'NONE',  ( 6.584508673715999905, -78.50595584965400064, 7.154582167228999978 ) ) ;
#3861 = CARTESIAN_POINT ( 'NONE',  ( 8.977320902561999105, -78.98328771936498072, 3.091814932086999868 ) ) ;
#3862 = CARTESIAN_POINT ( 'NONE',  ( -1.056237665594999875, -53.75133986268999564, -12.77256098193999989 ) ) ;
#3863 = CARTESIAN_POINT ( 'NONE',  ( 11.52879444111039753, -75.96520208080863767, 2.268419725861221981 ) ) ;
#3864 = CARTESIAN_POINT ( 'NONE',  ( -2.764837346329003687, -86.07389998728977787, 3.732097096069626474 ) ) ;
#3865 = ORIENTED_EDGE ( 'NONE', *, *, #30390, .T. ) ;
#3866 = CARTESIAN_POINT ( 'NONE',  ( 2.951189771924321192, -78.14999999999996305, 9.074256859245705797 ) ) ;
#3867 = CARTESIAN_POINT ( 'NONE',  ( 0.1963495408493571848, -79.26458333333334849, 1.500000000000000666 ) ) ;
#3868 = CARTESIAN_POINT ( 'NONE',  ( -2.750680930259973511, -78.80596977890112953, -11.46145582561345044 ) ) ;
#3869 = CARTESIAN_POINT ( 'NONE',  ( 11.59999999999999964, -87.70000000000000284, 0.000000000000000000 ) ) ;
#3870 = AXIS2_PLACEMENT_3D ( 'NONE', #39423, #57710, #3695 ) ;
#3871 = CARTESIAN_POINT ( 'NONE',  ( -4.277738290159001089, -79.02329186277498252, -10.10766895494000117 ) ) ;
#3872 = CARTESIAN_POINT ( 'NONE',  ( -1.980584515756000030, -18.73514849905999924, 12.76303204340999997 ) ) ;
#3873 = CARTESIAN_POINT ( 'NONE',  ( 12.30622754380999950, -76.18204548927899111, -1.412018855228999836 ) ) ;
#3874 = CARTESIAN_POINT ( 'NONE',  ( -0.1834469635243000107, -79.61327907013999550, -1.236465612773999911 ) ) ;
#3875 = DIRECTION ( 'NONE',  ( 0.000000000000000000, -1.000000000000000000, 0.000000000000000000 ) ) ;
#3876 = ORIENTED_EDGE ( 'NONE', *, *, #16713, .F. ) ;
#3877 = VECTOR ( 'NONE', #5772, 1000.000000000000000 ) ;
#3878 = CARTESIAN_POINT ( 'NONE',  ( 4.576365007000999796, -78.80017638237299593, -10.03785921918999868 ) ) ;
#3879 = CARTESIAN_POINT ( 'NONE',  ( -2.868749083076024498, -77.39991823718625596, 8.824073868535768028 ) ) ;
#3880 = CARTESIAN_POINT ( 'NONE',  ( 9.611650271896847286, -77.80833333333332291, -5.539808784079878201 ) ) ;
#3881 = CARTESIAN_POINT ( 'NONE',  ( -11.03994916103999913, -78.31013882934497872, -0.4443153950920000206 ) ) ;
#3882 = CARTESIAN_POINT ( 'NONE',  ( -10.75000000000000533, -76.49166666666666003, 1.125737367536309597 ) ) ;
#3883 = CARTESIAN_POINT ( 'NONE',  ( 9.377644441546999943, -78.13244088799798703, 7.928150093746000771 ) ) ;
#3884 = CARTESIAN_POINT ( 'NONE',  ( 9.502921960400678714, -17.25907999996281816, -8.179400289337134922 ) ) ;
#3885 = CARTESIAN_POINT ( 'NONE',  ( -10.75000000000000355, -78.48958333333331439, 1.407171709420384609 ) ) ;
#3886 = EDGE_CURVE ( 'NONE', #616, #8229, #9683, .T. ) ;
#3887 = CARTESIAN_POINT ( 'NONE',  ( -12.54976804508999955, -25.04775476228000031, -0.05637402076006000490 ) ) ;
#3888 = EDGE_LOOP ( 'NONE', ( #26253, #33918, #22380, #11114, #9128, #48558, #52479 ) ) ;
#3889 = ORIENTED_EDGE ( 'NONE', *, *, #43305, .T. ) ;
#3890 = CARTESIAN_POINT ( 'NONE',  ( 10.60216386470985839, -78.83683079414333861, -1.778172759129439395 ) ) ;
#3891 = VERTEX_POINT ( 'NONE', #7282 ) ;
#3892 = CARTESIAN_POINT ( 'NONE',  ( 6.688645397968000950, -78.88109438844000465, 10.27915892414000076 ) ) ;
#3893 = ORIENTED_EDGE ( 'NONE', *, *, #57288, .F. ) ;
#3894 = CARTESIAN_POINT ( 'NONE',  ( 7.618386461942000309, -23.22712559346000205, 10.53495196323000016 ) ) ;
#3895 = CARTESIAN_POINT ( 'NONE',  ( -6.481772035086000194, -76.64782152666799675, -8.784189910979000260 ) ) ;
#3896 = CARTESIAN_POINT ( 'NONE',  ( 4.299985066278999568, -78.96773998579799070, 8.680515821880000260 ) ) ;
#3897 = CARTESIAN_POINT ( 'NONE',  ( -3.528673621653970471, -78.19399569326179744, -8.550395938606023094 ) ) ;
#3898 = CARTESIAN_POINT ( 'NONE',  ( 8.645668071321999548, -78.50328462564201004, 7.146365085715999044 ) ) ;
#3899 = CARTESIAN_POINT ( 'NONE',  ( 0.9450683339454785115, -79.40746036129796437, 0.8222713226707200063 ) ) ;
#3900 = ADVANCED_FACE ( 'NONE', ( #38281 ), #30571, .T. ) ;
#3901 = VERTEX_POINT ( 'NONE', #47749 ) ;
#3902 = ORIENTED_EDGE ( 'NONE', *, *, #15168, .F. ) ;
#3903 = CARTESIAN_POINT ( 'NONE',  ( 1.394768719700775872, -77.46297058018842563, 9.144265183523252460 ) ) ;
#3904 = TOROIDAL_SURFACE ( 'NONE', #52017, 13.50000000000000000, 0.5000000000000000000 ) ;
#3905 = CARTESIAN_POINT ( 'NONE',  ( -1.996894868142000012, -77.19901894948809229, 10.85801781015000067 ) ) ;
#3906 = CARTESIAN_POINT ( 'NONE',  ( -9.500000000000001776, -77.41041666666667709, -1.243547092045959923 ) ) ;
#3907 = CIRCLE ( 'NONE', #45448, 4.299999999999999822 ) ;
#3908 = CARTESIAN_POINT ( 'NONE',  ( -7.843978203195000276, -77.84035887812699173, 5.713380375430999969 ) ) ;
#3909 = CARTESIAN_POINT ( 'NONE',  ( 6.215989686684999960, -76.16613641031999293, 11.19887415192999924 ) ) ;
#3910 = CARTESIAN_POINT ( 'NONE',  ( 2.880779477859606974, -2.210505338566499667, -1.557632211155396185 ) ) ;
#3911 = CARTESIAN_POINT ( 'NONE',  ( 7.712209501855907590, -54.73822238195494805, -10.27335463208971866 ) ) ;
#3912 = CARTESIAN_POINT ( 'NONE',  ( -10.55592303174000079, -79.83773888608898517, -3.904632140253000205 ) ) ;
#3913 = CARTESIAN_POINT ( 'NONE',  ( 12.43652237962999862, -17.07935153061999856, -0.1283967009857999997 ) ) ;
#3914 = CARTESIAN_POINT ( 'NONE',  ( -9.992017125381000398, -24.16084087012999859, -7.762968460669999793 ) ) ;
#3915 = CARTESIAN_POINT ( 'NONE',  ( -4.760969735703844741, -79.21703514507530031, 8.244157308523952565 ) ) ;
#3916 = EDGE_LOOP ( 'NONE', ( #20829, #55857, #38689, #5037, #28740, #25102 ) ) ;
#3917 = CARTESIAN_POINT ( 'NONE',  ( 8.190016797772999624, -79.75825050192599974, 9.199421104438000540 ) ) ;
#3918 = CARTESIAN_POINT ( 'NONE',  ( -8.252512830309999714, -53.86594982524999864, 9.650910120403001002 ) ) ;
#3919 = CARTESIAN_POINT ( 'NONE',  ( 7.483561698776000526, -78.52299011434399745, 9.354804580292000793 ) ) ;
#3920 = EDGE_CURVE ( 'NONE', #54465, #20866, #4378, .T. ) ;
#3921 = CARTESIAN_POINT ( 'NONE',  ( -12.70455691847952906, -61.36014620562671951, 1.489817752284223085 ) ) ;
#3923 = CARTESIAN_POINT ( 'NONE',  ( -1.484804496640999893, -17.28130846616999605, -12.77261165608999960 ) ) ;
#3922 = CARTESIAN_POINT ( 'NONE',  ( 7.654537165450999936, -55.51943464808999806, 10.01332852686999964 ) ) ;
#3924 = CARTESIAN_POINT ( 'NONE',  ( -1.247385798842000071, -54.32277743483000165, 12.50301438874000048 ) ) ;
#3925 = CARTESIAN_POINT ( 'NONE',  ( -10.86942385660000099, -80.59640203517098200, 3.442886605850000059 ) ) ;
#3926 = FACE_OUTER_BOUND ( 'NONE', #11696, .T. ) ;
#3927 = CARTESIAN_POINT ( 'NONE',  ( 0.5495723139228999576, -76.95229421267099212, -11.24864145460999865 ) ) ;
#3928 = DIRECTION ( 'NONE',  ( 1.000000000000000000, 0.000000000000000000, 0.000000000000000000 ) ) ;
#3929 = CARTESIAN_POINT ( 'NONE',  ( 4.329053196835999984, -80.47982502223689494, -10.39004403086999950 ) ) ;
#3930 = ORIENTED_EDGE ( 'NONE', *, *, #44181, .T. ) ;
#3931 = CARTESIAN_POINT ( 'NONE',  ( 13.49939038839240979, -46.09579702914000165, 0.1282931867975413143 ) ) ;
#3932 = DIRECTION ( 'NONE',  ( 0.000000000000000000, 0.000000000000000000, -1.000000000000000000 ) ) ;
#3933 = CARTESIAN_POINT ( 'NONE',  ( 7.686941364959000822, -21.75472017805000036, -10.48774103561000182 ) ) ;
#3934 = CARTESIAN_POINT ( 'NONE',  ( 1.455189730649000035, -1.703650774374000143, -3.167229696986999965 ) ) ;
#3935 = PRESENTATION_LAYER_ASSIGNMENT (  '', '', ( #5834 ) ) ;
#3936 = CARTESIAN_POINT ( 'NONE',  ( -0.4701581901367999916, -79.39978501252298315, 9.413031935884999868 ) ) ;
#3937 = CARTESIAN_POINT ( 'NONE',  ( 10.74983318585575631, -76.85537858145019641, 0.7036223827703862455 ) ) ;
#3938 = CARTESIAN_POINT ( 'NONE',  ( 10.19329140123695154, -77.31875000000002274, -4.224121120694948495 ) ) ;
#3939 = CARTESIAN_POINT ( 'NONE',  ( -7.958776492183998741, -24.47699850274999989, 9.723157982400998378 ) ) ;
#3940 = CARTESIAN_POINT ( 'NONE',  ( 12.54977952618000003, -16.95167110035999869, -0.03756586072996000170 ) ) ;
#3941 = CARTESIAN_POINT ( 'NONE',  ( 3.046345631554999933, -84.18624735065199616, 2.854711556928000160 ) ) ;
#3942 = DIRECTION ( 'NONE',  ( 0.000000000000000000, 1.000000000000000000, 0.000000000000000000 ) ) ;
#3943 = CARTESIAN_POINT ( 'NONE',  ( 11.94498200941940347, -77.21677916375155348, 2.095992703329072171 ) ) ;
#3944 = B_SPLINE_CURVE_WITH_KNOTS ( 'NONE', 3,
 ( #39115, #57121, #16687, #12252, #26681, #9281, #39976, #57990, #40576, #18437 ),
 .UNSPECIFIED., .F., .F.,
 ( 4, 2, 2, 2, 4 ),
 ( 0.000000000000000000, 0.2500000000000000555, 0.5000000000000003331, 0.7500000000000003331, 1.000000000000000000 ),
 .UNSPECIFIED. ) ;
#3945 = CARTESIAN_POINT ( 'NONE',  ( -11.10013370946000144, -76.70156662648800250, 1.020686637641000205 ) ) ;
#3946 = CARTESIAN_POINT ( 'NONE',  ( 0.8682910081118865309, -81.91446363364094907, 0.8987380763722911947 ) ) ;
#3947 = CARTESIAN_POINT ( 'NONE',  ( 0.07350186345039000368, -79.58564247267000269, -1.355733752427000116 ) ) ;
#3948 = CARTESIAN_POINT ( 'NONE',  ( -2.880544446985999762, -76.99112385945399240, -9.112186890989001142 ) ) ;
#3949 = CARTESIAN_POINT ( 'NONE',  ( 0.6752050339386822531, -83.08805329458888878, 1.352705552778453502 ) ) ;
#3950 = CIRCLE ( 'NONE', #26562, 5.000000000000000000 ) ;
#3951 = CARTESIAN_POINT ( 'NONE',  ( -12.82202361519000000, -60.22627773000999696, 2.066043355638000012 ) ) ;
#3952 = CARTESIAN_POINT ( 'NONE',  ( 4.121696569562778301, -80.25639609395949492, -9.928389259389652111 ) ) ;
#3953 = CARTESIAN_POINT ( 'NONE',  ( -6.606377239730330864, -77.07291666666667140, -8.596418555780440229 ) ) ;
#3954 = CARTESIAN_POINT ( 'NONE',  ( 7.561997864713030815, -75.80000000000001137, 9.323372221969927764 ) ) ;
#3955 = VERTEX_POINT ( 'NONE', #22303 ) ;
#3956 = DIRECTION ( 'NONE',  ( 0.000000000000000000, -1.000000000000000000, 0.000000000000000000 ) ) ;
#3957 = EDGE_CURVE ( 'NONE', #34611, #40996, #52472, .T. ) ;
#3958 = DIRECTION ( 'NONE',  ( -1.000000000000000000, 0.000000000000000000, 0.000000000000000000 ) ) ;
#3959 = CARTESIAN_POINT ( 'NONE',  ( 4.752670204043000446, -79.73108495741900015, 10.08299194199999960 ) ) ;
#3960 = LINE ( 'NONE', #21963, #22410 ) ;
#3961 = VERTEX_POINT ( 'NONE', #40013 ) ;
#3962 = ORIENTED_EDGE ( 'NONE', *, *, #50470, .T. ) ;
#3963 = ADVANCED_FACE ( 'NONE', ( #53311 ), #42106, .T. ) ;
#3964 = CARTESIAN_POINT ( 'NONE',  ( 1.478892026253000092, -81.20907286634400180, -0.6481452774650000581 ) ) ;
#3965 = ORIENTED_EDGE ( 'NONE', *, *, #54374, .T. ) ;
#3966 = PRESENTATION_STYLE_ASSIGNMENT (( #45008 ) ) ;
#3967 = VERTEX_POINT ( 'NONE', #31441 ) ;
#3968 = AXIS2_PLACEMENT_3D ( 'NONE', #18638, #45211, #14481 ) ;
#3969 = CARTESIAN_POINT ( 'NONE',  ( -9.254189652385859333, -79.87418719991859462, 5.469689899798553689 ) ) ;
#3970 = CARTESIAN_POINT ( 'NONE',  ( -5.305451056584999492, -79.72621204443500176, -9.672327717035999584 ) ) ;
#3971 = CARTESIAN_POINT ( 'NONE',  ( -3.140974612311351777, -76.40416666663691103, -11.68767212001978884 ) ) ;
#3972 = CARTESIAN_POINT ( 'NONE',  ( -0.05794900967641999218, -80.13320636806399477, 3.962654676452000757 ) ) ;
#3973 = CARTESIAN_POINT ( 'NONE',  ( -7.560040866215333111, -79.34781027512715923, 5.752875731716930119 ) ) ;
#3974 = ORIENTED_EDGE ( 'NONE', *, *, #11053, .T. ) ;
#3975 = DIRECTION ( 'NONE',  ( 1.000000000000000000, 0.000000000000000000, 0.000000000000000000 ) ) ;
#3977 = ADVANCED_FACE ( 'NONE', ( #13735 ), #58327, .T. ) ;
#3976 = CARTESIAN_POINT ( 'NONE',  ( 10.90767474025000006, -79.29456715226000085, 5.809805964757000396 ) ) ;
#3978 = ORIENTED_EDGE ( 'NONE', *, *, #53175, .F. ) ;
#3979 = ORIENTED_EDGE ( 'NONE', *, *, #12974, .T. ) ;
#3980 = CARTESIAN_POINT ( 'NONE',  ( 12.85144117164000122, -58.55472016995999951, -1.980464439859999981 ) ) ;
#3981 = CYLINDRICAL_SURFACE ( 'NONE', #54615, 10.75000000000000000 ) ;
#3982 = B_SPLINE_CURVE_WITH_KNOTS ( 'NONE', 3,
 ( #56228, #51228, #29626, #34052, #6039, #29339 ),
 .UNSPECIFIED., .F., .F.,
 ( 4, 1, 1, 4 ),
 ( 0.000000000000000000, 0.3333333311588953518, 0.6666666623178907347, 0.9999999934767860310 ),
 .UNSPECIFIED. ) ;
#3983 = CARTESIAN_POINT ( 'NONE',  ( 1.329937235669000017, -79.50973555599499321, -0.09921221311570001256 ) ) ;
#3984 = CARTESIAN_POINT ( 'NONE',  ( 9.367484565636001292, -78.93852241191899566, -2.533990228858999938 ) ) ;
#3985 = CARTESIAN_POINT ( 'NONE',  ( 3.518657424384936672, -86.36264283715698298, -1.566607219110143223 ) ) ;
#3986 = CARTESIAN_POINT ( 'NONE',  ( 0.4177217270225673240, -85.94664870426311154, 3.455032609703315494 ) ) ;
#3987 = CARTESIAN_POINT ( 'NONE',  ( 11.98112765039999950, -78.28893426687999124, 5.330601325896000553 ) ) ;
#3988 = CARTESIAN_POINT ( 'NONE',  ( -12.59654320151999940, -76.75108497556999509, -1.064070293361000008 ) ) ;
#3989 = CARTESIAN_POINT ( 'NONE',  ( 5.236819022057999540, -76.36164720732999456, 9.541811095419998168 ) ) ;
#3990 = CARTESIAN_POINT ( 'NONE',  ( -9.205306792771352775, -78.60791254279841667, -0.9089956325551382665 ) ) ;
#3991 = CARTESIAN_POINT ( 'NONE',  ( 3.939216039107999556, -82.66232476339300206, 0.3973570580265000651 ) ) ;
#3992 = AXIS2_PLACEMENT_3D ( 'NONE', #18534, #27370, #28237 ) ;
#3993 = CARTESIAN_POINT ( 'NONE',  ( -10.53101998745000145, -55.49360374314999689, 7.613962827161000035 ) ) ;
#3994 = CARTESIAN_POINT ( 'NONE',  ( -0.7135609970306604488, -2.993047182741839229, 3.178329152650583023 ) ) ;
#3995 = CARTESIAN_POINT ( 'NONE',  ( -2.689955776593000003, -81.68442549782599826, -2.376525467545999692 ) ) ;
#3996 = FACE_OUTER_BOUND ( 'NONE', #48852, .T. ) ;
#3997 = CARTESIAN_POINT ( 'NONE',  ( 11.02326530841000007, -81.16017192083839404, 1.187788371667000131 ) ) ;
#3998 = CARTESIAN_POINT ( 'NONE',  ( 1.432628882339999965, -2.403710179781999745, -3.526139092948999743 ) ) ;
#3999 = CARTESIAN_POINT ( 'NONE',  ( 1.058402703809858236, -79.54706147304830210, 0.7107250344689944876 ) ) ;
#4000 = VERTEX_POINT ( 'NONE', #22604 ) ;
#4001 = CARTESIAN_POINT ( 'NONE',  ( 0.5392637480170930919, -23.41532333362685847, 10.98678411023718304 ) ) ;
#4002 = DIRECTION ( 'NONE',  ( -1.776356839400000238E-14, -1.000000000000000000, 8.585724723767000453E-14 ) ) ;
#4003 = CARTESIAN_POINT ( 'NONE',  ( -0.6509962010243000030, -81.63746790025000166, 1.163950211895000031 ) ) ;
#4004 = CARTESIAN_POINT ( 'NONE',  ( -7.941500096889264171, -78.94666666666665833, -5.274086223140034058 ) ) ;
#4005 = CARTESIAN_POINT ( 'NONE',  ( 5.647598101448999763, -77.82194253125999239, 11.72364604052000203 ) ) ;
#4006 = EDGE_CURVE ( 'NONE', #11264, #30476, #40318, .T. ) ;
#4007 = CARTESIAN_POINT ( 'NONE',  ( -10.21026636381520625, -61.05606635916441149, -7.764233071732244085 ) ) ;
#4008 = CARTESIAN_POINT ( 'NONE',  ( 10.03847181070773331, -18.20634590497699179, 7.678636148852304721 ) ) ;
#4009 = ORIENTED_EDGE ( 'NONE', *, *, #33603, .T. ) ;
#4010 = DIRECTION ( 'NONE',  ( 0.000000000000000000, 0.000000000000000000, 1.000000000000000000 ) ) ;
#4011 = CARTESIAN_POINT ( 'NONE',  ( 5.626087561713998930, -77.01161118349268975, 9.492708140575000897 ) ) ;
#4012 = CARTESIAN_POINT ( 'NONE',  ( 1.267480381879000140, -81.47145997305000265, -0.3336381545036999907 ) ) ;
#4013 = CARTESIAN_POINT ( 'NONE',  ( -3.140974612311352221, -79.00416666666664867, -11.68767212001979061 ) ) ;
#4014 = CARTESIAN_POINT ( 'NONE',  ( 5.816771686847000744, -78.13423299304498926, -7.538935161885000014 ) ) ;
#4015 = CARTESIAN_POINT ( 'NONE',  ( -2.666500435283000403, -84.50306218606498021, 3.209337609828999849 ) ) ;
#4016 = CARTESIAN_POINT ( 'NONE',  ( -1.799490220168999954, -59.57129148919000272, -12.64502302236999931 ) ) ;
#4017 = CARTESIAN_POINT ( 'NONE',  ( -1.327188084842999993, -79.09869725658599293, 0.06657717027841000834 ) ) ;
#4018 = ORIENTED_EDGE ( 'NONE', *, *, #5557, .F. ) ;
#4019 = B_SPLINE_CURVE_WITH_KNOTS ( 'NONE', 3,
 ( #45882, #23712, #5414, #41434, #1020, #1300, #41722, #19001, #55009, #14847, #32841, #51763, #38160, #11314, #56183, #34591, #3031, #29295 ),
 .UNSPECIFIED., .F., .F.,
 ( 4, 2, 2, 2, 2, 2, 2, 2, 4 ),
 ( 0.000000000000000000, 0.1250000000000000000, 0.2500000000000000000, 0.3750000000000000000, 0.5000000000000000000, 0.6250000000000000000, 0.7500000000000000000, 0.8750000000000000000, 1.000000000000000000 ),
 .UNSPECIFIED. ) ;
#4020 = CARTESIAN_POINT ( 'NONE',  ( 7.615030601986474856, -77.28781258845663160, -7.587605221805258537 ) ) ;
#4021 = CARTESIAN_POINT ( 'NONE',  ( -0.6565412214492993837, -82.19791666666498031, 1.137416565959658232 ) ) ;
#4022 = CARTESIAN_POINT ( 'NONE',  ( 0.8592843842366197915, -78.91394566548676437, -3.814601581028083555 ) ) ;
#4023 = ORIENTED_EDGE ( 'NONE', *, *, #56145, .T. ) ;
#4024 = VERTEX_POINT ( 'NONE', #21720 ) ;
#4025 = CARTESIAN_POINT ( 'NONE',  ( -7.579884289019999777, -79.80672464109399300, 7.888812675972000754 ) ) ;
#4026 = CARTESIAN_POINT ( 'NONE',  ( 0.000000000000000000, -0.2000000000000000111, 0.000000000000000000 ) ) ;
#4027 = CARTESIAN_POINT ( 'NONE',  ( 7.164651402987000317, -80.12745930235598735, 8.777043346749001884 ) ) ;
#4028 = ORIENTED_EDGE ( 'NONE', *, *, #48091, .F. ) ;
#4029 = EDGE_CURVE ( 'NONE', #22857, #41402, #6281, .T. ) ;
#4030 = CARTESIAN_POINT ( 'NONE',  ( -7.209427067528999977, -77.61717634323900938, 9.655047023863000177 ) ) ;
#4031 = ORIENTED_EDGE ( 'NONE', *, *, #34935, .T. ) ;
#4032 = VERTEX_POINT ( 'NONE', #212 ) ;
#4033 = CIRCLE ( 'NONE', #5942, 1.000000000000000000 ) ;
#4034 = CARTESIAN_POINT ( 'NONE',  ( 11.61765826232213250, -76.62845391823577756, -3.111680234998253525 ) ) ;
#4035 = CARTESIAN_POINT ( 'NONE',  ( -1.184050902616055501, -1.449062058922204965, -3.841969317884664559 ) ) ;
#4036 = B_SPLINE_SURFACE_WITH_KNOTS ( 'NONE', 3, 3, ( 
 ( #40112, #48696, #58125, #17687 ),
 ( #44848, #8240, #4402, #17988 ),
 ( #45152, #4704, #22701, #57254 ),
 ( #54590, #36857, #51046, #27990 ),
 ( #46039, #15002, #36569, #37441 ),
 ( #879, #27412, #5563, #14129 ),
 ( #50166, #45744, #32999, #19153 ),
 ( #23286, #41296, #27701, #18865 ) ),
 .UNSPECIFIED., .F., .F., .F.,
 ( 4, 1, 1, 1, 1, 4 ),
 ( 4, 4 ),
 ( -0.01200407347462999902, 0.000000000000000000, 0.3333333333333000081, 0.6666666666667000474, 1.000000000000000000, 1.011997855551999947 ),
 ( -0.3559705542741999906, 1.355970554273999928 ),
 .UNSPECIFIED. ) ;
#4037 = ORIENTED_EDGE ( 'NONE', *, *, #20942, .F. ) ;
#4039 = EDGE_CURVE ( 'NONE', #40109, #10164, #49176, .T. ) ;
#4038 = CARTESIAN_POINT ( 'NONE',  ( 8.838834764832000701, -60.04999999966999980, 8.838834764832000701 ) ) ;
#4040 = ORIENTED_EDGE ( 'NONE', *, *, #46328, .F. ) ;
#4041 = DIRECTION ( 'NONE',  ( 0.000000000000000000, -1.000000000000000000, 0.000000000000000000 ) ) ;
#4042 = CARTESIAN_POINT ( 'NONE',  ( 3.407095545933000125, -78.77851879815550262, -2.010777145231034346 ) ) ;
#4043 = VECTOR ( 'NONE', #9762, 1000.000000000000000 ) ;
#4044 = LINE ( 'NONE', #45094, #2011 ) ;
#4045 = CARTESIAN_POINT ( 'NONE',  ( -7.642160924884000117, -19.21538333566000034, -10.55911395187000146 ) ) ;
#4046 = DIRECTION ( 'NONE',  ( 0.9999999923520045408, 0.000000000000000000, 0.0001236769620553006580 ) ) ;
#4047 = AXIS2_PLACEMENT_3D ( 'NONE', #20871, #33573, #34141 ) ;
#4048 = CARTESIAN_POINT ( 'NONE',  ( 11.75000000000000355, -76.54297251775334132, -1.037641870170386005 ) ) ;
#4049 = CARTESIAN_POINT ( 'NONE',  ( 11.20799393363000185, -77.92872135264997269, 4.230477091134000389 ) ) ;
#4050 = DIRECTION ( 'NONE',  ( 0.000000000000000000, 1.000000000000000000, 0.000000000000000000 ) ) ;
#4051 = CARTESIAN_POINT ( 'NONE',  ( -9.835223439032999337, -24.08138927656000305, 7.760980897158999525 ) ) ;
#4052 = CARTESIAN_POINT ( 'NONE',  ( 0.7554284705563509839, -80.06666666666669130, -1.310679582531386167 ) ) ;
#4053 = CARTESIAN_POINT ( 'NONE',  ( -1.405170778590000058, -82.00555496681198520, -3.928813311532000530 ) ) ;
#4054 = CARTESIAN_POINT ( 'NONE',  ( 6.922694868096999521, -76.94662000473400099, -6.559930598350000253 ) ) ;
#4055 = CARTESIAN_POINT ( 'NONE',  ( -1.250000000000000000, -83.49999999999998579, 0.000000000000000000 ) ) ;
#4056 = CARTESIAN_POINT ( 'NONE',  ( 12.76303204294999993, -23.26485150694999859, -1.980584515756000030 ) ) ;
#4057 = CARTESIAN_POINT ( 'NONE',  ( 1.044910384896000188, -25.05526494194999643, 12.77260826199000121 ) ) ;
#4058 = CARTESIAN_POINT ( 'NONE',  ( 0.6416220162505898994, -80.91538276820625697, -1.159482954178659320 ) ) ;
#4059 = DIRECTION ( 'NONE',  ( 0.000000000000000000, 0.000000000000000000, -1.000000000000000000 ) ) ;
#4060 = CARTESIAN_POINT ( 'NONE',  ( 2.583538554219000360, -1.367443126209999971, 2.539878903945000044 ) ) ;
#4061 = CARTESIAN_POINT ( 'NONE',  ( -3.948661938011531092, -79.74013365314458213, -8.441925471967053340 ) ) ;
#4062 = CARTESIAN_POINT ( 'NONE',  ( 1.330394425097165323, -80.05981249656014143, -0.7208325465702845047 ) ) ;
#4063 = CARTESIAN_POINT ( 'NONE',  ( -0.9441204537501906024, -78.54342336913121869, 0.8192162103976715626 ) ) ;
#4064 = FACE_OUTER_BOUND ( 'NONE', #50399, .T. ) ;
#4065 = AXIS2_PLACEMENT_3D ( 'NONE', #53827, #9246, #13362 ) ;
#4066 = CARTESIAN_POINT ( 'NONE',  ( -12.51072239526000196, -15.69705297114000331, 0.7871079366006996647 ) ) ;
#4067 = CARTESIAN_POINT ( 'NONE',  ( -8.418448289622000758, -78.08151106797200214, -6.950186643912999784 ) ) ;
#4068 = EDGE_CURVE ( 'NONE', #26175, #36059, #53606, .T. ) ;
#4069 = CARTESIAN_POINT ( 'NONE',  ( -1.881092013513000039, -77.76064764102999050, 12.13496073407999987 ) ) ;
#4070 = CYLINDRICAL_SURFACE ( 'NONE', #37281, 1.750000000000001332 ) ;
#4072 = CARTESIAN_POINT ( 'NONE',  ( -1.344169958103999862, -78.81440746632799232, 0.7015335173854999606 ) ) ;
#4071 = DIRECTION ( 'NONE',  ( -0.7071067811865474617, 0.000000000000000000, 0.7071067811865474617 ) ) ;
#4073 = CARTESIAN_POINT ( 'NONE',  ( 1.614964347157999747, -82.04565794024999548, 0.5400991692461000193 ) ) ;
#4074 = SHAPE_REPRESENTATION ( 'Security screw', ( #43526 ), #6767 ) ;
#4075 = ORIENTED_EDGE ( 'NONE', *, *, #32990, .T. ) ;
#4076 = EDGE_CURVE ( 'NONE', #13840, #8528, #52658, .T. ) ;
#4077 = CARTESIAN_POINT ( 'NONE',  ( -1.092232985442822102, -82.04166666666664298, -0.6295237254636245616 ) ) ;
#4078 = CIRCLE ( 'NONE', #22929, 14.00000000000000000 ) ;
#4079 = CARTESIAN_POINT ( 'NONE',  ( -11.88541927438999934, -79.62999754497099048, -0.9862366044713999358 ) ) ;
#4080 = CARTESIAN_POINT ( 'NONE',  ( -9.997577002847000571, -80.67795857467889675, -4.987204589701000224 ) ) ;
#4081 = DIRECTION ( 'NONE',  ( 0.000000000000000000, -1.000000000000000000, 0.000000000000000000 ) ) ;
#4082 = FACE_BOUND ( 'NONE', #6449, .T. ) ;
#4083 = CARTESIAN_POINT ( 'NONE',  ( 0.5473670387515998659, -76.96277908592900019, -11.20350390113000039 ) ) ;
#4084 = CARTESIAN_POINT ( 'NONE',  ( -10.36222489920000100, -60.02120223818999989, 7.631889817968999346 ) ) ;
#4085 = CARTESIAN_POINT ( 'NONE',  ( -12.50000000000000000, -28.92928575306000383, 0.000000000000000000 ) ) ;
#4086 = CARTESIAN_POINT ( 'NONE',  ( 2.799999999999999822, -78.69999999999998863, 0.000000000000000000 ) ) ;
#4087 = CARTESIAN_POINT ( 'NONE',  ( -4.615667697956999938, -79.05765853095599027, 8.497672865486000759 ) ) ;
#4088 = DIRECTION ( 'NONE',  ( 0.000000000000000000, 0.000000000000000000, -1.000000000000000000 ) ) ;
#4089 = FACE_OUTER_BOUND ( 'NONE', #55085, .T. ) ;
#4090 = ORIENTED_EDGE ( 'NONE', *, *, #42289, .T. ) ;
#4091 = DIRECTION ( 'NONE',  ( 0.000000000000000000, 1.000000000000000000, 0.000000000000000000 ) ) ;
#4092 = CARTESIAN_POINT ( 'NONE',  ( -12.65372179309999900, -57.04935286341999756, 1.750000000000000000 ) ) ;
#4093 = CARTESIAN_POINT ( 'NONE',  ( -12.52133763471513639, -18.07246868480434898, 1.618901767043031681 ) ) ;
#4094 = VECTOR ( 'NONE', #4091, 1000.000000000000000 ) ;
#4095 = CARTESIAN_POINT ( 'NONE',  ( -10.07722254367000048, -58.54800977479000323, -7.718368845781999887 ) ) ;
#4096 = CARTESIAN_POINT ( 'NONE',  ( -2.902373257307000021, -86.03492953870899385, 2.039717538649000073 ) ) ;
#4097 = DIRECTION ( 'NONE',  ( 0.000000000000000000, -1.000000000000000000, 0.000000000000000000 ) ) ;
#4098 = ORIENTED_EDGE ( 'NONE', *, *, #31074, .F. ) ;
#4099 = CARTESIAN_POINT ( 'NONE',  ( 5.272298825061000116, -77.59356652213799066, -9.769775999529000998 ) ) ;
#4100 = CARTESIAN_POINT ( 'NONE',  ( -3.044724405606854756, -77.80247681429408146, -11.37341351363359543 ) ) ;
#4101 = CARTESIAN_POINT ( 'NONE',  ( -2.598917237794085455, -1.052083333333333481, -1.997276839918474600 ) ) ;
#4102 = VERTEX_POINT ( 'NONE', #22007 ) ;
#4103 = ORIENTED_EDGE ( 'NONE', *, *, #33823, .T. ) ;
#4104 = CARTESIAN_POINT ( 'NONE',  ( -12.58338334669999981, -58.54800977479000323, 1.667961445601999992 ) ) ;
#4105 = CARTESIAN_POINT ( 'NONE',  ( -7.636247231009999581, -55.03676232846999739, -10.30460520059999929 ) ) ;
#4106 = CARTESIAN_POINT ( 'NONE',  ( 3.269429986698999979, -79.61768715412398478, 9.203886808668999109 ) ) ;
#4107 = ORIENTED_EDGE ( 'NONE', *, *, #58364, .T. ) ;
#4108 = ORIENTED_EDGE ( 'NONE', *, *, #3507, .T. ) ;
#4110 = EDGE_CURVE ( 'NONE', #37084, #11057, #57183, .T. ) ;
#4109 = CARTESIAN_POINT ( 'NONE',  ( 8.222285421689999652, -77.37736394690199404, -8.489546592527000612 ) ) ;
#4111 = CARTESIAN_POINT ( 'NONE',  ( -10.50169165321555553, -78.61722614632127204, -2.300187871545900098 ) ) ;
#4112 = CARTESIAN_POINT ( 'NONE',  ( 0.3277382951148000156, -78.62904613799999254, 1.615386606358000243 ) ) ;
#4113 = EDGE_CURVE ( 'NONE', #46129, #20252, #495, .T. ) ;
#4114 = ORIENTED_EDGE ( 'NONE', *, *, #9647, .F. ) ;
#4115 = CARTESIAN_POINT ( 'NONE',  ( -7.264520526674999701, -77.74583084965399848, -6.114261184555999762 ) ) ;
#4116 = CARTESIAN_POINT ( 'NONE',  ( -9.497876546326999403, -77.35168256874098347, -0.2008509664869000122 ) ) ;
#4117 = CARTESIAN_POINT ( 'NONE',  ( 1.249621755023126113, -80.34836072372822002, -0.03568039317074558903 ) ) ;
#4118 = CARTESIAN_POINT ( 'NONE',  ( 11.88773275212999891, -76.77906641171999524, 5.537155082298999886 ) ) ;
#4119 = CARTESIAN_POINT ( 'NONE',  ( 9.668944085725000193, -77.04230325147001679, 5.685915129398998680 ) ) ;
#4120 = CARTESIAN_POINT ( 'NONE',  ( 0.000000000000000000, -76.29999999999999716, 0.000000000000000000 ) ) ;
#4121 = CARTESIAN_POINT ( 'NONE',  ( 3.576074390005824721, -86.31452044229999387, -1.592170899228392944 ) ) ;
#4122 = CIRCLE ( 'NONE', #44680, 1.250000000000000000 ) ;
#4123 = CARTESIAN_POINT ( 'NONE',  ( -10.39759693597000023, -79.93228572055228653, -4.208097972746998927 ) ) ;
#4124 = CARTESIAN_POINT ( 'NONE',  ( 1.356865283789024712, -79.96379466601229069, 9.149687343425433994 ) ) ;
#4125 = CARTESIAN_POINT ( 'NONE',  ( -10.74912230115235801, -80.44221474356261581, 1.099349670086620989 ) ) ;
#4126 = VERTEX_POINT ( 'NONE', #9031 ) ;
#4127 = CARTESIAN_POINT ( 'NONE',  ( -5.907589619820999616, -78.53973750712998481, 9.593191298321000815 ) ) ;
#4128 = B_SPLINE_CURVE_WITH_KNOTS ( 'NONE', 3,
 ( #5350, #6218, #1520, #19812, #665, #54658, #14490, #23644, #18651, #5065, #36639, #23062, #19514, #28353, #14198, #33071, #37509, #41369, #15074, #32483, #46698, #23358, #41075, #5927, #1815, #23932, #27772, #24233, #55527, #32195, #41951, #41657, #55231, #952, #51116, #10670, #50236, #36926, #50527, #9784, #28648, #14778, #28942, #42251, #15377, #37805, #55825, #33370, #45814, #18936, #54940, #10082, #28062, #46108, #1236, #19225, #11818, #25095, #43118, #20954, #38095, #56116, #38671, #46985, #29793 ),
 .UNSPECIFIED., .F., .F.,
 ( 4, 1, 1, 1, 1, 1, 1, 1, 1, 1, 1, 1, 1, 1, 1, 1, 1, 1, 1, 1, 1, 1, 1, 1, 1, 1, 1, 1, 1, 1, 1, 1, 1, 1, 1, 1, 1, 1, 1, 1, 1, 1, 1, 1, 1, 1, 1, 1, 1, 1, 1, 1, 1, 1, 1, 1, 1, 1, 1, 1, 1, 1, 4 ),
 ( 0.000000000000000000, 0.01249975014491727481, 0.02874975858096980377, 0.04499976701702233101, 0.06124977545307485477, 0.07749978388912738547, 0.09374979232517990924, 0.1099998007612324469, 0.1262498091972849568, 0.1424998176333374944, 0.1587498260693900320, 0.1749998345054425419, 0.1912498429414950796, 0.2074998513775475895, 0.2237498598136001271, 0.2399998682496526647, 0.2562498766857052024, 0.2724998851217577678, 0.2887498935578102777, 0.3049999019938627876, 0.3212499104299152974, 0.3374999188659678628, 0.3537499273020203727, 0.3699999357380729381, 0.3862499441741254480, 0.4024999526101780134, 0.4187499610462305233, 0.4349999694822830332, 0.4512499779183355431, 0.4674999863543881085, 0.4837499947904406183, 0.5000000032264931837, 0.5162500116625455826, 0.5325000200985980925, 0.5487500285346506024, 0.5650000369707031123, 0.5812500454067557332, 0.5975000538428082431, 0.6137500622788607529, 0.6300000707149132628, 0.6462500791509657727, 0.6625000875870183936, 0.6787500960230709035, 0.6950001044591234134, 0.7112501128951760343, 0.7275001213312285442, 0.7437501297672810541, 0.7600001382033335640, 0.7762501466393860738, 0.7925001550754385837, 0.8087501635114910936, 0.8250001719475436035, 0.8412501803835962244, 0.8575001888196487343, 0.8737501972557012442, 0.8900002056917537541, 0.9062502141278062640, 0.9225002225638587738, 0.9387502309999112837, 0.9550002394359637936, 0.9712502478720163035, 0.9875002563080689244, 1.000000000000000000 ),
 .UNSPECIFIED. ) ;
#4129 = CARTESIAN_POINT ( 'NONE',  ( -6.282410744257000523, -75.93495447697000600, 10.58616248715999930 ) ) ;
#4130 = CARTESIAN_POINT ( 'NONE',  ( -1.211530263941000163, -79.85058255474299926, 1.067430724879000037 ) ) ;
#4131 = B_SPLINE_CURVE_WITH_KNOTS ( 'NONE', 3,
 ( #47897, #47029, #25140, #56159, #7429, #6559, #34565, #47615, #11581, #7139, #25432, #56740, #12148, #20434, #43166, #7717, #43447, #24567, #3008, #21004, #20719, #2431, #15420 ),
 .UNSPECIFIED., .F., .F.,
 ( 4, 2, 2, 2, 1, 1, 1, 2, 2, 2, 2, 2, 4 ),
 ( 0.000000000000000000, 0.2499999999999713007, 0.3749999999999568678, 0.4374999999999500955, 0.4687499999999468758, 0.4843749999999452105, 0.4921874999999448219, 0.4960937499999449884, 0.4999999999999451550, 0.6249999999999588107, 0.7499999999999724665, 0.8749999999999862332, 1.000000000000000000 ),
 .UNSPECIFIED. ) ;
#4132 = CARTESIAN_POINT ( 'NONE',  ( -0.6498089757737999239, -78.07404029686399838, 1.148178518287000127 ) ) ;
#4133 = CIRCLE ( 'NONE', #14501, 1.000000000000000000 ) ;
#4134 = CARTESIAN_POINT ( 'NONE',  ( -2.913600672515707757, -2.800140272586570500, 2.082966609014084813 ) ) ;
#4135 = EDGE_CURVE ( 'NONE', #8528, #52835, #23749, .T. ) ;
#4136 = CARTESIAN_POINT ( 'NONE',  ( 12.50385602700769994, -54.01562691795769666, -0.8579623876370696678 ) ) ;
#4137 = CARTESIAN_POINT ( 'NONE',  ( -11.38972971424999869, -76.73218649614399567, -4.593112662244999811 ) ) ;
#4138 = CYLINDRICAL_SURFACE ( 'NONE', #33583, 10.75000000000000000 ) ;
#4139 = CARTESIAN_POINT ( 'NONE',  ( 10.92153517268999963, -79.29054004199397809, -2.282908042080999955 ) ) ;
#4140 = CARTESIAN_POINT ( 'NONE',  ( -9.504662724600999368, -76.89676498579798647, -2.115138623684999608 ) ) ;
#4141 = CARTESIAN_POINT ( 'NONE',  ( 10.21381326473999884, -19.22870851082999977, -7.668949790020999302 ) ) ;
#4142 = CARTESIAN_POINT ( 'NONE',  ( 10.47020627418439531, -79.72916666666665719, -2.813789756862242974 ) ) ;
#4143 = CARTESIAN_POINT ( 'NONE',  ( -1.780884232981000181, -79.86231230381177681, -11.07459082487999957 ) ) ;
#4144 = DIRECTION ( 'NONE',  ( -1.000000000000000000, 0.000000000000000000, 0.000000000000000000 ) ) ;
#4145 = ORIENTED_EDGE ( 'NONE', *, *, #53630, .T. ) ;
#4146 = CARTESIAN_POINT ( 'NONE',  ( 1.420454834158999979, -81.72706753059999585, 0.3724989704330000095 ) ) ;
#4147 = CARTESIAN_POINT ( 'NONE',  ( 0.9992737233374668904, -78.79819669903726265, -0.7680393074100418938 ) ) ;
#4148 = DIRECTION ( 'NONE',  ( 0.000000000000000000, 0.000000000000000000, -1.000000000000000000 ) ) ;
#4149 = CARTESIAN_POINT ( 'NONE',  ( -7.000000000000000000, -81.10000000285099020, 0.000000000000000000 ) ) ;
#4150 = CARTESIAN_POINT ( 'NONE',  ( 5.602396075985502932, -76.95000000000000284, -7.708428217489914580 ) ) ;
#4151 = CARTESIAN_POINT ( 'NONE',  ( 1.541440768196999933, -82.55134846604198628, 0.6318380856084999664 ) ) ;
#4152 = CARTESIAN_POINT ( 'NONE',  ( -9.654076420390000024, -78.12660472681200474, -7.016716533807999312 ) ) ;
#4153 = CARTESIAN_POINT ( 'NONE',  ( -5.600962501326000265, -77.99379805011500366, 7.948110234177999445 ) ) ;
#4154 = CARTESIAN_POINT ( 'NONE',  ( -7.400482488103000023, -78.65167637952700375, 6.163283938603000500 ) ) ;
#4155 = CARTESIAN_POINT ( 'NONE',  ( -9.689272046653734094, -24.97888144173617775, -8.274769670417640555 ) ) ;
#4156 = CARTESIAN_POINT ( 'NONE',  ( -10.07627163191000008, -18.75000000310999937, -7.601397897754999633 ) ) ;
#4157 = CARTESIAN_POINT ( 'NONE',  ( -3.677663026310137084, -86.02148118236289065, 1.555017880480947801 ) ) ;
#4158 = ORIENTED_EDGE ( 'NONE', *, *, #55225, .T. ) ;
#4159 = ADVANCED_FACE ( 'NONE', ( #10788 ), #27888, .T. ) ;
#4160 = CARTESIAN_POINT ( 'NONE',  ( -8.872994237323279521, -78.27000000000003865, 3.510218210012939100 ) ) ;
#4161 = CARTESIAN_POINT ( 'NONE',  ( -1.638273008393710262, -2.184753700216213179, -2.842570767342633697 ) ) ;
#4162 = CARTESIAN_POINT ( 'NONE',  ( -11.30034656532730430, -78.72488567633864420, -3.687091655504522336 ) ) ;
#4163 = AXIS2_PLACEMENT_3D ( 'NONE', #10976, #52562, #47288 ) ;
#4164 = CARTESIAN_POINT ( 'NONE',  ( 2.148673102446170713, -78.39678895079168797, -3.720415885850087534 ) ) ;
#4165 = CARTESIAN_POINT ( 'NONE',  ( -1.324613189995999862, -83.36847537123300356, -0.7038465009425000085 ) ) ;
#4166 = CARTESIAN_POINT ( 'NONE',  ( -5.751434148371999733, -77.91605109099198501, -9.630115047516998317 ) ) ;
#4167 = CARTESIAN_POINT ( 'NONE',  ( -10.81649518602000093, -79.41658482343198955, 1.862108609190000097 ) ) ;
#4168 = CARTESIAN_POINT ( 'NONE',  ( -1.495357591770747341, -17.44123662637707994, 12.70444646759436047 ) ) ;
#4169 = CARTESIAN_POINT ( 'NONE',  ( -11.24870262279999977, -76.47616898352099213, 4.900433263621000179 ) ) ;
#4170 = CARTESIAN_POINT ( 'NONE',  ( 3.916804611567557437, -78.54668480355715587, 11.07851578385000302 ) ) ;
#4171 = CYLINDRICAL_SURFACE ( 'NONE', #18263, 1.750000000000001332 ) ;
#4172 = ORIENTED_EDGE ( 'NONE', *, *, #30759, .T. ) ;
#4173 = AXIS2_PLACEMENT_3D ( 'NONE', #54775, #9614, #45644 ) ;
#4174 = CARTESIAN_POINT ( 'NONE',  ( 2.026540639977999714, -79.84841179485169960, -10.96119216345999803 ) ) ;
#4175 = CARTESIAN_POINT ( 'NONE',  ( 0.8822134339024870764, -79.91310085715470279, 0.8851451072459763925 ) ) ;
#4176 = CARTESIAN_POINT ( 'NONE',  ( -13.99936781018472232, -46.09579702914000165, -0.1330447863085613691 ) ) ;
#4177 = CARTESIAN_POINT ( 'NONE',  ( -0.03734817897619031879, -78.54828561723799396, 3.962636354764707658 ) ) ;
#4178 = VECTOR ( 'NONE', #50468, 1000.000000000000000 ) ;
#4179 = CARTESIAN_POINT ( 'NONE',  ( 9.014082483815000657, -78.44290956889000199, -6.575554473347999362 ) ) ;
#4180 = DIRECTION ( 'NONE',  ( 0.4045849533085069116, -0.8201353736504155556, -0.4045849533085069116 ) ) ;
#4181 = CARTESIAN_POINT ( 'NONE',  ( -0.1062458101858989590, -81.72988145023380469, 1.508520553443295942 ) ) ;
#4182 = CARTESIAN_POINT ( 'NONE',  ( -5.393290222407999934, -77.91540636460800329, -11.03214393298000040 ) ) ;
#4183 = VERTEX_POINT ( 'NONE', #19347 ) ;
#4184 = CARTESIAN_POINT ( 'NONE',  ( 8.385806979700950237, -17.11189753004608605, -9.298530586708613654 ) ) ;
#4185 = DIRECTION ( 'NONE',  ( 1.000000000000000000, 0.000000000000000000, 0.000000000000000000 ) ) ;
#4186 =( NAMED_UNIT ( * ) SI_UNIT ( $, .STERADIAN. ) SOLID_ANGLE_UNIT ( ) );
#4187 = DIRECTION ( 'NONE',  ( 0.9999433559010179051, 0.000000000000000000, 0.01064354214585019887 ) ) ;
#4188 = ORIENTED_EDGE ( 'NONE', *, *, #30663, .T. ) ;
#4189 = ORIENTED_EDGE ( 'NONE', *, *, #57105, .F. ) ;
#4190 = CARTESIAN_POINT ( 'NONE',  ( -5.838193839761687265, -78.47291666666666288, -7.596835002782715840 ) ) ;
#4191 = CARTESIAN_POINT ( 'NONE',  ( 0.6948940501455999064, -77.49853998579800418, 9.517234252032999109 ) ) ;
#4192 = VERTEX_POINT ( 'NONE', #41194 ) ;
#4193 = CARTESIAN_POINT ( 'NONE',  ( 0.000000000000000000, -2.660000000000000142, 0.000000000000000000 ) ) ;
#4194 = EDGE_LOOP ( 'NONE', ( #3504, #51425, #48433, #50870 ) ) ;
#4195 = CARTESIAN_POINT ( 'NONE',  ( 3.325701842495000005, -82.39999999999999147, -0.7068997487804000723 ) ) ;
#4196 = CARTESIAN_POINT ( 'NONE',  ( 8.145694891731999121, -77.83223865415499176, -7.439717004853999782 ) ) ;
#4197 = LINE ( 'NONE', #20828, #56099 ) ;
#4198 = CARTESIAN_POINT ( 'NONE',  ( 7.022198843594999573, -77.93705665246400827, 6.200125618097000135 ) ) ;
#4199 = CARTESIAN_POINT ( 'NONE',  ( -12.50483465194470689, -24.86452578687041637, -0.6958747604665329600 ) ) ;
#4200 = CARTESIAN_POINT ( 'NONE',  ( -4.019809786096000259, -79.10248417168200774, 10.47183077952999852 ) ) ;
#4201 = CARTESIAN_POINT ( 'NONE',  ( -1.086186157952083509, -79.55861393801417591, 0.6243850812737060663 ) ) ;
#4202 = AXIS2_PLACEMENT_3D ( 'NONE', #17965, #9105, #35955 ) ;
#4203 = EDGE_LOOP ( 'NONE', ( #19819, #10461, #32782, #18036, #32710 ) ) ;
#4204 = ORIENTED_EDGE ( 'NONE', *, *, #55099, .T. ) ;
#4205 = CARTESIAN_POINT ( 'NONE',  ( -0.04490943164332775878, -77.47554393188570998, 9.249810934786108163 ) ) ;
#4206 = DIRECTION ( 'NONE',  ( 1.000000000000000000, 0.000000000000000000, 0.000000000000000000 ) ) ;
#4207 = DIRECTION ( 'NONE',  ( 0.000000000000000000, 1.000000000000000000, 0.000000000000000000 ) ) ;
#4208 = CARTESIAN_POINT ( 'NONE',  ( 6.240531904507999883, -78.20986865680399092, 7.431451467605000083 ) ) ;
#4209 = CARTESIAN_POINT ( 'NONE',  ( 3.541185312415000119, -75.59580845059001319, 11.43528872558000131 ) ) ;
#4210 = ADVANCED_FACE ( 'NONE', ( #46525 ), #37342, .F. ) ;
#4211 = CARTESIAN_POINT ( 'NONE',  ( -9.148289698020947824, -79.42135170196439731, -2.562996480311285019 ) ) ;
#4212 = CARTESIAN_POINT ( 'NONE',  ( -9.500000000000000000, -74.70999999999999375, 0.000000000000000000 ) ) ;
#4213 = CARTESIAN_POINT ( 'NONE',  ( -0.3862712429687000237, -82.25000000000000000, -1.188820645369000006 ) ) ;
#4214 = CARTESIAN_POINT ( 'NONE',  ( 12.54981748964999966, -16.95163512371999914, 0.03767836620435999206 ) ) ;
#4215 = CIRCLE ( 'NONE', #44759, 1.749999999999998002 ) ;
#4216 = LINE ( 'NONE', #36089, #13049 ) ;
#4217 = EDGE_LOOP ( 'NONE', ( #23361, #54592, #1307, #38166, #34155, #25462, #27092, #36877, #27817, #27219, #29425 ) ) ;
#4218 = CARTESIAN_POINT ( 'NONE',  ( 1.519276649035000037, -79.23866123649499116, 12.34025290414999887 ) ) ;
#4219 = FACE_BOUND ( 'NONE', #7187, .T. ) ;
#4220 = CARTESIAN_POINT ( 'NONE',  ( -5.974663857816401524, -78.02206841552093408, 8.936645035771457302 ) ) ;
#4221 = CARTESIAN_POINT ( 'NONE',  ( -9.788022091682998749, -17.47120090402999892, -7.956349397064001572 ) ) ;
#4223 = FACE_OUTER_BOUND ( 'NONE', #40712, .T. ) ;
#4222 = CARTESIAN_POINT ( 'NONE',  ( 11.75000000000000178, -78.53958333333331154, -1.538071403319980268 ) ) ;
#4224 = CARTESIAN_POINT ( 'NONE',  ( -10.07627163191000008, -55.55000000278000272, -7.601397897754999633 ) ) ;
#4225 = CARTESIAN_POINT ( 'NONE',  ( 6.244078553291731559, -80.92595668623671656, 8.750503958027614715 ) ) ;
#4226 = CARTESIAN_POINT ( 'NONE',  ( -0.2898532571746000319, -80.24379038178499002, -11.39804518048999959 ) ) ;
#4227 = DIRECTION ( 'NONE',  ( 0.000000000000000000, -1.000000000000000000, 0.000000000000000000 ) ) ;
#4228 = CARTESIAN_POINT ( 'NONE',  ( -6.686799317902000439, -76.89782152666799675, -9.062045808939998892 ) ) ;
#4229 = CARTESIAN_POINT ( 'NONE',  ( -0.4254240051736287720, -1.885416666666666519, 3.249999999999998224 ) ) ;
#4230 = CARTESIAN_POINT ( 'NONE',  ( 2.042758677500000175, -81.03081043471520672, -10.95189639700000050 ) ) ;
#4231 = ORIENTED_EDGE ( 'NONE', *, *, #10356, .F. ) ;
#4232 = CARTESIAN_POINT ( 'NONE',  ( -0.8525066185231022775, -1.497527708407747626, 3.168802892732555776 ) ) ;
#4233 = EDGE_CURVE ( 'NONE', #46084, #55147, #40190, .T. ) ;
#4234 = CARTESIAN_POINT ( 'NONE',  ( -0.4356486348728999536, -53.91935044157000334, 12.43591427117000059 ) ) ;
#4235 = CARTESIAN_POINT ( 'NONE',  ( 8.838834764832000701, -18.75000000000000000, 8.838834764832000701 ) ) ;
#4236 = CARTESIAN_POINT ( 'NONE',  ( 1.220124496691999960, -2.455504995393999579, -3.773911729633000256 ) ) ;
#4237 = CARTESIAN_POINT ( 'NONE',  ( -9.412027495909001118, -79.51667564555398826, 0.4898595818372999400 ) ) ;
#4238 = CARTESIAN_POINT ( 'NONE',  ( 5.948947503763784894, -77.81911908264200406, 7.191054624583967048 ) ) ;
#4239 = CARTESIAN_POINT ( 'NONE',  ( -0.006333666751042999442, -62.13262644267000212, 12.77652491961000081 ) ) ;
#4240 = CARTESIAN_POINT ( 'NONE',  ( 12.77651065923999951, -16.69103388611000227, -0.04307580168118999714 ) ) ;
#4241 = B_SPLINE_SURFACE_WITH_KNOTS ( 'NONE', 3, 3, ( 
 ( #33205, #51543, #46831, #24665, #45951, #46244, #6063, #20239, #14626, #42673, #28785, #37651, #15214, #6357, #24374, #19649, #42386, #32618, #11100 ),
 ( #55961, #10212, #15512, #23488, #1957, #37355, #19950, #41501, #50670, #29080, #38232, #56253, #47125, #15803, #50376, #9923, #41794, #28191, #23779 ),
 ( #27905, #1366, #46541, #5482, #14916, #19362, #55371, #32911, #50955, #1659, #10507, #28490, #24073, #42090, #3387, #42967, #39395, #7811, #16677 ),
 ( #52975, #34658, #25812, #34080, #3669, #21669, #43840, #21382, #33792, #7232, #57403, #38524, #48275, #16961, #34943, #29651, #29365, #30522, #20526 ) ),
 .UNSPECIFIED., .F., .F., .F.,
 ( 4, 4 ),
 ( 4, 1, 1, 1, 1, 1, 1, 1, 1, 1, 1, 1, 1, 1, 1, 1, 4 ),
 ( -0.4015584965371999937, 1.401558496537000043 ),
 ( 0.5889552238806000650, 0.6151492537313000275, 0.6413432835821000211, 0.6675373134327999836, 0.6937313432835999771, 0.7199253731343000506, 0.7461194029851000442, 0.7723134328358000067, 0.7985074626866000003, 0.8247014925372999627, 0.8508955223880999563, 0.8770895522388000298, 0.9032835820896000234, 0.9294776119402999859, 0.9556716417910000594, 0.9818656716417999419, 1.008059701493000171 ),
 .UNSPECIFIED. ) ;
#4242 = CARTESIAN_POINT ( 'NONE',  ( -0.7781692987085999658, -84.55857450217399673, 4.056224359023000048 ) ) ;
#4243 = CARTESIAN_POINT ( 'NONE',  ( -12.99999999992999911, -5.999999999934908956, -2.526613301470000081E-09 ) ) ;
#4244 = EDGE_CURVE ( 'NONE', #9459, #3462, #18783, .T. ) ;
#4245 = FACE_OUTER_BOUND ( 'NONE', #56485, .T. ) ;
#4247 = EDGE_CURVE ( 'NONE', #49218, #15698, #10038, .T. ) ;
#4246 = CARTESIAN_POINT ( 'NONE',  ( -3.644841321323999850, -78.56852404215999286, 11.22553106161999992 ) ) ;
#4248 = AXIS2_PLACEMENT_3D ( 'NONE', #49786, #4010, #31448 ) ;
#4249 = CARTESIAN_POINT ( 'NONE',  ( -0.8202502003661000796, -77.32800251553000237, -11.11673469052999863 ) ) ;
#4250 = CARTESIAN_POINT ( 'NONE',  ( 0.07675521435781498814, -81.97078358942633258, 1.247900519352959092 ) ) ;
#4251 = CARTESIAN_POINT ( 'NONE',  ( 0.1580158025359000018, -78.26021020222999880, 1.541016301036999936 ) ) ;
#4252 = CARTESIAN_POINT ( 'NONE',  ( 1.308715794682547395, -61.54404499166074061, 12.70256747360829408 ) ) ;
#4253 = CARTESIAN_POINT ( 'NONE',  ( 0.3159905065672543589, -83.10829663276524570, 1.478797643683121166 ) ) ;
#4254 = DIRECTION ( 'NONE',  ( -0.7071067811865475727, 0.000000000000000000, 0.7071067811865475727 ) ) ;
#4255 = CARTESIAN_POINT ( 'NONE',  ( 0.04941934297688648642, -80.22561524380986953, -10.74974344490763656 ) ) ;
#4256 = DIRECTION ( 'NONE',  ( -1.000000000000000000, 0.000000000000000000, 0.000000000000000000 ) ) ;
#4257 = CARTESIAN_POINT ( 'NONE',  ( 9.454069809452303019, -79.14512987373443309, 6.036735293332626817 ) ) ;
#4258 = CARTESIAN_POINT ( 'NONE',  ( 0.4912582738047306941, -81.75727386977339961, -1.149340960687430968 ) ) ;
#4259 = AXIS2_PLACEMENT_3D ( 'NONE', #57813, #39517, #26225 ) ;
#4260 = CARTESIAN_POINT ( 'NONE',  ( 10.71369944335147828, -79.37083333333336554, 2.879226727952053810 ) ) ;
#4261 = CARTESIAN_POINT ( 'NONE',  ( -1.478754609759999950, -78.43772245792399644, -10.94487265352999827 ) ) ;
#4262 = CARTESIAN_POINT ( 'NONE',  ( 7.342331066867000544, -55.64999999967000122, 8.190859204290999784 ) ) ;
#4263 = ORIENTED_EDGE ( 'NONE', *, *, #16967, .F. ) ;
#4264 = ORIENTED_EDGE ( 'NONE', *, *, #10969, .T. ) ;
#4265 = CARTESIAN_POINT ( 'NONE',  ( 0.000000000000000000, -76.39999999999999147, 0.000000000000000000 ) ) ;
#4266 = EDGE_CURVE ( 'NONE', #48292, #52197, #13602, .T. ) ;
#4267 = VERTEX_POINT ( 'NONE', #36756 ) ;
#4268 = DIRECTION ( 'NONE',  ( 0.000000000000000000, 0.000000000000000000, -1.000000000000000000 ) ) ;
#4269 = ORIENTED_EDGE ( 'NONE', *, *, #56979, .T. ) ;
#4270 = DIRECTION ( 'NONE',  ( 0.000000000000000000, 0.000000000000000000, 1.000000000000000000 ) ) ;
#4271 = CARTESIAN_POINT ( 'NONE',  ( 1.500000000000000000, -78.25000000000000000, 0.000000000000000000 ) ) ;
#4272 = CARTESIAN_POINT ( 'NONE',  ( 4.703593957913000168, -79.48108495741900015, 9.978874598900000947 ) ) ;
#4273 = CARTESIAN_POINT ( 'NONE',  ( 1.890224871707000043, -23.74789248015000354, -12.68696160873999901 ) ) ;
#4274 = CARTESIAN_POINT ( 'NONE',  ( 3.746144170002000173, -79.77245509461999973, 0.2788807567526999653 ) ) ;
#4275 = CARTESIAN_POINT ( 'NONE',  ( -5.548822036515788980, -79.32452569715752588, 7.710984173510062156 ) ) ;
#4276 = EDGE_LOOP ( 'NONE', ( #39331, #12187, #50106, #11266 ) ) ;
#4277 = CARTESIAN_POINT ( 'NONE',  ( -10.47078769030999901, -77.87566818494818222, -3.499536356729999742 ) ) ;
#4278 = CARTESIAN_POINT ( 'NONE',  ( -5.507598458736999270, -79.00630127599001185, -10.89743148201000089 ) ) ;
#4279 = ORIENTED_EDGE ( 'NONE', *, *, #2481, .F. ) ;
#4280 = ORIENTED_EDGE ( 'NONE', *, *, #19550, .F. ) ;
#4281 = CARTESIAN_POINT ( 'NONE',  ( 5.442299421053111708, -79.47333333333332916, -7.827182525635441479 ) ) ;
#4282 = CARTESIAN_POINT ( 'NONE',  ( -0.4872545538094000261, -79.36089768585199522, -1.241463230931000084 ) ) ;
#4283 = CARTESIAN_POINT ( 'NONE',  ( -6.473047519705999342, -78.14265519630798451, 7.229824698717000508 ) ) ;
#4284 = CARTESIAN_POINT ( 'NONE',  ( 3.647699722740934014, -86.17851881763699851, -1.624060551956148624 ) ) ;
#4285 = FACE_OUTER_BOUND ( 'NONE', #26466, .T. ) ;
#4286 = DIRECTION ( 'NONE',  ( -0.9903465037221068634, -0.1386138613754009652, 0.000000000000000000 ) ) ;
#4287 = CARTESIAN_POINT ( 'NONE',  ( -1.240843214692000096, -81.11237249610999811, -0.5344114414419000036 ) ) ;
#4288 = MECHANICAL_DESIGN_GEOMETRIC_PRESENTATION_REPRESENTATION (  '', ( #23168 ), #56180 ) ;
#4289 = CARTESIAN_POINT ( 'NONE',  ( 2.042225293701000144, -76.31900208490598914, 10.80792172197000056 ) ) ;
#4290 = CARTESIAN_POINT ( 'NONE',  ( 0.000000000000000000, -86.39999999999999147, 0.000000000000000000 ) ) ;
#4291 = CARTESIAN_POINT ( 'NONE',  ( 3.242112172283999616, -80.97881882065600223, -2.558754062436000343 ) ) ;
#4292 = CARTESIAN_POINT ( 'NONE',  ( -12.76303204517000012, -18.73514852243999940, 1.980584515753000208 ) ) ;
#4293 = CARTESIAN_POINT ( 'NONE',  ( 1.998746230246073452, -76.83803665960124363, -11.64838672263795338 ) ) ;
#4294 = CARTESIAN_POINT ( 'NONE',  ( -3.445820259768999971, -81.44392549782598678, 1.005017585769000021 ) ) ;
#4295 = CARTESIAN_POINT ( 'NONE',  ( 11.00000000000000000, -78.44999999999998863, 0.000000000000000000 ) ) ;
#4296 = CARTESIAN_POINT ( 'NONE',  ( -8.418594644163000851, -80.95952068081420805, -7.485750452785000064 ) ) ;
#4297 = CARTESIAN_POINT ( 'NONE',  ( 3.383845406481000406, -2.460161638760999914, -1.742318191517000070 ) ) ;
#4298 = CARTESIAN_POINT ( 'NONE',  ( 0.7897348250228778399, -80.07181507767086259, 1.000737493962424507 ) ) ;
#4299 = ORIENTED_EDGE ( 'NONE', *, *, #54449, .F. ) ;
#4300 = CARTESIAN_POINT ( 'NONE',  ( 0.000000000000000000, 4.040000000000000036, 0.000000000000000000 ) ) ;
#4301 = ADVANCED_FACE ( 'NONE', ( #14316 ), #50359, .F. ) ;
#4302 = CARTESIAN_POINT ( 'NONE',  ( 0.000000000000000000, -75.20000000000000284, 0.000000000000000000 ) ) ;
#4303 = CARTESIAN_POINT ( 'NONE',  ( 1.289124607492999841, -80.94872977871700925, 0.3416633729347999804 ) ) ;
#4304 = ADVANCED_FACE ( 'NONE', ( #1070, #19058 ), #37046, .T. ) ;
#4305 = CARTESIAN_POINT ( 'NONE',  ( -6.380391360217929630, -78.96666666666666856, -7.083361869089003449 ) ) ;
#4306 = CARTESIAN_POINT ( 'NONE',  ( 12.51033564907000084, -78.21047501799000656, -3.582046052171000028 ) ) ;
#4307 = CARTESIAN_POINT ( 'NONE',  ( -7.712213536754459753, -60.86179137581871146, -10.27334987168057090 ) ) ;
#4308 = CARTESIAN_POINT ( 'NONE',  ( 12.80900240953000058, -21.75365779208000205, -1.930989144707000005 ) ) ;
#4309 = VERTEX_POINT ( 'NONE', #52100 ) ;
#4310 = CARTESIAN_POINT ( 'NONE',  ( -8.835193196228999568, -77.12585001815408248, 7.003236733173999973 ) ) ;
#4311 = EDGE_CURVE ( 'NONE', #469, #55491, #13171, .T. ) ;
#4312 = CARTESIAN_POINT ( 'NONE',  ( -0.1286311518798999853, -80.97088155641299068, -1.500807616117999954 ) ) ;
#4313 = CARTESIAN_POINT ( 'NONE',  ( 7.626500777237000150, -18.68415268018999953, -10.35747145892000098 ) ) ;
#4314 = CARTESIAN_POINT ( 'NONE',  ( -9.487842642213001554, -77.96369001827098089, -0.8069809344749999669 ) ) ;
#4316 = CARTESIAN_POINT ( 'NONE',  ( -3.616527695712999702, -1.863176978014000174, -0.5438149879621999583 ) ) ;
#4315 = CARTESIAN_POINT ( 'NONE',  ( 2.168860615702000061, -82.38203554481998481, 3.316922010221999617 ) ) ;
#4317 = CARTESIAN_POINT ( 'NONE',  ( -2.062597299672999540, -56.01514526721999943, -12.87022657272000004 ) ) ;
#4318 = B_SPLINE_CURVE_WITH_KNOTS ( 'NONE', 3,
 ( #12250, #1745, #47999, #52696 ),
 .UNSPECIFIED., .F., .F.,
 ( 4, 4 ),
 ( 0.000000000000000000, 1.000000000000000000 ),
 .UNSPECIFIED. ) ;
#4319 = CARTESIAN_POINT ( 'NONE',  ( -0.3384184472371999930, -79.44022655590600834, 1.477976681755000188 ) ) ;
#4320 = ORIENTED_EDGE ( 'NONE', *, *, #20420, .F. ) ;
#4321 = CARTESIAN_POINT ( 'NONE',  ( -0.8545357605647209143, -77.21876371591302757, -10.72076371046810017 ) ) ;
#4322 = CARTESIAN_POINT ( 'NONE',  ( 0.1963495408493637351, -79.03541666666667709, -1.499999999999999778 ) ) ;
#4323 = CARTESIAN_POINT ( 'NONE',  ( 0.9410294744130467404, -78.91653188272211139, -3.792696602583483845 ) ) ;
#4324 = VERTEX_POINT ( 'NONE', #7793 ) ;
#4325 = EDGE_LOOP ( 'NONE', ( #27413, #52065, #13250, #55978 ) ) ;
#4326 = FACE_OUTER_BOUND ( 'NONE', #27734, .T. ) ;
#4327 = COLOUR_RGB ( '', 0.72549020, 0.75294118, 0.79215686) ;
#4328 = CARTESIAN_POINT ( 'NONE',  ( 12.50000000000000000, -18.75000000000000000, 1.250000000000000000 ) ) ;
#4329 = ORIENTED_EDGE ( 'NONE', *, *, #45187, .T. ) ;
#4330 = CARTESIAN_POINT ( 'NONE',  ( 0.4872551020249000220, -77.56291771239200727, 12.03986520427999984 ) ) ;
#4331 = EDGE_CURVE ( 'NONE', #38464, #40725, #54158, .T. ) ;
#4332 = EDGE_LOOP ( 'NONE', ( #25034, #22262, #43485, #12254 ) ) ;
#4333 = CIRCLE ( 'NONE', #43117, 12.50000000000000000 ) ;
#4334 = ORIENTED_EDGE ( 'NONE', *, *, #851, .T. ) ;
#4335 = CARTESIAN_POINT ( 'NONE',  ( 7.398464061244442114, -60.25160423312497215, 8.140250184783569765 ) ) ;
#4336 = B_SPLINE_SURFACE_WITH_KNOTS ( 'NONE', 3, 3, ( 
 ( #16440, #25862, #12010, #21146, #39155, #25574, #30575, #12292, #43307, #8154, #57737, #30283, #7863, #44173, #26153, #3722, #39729, #17296, #16728, #34128, #35284, #43891, #11439, #56592, #29989, #16151, #29419, #6997, #48043, #47472, #25000, #43020, #7285, #7576, #2577 ),
 ( #11727, #25287, #34709, #43594, #2864, #20860, #38862, #40619, #41196, #40911, #58033, #501, #22898, #36186, #13148, #215, #785, #22607, #18191, #4609, #31444, #4900, #32031, #23191, #45647, #54203, #12857, #17894, #13738, #31142, #53314, #31737, #50074, #49781, #17593 ),
 ( #53913, #9327, #45057, #13445, #18478, #9617, #27318, #45350, #27605, #36469, #35580, #8437, #18765, #54496, #30858, #14034, #5187, #48896, #35884, #26433, #49182, #44454, #4005, #22010, #40018, #53609, #8733, #26726, #44754, #4306, #49485, #27021, #22306, #40321, #58330 ),
 ( #9034, #19061, #50361, #2227, #46528, #24650, #37636, #47111, #42078, #19937, #6641, #32313, #11088, #41486, #42660, #29067, #36758, #28478, #37048, #1648, #14903, #32901, #10791, #27892, #23767, #45939, #5471, #50945, #55950, #10493, #6346, #54777, #55360, #6052, #55065 ) ),
 .UNSPECIFIED., .F., .F., .F.,
 ( 4, 4 ),
 ( 4, 1, 1, 1, 1, 1, 1, 1, 1, 1, 1, 1, 1, 1, 1, 1, 1, 1, 1, 1, 1, 1, 1, 1, 1, 1, 1, 1, 1, 1, 1, 1, 4 ),
 ( -0.02000000000002000178, 1.020000000000000018 ),
 ( -0.02000000000000000042, 0.01250000000000000069, 0.04499999999999999833, 0.07749999999999999944, 0.1100000000000000006, 0.1424999999999999878, 0.1749999999999999889, 0.2074999999999999900, 0.2399999999999999911, 0.2725000000000000200, 0.3049999999999999933, 0.3375000000000000222, 0.3699999999999999956, 0.4025000000000000244, 0.4349999999999999978, 0.4675000000000000266, 0.5000000000000000000, 0.5324999999999999734, 0.5649999999999999467, 0.5975000000000000311, 0.6300000000000000044, 0.6624999999999999778, 0.6949999999999999512, 0.7275000000000000355, 0.7600000000000000089, 0.7924999999999999822, 0.8249999999999999556, 0.8575000000000000400, 0.8900000000000000133, 0.9224999999999999867, 0.9549999999999999600, 0.9875000000000000444, 1.020000000000000018 ),
 .UNSPECIFIED. ) ;
#4337 = DIRECTION ( 'NONE',  ( -1.000000000000000000, 0.000000000000000000, 0.000000000000000000 ) ) ;
#4338 = CARTESIAN_POINT ( 'NONE',  ( 5.411006671257999834, -79.57828900368951963, 8.131518144102999557 ) ) ;
#4339 = ORIENTED_EDGE ( 'NONE', *, *, #16382, .T. ) ;
#4340 = CARTESIAN_POINT ( 'NONE',  ( 0.3859110462609495196, -82.02864582858185827, -1.432732671933543811 ) ) ;
#4341 = ORIENTED_EDGE ( 'NONE', *, *, #21619, .T. ) ;
#4342 = CARTESIAN_POINT ( 'NONE',  ( -0.9313275411143693283, -79.58998078605505100, 0.8705974481289671107 ) ) ;
#4343 = CARTESIAN_POINT ( 'NONE',  ( -11.05835115351384879, -79.80000000000001137, -4.525376038907399590 ) ) ;
#4344 = EDGE_CURVE ( 'NONE', #18184, #30606, #22055, .T. ) ;
#4345 = CARTESIAN_POINT ( 'NONE',  ( 10.36222501928999939, -55.57880030132999849, 7.631889976297999922 ) ) ;
#4346 = CARTESIAN_POINT ( 'NONE',  ( -7.627487525415999947, -23.29778754190000001, -10.35845608625999859 ) ) ;
#4347 = CARTESIAN_POINT ( 'NONE',  ( -8.160216722324735272, -79.66145833332932114, 4.702279492088285551 ) ) ;
#4348 = DIRECTION ( 'NONE',  ( 0.000000000000000000, 0.000000000000000000, -1.000000000000000000 ) ) ;
#4349 = CARTESIAN_POINT ( 'NONE',  ( 7.705119999435999567, -57.04828923575999511, -10.24996238029999951 ) ) ;
#4350 = CARTESIAN_POINT ( 'NONE',  ( -10.12290050124000018, -23.24999999991999644, -7.648026767085999822 ) ) ;
#4351 = CARTESIAN_POINT ( 'NONE',  ( -10.18127202938000053, -23.38645218951999993, 7.633406483298000644 ) ) ;
#4352 = CARTESIAN_POINT ( 'NONE',  ( 10.42531124903999995, -55.53514851492000304, -7.624341765436000173 ) ) ;
#4353 = CARTESIAN_POINT ( 'NONE',  ( -10.07979664880000037, -76.97175206120299151, 3.736335038366999761 ) ) ;
#4354 = CARTESIAN_POINT ( 'NONE',  ( 4.658259624636106544, -77.76681350748577870, -8.082155137772446096 ) ) ;
#4355 = CARTESIAN_POINT ( 'NONE',  ( -2.384909972384000376, -80.44230496681200293, -3.423779596157999983 ) ) ;
#4356 = CARTESIAN_POINT ( 'NONE',  ( -6.446975197297999394, -77.18928667140100686, 7.331209084132000342 ) ) ;
#4357 = CARTESIAN_POINT ( 'NONE',  ( -12.66316398248999953, -16.82133896655000171, -0.04044089952540000366 ) ) ;
#4358 = CARTESIAN_POINT ( 'NONE',  ( 7.919595949288999570, -59.94999999969000015, 8.768124086712999699 ) ) ;
#4359 = FACE_OUTER_BOUND ( 'NONE', #8727, .T. ) ;
#4360 = B_SPLINE_CURVE_WITH_KNOTS ( 'NONE', 3,
 ( #51971, #20663, #23923, #47560, #11528, #7085 ),
 .UNSPECIFIED., .F., .F.,
 ( 4, 2, 4 ),
 ( 0.000000000000000000, 0.5000000000000000000, 1.000000000000000000 ),
 .UNSPECIFIED. ) ;
#4361 = CARTESIAN_POINT ( 'NONE',  ( -0.9820397338569999413, -80.80308451575899653, -0.7733679338621000099 ) ) ;
#4362 = CARTESIAN_POINT ( 'NONE',  ( 0.000000000000000000, -92.79999999999999716, 0.000000000000000000 ) ) ;
#4363 = CARTESIAN_POINT ( 'NONE',  ( 2.370180320845999944, -1.873872700496999943, 2.739986503352000113 ) ) ;
#4364 = EDGE_CURVE ( 'NONE', #900, #32341, #55438, .T. ) ;
#4365 = CARTESIAN_POINT ( 'NONE',  ( -2.364557222828000072, -79.54490095943376105, 9.257622954664000758 ) ) ;
#4367 = ADVANCED_FACE ( 'NONE', ( #25794 ), #41891, .T. ) ;
#4366 = CARTESIAN_POINT ( 'NONE',  ( 1.448902839066656512, -81.12261281811970548, 0.4373190867481531185 ) ) ;
#4368 = CARTESIAN_POINT ( 'NONE',  ( 12.79895559718999998, -60.60469146232000526, -2.015913954445999856 ) ) ;
#4369 = CYLINDRICAL_SURFACE ( 'NONE', #57062, 0.5999999999999999778 ) ;
#4370 = DIRECTION ( 'NONE',  ( 0.000000000000000000, 1.000000000000000000, 0.000000000000000000 ) ) ;
#4371 = CARTESIAN_POINT ( 'NONE',  ( 10.47129194184999967, -78.29940181198600158, 3.086650459461000473 ) ) ;
#4372 = AXIS2_PLACEMENT_3D ( 'NONE', #14606, #28175, #46228 ) ;
#4373 = CARTESIAN_POINT ( 'NONE',  ( 11.54375705602000046, -77.66559881290099554, -3.837213001227999687 ) ) ;
#4374 = LINE ( 'NONE', #40387, #52388 ) ;
#4376 = CARTESIAN_POINT ( 'NONE',  ( 1.360845176917000021, -78.56634434942300516, -0.6686124113221000309 ) ) ;
#4375 = FACE_OUTER_BOUND ( 'NONE', #24167, .T. ) ;
#4377 = CARTESIAN_POINT ( 'NONE',  ( -0.6718767921597000869, -82.67725009134899494, 1.564735933714000105 ) ) ;
#4378 = CIRCLE ( 'NONE', #22283, 4.100000000000000533 ) ;
#4379 = ORIENTED_EDGE ( 'NONE', *, *, #13017, .T. ) ;
#4380 = CARTESIAN_POINT ( 'NONE',  ( 3.318044994455000118, -82.87121544543099105, 1.761282353723000016 ) ) ;
#4381 = FACE_OUTER_BOUND ( 'NONE', #53864, .T. ) ;
#4382 = CARTESIAN_POINT ( 'NONE',  ( -1.100349016362999865, -80.25828634263528727, -11.11813777798999858 ) ) ;
#4383 = EDGE_CURVE ( 'NONE', #56919, #35878, #42731, .T. ) ;
#4384 = AXIS2_PLACEMENT_3D ( 'NONE', #30778, #12780, #49696 ) ;
#4385 = CARTESIAN_POINT ( 'NONE',  ( 8.500000000000000000, -7.000000000000000000, 0.000000000000000000 ) ) ;
#4386 = CARTESIAN_POINT ( 'NONE',  ( -1.673666828592297096, -85.94583333953119109, 3.009623589966792689 ) ) ;
#4387 = CARTESIAN_POINT ( 'NONE',  ( 4.013660496580000903, -78.55580284730699248, -10.47417304634999979 ) ) ;
#4388 = CARTESIAN_POINT ( 'NONE',  ( -9.835223439052001027, -60.88138927622999574, 7.760980897183999971 ) ) ;
#4389 = CARTESIAN_POINT ( 'NONE',  ( 0.000000000000000000, -77.19999999999998863, 0.000000000000000000 ) ) ;
#4390 = CARTESIAN_POINT ( 'NONE',  ( -1.842588707444517082, -76.41257734936500867, -11.67485934150305305 ) ) ;
#4391 = CARTESIAN_POINT ( 'NONE',  ( 12.57354097141999993, -23.72384125742000194, -1.757953070309000054 ) ) ;
#4392 = DIRECTION ( 'NONE',  ( -1.000000000000000000, 0.000000000000000000, 0.000000000000000000 ) ) ;
#4393 = ORIENTED_EDGE ( 'NONE', *, *, #48882, .T. ) ;
#4394 = CARTESIAN_POINT ( 'NONE',  ( 0.000000000000000000, -77.50000000000000000, 0.000000000000000000 ) ) ;
#4395 = CARTESIAN_POINT ( 'NONE',  ( -2.978309893851999846, -79.79237999526598912, -8.903583414616999647 ) ) ;
#4396 = CARTESIAN_POINT ( 'NONE',  ( -0.1371744130071849144, -1.722991222295529257, -3.270659802130597704 ) ) ;
#4397 = CARTESIAN_POINT ( 'NONE',  ( 3.133406165714999858, -82.54767953870899078, 1.663272498094999996 ) ) ;
#4398 = CARTESIAN_POINT ( 'NONE',  ( -12.53241208775000004, -56.03537109808000594, -1.667936697358999965 ) ) ;
#4399 = ORIENTED_EDGE ( 'NONE', *, *, #36754, .T. ) ;
#4400 = DIRECTION ( 'NONE',  ( 0.000000000000000000, 1.000000000000000000, 0.000000000000000000 ) ) ;
#4401 = CARTESIAN_POINT ( 'NONE',  ( 5.891586754291419759, -77.86430406625845535, -10.19928502571758244 ) ) ;
#4402 = CARTESIAN_POINT ( 'NONE',  ( -1.799501877793999949, -23.28917723430000208, 12.60552511010000032 ) ) ;
#4403 = ORIENTED_EDGE ( 'NONE', *, *, #1881, .F. ) ;
#4404 = CARTESIAN_POINT ( 'NONE',  ( -7.762982794220000038, -54.63910040255000666, -9.991998894170999179 ) ) ;
#4405 = FILL_AREA_STYLE ('',( #22407 ) ) ;
#4406 = CARTESIAN_POINT ( 'NONE',  ( -9.387315177295000979, -79.80788071282599105, 2.697965643110000311 ) ) ;
#4407 = ORIENTED_EDGE ( 'NONE', *, *, #46423, .F. ) ;
#4408 = VERTEX_POINT ( 'NONE', #38215 ) ;
#4409 = CARTESIAN_POINT ( 'NONE',  ( -1.996166675347000208, -76.07957723391299965, 11.82412830296999928 ) ) ;
#4410 = CARTESIAN_POINT ( 'NONE',  ( -0.1834469635243000107, -79.21327907014000402, -1.236465612773999911 ) ) ;
#4411 = CARTESIAN_POINT ( 'NONE',  ( -1.069737409789999871, -78.83877241711999773, -1.254012819428000247 ) ) ;
#4412 = ORIENTED_EDGE ( 'NONE', *, *, #54106, .F. ) ;
#4413 = CARTESIAN_POINT ( 'NONE',  ( 4.574312611392000072, -77.52515584965399853, 8.320643751074999983 ) ) ;
#4414 = VECTOR ( 'NONE', #23046, 1000.000000000000000 ) ;
#4415 = EDGE_CURVE ( 'NONE', #6738, #33527, #3371, .T. ) ;
#4416 = CARTESIAN_POINT ( 'NONE',  ( 0.9762155229984909033, -80.29668698289697204, -0.7812602609263914477 ) ) ;
#4417 = CARTESIAN_POINT ( 'NONE',  ( -1.332847799107999887, -78.19825864453000008, -12.88744032790000027 ) ) ;
#4418 = VECTOR ( 'NONE', #25494, 999.9999999999998863 ) ;
#4419 = CARTESIAN_POINT ( 'NONE',  ( 0.5473670387515998659, -76.87888519345946747, -11.20350390113000039 ) ) ;
#4420 = CARTESIAN_POINT ( 'NONE',  ( -8.031347306244652984, -78.38283164370827194, 9.096189540893634629 ) ) ;
#4421 = CARTESIAN_POINT ( 'NONE',  ( -2.355016251976907782, -86.17851879815599148, 3.178902848252080915 ) ) ;
#4422 = CARTESIAN_POINT ( 'NONE',  ( -0.4146318973825999787, -79.52374057552499664, -11.20920117498000046 ) ) ;
#4423 = CARTESIAN_POINT ( 'NONE',  ( 5.403870014527243804, -79.92583434048029289, 7.507032179181077680 ) ) ;
#4424 = VECTOR ( 'NONE', #56506, 1000.000000000000114 ) ;
#4425 = CARTESIAN_POINT ( 'NONE',  ( -10.84994315462449421, -79.96754507315236538, -2.381405434182155112 ) ) ;
#4426 = ORIENTED_EDGE ( 'NONE', *, *, #39795, .F. ) ;
#4427 = LINE ( 'NONE', #5299, #30646 ) ;
#4428 = CARTESIAN_POINT ( 'NONE',  ( 10.69843650790000034, -76.34317683517998887, 6.089250768039999429 ) ) ;
#4429 = CARTESIAN_POINT ( 'NONE',  ( 1.416781233620999947, -80.19787091841099880, 0.7745610770380000343 ) ) ;
#4430 = VECTOR ( 'NONE', #18510, 1000.000000000000000 ) ;
#4431 = CARTESIAN_POINT ( 'NONE',  ( -3.472969013104772795, -2.868348082004792410, -0.8615918643323726700 ) ) ;
#4432 = CARTESIAN_POINT ( 'NONE',  ( -1.178447680628000205, -80.55308451575899653, -0.9280415206345000723 ) ) ;
#4433 = CARTESIAN_POINT ( 'NONE',  ( -1.750000000000000000, -21.75064714178000003, 12.65372179279999898 ) ) ;
#4434 = FACE_OUTER_BOUND ( 'NONE', #31026, .T. ) ;
#4435 = CARTESIAN_POINT ( 'NONE',  ( -8.084017119143000585, -76.98881332859899373, -5.230585977929000485 ) ) ;
#4436 = CARTESIAN_POINT ( 'NONE',  ( 11.02852943141175857, -76.76673008103259122, -4.905271118666760799 ) ) ;
#4437 = CARTESIAN_POINT ( 'NONE',  ( 10.75000000000000000, -79.75000000000000000, 0.000000000000000000 ) ) ;
#4438 = CARTESIAN_POINT ( 'NONE',  ( 4.782478426736999744, -79.58994887379353145, 10.14623135401999932 ) ) ;
#4439 = ORIENTED_EDGE ( 'NONE', *, *, #23257, .T. ) ;
#4441 = EDGE_CURVE ( 'NONE', #1255, #39893, #43523, .T. ) ;
#4440 = CARTESIAN_POINT ( 'NONE',  ( -0.5511181765943999888, -82.99009435914298649, -1.486830790314999984 ) ) ;
#4442 = CARTESIAN_POINT ( 'NONE',  ( -0.7285569484545000307, -80.09966061487999411, -1.138057995564000002 ) ) ;
#4443 = DIRECTION ( 'NONE',  ( 0.000000000000000000, -1.000000000000000000, 0.000000000000000000 ) ) ;
#4444 = CARTESIAN_POINT ( 'NONE',  ( -6.099999999940000528, -80.79999999975800051, -5.338250164827000611E-09 ) ) ;
#4445 = CARTESIAN_POINT ( 'NONE',  ( 8.185698792048100358, -77.00000000000001421, 4.534146512987735633 ) ) ;
#4446 = CARTESIAN_POINT ( 'NONE',  ( -1.552248384014999871, -82.74082611137200161, 0.6048007385293000526 ) ) ;
#4447 = CARTESIAN_POINT ( 'NONE',  ( 6.891697027498000061, -78.75057898155800729, -9.743716654505998775 ) ) ;
#4448 = CARTESIAN_POINT ( 'NONE',  ( 6.584508673715999905, -78.38574805011499791, 7.154582167228999978 ) ) ;
#4449 = CARTESIAN_POINT ( 'NONE',  ( -1.922928979007999750, -77.25188066968198086, -9.325916353809999393 ) ) ;
#4450 = CARTESIAN_POINT ( 'NONE',  ( -0.5506765233279999894, -53.54045707723000191, -12.77514798307000099 ) ) ;
#4451 = CARTESIAN_POINT ( 'NONE',  ( 4.974995203995084658, -76.03968481403192925, 10.64665306664898026 ) ) ;
#4452 = CARTESIAN_POINT ( 'NONE',  ( 10.91479203715999979, -80.27508423127190440, -0.2066369003937000015 ) ) ;
#4453 = DIRECTION ( 'NONE',  ( -0.7071067811865475727, 0.000000000000000000, 0.7071067811865475727 ) ) ;
#4454 = ORIENTED_EDGE ( 'NONE', *, *, #25310, .T. ) ;
#4455 = CARTESIAN_POINT ( 'NONE',  ( -3.234762833941021931, -78.20250000000001478, 8.977080150340221110 ) ) ;
#4456 = FACE_OUTER_BOUND ( 'NONE', #1970, .T. ) ;
#4457 = CARTESIAN_POINT ( 'NONE',  ( 3.548349909811000735, -78.43735717367049176, -1.307818870560639724E-15 ) ) ;
#4458 = ADVANCED_FACE ( 'NONE', ( #11085 ), #23972, .F. ) ;
#4459 = CARTESIAN_POINT ( 'NONE',  ( -6.410916551769402005, -76.27903085470401834, -9.847934956580132848 ) ) ;
#4460 = CARTESIAN_POINT ( 'NONE',  ( 4.634563706678000550, -78.77046067378098826, 9.949112313689999709 ) ) ;
#4461 = EDGE_CURVE ( 'NONE', #3236, #26282, #28686, .T. ) ;
#4462 = CARTESIAN_POINT ( 'NONE',  ( 10.71369944335146585, -79.32916666666666572, -2.879226727952113318 ) ) ;
#4463 = CARTESIAN_POINT ( 'NONE',  ( 8.082813797676999812, -77.12536394690199870, -8.776523399436001682 ) ) ;
#4464 = DIRECTION ( 'NONE',  ( 0.000000000000000000, 1.000000000000000000, 0.000000000000000000 ) ) ;
#4465 = FACE_OUTER_BOUND ( 'NONE', #31696, .T. ) ;
#4466 = ORIENTED_EDGE ( 'NONE', *, *, #36578, .F. ) ;
#4467 = CIRCLE ( 'NONE', #3480, 0.5999999999999999778 ) ;
#4468 = CARTESIAN_POINT ( 'NONE',  ( 11.07171638148000170, -78.94961247579199437, -1.292941197001999942 ) ) ;
#4469 = CARTESIAN_POINT ( 'NONE',  ( 8.572837821482822918, -77.28120002596543259, 3.549340890814673966 ) ) ;
#4470 = CARTESIAN_POINT ( 'NONE',  ( 0.000000000000000000, -23.25000000000000000, -12.50000000000000000 ) ) ;
#4471 = CARTESIAN_POINT ( 'NONE',  ( -0.01108750193282677897, -76.32470312858129091, -11.74984001957459867 ) ) ;
#4472 = B_SPLINE_CURVE_WITH_KNOTS ( 'NONE', 3,
 ( #58362, #31174, #816, #45086, #27636, #22641, #45678, #23223, #41227, #54809, #40353, #22930, #14351, #49215, #48923, #8764, #242, #17625, #44483, #4034, #22338, #31471, #22040 ),
 .UNSPECIFIED., .F., .F.,
 ( 4, 2, 2, 1, 2, 2, 2, 2, 2, 2, 2, 4 ),
 ( 0.2857074366539503751, 0.3749940070722066476, 0.4196372922813347284, 0.4642805774904628646, 0.5089238626995910009, 0.5535671479087190816, 0.6428537183269752431, 0.7321402887452314046, 0.8214268591634875660, 0.9107134295817437275, 0.9553567147908719193, 1.000000000000000000 ),
 .UNSPECIFIED. ) ;
#4473 = CARTESIAN_POINT ( 'NONE',  ( -10.87436498444000144, -79.73515786819298512, 1.083693866698000052 ) ) ;
#4474 = CARTESIAN_POINT ( 'NONE',  ( 13.89999999999999858, -6.000000000000000000, 0.000000000000000000 ) ) ;
#4475 = CIRCLE ( 'NONE', #52553, 8.800000000000000711 ) ;
#4476 = CARTESIAN_POINT ( 'NONE',  ( -10.98768939184211568, -23.45050660130693032, 0.5207199486336721028 ) ) ;
#4477 = CARTESIAN_POINT ( 'NONE',  ( 8.990136242696999958, -79.13622555867699759, 8.365012251980999736 ) ) ;
#4478 = EDGE_CURVE ( 'NONE', #23873, #31323, #3367, .T. ) ;
#4479 = AXIS2_PLACEMENT_3D ( 'NONE', #18060, #36053, #4480 ) ;
#4480 = DIRECTION ( 'NONE',  ( -0.7071067811865970887, 0.000000000000000000, 0.7071067811864981678 ) ) ;
#4481 = B_SPLINE_CURVE_WITH_KNOTS ( 'NONE', 3,
 ( #52848, #44866, #4420, #57556, #23232, #17117, #827, #55398, #28222, #47154, #42122, #14945, #47444, #51573, #38260, #6093, #50986, #6683, #24692, #10537, #41823, #15833, #5801, #10241, #55107, #2270, #28520, #56283, #6972, #51860, #46860, #24102, #46569, #14652, #1987 ),
 .UNSPECIFIED., .F., .F.,
 ( 4, 1, 1, 1, 1, 1, 1, 1, 1, 1, 1, 1, 1, 1, 1, 1, 1, 1, 1, 1, 1, 1, 1, 1, 1, 1, 1, 1, 1, 1, 1, 1, 4 ),
 ( 0.000000000000000000, 0.01250068083058953131, 0.04500063614458217620, 0.07750059145855550669, 0.1100005467725481551, 0.1425005020865408034, 0.1750004574005334379, 0.2075004127145260724, 0.2400003680285573704, 0.2725003233423954896, 0.3050002786564267598, 0.3375002339704580856, 0.3700001892844893003, 0.4025001445985205706, 0.4350000999123587730, 0.4675000552263899878, 0.5000000105404213135, 0.5324999658544524728, 0.5649999211682906752, 0.5974998764823219455, 0.6299998317963532157, 0.6624997871103845970, 0.6949997424244157562, 0.7274996977382539587, 0.7599996530522852289, 0.7924996083663163882, 0.8249995636803477694, 0.8574995189941858609, 0.8899994743082172421, 0.9224994296222484014, 0.9549993849362796716, 0.9874993402501176520, 1.000000000000000000 ),
 .UNSPECIFIED. ) ;
#4482 = CARTESIAN_POINT ( 'NONE',  ( -12.50000000000000000, -54.11762331445000029, -1.005384021965999963 ) ) ;
#4483 = CARTESIAN_POINT ( 'NONE',  ( 10.47020627418438643, -78.27083333333332860, 2.813789756862283387 ) ) ;
#4484 = CARTESIAN_POINT ( 'NONE',  ( -12.66314513616999982, -25.17864743362000013, -0.04033065750139999683 ) ) ;
#4485 = EDGE_LOOP ( 'NONE', ( #3054, #55026, #18370 ) ) ;
#4486 = VERTEX_POINT ( 'NONE', #47107 ) ;
#4487 = DIRECTION ( 'NONE',  ( -9.386985813191000447E-11, -1.000000000000000000, 5.363052387336999862E-10 ) ) ;
#4488 = CARTESIAN_POINT ( 'NONE',  ( 9.022242495772999860, -77.35293998579798824, -3.108016392540000172 ) ) ;
#4489 = EDGE_LOOP ( 'NONE', ( #53032, #31030, #48854, #29672 ) ) ;
#4490 = DIRECTION ( 'NONE',  ( 1.000000000000000000, 0.000000000000000000, 0.000000000000000000 ) ) ;
#4491 = ORIENTED_EDGE ( 'NONE', *, *, #56196, .T. ) ;
#4492 = CARTESIAN_POINT ( 'NONE',  ( 10.07616267220999973, -24.72631139030000114, 7.986947465007999014 ) ) ;
#4493 = ADVANCED_FACE ( 'NONE', ( #2223 ), #46977, .F. ) ;
#4494 = ADVANCED_FACE ( 'NONE', ( #39659 ), #30787, .F. ) ;
#4495 = CARTESIAN_POINT ( 'NONE',  ( -7.396918292183162436, -79.55208333333334281, -5.684557159767966716 ) ) ;
#4496 = CARTESIAN_POINT ( 'NONE',  ( 2.006136628026000235, -78.27093998579799461, -9.477164255927000625 ) ) ;
#4497 = CARTESIAN_POINT ( 'NONE',  ( -7.176767133925851638, -78.15496581618874927, -5.904501853725552252 ) ) ;
#4498 = CARTESIAN_POINT ( 'NONE',  ( 10.12058791103999944, -79.48379297370699703, 4.836508133599999759 ) ) ;
#4499 = CARTESIAN_POINT ( 'NONE',  ( 4.790152371929814912, -79.21780269203372882, -7.968054111795736638 ) ) ;
#4500 = ORIENTED_EDGE ( 'NONE', *, *, #43545, .T. ) ;
#4501 = ORIENTED_EDGE ( 'NONE', *, *, #1465, .T. ) ;
#4502 = CARTESIAN_POINT ( 'NONE',  ( 5.621132263311789501, -77.42329830751356212, 7.378911456533854718 ) ) ;
#4503 = CARTESIAN_POINT ( 'NONE',  ( 7.528714304401000312, -78.11486751746299717, -8.074838600060001426 ) ) ;
#4504 = CARTESIAN_POINT ( 'NONE',  ( 1.882180247600000245, -78.74992141025498427, 9.519879562373999349 ) ) ;
#4505 = CARTESIAN_POINT ( 'NONE',  ( 12.08658817094000071, -76.05461784646999490, -4.238831966694000641 ) ) ;
#4506 = CARTESIAN_POINT ( 'NONE',  ( -6.849002874435582200, -79.46067733726329152, -6.583439657378555410 ) ) ;
#4507 = CARTESIAN_POINT ( 'NONE',  ( 10.41144070831380120, -55.27453159746022493, -7.610433246081189651 ) ) ;
#4508 = CARTESIAN_POINT ( 'NONE',  ( -0.6023433875411666749, -79.42080894732758622, -9.578712713088513908 ) ) ;
#4509 = CARTESIAN_POINT ( 'NONE',  ( 12.54673671099000032, -17.17796527435999820, -0.9173654211231000444 ) ) ;
#4510 = CYLINDRICAL_SURFACE ( 'NONE', #28008, 1.750000000000000000 ) ;
#4511 = AXIS2_PLACEMENT_3D ( 'NONE', #58207, #22482, #21889 ) ;
#4512 = CARTESIAN_POINT ( 'NONE',  ( -11.51097801420635491, -76.68374859038704017, 2.357506540188898825 ) ) ;
#4513 = CARTESIAN_POINT ( 'NONE',  ( -3.579678601589999953, -85.86929758755698572, 0.3912085550186999994 ) ) ;
#4514 = EDGE_LOOP ( 'NONE', ( #8553, #135, #23406, #48612, #13860, #9789 ) ) ;
#4515 = CARTESIAN_POINT ( 'NONE',  ( -1.810985506639999798, -79.76004069920800532, 12.30075622849999917 ) ) ;
#4516 = CARTESIAN_POINT ( 'NONE',  ( 7.350255374610999759, -76.45613051119899239, -8.990260894034001637 ) ) ;
#4517 = CARTESIAN_POINT ( 'NONE',  ( -6.285277716731378028, -78.02485450714230808, 8.721419318336506521 ) ) ;
#4518 = CARTESIAN_POINT ( 'NONE',  ( 2.956870837876000468, -78.98874476440199999, 11.44999256673999888 ) ) ;
#4519 = CARTESIAN_POINT ( 'NONE',  ( -10.53559655343999957, -18.79430958026000198, 7.620036381602000475 ) ) ;
#4521 = DIRECTION ( 'NONE',  ( -3.552713678800000476E-14, -1.000000000000000000, 1.317464655887999919E-13 ) ) ;
#4520 = CARTESIAN_POINT ( 'NONE',  ( 11.44417895085271475, -78.52916666666665435, -3.075537641221520069 ) ) ;
#4522 = AXIS2_PLACEMENT_3D ( 'NONE', #40999, #46032, #1446 ) ;
#4523 = CARTESIAN_POINT ( 'NONE',  ( 3.380118192976000469, -86.40321104920799655, -1.504925579245999900 ) ) ;
#4524 = CARTESIAN_POINT ( 'NONE',  ( 1.648069335750886433, -80.96312284482743848, 10.62269281186031655 ) ) ;
#4525 = CARTESIAN_POINT ( 'NONE',  ( 10.04115011118999945, -59.56486430393999854, -7.682331425190000118 ) ) ;
#4526 = CARTESIAN_POINT ( 'NONE',  ( -8.300970689365446020, -78.34166666666668277, -4.784380313523547201 ) ) ;
#4527 = CARTESIAN_POINT ( 'NONE',  ( 10.94776161156000072, -77.15620299209300015, 2.097883759165000139 ) ) ;
#4528 = CARTESIAN_POINT ( 'NONE',  ( -3.250000000000000000, -2.000000000000000000, 0.000000000000000000 ) ) ;
#4529 = CARTESIAN_POINT ( 'NONE',  ( 10.87801983317999976, -80.69582220907369674, -1.798845711797000035 ) ) ;
#4530 = ORIENTED_EDGE ( 'NONE', *, *, #49929, .F. ) ;
#4531 = CARTESIAN_POINT ( 'NONE',  ( 3.089702623610774967, -78.34792614711045644, -10.47025075772299374 ) ) ;
#4532 = CARTESIAN_POINT ( 'NONE',  ( 0.006333666751320000086, -53.46737355666999747, 12.77652491951000080 ) ) ;
#4533 = CARTESIAN_POINT ( 'NONE',  ( 9.136202122873999798, -77.42194903538302242, 2.585973524421999237 ) ) ;
#4534 = CARTESIAN_POINT ( 'NONE',  ( -3.866967310333000007, -2.823463749271000189, -0.8818601717001000040 ) ) ;
#4535 = CARTESIAN_POINT ( 'NONE',  ( 1.508420534579999917, -77.56258324042499908, 11.11497989572000122 ) ) ;
#4536 = CARTESIAN_POINT ( 'NONE',  ( 0.8506806241676642122, -1.645833333333333037, -3.165411199172024848 ) ) ;
#4537 = CARTESIAN_POINT ( 'NONE',  ( 3.986964100386339638, -82.47708331396407289, 0.4532267925817293208 ) ) ;
#4538 = CARTESIAN_POINT ( 'NONE',  ( -1.995901252186330854, -2.028574367018873836, 2.598485926919212652 ) ) ;
#4539 = FACE_OUTER_BOUND ( 'NONE', #11687, .T. ) ;
#4540 = CARTESIAN_POINT ( 'NONE',  ( -3.894441588578999802, -83.34449735065199150, -1.504301970839000191 ) ) ;
#4541 = CARTESIAN_POINT ( 'NONE',  ( -10.79468190574739594, -76.05000000000001137, 4.801183946204664821 ) ) ;
#4542 = CARTESIAN_POINT ( 'NONE',  ( 11.69170080689889701, -76.72310112267754789, 3.011422183730339874 ) ) ;
#4543 = CARTESIAN_POINT ( 'NONE',  ( -1.762986776941000144, -79.36934499803000165, -12.35752141779000013 ) ) ;
#4544 = B_SPLINE_SURFACE_WITH_KNOTS ( 'NONE', 3, 3, ( 
 ( #25701, #8275, #12133, #16567 ),
 ( #21846, #43730, #3562, #49019 ),
 ( #12982, #30697, #34837, #20990 ),
 ( #30121, #39853, #21275, #26278 ),
 ( #38995, #44011, #16856, #52867 ),
 ( #12422, #21565, #4141, #57869 ),
 ( #17422, #44292, #57573, #34550 ),
 ( #22139, #39571, #17137, #25985 ) ),
 .UNSPECIFIED., .F., .F., .F.,
 ( 4, 1, 1, 1, 1, 4 ),
 ( 4, 4 ),
 ( -0.01200407347462999902, 0.000000000000000000, 0.3333333333333000081, 0.6666666666667000474, 1.000000000000000000, 1.011997855551999947 ),
 ( -0.3559705542741999906, 1.355970554273999928 ),
 .UNSPECIFIED. ) ;
#4545 = CARTESIAN_POINT ( 'NONE',  ( -7.835303970625000503, -78.21281986999699143, 8.089621514298000804 ) ) ;
#4546 = CARTESIAN_POINT ( 'NONE',  ( 1.520902128651999918, -80.98694329177000384, -0.6797894616744000196 ) ) ;
#4547 = CARTESIAN_POINT ( 'NONE',  ( 1.182381611807000077, -79.15875043768998864, -0.8124367623325000620 ) ) ;
#4548 = CARTESIAN_POINT ( 'NONE',  ( -1.318114156651510216, -61.53572477165713650, 12.70261578166483929 ) ) ;
#4549 = CARTESIAN_POINT ( 'NONE',  ( 0.6083220426053820296, -82.59209150926855614, 1.384507690863692408 ) ) ;
#4550 = CARTESIAN_POINT ( 'NONE',  ( -12.54983138332999815, -61.85098386317000063, 0.1356331847737999863 ) ) ;
#4551 = CARTESIAN_POINT ( 'NONE',  ( 0.000000000000000000, -80.99999999999998579, 0.000000000000000000 ) ) ;
#4552 = DIRECTION ( 'NONE',  ( 0.000000000000000000, -0.7071067811866525998, -0.7071067811864425456 ) ) ;
#4553 = CARTESIAN_POINT ( 'NONE',  ( -10.34340836277019449, -78.81829375771278023, 4.339989908386851170 ) ) ;
#4555 = EDGE_CURVE ( 'NONE', #24152, #11369, #34302, .T. ) ;
#4554 = AXIS2_PLACEMENT_3D ( 'NONE', #46213, #50636, #19039 ) ;
#4556 = CARTESIAN_POINT ( 'NONE',  ( 1.155696476636351555, -81.81899358315281745, -0.4761507332103875889 ) ) ;
#4557 = ADVANCED_FACE ( 'NONE', ( #9545 ), #11222, .F. ) ;
#4558 = CYLINDRICAL_SURFACE ( 'NONE', #42555, 12.50000000000000000 ) ;
#4559 = CARTESIAN_POINT ( 'NONE',  ( -11.13698119474000059, -79.89450301542969157, -0.4714344481541999921 ) ) ;
#4560 = DIRECTION ( 'NONE',  ( -1.000000000000000000, 0.000000000000000000, 0.000000000000000000 ) ) ;
#4561 = ORIENTED_EDGE ( 'NONE', *, *, #44622, .F. ) ;
#4562 = ORIENTED_EDGE ( 'NONE', *, *, #18886, .F. ) ;
#4563 = FACE_OUTER_BOUND ( 'NONE', #9355, .T. ) ;
#4564 = ORIENTED_EDGE ( 'NONE', *, *, #31426, .F. ) ;
#4565 = ORIENTED_EDGE ( 'NONE', *, *, #49843, .F. ) ;
#4566 = CARTESIAN_POINT ( 'NONE',  ( -1.758095523367999791, -18.27708336119999899, 12.57362173515999970 ) ) ;
#4567 = LINE ( 'NONE', #26395, #28221 ) ;
#4568 = AXIS2_PLACEMENT_3D ( 'NONE', #15408, #1848, #11568 ) ;
#4569 = CARTESIAN_POINT ( 'NONE',  ( 10.26699006316253637, -77.50833333333329733, -5.917523019358050362 ) ) ;
#4570 = EDGE_CURVE ( 'NONE', #20424, #56848, #43795, .T. ) ;
#4571 = CARTESIAN_POINT ( 'NONE',  ( 1.930009203935999951, -23.20099032317000365, -12.72537718777000038 ) ) ;
#4572 = CARTESIAN_POINT ( 'NONE',  ( -1.357398369685000050, -79.29145339669528880, -3.502682470260999992 ) ) ;
#4573 = CARTESIAN_POINT ( 'NONE',  ( -7.688125331226709491, -79.34962435731765140, 5.580139227232765009 ) ) ;
#4574 = CARTESIAN_POINT ( 'NONE',  ( 12.70556836343000029, -53.57227722738999631, -1.774194422348999890E-09 ) ) ;
#4575 = CARTESIAN_POINT ( 'NONE',  ( -12.20786306117000031, -78.92007912177000151, -0.2360786541355999746 ) ) ;
#4576 = EDGE_LOOP ( 'NONE', ( #27409, #54589, #29028, #21262 ) ) ;
#4577 = ORIENTED_EDGE ( 'NONE', *, *, #41177, .T. ) ;
#4578 = DIRECTION ( 'NONE',  ( 0.000000000000000000, -1.000000000000000000, 0.000000000000000000 ) ) ;
#4579 = CARTESIAN_POINT ( 'NONE',  ( -1.750000000001000089, -18.75000001325000198, -12.56594318051000059 ) ) ;
#4580 = CARTESIAN_POINT ( 'NONE',  ( -1.213636094208999872, -80.75588974632400152, -0.5527192377158001158 ) ) ;
#4581 = CARTESIAN_POINT ( 'NONE',  ( 3.248345031021000029, -78.05738370892098033, 9.144340540792999406 ) ) ;
#4582 = CARTESIAN_POINT ( 'NONE',  ( 2.668955399247460392, -86.25171438276200320, -3.748372073262821846 ) ) ;
#4584 = EDGE_CURVE ( 'NONE', #46717, #24388, #36398, .T. ) ;
#4583 = CARTESIAN_POINT ( 'NONE',  ( 10.12567350656000009, -76.18657555664699998, 4.748118780173999909 ) ) ;
#4585 = CARTESIAN_POINT ( 'NONE',  ( -1.332847799107999887, -78.03533949426000049, -12.88744032790000027 ) ) ;
#4586 = CARTESIAN_POINT ( 'NONE',  ( 1.288070761429999989, -80.35446191477998923, 0.4084665662698999666 ) ) ;
#4587 = EDGE_CURVE ( 'NONE', #18023, #822, #32139, .T. ) ;
#4588 = B_SPLINE_CURVE_WITH_KNOTS ( 'NONE', 3,
 ( #52525, #12367, #20653, #48396, #17372, #47830, #53102, #12082, #25077, #7933, #25934, #21795, #12651, #30644, #30064, #25646, #39799, #7361 ),
 .UNSPECIFIED., .F., .F.,
 ( 4, 2, 2, 2, 2, 2, 2, 2, 4 ),
 ( 0.000000000000000000, 0.1250000000000000000, 0.2500000000000000000, 0.3749999999999999445, 0.4999999999999998890, 0.6249999999999998890, 0.7499999999999998890, 0.8749999999999998890, 1.000000000000000000 ),
 .UNSPECIFIED. ) ;
#4589 = CARTESIAN_POINT ( 'NONE',  ( -10.38689113780999840, -77.00541705171700357, 2.826523783570000337 ) ) ;
#4590 = CARTESIAN_POINT ( 'NONE',  ( -0.8333782921101757779, -79.16723044587702418, -0.9320641449025461878 ) ) ;
#4591 = LINE ( 'NONE', #197, #1972 ) ;
#4592 = CARTESIAN_POINT ( 'NONE',  ( -2.684723000728000297, -77.10913667140100358, -9.133676008435999805 ) ) ;
#4593 = CARTESIAN_POINT ( 'NONE',  ( 3.755245102247999789, -79.53581372688118734, -1.719490641506999928 ) ) ;
#4594 = CARTESIAN_POINT ( 'NONE',  ( -0.9849936891751999157, -80.95192749954530598, -11.22225356808999841 ) ) ;
#4595 = DIRECTION ( 'NONE',  ( 0.7071067811865475727, 0.000000000000000000, -0.7071067811865475727 ) ) ;
#4596 = CARTESIAN_POINT ( 'NONE',  ( 10.13881649148000008, -76.90783510652001098, -5.938594122520999719 ) ) ;
#4597 = CARTESIAN_POINT ( 'NONE',  ( -13.49939038839240979, -9.295797029142999435, -0.1282931867975413143 ) ) ;
#4598 = CARTESIAN_POINT ( 'NONE',  ( -1.159125165887999964, -77.73513018121029461, 0.4678983327651999868 ) ) ;
#4599 = VECTOR ( 'NONE', #30627, 1000.000000000000000 ) ;
#4600 = CARTESIAN_POINT ( 'NONE',  ( -0.6747260877994001316, -82.22962677363800310, -1.052256958371999840 ) ) ;
#4601 = LINE ( 'NONE', #14310, #5260 ) ;
#4602 = CARTESIAN_POINT ( 'NONE',  ( 1.781953555039999859, -2.981106643931000111, -3.363141973650999983 ) ) ;
#4603 = CARTESIAN_POINT ( 'NONE',  ( 1.169602984591961103, -80.53296218476353374, 0.5073077260901295293 ) ) ;
#4604 = ORIENTED_EDGE ( 'NONE', *, *, #18299, .F. ) ;
#4605 = DIRECTION ( 'NONE',  ( 0.000000000000000000, -1.000000000000000000, 0.000000000000000000 ) ) ;
#4606 = CARTESIAN_POINT ( 'NONE',  ( -9.611650271896850839, -79.15833333333331723, 5.539808784079868431 ) ) ;
#4607 = CARTESIAN_POINT ( 'NONE',  ( -0.5935892672256000147, -82.17736815163898711, 1.194249225580000129 ) ) ;
#4608 = CARTESIAN_POINT ( 'NONE',  ( 2.062670899148999926, -60.10639625617000092, 12.83044039277999993 ) ) ;
#4609 = CARTESIAN_POINT ( 'NONE',  ( 7.349802007153999561, -77.69009527504000800, -10.73869877321999944 ) ) ;
#4610 = B_SPLINE_CURVE_WITH_KNOTS ( 'NONE', 3,
 ( #49132, #8684, #4260, #22256, #58282, #17845, #53861, #31395, #49435, #22559, #40570, #163, #18138, #54150, #9276, #27265, #24601, #37879 ),
 .UNSPECIFIED., .F., .F.,
 ( 4, 2, 2, 2, 2, 2, 2, 2, 4 ),
 ( 0.000000000000000000, 0.1250000000000000000, 0.2500000000000000000, 0.3750000000000000000, 0.5000000000000000000, 0.6250000000000000000, 0.7500000000000000000, 0.8750000000000000000, 1.000000000000000000 ),
 .UNSPECIFIED. ) ;
#4611 = CARTESIAN_POINT ( 'NONE',  ( 9.504033308897000154, -79.32516001420199814, 0.5380116381770999601 ) ) ;
#4612 = CARTESIAN_POINT ( 'NONE',  ( 12.49306764015999960, -23.28056535155999995, -1.667917367065999912 ) ) ;
#4613 = ORIENTED_EDGE ( 'NONE', *, *, #33823, .F. ) ;
#4614 = DIRECTION ( 'NONE',  ( 0.000000000000000000, 1.000000000000000000, 0.000000000000000000 ) ) ;
#4615 = CARTESIAN_POINT ( 'NONE',  ( 8.813906587775187873, -53.78989792558270722, -8.872948314069059705 ) ) ;
#4616 = CARTESIAN_POINT ( 'NONE',  ( 0.3790021828235000112, -81.15063363487499259, 1.356521486386000230 ) ) ;
#4617 = CARTESIAN_POINT ( 'NONE',  ( 3.350444873057258022, -79.30441504825350307, -8.644740048361368778 ) ) ;
#4618 = CARTESIAN_POINT ( 'NONE',  ( 9.086766343481999186, -79.24979041159998872, -2.458053382951000287 ) ) ;
#4620 = CARTESIAN_POINT ( 'NONE',  ( 2.627446458840999810, -1.670251425905000087, 3.037392460054000320 ) ) ;
#4619 = CARTESIAN_POINT ( 'NONE',  ( 3.437033289993999929, -82.13767524227699823, -1.965227161882999951 ) ) ;
#4621 = CARTESIAN_POINT ( 'NONE',  ( -1.931087888049999979, -60.11584477251999203, -12.71658889743999943 ) ) ;
#4622 = CARTESIAN_POINT ( 'NONE',  ( 1.112922243992000126, -79.73790229619299907, -1.029731144982999780 ) ) ;
#4623 = ORIENTED_EDGE ( 'NONE', *, *, #23582, .T. ) ;
#4624 = CARTESIAN_POINT ( 'NONE',  ( 0.03815395216748320578, -77.22536730000003047, -10.74989112016262993 ) ) ;
#4625 = CARTESIAN_POINT ( 'NONE',  ( 0.000000000000000000, 4.040000000000000036, 0.000000000000000000 ) ) ;
#4626 = CARTESIAN_POINT ( 'NONE',  ( -3.999999999999708233, -78.70000000000000284, 7.999999999999366729 ) ) ;
#4627 = ORIENTED_EDGE ( 'NONE', *, *, #21672, .T. ) ;
#4628 = VERTEX_POINT ( 'NONE', #6485 ) ;
#4629 = DIRECTION ( 'NONE',  ( 0.000000000000000000, 1.000000000000000000, 0.000000000000000000 ) ) ;
#4630 = CARTESIAN_POINT ( 'NONE',  ( -1.548298113504216866, -76.12161458261024904, -11.82161455805163719 ) ) ;
#4631 = CARTESIAN_POINT ( 'NONE',  ( -2.981173517641313886, -80.39728512301172714, 10.37580895950596904 ) ) ;
#4632 = ORIENTED_EDGE ( 'NONE', *, *, #42622, .F. ) ;
#4633 = CARTESIAN_POINT ( 'NONE',  ( 3.237243043699999934, -78.77026847289599232, -11.48719983142999901 ) ) ;
#4634 = ORIENTED_EDGE ( 'NONE', *, *, #8150, .F. ) ;
#4635 = VERTEX_POINT ( 'NONE', #7068 ) ;
#4636 = CARTESIAN_POINT ( 'NONE',  ( -3.249653326647542251, -2.606879814458876066, -0.2573833159217454591 ) ) ;
#4637 = AXIS2_PLACEMENT_3D ( 'NONE', #4300, #41192, #17889 ) ;
#4638 = EDGE_CURVE ( 'NONE', #15196, #6738, #29388, .T. ) ;
#4639 = CARTESIAN_POINT ( 'NONE',  ( 11.00000000000000000, -79.44999999999998863, 0.000000000000000000 ) ) ;
#4640 = CARTESIAN_POINT ( 'NONE',  ( 2.303718438183066208, -1.521409140963204676, -3.294797006952866258 ) ) ;
#4641 = ORIENTED_EDGE ( 'NONE', *, *, #55762, .T. ) ;
#4642 = CARTESIAN_POINT ( 'NONE',  ( 1.500000000000000000, -81.65000000000000568, 0.000000000000000000 ) ) ;
#4643 = B_SPLINE_CURVE_WITH_KNOTS ( 'NONE', 3,
 ( #58141, #35695, #320, #18297, #14432, #18877, #23878, #55178, #19170, #50769 ),
 .UNSPECIFIED., .F., .F.,
 ( 4, 2, 2, 2, 4 ),
 ( 0.5000000007922399403, 0.6250000005941799275, 0.7500000003961200257, 0.8750000001980600128, 1.000000000000000000 ),
 .UNSPECIFIED. ) ;
#4644 = ORIENTED_EDGE ( 'NONE', *, *, #19378, .T. ) ;
#4645 = CARTESIAN_POINT ( 'NONE',  ( 9.250000000000000000, -79.34999999999999432, 0.000000000000000000 ) ) ;
#4646 = AXIS2_PLACEMENT_3D ( 'NONE', #43309, #2866, #12295 ) ;
#4647 = CARTESIAN_POINT ( 'NONE',  ( -11.02098641988770034, -79.79999999999999716, -4.612498697062771491 ) ) ;
#4648 = CARTESIAN_POINT ( 'NONE',  ( 1.500000000000000000, -77.50000000000000000, 0.000000000000000000 ) ) ;
#4649 = VECTOR ( 'NONE', #40281, 1000.000000000000114 ) ;
#4650 = CARTESIAN_POINT ( 'NONE',  ( -7.654537085030000299, -23.28056692670000061, -10.01332844637000008 ) ) ;
#4651 = DIRECTION ( 'NONE',  ( 0.000000000000000000, -1.000000000000000000, 0.000000000000000000 ) ) ;
#4652 = LINE ( 'NONE', #58075, #37418 ) ;
#4653 = ADVANCED_FACE ( 'NONE', ( #11510 ), #16523, .F. ) ;
#4654 = CARTESIAN_POINT ( 'NONE',  ( -1.835125225091999823, -78.03723861434511377, 11.83842809849000410 ) ) ;
#4655 = CARTESIAN_POINT ( 'NONE',  ( 0.1948337121880240608, -78.72684273210919059, -9.247945775061792162 ) ) ;
#4656 = CARTESIAN_POINT ( 'NONE',  ( 5.246383657897999875, -77.06100733245999379, -10.79237965019999912 ) ) ;
#4657 = CARTESIAN_POINT ( 'NONE',  ( -10.47840054245999930, -23.78693148451999662, 7.622763498569999463 ) ) ;
#4658 = CARTESIAN_POINT ( 'NONE',  ( 11.00000000000000000, -78.34999999999999432, 0.000000000000000000 ) ) ;
#4659 = CARTESIAN_POINT ( 'NONE',  ( -9.396085398178650294, -76.74791666666666856, 7.220923959705211281 ) ) ;
#4660 = CARTESIAN_POINT ( 'NONE',  ( 3.936869704505999490, -80.97450264934799691, 1.389480733867999751 ) ) ;
#4661 = CARTESIAN_POINT ( 'NONE',  ( -5.497893974011999418, -77.39866001420199382, -8.200266008636999615 ) ) ;
#4662 = CARTESIAN_POINT ( 'NONE',  ( 0.6809358820633165665, -79.67024612424833663, -1.063416950850958331 ) ) ;
#4663 = DIRECTION ( 'NONE',  ( -0.7071067811865475727, 0.000000000000000000, -0.7071067811865475727 ) ) ;
#4664 = CARTESIAN_POINT ( 'NONE',  ( 0.5045596072230998930, -25.13528913037999857, 12.66210649709999991 ) ) ;
#4665 = CARTESIAN_POINT ( 'NONE',  ( -0.4149502389179186013, -81.15050653439624284, 1.258535203000175295 ) ) ;
#4666 = CARTESIAN_POINT ( 'NONE',  ( 3.437841776182999798, -84.02832601947699231, 0.8751022178784999550 ) ) ;
#4667 = CARTESIAN_POINT ( 'NONE',  ( 2.081885476966999882, -0.9615064129436999840, -3.558236660806000096 ) ) ;
#4668 = CARTESIAN_POINT ( 'NONE',  ( -6.188001695094492050, -79.71856730628915955, -7.220675648484128573 ) ) ;
#4669 = PRODUCT_DEFINITION_FORMATION_WITH_SPECIFIED_SOURCE ( 'ANY', '', #40385, .NOT_KNOWN. ) ;
#4670 = CARTESIAN_POINT ( 'NONE',  ( 1.385745491928287665, -80.63676124254567412, 0.6939760826984652242 ) ) ;
#4671 = CARTESIAN_POINT ( 'NONE',  ( -0.9326541099288512271, -78.54231991824191539, 0.8322237885996108808 ) ) ;
#4672 = DIRECTION ( 'NONE',  ( 0.000000000000000000, 1.000000000000000000, 0.000000000000000000 ) ) ;
#4673 = DIRECTION ( 'NONE',  ( -1.000000000000000000, 0.000000000000000000, 0.000000000000000000 ) ) ;
#4674 = ADVANCED_FACE ( 'NONE', ( #31954 ), #27528, .T. ) ;
#4675 = CARTESIAN_POINT ( 'NONE',  ( -3.419437234775999812, -78.62623792800799549, -10.36738907398999920 ) ) ;
#4676 = CARTESIAN_POINT ( 'NONE',  ( -0.08732773870155000062, -78.24897531865799749, 12.27958277169999945 ) ) ;
#4677 = CARTESIAN_POINT ( 'NONE',  ( -6.364729966985086307, -78.17625342220868845, -9.067865724216229495 ) ) ;
#4678 = VECTOR ( 'NONE', #2965, 1000.000000000000000 ) ;
#4680 = CARTESIAN_POINT ( 'NONE',  ( -0.9728543758959999899, -78.36213479155139794, -1.031316509929999903 ) ) ;
#4679 = CARTESIAN_POINT ( 'NONE',  ( -12.00000000000000000, -78.89999999999999147, -1.868256502752000067E-14 ) ) ;
#4681 = ORIENTED_EDGE ( 'NONE', *, *, #7435, .F. ) ;
#4682 = CARTESIAN_POINT ( 'NONE',  ( -3.504176354730999865, -83.59271544543099708, -1.353554617958000028 ) ) ;
#4683 = CARTESIAN_POINT ( 'NONE',  ( 0.3693169358421000137, -79.94575047619699149, 11.04974602993000055 ) ) ;
#4684 = DIRECTION ( 'NONE',  ( 1.000000000000000000, 0.000000000000000000, 0.000000000000000000 ) ) ;
#4685 = PLANE ( 'NONE',  #14153 ) ;
#4686 = CARTESIAN_POINT ( 'NONE',  ( -10.18949719147000010, -60.01529250184999853, 7.645392405676999736 ) ) ;
#4687 = CARTESIAN_POINT ( 'NONE',  ( 1.889053048974999927, -78.68865341057399121, 9.554641504766999915 ) ) ;
#4688 = VECTOR ( 'NONE', #2380, 999.9999999999998863 ) ;
#4689 = CARTESIAN_POINT ( 'NONE',  ( -10.33814977949000102, -77.20682288379001079, 7.275158806450000348 ) ) ;
#4690 = CARTESIAN_POINT ( 'NONE',  ( 8.862101803403000133, -79.48419127858598188, -4.393033378783998799 ) ) ;
#4691 = CARTESIAN_POINT ( 'NONE',  ( 12.59651352881000008, -23.39056208384000257, -1.801710201210000140 ) ) ;
#4692 = DIRECTION ( 'NONE',  ( -0.7592504785508227272, -0.04890181650118147205, 0.6489586451872195738 ) ) ;
#4693 = VERTEX_POINT ( 'NONE', #34780 ) ;
#4694 = CARTESIAN_POINT ( 'NONE',  ( 0.000000000000000000, -0.09999999995300053179, 0.000000000000000000 ) ) ;
#4695 = AXIS2_PLACEMENT_3D ( 'NONE', #54251, #53073, #48652 ) ;
#4696 = CARTESIAN_POINT ( 'NONE',  ( -5.083316206963999662, -79.77331332859898794, -8.054784978366999582 ) ) ;
#4697 = DIRECTION ( 'NONE',  ( 0.000000000000000000, -1.000000000000000000, 0.000000000000000000 ) ) ;
#4698 = CARTESIAN_POINT ( 'NONE',  ( 1.500000000000000000, -81.65000000000000568, 0.000000000000000000 ) ) ;
#4699 = CARTESIAN_POINT ( 'NONE',  ( -2.281219053130000063, -83.38942953870899544, -2.716724548313999676 ) ) ;
#4700 = B_SPLINE_CURVE_WITH_KNOTS ( 'NONE', 3,
 ( #48001, #26107, #52128, #2534, #29376, #16974, #29662, #21682, #7243, #25248, #7823, #47423, #57695, #2821, #20816, #21393, #20537, #52986, #43852, #34670, #12537, #38823, #39687, #3398, #38534, #17251, #48567, #48285, #6953, #24958 ),
 .UNSPECIFIED., .F., .F.,
 ( 4, 2, 2, 2, 2, 2, 2, 2, 2, 2, 2, 2, 2, 2, 4 ),
 ( 0.000000000000000000, 0.1249999999999988343, 0.1874999999999990286, 0.2499999999999992228, 0.3124999999999993894, 0.3749999999999996114, 0.5000000000000005551, 0.5625000000000009992, 0.6250000000000014433, 0.6875000000000019984, 0.7500000000000025535, 0.8125000000000031086, 0.8437500000000033307, 0.8750000000000035527, 1.000000000000000000 ),
 .UNSPECIFIED. ) ;
#4701 = CARTESIAN_POINT ( 'NONE',  ( 10.98753362943493883, -23.45184359403916829, 0.5244447725534562288 ) ) ;
#4702 = VERTEX_POINT ( 'NONE', #3786 ) ;
#4703 = CARTESIAN_POINT ( 'NONE',  ( 3.757612933477000094, -77.84086580624799012, 10.56348085686000005 ) ) ;
#4704 = CARTESIAN_POINT ( 'NONE',  ( -1.931043762602999925, -22.77819125662999866, 12.75761570867000039 ) ) ;
#4705 = ORIENTED_EDGE ( 'NONE', *, *, #19301, .T. ) ;
#4706 = CARTESIAN_POINT ( 'NONE',  ( -7.633088938737000007, -55.40992532391999958, -10.18115029110999892 ) ) ;
#4707 = EDGE_CURVE ( 'NONE', #34022, #43554, #33497, .T. ) ;
#4708 = CARTESIAN_POINT ( 'NONE',  ( 3.366547962069000199, -79.48315413024698728, -9.168809063548000182 ) ) ;
#4709 = EDGE_LOOP ( 'NONE', ( #33523, #24387, #15603, #32761 ) ) ;
#4710 = CARTESIAN_POINT ( 'NONE',  ( 9.371326875074000640, -76.81784402283000190, -7.865448804155000140 ) ) ;
#4711 = CARTESIAN_POINT ( 'NONE',  ( -9.133843623092825936, -78.64447737370456082, -5.680053951677152213 ) ) ;
#4712 = ADVANCED_FACE ( 'NONE', ( #38646 ), #39510, .F. ) ;
#4713 = CARTESIAN_POINT ( 'NONE',  ( 0.3051819181680999749, -78.56572944923000534, 1.504208664230000103 ) ) ;
#4714 = ORIENTED_EDGE ( 'NONE', *, *, #32564, .F. ) ;
#4715 = CARTESIAN_POINT ( 'NONE',  ( 9.475051992780000987, -77.81477305011499368, -0.6170397550469999270 ) ) ;
#4716 = CARTESIAN_POINT ( 'NONE',  ( 0.08493805541549671878, -80.23085499046800351, -1.247011083204105919 ) ) ;
#4717 = CARTESIAN_POINT ( 'NONE',  ( -13.07317008567999927, -77.50062674423000431, -1.028553310913000063 ) ) ;
#4718 = CARTESIAN_POINT ( 'NONE',  ( -10.48543666025109111, -78.84166666666665435, -6.043427764450793660 ) ) ;
#4719 = CARTESIAN_POINT ( 'NONE',  ( 3.241578942234842220, -86.36264282632899381, -1.443243930775356176 ) ) ;
#4720 = CARTESIAN_POINT ( 'NONE',  ( -9.626984307556000431, -78.23995771838823998, 1.221426423741999834 ) ) ;
#4721 = CARTESIAN_POINT ( 'NONE',  ( 7.994721076134334581, -79.89245675932635038, 4.654034487047796098 ) ) ;
#4722 = EDGE_CURVE ( 'NONE', #29661, #34312, #8215, .T. ) ;
#4723 = CARTESIAN_POINT ( 'NONE',  ( 1.734545068753198915, -79.18177081765752234, -3.617932226706877863 ) ) ;
#4724 = VERTEX_POINT ( 'NONE', #16506 ) ;
#4725 = CARTESIAN_POINT ( 'NONE',  ( -9.350291827225385433, -77.23092893528344405, 2.280442541072182916 ) ) ;
#4726 = CARTESIAN_POINT ( 'NONE',  ( -1.476182556144000069, -76.43656575806998887, 12.22114576030999977 ) ) ;
#4727 = CARTESIAN_POINT ( 'NONE',  ( -1.487176594838000021, -80.83707595801799073, 0.2955346688291999868 ) ) ;
#4728 = B_SPLINE_SURFACE_WITH_KNOTS ( 'NONE', 3, 3, ( 
 ( #9036, #27023, #22012, #58035 ),
 ( #49185, #17595, #49784, #53611 ),
 ( #13150, #45355, #53316, #30861 ),
 ( #18481, #40621, #31144, #8736 ),
 ( #26729, #4308, #22308, #40323 ),
 ( #58334, #35886, #53916, #13448 ),
 ( #31446, #49488, #45059, #4612 ),
 ( #218, #18194, #13741, #36188 ) ),
 .UNSPECIFIED., .F., .F., .F.,
 ( 4, 1, 1, 1, 1, 4 ),
 ( 4, 4 ),
 ( -0.01200407345745999922, 0.000000000000000000, 0.3333333333333000081, 0.6666666666667000474, 1.000000000000000000, 1.011997855551999947 ),
 ( -0.3559705542741000150, 1.355970554273999928 ),
 .UNSPECIFIED. ) ;
#4729 = CIRCLE ( 'NONE', #15084, 14.00000000000000000 ) ;
#4730 = LINE ( 'NONE', #54894, #36062 ) ;
#4731 = FACE_OUTER_BOUND ( 'NONE', #55790, .T. ) ;
#4732 = DIRECTION ( 'NONE',  ( 0.000000000000000000, 1.000000000000000000, 0.000000000000000000 ) ) ;
#4733 = CARTESIAN_POINT ( 'NONE',  ( 7.439427647571000612, -79.74001771131699456, -8.315438409070999626 ) ) ;
#4734 = CARTESIAN_POINT ( 'NONE',  ( -4.454645851891000596, -77.35638832859899594, 8.536186251725998986 ) ) ;
#4735 = CARTESIAN_POINT ( 'NONE',  ( 12.02803943743313475, -76.79341500456992264, -1.008114833370821417 ) ) ;
#4736 = CARTESIAN_POINT ( 'NONE',  ( 0.000000000000000000, -76.15000000005198899, 0.000000000000000000 ) ) ;
#4737 = ORIENTED_EDGE ( 'NONE', *, *, #37279, .T. ) ;
#4738 = CARTESIAN_POINT ( 'NONE',  ( -0.7208041749482999583, -83.30589043469399257, 1.412512638229999951 ) ) ;
#4739 = CARTESIAN_POINT ( 'NONE',  ( 0.3269278782881216983, -78.74609622332656045, -1.249941949099096172 ) ) ;
#4740 = CARTESIAN_POINT ( 'NONE',  ( -1.500000000000000000, -80.50000000000000000, 0.000000000000000000 ) ) ;
#4741 = CARTESIAN_POINT ( 'NONE',  ( -1.250000000000000000, -79.00000000000000000, 0.000000000000000000 ) ) ;
#4742 = CARTESIAN_POINT ( 'NONE',  ( 8.534835205664490942, -77.00000000000000000, 3.862497297122138296 ) ) ;
#4743 = CARTESIAN_POINT ( 'NONE',  ( 0.000000000000000000, -87.20000000000000284, -10.05000000000000071 ) ) ;
#4744 = DIRECTION ( 'NONE',  ( 0.000000000000000000, -1.000000000000000000, 0.000000000000000000 ) ) ;
#4745 = CARTESIAN_POINT ( 'NONE',  ( 0.01248279339869594502, -76.07459138074202087, 11.74977687581417918 ) ) ;
#4746 = CARTESIAN_POINT ( 'NONE',  ( 3.281228840419999848, -79.67588468523199197, -10.41195962760999905 ) ) ;
#4747 = LINE ( 'NONE', #27161, #40774 ) ;
#4748 = ORIENTED_EDGE ( 'NONE', *, *, #15022, .T. ) ;
#4749 = FACE_OUTER_BOUND ( 'NONE', #15583, .T. ) ;
#4750 = CARTESIAN_POINT ( 'NONE',  ( -2.042798770927881868, -78.62148120184446043, -3.387993206663131307 ) ) ;
#4751 = CIRCLE ( 'NONE', #48129, 1.750000000000000000 ) ;
#4752 = CARTESIAN_POINT ( 'NONE',  ( -10.96673197750000206, -78.43335242178798694, -0.4413686857046000278 ) ) ;
#4753 = CARTESIAN_POINT ( 'NONE',  ( -0.8338927958969792886, -17.19946422253764950, -12.50366901602889058 ) ) ;
#4754 = CARTESIAN_POINT ( 'NONE',  ( -12.29672256689999976, -75.88792199503599534, -2.267527262250000231 ) ) ;
#4755 = DIRECTION ( 'NONE',  ( -1.000000000000000000, 0.000000000000000000, 0.000000000000000000 ) ) ;
#4756 = CARTESIAN_POINT ( 'NONE',  ( -6.417398495783289469, -76.92555371511903672, 8.714208636181064449 ) ) ;
#4757 = ORIENTED_EDGE ( 'NONE', *, *, #13222, .T. ) ;
#4758 = EDGE_CURVE ( 'NONE', #43330, #15471, #11791, .T. ) ;
#4759 = CARTESIAN_POINT ( 'NONE',  ( 10.67847671903000162, -80.05232057427369341, 3.578272902691999491 ) ) ;
#4760 = CARTESIAN_POINT ( 'NONE',  ( 12.74331394910317705, -18.47353206583634844, 1.980611464662580756 ) ) ;
#4761 = CARTESIAN_POINT ( 'NONE',  ( 6.760013919724077169, -77.77708333333333712, -8.796335266379973206 ) ) ;
#4762 = CARTESIAN_POINT ( 'NONE',  ( 3.778552491321000684, -78.40681307243320930, 2.230001049574967809 ) ) ;
#4764 = CARTESIAN_POINT ( 'NONE',  ( -1.156132896548696776, -81.56914977956330404, 0.4749676188561988144 ) ) ;
#4763 = CARTESIAN_POINT ( 'NONE',  ( -0.6992687060550999423, -81.07751218924100556, 1.118744323162000009 ) ) ;
#4765 =( REPRESENTATION_RELATIONSHIP ('NONE','NONE', #58051, #52046 ) REPRESENTATION_RELATIONSHIP_WITH_TRANSFORMATION ( #11623 )SHAPE_REPRESENTATION_RELATIONSHIP( ) );
#4766 = CARTESIAN_POINT ( 'NONE',  ( 10.14733453800999996, -78.52718663188798587, 4.639310447764000145 ) ) ;
#4767 = CARTESIAN_POINT ( 'NONE',  ( -2.251292830498186071, -76.39166666666665151, 10.57172952794456933 ) ) ;
#4768 = CARTESIAN_POINT ( 'NONE',  ( 1.077757070171020848, -81.53756520157187992, -1.059880615153325989 ) ) ;
#4769 = AXIS2_PLACEMENT_3D ( 'NONE', #10364, #45813, #36054 ) ;
#4770 = CARTESIAN_POINT ( 'NONE',  ( 11.00000000000000000, -74.59999999999999432, 0.000000000000000000 ) ) ;
#4771 = CARTESIAN_POINT ( 'NONE',  ( 10.74999999999999645, -79.26041666666667140, 1.407171709420451666 ) ) ;
#4772 = CARTESIAN_POINT ( 'NONE',  ( 8.596418555780418913, -78.30208333333331439, 6.606377239730356621 ) ) ;
#4773 = CARTESIAN_POINT ( 'NONE',  ( 12.50000000000000000, -18.75000000000000000, 0.000000000000000000 ) ) ;
#4774 = ORIENTED_EDGE ( 'NONE', *, *, #10261, .F. ) ;
#4775 = ORIENTED_EDGE ( 'NONE', *, *, #51729, .T. ) ;
#4776 = CARTESIAN_POINT ( 'NONE',  ( -2.486604901413153268, -78.50416666666667709, -9.252740428348998236 ) ) ;
#4777 = EDGE_CURVE ( 'NONE', #308, #37604, #44874, .T. ) ;
#4778 = ORIENTED_EDGE ( 'NONE', *, *, #43702, .T. ) ;
#4779 = DIRECTION ( 'NONE',  ( 0.000000000000000000, 1.000000000000000000, 0.000000000000000000 ) ) ;
#4780 = ORIENTED_EDGE ( 'NONE', *, *, #35176, .T. ) ;
#4781 = CARTESIAN_POINT ( 'NONE',  ( 3.420569553252711614, -82.47708335033021854, 0.3941913140830599627 ) ) ;
#4782 = CARTESIAN_POINT ( 'NONE',  ( 1.483539930421000186, -77.50540253813299785, 10.93164414240999882 ) ) ;
#4783 = CARTESIAN_POINT ( 'NONE',  ( 7.364280830341206396, -55.45989902438520858, -8.171144579308812439 ) ) ;
#4784 = CARTESIAN_POINT ( 'NONE',  ( 9.685875573750999834, -78.88063998579799829, 0.1582452683012000039 ) ) ;
#4785 = CARTESIAN_POINT ( 'NONE',  ( -5.555214266092813880, -78.17374655601618372, -7.396475742313247004 ) ) ;
#4786 = CARTESIAN_POINT ( 'NONE',  ( 10.05828973332000054, -78.97961832394499027, -4.964767691657000270 ) ) ;
#4787 = DIRECTION ( 'NONE',  ( 0.000000000000000000, 0.000000000000000000, -1.000000000000000000 ) ) ;
#4788 = ADVANCED_FACE ( 'NONE', ( #48107 ), #56878, .F. ) ;
#4789 = ORIENTED_EDGE ( 'NONE', *, *, #26674, .T. ) ;
#4790 = CARTESIAN_POINT ( 'NONE',  ( -10.98754182310630334, -18.54785535411248176, 0.5242772304794532934 ) ) ;
#4791 = AXIS2_PLACEMENT_3D ( 'NONE', #45431, #35659, #40698 ) ;
#4792 = ORIENTED_EDGE ( 'NONE', *, *, #40805, .T. ) ;
#4793 = CARTESIAN_POINT ( 'NONE',  ( 1.552764912756553706, -77.46160601996280093, 9.119532399810527323 ) ) ;
#4794 = CARTESIAN_POINT ( 'NONE',  ( 2.386167682861000117, -77.34811801783499163, 10.77916482977000001 ) ) ;
#4795 = ADVANCED_FACE ( 'NONE', ( #4064 ), #4369, .F. ) ;
#4796 = DIRECTION ( 'NONE',  ( 0.000000000000000000, 0.000000000000000000, 1.000000000000000000 ) ) ;
#4797 = CARTESIAN_POINT ( 'NONE',  ( -7.203390125892000562, -78.94888821415699454, -6.502451851937000704 ) ) ;
#4798 = CARTESIAN_POINT ( 'NONE',  ( -9.820549435267999172, -76.56333523746999958, -8.704928227648998984 ) ) ;
#4799 = CARTESIAN_POINT ( 'NONE',  ( -9.380299113924060350, -79.41227555779782676, -1.501938252706041643 ) ) ;
#4800 = CARTESIAN_POINT ( 'NONE',  ( 0.1429208184976999974, -78.63839451269998904, 1.621183732314999792 ) ) ;
#4801 = CARTESIAN_POINT ( 'NONE',  ( 0.000000000000000000, -77.00000000000000000, 0.000000000000000000 ) ) ;
#4802 = CARTESIAN_POINT ( 'NONE',  ( 9.949629901056999515, -78.71331089110499590, 4.548920879513999260 ) ) ;
#4803 = DIRECTION ( 'NONE',  ( 0.000000000000000000, 0.000000000000000000, 1.000000000000000000 ) ) ;
#4804 = CARTESIAN_POINT ( 'NONE',  ( 0.000000000000000000, -81.10000000285099020, -7.000000000000000000 ) ) ;
#4805 = CARTESIAN_POINT ( 'NONE',  ( 1.095285505811000037, -84.19350903806798669, 3.371249143215000021 ) ) ;
#4806 = EDGE_LOOP ( 'NONE', ( #34896, #44549, #17753, #49884 ) ) ;
#4807 = CARTESIAN_POINT ( 'NONE',  ( -11.92000176286999924, -78.99177042599900744, 2.600513710866999784 ) ) ;
#4808 = AXIS2_PLACEMENT_3D ( 'NONE', #22983, #13230, #40700 ) ;
#4809 = CARTESIAN_POINT ( 'NONE',  ( -9.323141007194999830, -76.18968473043899792, -6.517165561429999698 ) ) ;
#4810 = CARTESIAN_POINT ( 'NONE',  ( -4.144776331383936530, -78.00651457564580937, 9.918828337007836282 ) ) ;
#4811 = CARTESIAN_POINT ( 'NONE',  ( 1.720939166139000109, -77.33834334083999806, -11.69973432676000158 ) ) ;
#4812 = LINE ( 'NONE', #5387, #11801 ) ;
#4813 = AXIS2_PLACEMENT_3D ( 'NONE', #50698, #23518, #5800 ) ;
#4814 = CARTESIAN_POINT ( 'NONE',  ( -9.393376654192294950, -79.05850173436991213, 5.414072594118386483 ) ) ;
#4815 = PRODUCT_DEFINITION ( 'UNKNOWN', '', #22577, #7968 ) ;
#4816 = CARTESIAN_POINT ( 'NONE',  ( 3.518657424385000176, -86.36264283715698298, -1.566607219110000004 ) ) ;
#4817 = CARTESIAN_POINT ( 'NONE',  ( 5.710891535341052538, -80.93086402315771011, 9.111465207288862445 ) ) ;
#4818 = CARTESIAN_POINT ( 'NONE',  ( 10.01234990230000044, -60.09849137196000157, -7.653559502293999728 ) ) ;
#4819 = FACE_OUTER_BOUND ( 'NONE', #23078, .T. ) ;
#4820 = CARTESIAN_POINT ( 'NONE',  ( 0.1384068119873000102, -77.26514836410099463, 11.14609546546000018 ) ) ;
#4821 = CARTESIAN_POINT ( 'NONE',  ( 9.596002108778145967, -78.10208333333332575, 7.374560639699001996 ) ) ;
#4822 = CARTESIAN_POINT ( 'NONE',  ( -6.536208127187000727, -80.81602894668615988, 9.021928177040001273 ) ) ;
#4823 = ORIENTED_EDGE ( 'NONE', *, *, #19680, .T. ) ;
#4824 = CARTESIAN_POINT ( 'NONE',  ( -0.5390150933986999071, -53.53739108314999839, 12.77520260999999913 ) ) ;
#4825 = CARTESIAN_POINT ( 'NONE',  ( 7.430757984335999211, -77.45347403538301023, 5.911115298933000695 ) ) ;
#4826 = CARTESIAN_POINT ( 'NONE',  ( -10.03846658012971993, -23.79367507167474471, 7.678639819101479524 ) ) ;
#4827 = CARTESIAN_POINT ( 'NONE',  ( -11.21668965365999959, -77.69876495543400097, -0.06311738993059998193 ) ) ;
#4828 = CARTESIAN_POINT ( 'NONE',  ( 1.500000000000000000, -79.65000000000000568, 0.000000000000000000 ) ) ;
#4829 = CARTESIAN_POINT ( 'NONE',  ( 9.393285425842218928, -76.89183432704838594, 5.414042684532392791 ) ) ;
#4830 = CARTESIAN_POINT ( 'NONE',  ( 3.936689796931376772, -82.49635414750480322, 0.7746042215944272114 ) ) ;
#4831 = CARTESIAN_POINT ( 'NONE',  ( -8.779106447692180737, -78.54927823582298174, -6.259569139016079475 ) ) ;
#4832 = CARTESIAN_POINT ( 'NONE',  ( 12.49830607528000037, -18.79028586434999681, 1.666977523253999838 ) ) ;
#4833 = EDGE_CURVE ( 'NONE', #44267, #28437, #28775, .T. ) ;
#4834 = CARTESIAN_POINT ( 'NONE',  ( -3.413427344757999915, -86.03492953870899385, 2.398873957536999946 ) ) ;
#4835 = CARTESIAN_POINT ( 'NONE',  ( 5.137083998358000336, -77.31100733245999379, -10.56753840748999984 ) ) ;
#4836 = B_SPLINE_CURVE_WITH_KNOTS ( 'NONE', 3,
 ( #22588, #44739, #9017, #22290 ),
 .UNSPECIFIED., .F., .F.,
 ( 4, 4 ),
 ( 0.000000000000000000, 0.2499999978686767710 ),
 .UNSPECIFIED. ) ;
#4837 = EDGE_CURVE ( 'NONE', #58165, #22857, #26490, .T. ) ;
#4838 = CARTESIAN_POINT ( 'NONE',  ( 10.35398565885000011, -55.39211376237999929, -7.619387877908000206 ) ) ;
#4839 = AXIS2_PLACEMENT_3D ( 'NONE', #37144, #13239, #18859 ) ;
#4840 = CARTESIAN_POINT ( 'NONE',  ( -10.97713377773999888, -78.29452889900299795, -2.517240518847000175 ) ) ;
#4841 = CARTESIAN_POINT ( 'NONE',  ( 0.3704480504712000521, -79.85402031102998421, -1.624200486671999899 ) ) ;
#4842 = CARTESIAN_POINT ( 'NONE',  ( -0.6865653500940999132, -77.98180235332999644, -1.388644167491000170 ) ) ;
#4843 = CARTESIAN_POINT ( 'NONE',  ( -3.831287612370999796, -76.92211781146049532, -8.693171758988999187 ) ) ;
#4844 = CARTESIAN_POINT ( 'NONE',  ( 1.475387890451711925, -83.01720161097178163, 0.3238678118364496927 ) ) ;
#4845 = B_SPLINE_CURVE_WITH_KNOTS ( 'NONE', 3,
 ( #6542, #29830, #7125, #20703 ),
 .UNSPECIFIED., .F., .F.,
 ( 4, 4 ),
 ( 0.000000000000000000, 1.000000000000000000 ),
 .UNSPECIFIED. ) ;
#4846 = CARTESIAN_POINT ( 'NONE',  ( -12.49989425042000235, -59.99225390429000271, 1.666425739590000177 ) ) ;
#4847 = CARTESIAN_POINT ( 'NONE',  ( -10.02265812545943469, -80.13001055447919896, -3.947397417359383986 ) ) ;
#4848 = CARTESIAN_POINT ( 'NONE',  ( 0.000000000000000000, -80.99999999999998579, 0.000000000000000000 ) ) ;
#4849 = CARTESIAN_POINT ( 'NONE',  ( 1.012234255459822041, -77.95212815520520167, 0.7735125553324427861 ) ) ;
#4850 = ORIENTED_EDGE ( 'NONE', *, *, #54858, .F. ) ;
#4851 = B_SPLINE_CURVE_WITH_KNOTS ( 'NONE', 3,
 ( #4741, #22740, #345, #36316, #55495, #33037, #10632, #1491, #19481, #41335, #33336, #24200, #19777, #37474, #23900, #15045, #28315, #46953 ),
 .UNSPECIFIED., .F., .F.,
 ( 4, 2, 2, 2, 2, 2, 2, 2, 4 ),
 ( 0.000000000000000000, 0.1249999999999999722, 0.2500000000000000000, 0.3750000000000000000, 0.5000000000000001110, 0.6250000000000001110, 0.7500000000000000000, 0.8750000000000000000, 1.000000000000000000 ),
 .UNSPECIFIED. ) ;
#4852 = CARTESIAN_POINT ( 'NONE',  ( -5.100000000000000533, -76.79999999999999716, 0.000000000000000000 ) ) ;
#4853 = CARTESIAN_POINT ( 'NONE',  ( 0.000000000000000000, -79.79999999999999716, 0.000000000000000000 ) ) ;
#4854 = CARTESIAN_POINT ( 'NONE',  ( 7.759949366729999909, -79.07741272537499810, -8.002361301306001096 ) ) ;
#4855 = CARTESIAN_POINT ( 'NONE',  ( 7.666647577131698199, -55.04957415510976659, 7.889735440111296683 ) ) ;
#4856 = ORIENTED_EDGE ( 'NONE', *, *, #5762, .T. ) ;
#4857 = ORIENTED_EDGE ( 'NONE', *, *, #33179, .T. ) ;
#4858 = CARTESIAN_POINT ( 'NONE',  ( 0.8222529417517999706, -81.15946024296299299, -1.389645287737000245 ) ) ;
#4859 = CIRCLE ( 'NONE', #35929, 1.000000000000000000 ) ;
#4860 = ORIENTED_EDGE ( 'NONE', *, *, #29990, .T. ) ;
#4861 = ORIENTED_EDGE ( 'NONE', *, *, #41988, .T. ) ;
#4862 = CARTESIAN_POINT ( 'NONE',  ( 1.151665787602303759, -80.38188276058083659, 0.4857789717937905372 ) ) ;
#4863 = CARTESIAN_POINT ( 'NONE',  ( 7.601397897754999633, -18.75000000310999937, -10.07627163191000008 ) ) ;
#4864 = CARTESIAN_POINT ( 'NONE',  ( -3.391956917632873214, -80.24166665785288899, -0.5931127412343725203 ) ) ;
#4865 = CARTESIAN_POINT ( 'NONE',  ( 1.930638663166000191, -23.22122063288999883, -12.72375916873000001 ) ) ;
#4866 = CARTESIAN_POINT ( 'NONE',  ( 3.705840671984999890, -81.21546018839499936, -0.6149109081260000220 ) ) ;
#4867 = CARTESIAN_POINT ( 'NONE',  ( 10.07627163191000008, -60.04999999725999515, 7.601397897754999633 ) ) ;
#4868 = CARTESIAN_POINT ( 'NONE',  ( -9.202058689291000348, -78.77551683587999776, 7.798053816622000589 ) ) ;
#4869 = EDGE_CURVE ( 'NONE', #23631, #24315, #29322, .T. ) ;
#4870 = ORIENTED_EDGE ( 'NONE', *, *, #27294, .F. ) ;
#4871 = ORIENTED_EDGE ( 'NONE', *, *, #21468, .T. ) ;
#4872 = CARTESIAN_POINT ( 'NONE',  ( 14.00000000000000000, -32.88214388149999934, -1.168362945876000107E-11 ) ) ;
#4873 = LINE ( 'NONE', #18451, #19696 ) ;
#4874 = ADVANCED_FACE ( 'NONE', ( #31204 ), #31502, .F. ) ;
#4875 = CARTESIAN_POINT ( 'NONE',  ( 0.2020314717676000016, -80.35898875927600216, -1.318241039644999946 ) ) ;
#4876 = CARTESIAN_POINT ( 'NONE',  ( -2.572125540837000290, -78.31319817108199288, -9.357076443458000270 ) ) ;
#4877 = FACE_OUTER_BOUND ( 'NONE', #6668, .T. ) ;
#4878 = CARTESIAN_POINT ( 'NONE',  ( 3.514555345245232942, -85.82264533963498820, 1.481929043551247549 ) ) ;
#4879 = CARTESIAN_POINT ( 'NONE',  ( -9.299140214181999653, -77.97983485329999098, -9.021566674317000434 ) ) ;
#4880 = CARTESIAN_POINT ( 'NONE',  ( -1.348464306027999937, -81.17568918487999952, -0.5807621341562000383 ) ) ;
#4881 = CARTESIAN_POINT ( 'NONE',  ( 9.854749457207999441, -76.31148332335199314, 4.621077397111999829 ) ) ;
#4882 = LINE ( 'NONE', #50054, #49179 ) ;
#4883 = CARTESIAN_POINT ( 'NONE',  ( -3.811244649200000278, -78.68248402847228817, 1.220956923171000019 ) ) ;
#4884 = CARTESIAN_POINT ( 'NONE',  ( 6.985849709488999970, -81.01212287155250635, -8.837815942395002011 ) ) ;
#4885 = FACE_OUTER_BOUND ( 'NONE', #38599, .T. ) ;
#4886 = CARTESIAN_POINT ( 'NONE',  ( 3.237146527450594391, -2.859107922686362269, 0.3631461997434258793 ) ) ;
#4887 = CARTESIAN_POINT ( 'NONE',  ( 3.537670483016999601, -79.48657046129088144, 0.2635152204372000484 ) ) ;
#4888 = CARTESIAN_POINT ( 'NONE',  ( -0.2406813341972999787, -78.83244650139599230, -1.311734976874999958 ) ) ;
#4889 = EDGE_CURVE ( 'NONE', #12183, #35168, #21594, .T. ) ;
#4890 = FACE_OUTER_BOUND ( 'NONE', #42330, .T. ) ;
#4891 = CARTESIAN_POINT ( 'NONE',  ( -6.711381441964999972, -80.32746927473799303, 9.048015653393999713 ) ) ;
#4892 = CARTESIAN_POINT ( 'NONE',  ( -2.707053224964000027, -2.755300808012999703, 2.675433656965999774 ) ) ;
#4893 = CARTESIAN_POINT ( 'NONE',  ( 0.9151864714589287297, -77.20000000000000284, -10.94417769061167967 ) ) ;
#4894 = VERTEX_POINT ( 'NONE', #41264 ) ;
#4895 = DIRECTION ( 'NONE',  ( 0.000000000000000000, -1.000000000000000000, 0.000000000000000000 ) ) ;
#4896 = CARTESIAN_POINT ( 'NONE',  ( -0.3135214471519903734, -18.31418618814238997, -10.99610567419574636 ) ) ;
#4897 = DIRECTION ( 'NONE',  ( -1.000000000000000000, 0.000000000000000000, 0.000000000000000000 ) ) ;
#4898 = DIRECTION ( 'NONE',  ( 0.000000000000000000, -1.000000000000000000, 0.000000000000000000 ) ) ;
#4899 = CARTESIAN_POINT ( 'NONE',  ( 2.062503053667999797, -57.04263462147999775, 12.92177931909999877 ) ) ;
#4900 = CARTESIAN_POINT ( 'NONE',  ( 11.85869973992999959, -77.80110455695999860, 5.358216250391999225 ) ) ;
#4901 = CARTESIAN_POINT ( 'NONE',  ( -2.714236658744829445, -79.49531908340782138, 10.40320972029338442 ) ) ;
#4902 = CARTESIAN_POINT ( 'NONE',  ( -9.433548213809427097, -61.92797454580141192, -8.532643227302681765 ) ) ;
#4903 = CARTESIAN_POINT ( 'NONE',  ( -9.328742748748998892, -76.43633340635999218, 8.338699562703999035 ) ) ;
#4904 = ORIENTED_EDGE ( 'NONE', *, *, #32931, .T. ) ;
#4905 = EDGE_CURVE ( 'NONE', #2252, #55921, #13688, .T. ) ;
#4906 = CARTESIAN_POINT ( 'NONE',  ( 6.158633396698134810, -80.07777475630253150, 9.129463103461906925 ) ) ;
#4907 = CARTESIAN_POINT ( 'NONE',  ( 2.799999999997999645, -75.99999999999900524, 5.978114955471999489E-11 ) ) ;
#4908 = CARTESIAN_POINT ( 'NONE',  ( 1.238425546590999904, -81.51848472628699938, 0.4290956794724000156 ) ) ;
#4909 = CARTESIAN_POINT ( 'NONE',  ( 7.641012386039999882, -23.28917565320000094, -10.18589234708000113 ) ) ;
#4910 = CARTESIAN_POINT ( 'NONE',  ( -7.696817093642000174, -77.90684236001300178, 5.606191475415999825 ) ) ;
#4912 = CARTESIAN_POINT ( 'NONE',  ( -0.7824435345810000220, -1.707931841279000107, 3.939770163431000061 ) ) ;
#4911 = CARTESIAN_POINT ( 'NONE',  ( 2.168906614795000021, -85.50468686974798516, 3.514878928686000048 ) ) ;
#4913 = CARTESIAN_POINT ( 'NONE',  ( -2.062670899148999926, -60.10639625617000092, -12.83044039277999993 ) ) ;
#4914 = CARTESIAN_POINT ( 'NONE',  ( -1.294028136707999987, -80.64244764574600310, 0.2571518259264999884 ) ) ;
#4915 = ORIENTED_EDGE ( 'NONE', *, *, #16294, .F. ) ;
#4916 = CARTESIAN_POINT ( 'NONE',  ( -2.546404564821087124, -77.20613843984394009, -10.44401662958821220 ) ) ;
#4917 = CARTESIAN_POINT ( 'NONE',  ( 11.99999999999999822, -79.05670863885251265, 1.011638905658235110 ) ) ;
#4918 = ORIENTED_EDGE ( 'NONE', *, *, #37753, .F. ) ;
#4919 = ORIENTED_EDGE ( 'NONE', *, *, #2639, .F. ) ;
#4920 = CARTESIAN_POINT ( 'NONE',  ( -11.22206352833000054, -79.73100370980900209, -4.332716936452000844 ) ) ;
#4921 = CARTESIAN_POINT ( 'NONE',  ( -8.625997596412716462, -80.44864256150583515, 6.491299759919599843 ) ) ;
#4922 = ORIENTED_EDGE ( 'NONE', *, *, #8142, .F. ) ;
#4923 = B_SPLINE_CURVE_WITH_KNOTS ( 'NONE', 3,
 ( #39029, #21024, #2451, #48205, #38450, #7736, #11602, #47048, #25736, #29010, #42604, #47635, #3314, #56178, #34010, #33725, #15727, #7158 ),
 .UNSPECIFIED., .F., .F.,
 ( 4, 2, 2, 2, 2, 2, 2, 2, 4 ),
 ( 0.000000000000000000, 0.1249999999999999722, 0.2500000000000000000, 0.3750000000000000000, 0.5000000000000001110, 0.6250000000000001110, 0.7500000000000000000, 0.8750000000000000000, 1.000000000000000000 ),
 .UNSPECIFIED. ) ;
#4924 = CARTESIAN_POINT ( 'NONE',  ( 0.9683650813416999625, -78.32253854425700013, -12.01074688531000056 ) ) ;
#4925 = VERTEX_POINT ( 'NONE', #9391 ) ;
#4926 = EDGE_LOOP ( 'NONE', ( #39471, #21360, #44474, #39902, #44927, #40137 ) ) ;
#4927 = DIRECTION ( 'NONE',  ( 0.7071067811864976127, -3.445410891335986341E-11, -0.7071067811865975328 ) ) ;
#4928 = DIRECTION ( 'NONE',  ( -1.000000000000000000, 0.000000000000000000, 0.000000000000000000 ) ) ;
#4929 = DIRECTION ( 'NONE',  ( 0.000000000000000000, -1.000000000000000000, 0.000000000000000000 ) ) ;
#4930 = ORIENTED_EDGE ( 'NONE', *, *, #34287, .T. ) ;
#4931 = FACE_OUTER_BOUND ( 'NONE', #27034, .T. ) ;
#4932 = EDGE_LOOP ( 'NONE', ( #43859, #51912, #38368, #16701 ) ) ;
#4933 = CARTESIAN_POINT ( 'NONE',  ( -0.9820397338569999413, -80.70308451575900222, -0.7733679338621000099 ) ) ;
#4934 = VECTOR ( 'NONE', #48228, 1000.000000000000114 ) ;
#4935 = LINE ( 'NONE', #30897, #51015 ) ;
#4936 = B_SPLINE_CURVE_WITH_KNOTS ( 'NONE', 3,
 ( #14359, #9070, #17930, #32358, #31777, #27056, #50402, #45093, #8771, #49818, #44792, #45393, #9951, #5507, #4343, #4647, #2551, #6091, #41820, #33533, #15538, #47440, #5799, #10834, #33818, #37677, #11412, #55396, #51857, #32942, #24400, #23805, #10239, #20553, #10535, #29392, #29106, #33236, #2266, #42702, #15830, #1395, #24100, #38549, #15243, #50984, #51280, #24973, #6969, #56281, #42994, #6681, #14650, #19676, #28518, #20266, #38257, #42120, #14942 ),
 .UNSPECIFIED., .F., .F.,
 ( 4, 1, 1, 1, 1, 1, 2, 2, 1, 1, 1, 1, 1, 2, 2, 1, 2, 2, 1, 1, 1, 2, 2, 1, 1, 2, 2, 1, 2, 2, 1, 1, 2, 2, 1, 1, 1, 1, 2, 2, 4 ),
 ( 0.000000000000000000, 0.06250000000000048572, 0.09375000000000070777, 0.1093750000000008049, 0.1171875000000008465, 0.1210937500000008604, 0.1230468750000009021, 0.1250000000000009437, 0.1875000000000023037, 0.2187500000000028866, 0.2343750000000032196, 0.2421875000000033862, 0.2460937500000035250, 0.2480468750000035805, 0.2500000000000036637, 0.3125000000000029421, 0.3437500000000026090, 0.3750000000000022760, 0.4375000000000016098, 0.4687500000000012212, 0.4843750000000010547, 0.4921875000000009437, 0.5000000000000007772, 0.5625000000000007772, 0.5937500000000008882, 0.6093750000000008882, 0.6250000000000008882, 0.6875000000000006661, 0.7187500000000006661, 0.7500000000000006661, 0.7812500000000006661, 0.7968750000000006661, 0.8046875000000005551, 0.8125000000000005551, 0.8437500000000004441, 0.8593750000000003331, 0.8671875000000003331, 0.8710937500000003331, 0.8730468750000003331, 0.8750000000000003331, 1.000000000000000000 ),
 .UNSPECIFIED. ) ;
#4937 = CARTESIAN_POINT ( 'NONE',  ( -7.641012305222999679, -23.28917723430000208, -10.18589226631999978 ) ) ;
#4938 = CARTESIAN_POINT ( 'NONE',  ( 1.250000000000000000, -55.54999999966999980, 12.50000000000000000 ) ) ;
#4939 = AXIS2_PLACEMENT_3D ( 'NONE', #51721, #20984, #6827 ) ;
#4940 = LINE ( 'NONE', #41240, #26122 ) ;
#4941 = FACE_OUTER_BOUND ( 'NONE', #50756, .T. ) ;
#4942 = CARTESIAN_POINT ( 'NONE',  ( 6.543182841190322563, -78.78770266721694782, -6.538132477336259463 ) ) ;
#4943 = CARTESIAN_POINT ( 'NONE',  ( -1.179576631548999943, -77.45566001420199598, 9.337310497832001843 ) ) ;
#4944 = CARTESIAN_POINT ( 'NONE',  ( -0.5470841013496000604, -79.72570186692699679, -1.216254552179000026 ) ) ;
#4945 = CARTESIAN_POINT ( 'NONE',  ( -11.00000000000000888, -78.58958333333332291, 1.439896632895276252 ) ) ;
#4946 = CARTESIAN_POINT ( 'NONE',  ( -11.75000000000000711, -76.78958333333332575, 1.538071403319954955 ) ) ;
#4947 = CARTESIAN_POINT ( 'NONE',  ( 3.939216473890999826, -82.28567549782599144, 0.3973527477657000095 ) ) ;
#4948 = VECTOR ( 'NONE', #11174, 1000.000000000000000 ) ;
#4949 = CARTESIAN_POINT ( 'NONE',  ( -12.83677071377000090, -18.77261389757000032, 2.062839858857999698 ) ) ;
#4950 = EDGE_CURVE ( 'NONE', #31999, #30580, #20918, .T. ) ;
#4951 = FACE_OUTER_BOUND ( 'NONE', #14127, .T. ) ;
#4952 = CARTESIAN_POINT ( 'NONE',  ( 1.576170184332999824, -24.16086967216000048, 12.55466896104999996 ) ) ;
#4953 = DIRECTION ( 'NONE',  ( 1.000000000000000000, 0.000000000000000000, 0.000000000000000000 ) ) ;
#4954 = B_SPLINE_CURVE_WITH_KNOTS ( 'NONE', 3,
 ( #46086, #56096, #11227, #24501 ),
 .UNSPECIFIED., .F., .F.,
 ( 4, 4 ),
 ( 0.000000000000000000, 1.000000000000000000 ),
 .UNSPECIFIED. ) ;
#4955 = CARTESIAN_POINT ( 'NONE',  ( 1.913681202397000014, -1.135668112399999874, -3.270751771314000411 ) ) ;
#4956 = CARTESIAN_POINT ( 'NONE',  ( -7.769589423449606791, -78.16171743685177375, -7.614127194111606656 ) ) ;
#4957 = CARTESIAN_POINT ( 'NONE',  ( -1.798944584243999945, -23.21533228280000216, -12.61116915999999932 ) ) ;
#4958 = CARTESIAN_POINT ( 'NONE',  ( 12.77651065753999937, -62.10896598063000340, 0.04308629978602999955 ) ) ;
#4959 = CYLINDRICAL_SURFACE ( 'NONE', #32801, 0.5000000000000006661 ) ;
#4960 = CARTESIAN_POINT ( 'NONE',  ( -7.000000000000000000, -80.99999999999998579, 0.000000000000000000 ) ) ;
#4961 = CARTESIAN_POINT ( 'NONE',  ( 0.000000000000000000, -49.87071424677999687, 0.000000000000000000 ) ) ;
#4962 = CARTESIAN_POINT ( 'NONE',  ( -1.980532734072999901, -56.03767313155999830, 12.80090744964999949 ) ) ;
#4963 = CARTESIAN_POINT ( 'NONE',  ( -1.500000000000000000, -79.90000000000000568, 0.000000000000000000 ) ) ;
#4964 = ORIENTED_EDGE ( 'NONE', *, *, #37684, .T. ) ;
#4965 = EDGE_CURVE ( 'NONE', #12394, #36999, #36246, .T. ) ;
#4966 = CARTESIAN_POINT ( 'NONE',  ( 0.1743933192647000030, -85.86974735065199127, 3.540409746406000036 ) ) ;
#4967 = CARTESIAN_POINT ( 'NONE',  ( 7.859834628577000437, -80.32823171464259815, -7.940198685096999220 ) ) ;
#4968 = DIRECTION ( 'NONE',  ( 0.000000000000000000, -1.000000000000000000, 0.000000000000000000 ) ) ;
#4969 = CARTESIAN_POINT ( 'NONE',  ( -0.7698650111177089972, -85.02083334241058310, -3.355916637785700374 ) ) ;
#4970 = CARTESIAN_POINT ( 'NONE',  ( -10.86658628928999981, -76.85383371392200047, -2.781249891074999869 ) ) ;
#4971 = CARTESIAN_POINT ( 'NONE',  ( 12.66322081666000088, -53.61838367289999496, -0.1487102037790999920 ) ) ;
#4972 = CARTESIAN_POINT ( 'NONE',  ( -10.98362417419999915, -23.15000000000000213, 0.5999999999999999778 ) ) ;
#4973 = AXIS2_PLACEMENT_3D ( 'NONE', #48728, #39567, #22432 ) ;
#4974 = CARTESIAN_POINT ( 'NONE',  ( -12.00000000000000000, -76.79999999999999716, 1.164316068523999942E-14 ) ) ;
#4975 = CARTESIAN_POINT ( 'NONE',  ( -11.53944584717811317, -76.31731959221001205, -2.557081017239585918 ) ) ;
#4976 = CARTESIAN_POINT ( 'NONE',  ( -1.000000000000000000, -81.19999999999998863, 7.000000000000000000 ) ) ;
#4977 = CARTESIAN_POINT ( 'NONE',  ( 8.899186938125001944, -76.04999999999999716, 6.465637775217000005 ) ) ;
#4978 = ORIENTED_EDGE ( 'NONE', *, *, #43478, .F. ) ;
#4979 = CARTESIAN_POINT ( 'NONE',  ( 0.000000000000000000, -90.29999999999999716, 0.000000000000000000 ) ) ;
#4980 = CARTESIAN_POINT ( 'NONE',  ( -3.858678039026999684, -79.53793998579800473, 8.589155328362998887 ) ) ;
#4981 = CARTESIAN_POINT ( 'NONE',  ( 11.74913005080746409, -75.94346313125201675, -0.9228039449030241981 ) ) ;
#4982 = EDGE_CURVE ( 'NONE', #34855, #20949, #36827, .T. ) ;
#4983 = CARTESIAN_POINT ( 'NONE',  ( -0.1963495408493606265, -81.51458333333333428, -1.500000000000000222 ) ) ;
#4984 = ADVANCED_FACE ( 'NONE', ( #14383 ), #54243, .T. ) ;
#4985 = DIRECTION ( 'NONE',  ( 0.000000000000000000, 1.000000000000000000, 0.000000000000000000 ) ) ;
#4986 = VERTEX_POINT ( 'NONE', #9977 ) ;
#4987 = CARTESIAN_POINT ( 'NONE',  ( 3.570960563072000049, -77.14385634160659322, -10.62807481261000220 ) ) ;
#4988 = LINE ( 'NONE', #597, #34625 ) ;
#4989 = VERTEX_POINT ( 'NONE', #23538 ) ;
#4990 = ORIENTED_EDGE ( 'NONE', *, *, #14207, .F. ) ;
#4991 = AXIS2_PLACEMENT_3D ( 'NONE', #48751, #26877, #5329 ) ;
#4992 = CARTESIAN_POINT ( 'NONE',  ( -1.207620444084886113, -80.57949090611919019, 0.3245627370427532354 ) ) ;
#4993 = VECTOR ( 'NONE', #49259, 1000.000000000000000 ) ;
#4994 = SURFACE_STYLE_USAGE ( .BOTH. , #45451 ) ;
#4995 = CARTESIAN_POINT ( 'NONE',  ( 5.411006671257999834, -79.15842754766698874, 8.131518144102999557 ) ) ;
#4996 = ORIENTED_EDGE ( 'NONE', *, *, #5956, .F. ) ;
#4997 = CARTESIAN_POINT ( 'NONE',  ( 11.67908924396999915, -76.96753656385298825, 4.023272830065000250 ) ) ;
#4998 = DIRECTION ( 'NONE',  ( 0.7071067811865475727, 0.000000000000000000, -0.7071067811865475727 ) ) ;
#4999 = CARTESIAN_POINT ( 'NONE',  ( -1.312001604499999807, -77.67439276297999129, 0.5631709907292000716 ) ) ;
#5000 = ORIENTED_EDGE ( 'NONE', *, *, #39795, .T. ) ;
#5001 = EDGE_CURVE ( 'NONE', #50285, #32332, #39206, .T. ) ;
#5002 = CARTESIAN_POINT ( 'NONE',  ( 2.459440699436000077, -77.21579805011499786, -9.171074077620000153 ) ) ;
#5003 = FACE_OUTER_BOUND ( 'NONE', #38346, .T. ) ;
#5004 = CARTESIAN_POINT ( 'NONE',  ( 1.154865739624113985, -80.31888759917194420, -0.4781106390998191014 ) ) ;
#5005 = DIRECTION ( 'NONE',  ( -0.5721800012450894979, -0.8201280669353838704, 0.000000000000000000 ) ) ;
#5006 = CARTESIAN_POINT ( 'NONE',  ( 3.140974612311377090, -78.94583333333332575, -11.68767212001978528 ) ) ;
#5007 = CARTESIAN_POINT ( 'NONE',  ( 5.434802443507552816, -79.92549811133810067, 7.484660366369180196 ) ) ;
#5008 = CARTESIAN_POINT ( 'NONE',  ( -3.805607895093767290, -78.77708331314624957, -1.272258977157935345 ) ) ;
#5009 = ORIENTED_EDGE ( 'NONE', *, *, #32647, .F. ) ;
#5010 = CARTESIAN_POINT ( 'NONE',  ( -7.805809014822999714, -80.05672464109399300, 8.123945268076997905 ) ) ;
#5011 = CARTESIAN_POINT ( 'NONE',  ( 12.02702378446000075, -75.79321984486000474, -1.341316611471999876 ) ) ;
#5012 = CARTESIAN_POINT ( 'NONE',  ( 1.364204221418999774, -80.63862546449399815, 0.6617315995101000770 ) ) ;
#5013 = CONICAL_SURFACE ( 'NONE', #36113, 1.099999997157999232, 0.7853981633972997312 ) ;
#5014 = CARTESIAN_POINT ( 'NONE',  ( 3.520806411577878325, -2.101010226048630081, 0.07559986181835516572 ) ) ;
#5015 = CARTESIAN_POINT ( 'NONE',  ( 7.974014308154000474, -61.43100890296999950, -9.929675091768999096 ) ) ;
#5016 = CARTESIAN_POINT ( 'NONE',  ( -11.38660623898999980, -79.08227941497999325, -4.554589311945999697 ) ) ;
#5017 = DIRECTION ( 'NONE',  ( -1.000000000000000000, 0.000000000000000000, 0.000000000000000000 ) ) ;
#5018 = CARTESIAN_POINT ( 'NONE',  ( 12.70259395227655475, -17.26112126508259337, -1.314575638817670145 ) ) ;
#5019 = CARTESIAN_POINT ( 'NONE',  ( 10.89322882296999850, -79.82429477431499265, 2.414366480783999958 ) ) ;
#5020 = CARTESIAN_POINT ( 'NONE',  ( 4.982928723802999116, -77.54708998579799584, -8.365578579050000130 ) ) ;
#5021 = CARTESIAN_POINT ( 'NONE',  ( 5.203459128634499997, -77.38937829694961579, 10.83448682463159507 ) ) ;
#5022 = CARTESIAN_POINT ( 'NONE',  ( 1.859746058491110965, -75.81538667321693481, 12.00664290235934217 ) ) ;
#5023 = VECTOR ( 'NONE', #19324, 1000.000000000000000 ) ;
#5024 = B_SPLINE_SURFACE_WITH_KNOTS ( 'NONE', 3, 3, ( 
 ( #2630, #7621, #28380, #12058, #29748, #33894, #19251, #38628, #46426, #38912, #41977, #20339, #25623, #11774, #20627, #56358, #29466, #1548, #47522, #56645, #39196, #56930, #37246, #52500, #43351, #16203, #43646, #7051, #14518, #55258, #41684, #32510, #50555, #14807, #10107 ),
 ( #50848, #25334, #5662, #32800, #5955, #34180, #38334, #47803, #7333, #57211, #17640, #8484, #31192, #34760, #48939, #57787, #4355, #53960, #35629, #53657, #13497, #13197, #39493, #12340, #22660, #26478, #45107, #58081, #9081, #4053, #8198, #30621, #48370, #49231, #43932 ),
 ( #17940, #25910, #7908, #12906, #57497, #58378, #8783, #31489, #52786, #3481, #44502, #16778, #22056, #44218, #53358, #21486, #35931, #35039, #21769, #22357, #26774, #4660, #44803, #27068, #40064, #26200, #48654, #17059, #40370, #53074, #12625, #49535, #30904, #30328, #3767 ),
 ( #39773, #17343, #35332, #36233, #31788, #32372, #40669, #5520, #27657, #36813, #49831, #41837, #18532, #5238, #5811, #19111, #9379, #1412, #32660, #28236, #27945, #50414, #23529, #54831, #37102, #14372, #45406, #45699, #46287, #51001, #10549, #37393, #13787, #23243, #4947 ),
 ( #1123, #41541, #14958, #10252, #23818, #41251, #838, #32956, #28532, #9964, #46581, #45994, #27368, #18820, #22953, #19402, #54256, #55119, #6108, #55412, #14662, #36524, #50712, #260, #50125, #18243, #40963, #54546, #554, #14088, #32085, #9668, #34411, #16139, #2850 ),
 ( #11715, #52158, #6983, #52440, #42716, #38851, #28823, #33251, #42134, #47741, #24414, #20847, #12000, #16428, #11425, #29118, #11144, #29692, #24987, #56292, #56869, #55712, #51871, #19993, #25275, #2282, #37693, #43007, #24704, #15845, #1999, #34114, #7274, #24115, #56004 ),
 ( #15259, #48031, #33833, #29405, #43294, #29978, #1699, #19693, #20565, #37980, #51293, #10850, #46872, #15554, #20278, #6399, #42430, #33547, #51586, #2564, #47458, #56579, #47164, #38563, #38271, #6696, #4294, #44443, #3995, #22294, #21997, #48312, #21133, #31433, #17281 ),
 ( #3145, #40310, #52729, #58319, #17881, #31130, #53014, #35871, #43583, #26712, #34699, #16717, #21712, #7851, #8721, #40005, #53900, #39142, #57152, #57725, #7563, #30846, #12567, #3709, #12280, #44743, #43879, #30564, #49169, #58021, #30270, #13432, #17582, #53595, #53304 ),
 ( #39718, #35569, #35271, #25852, #48595, #13135, #25563, #3427, #21428, #39436, #8141, #57443, #17003, #34984, #26141, #44162, #12847, #48881, #8424, #26421, #45927, #28169, #37330, #23463, #23754, #37038, #40896, #36747, #41768, #45337, #46221, #5460, #9605, #36171, #14307 ),
 ( #55053, #486, #55346, #50059, #27304, #18178, #14600, #32017, #4887, #1345, #41475, #5746, #54484, #9312, #19047, #32594, #18466, #31725, #19336, #27591, #50644, #14889, #54764, #203, #36457, #54190, #10191, #45043, #45633, #49473, #9023, #27879, #22885, #5174, #27009 ) ),
 .UNSPECIFIED., .F., .F., .F.,
 ( 4, 1, 1, 1, 1, 1, 1, 4 ),
 ( 4, 1, 1, 1, 1, 1, 1, 1, 1, 1, 1, 1, 1, 1, 1, 1, 1, 1, 1, 1, 1, 1, 1, 1, 1, 1, 1, 1, 1, 1, 1, 1, 4 ),
 ( 0.4899999999999999911, 0.5000000000000000000, 0.5999999999999999778, 0.6999999999999999556, 0.8000000000000000444, 0.9000000000000000222, 1.000000000000000000, 1.010000000000000009 ),
 ( -0.02000000000000000042, 0.01250000000000000069, 0.04499999999999999833, 0.07749999999999999944, 0.1100000000000000006, 0.1424999999999999878, 0.1749999999999999889, 0.2074999999999999900, 0.2399999999999999911, 0.2725000000000000200, 0.3049999999999999933, 0.3375000000000000222, 0.3699999999999999956, 0.4025000000000000244, 0.4349999999999999978, 0.4675000000000000266, 0.5000000000000000000, 0.5324999999999999734, 0.5649999999999999467, 0.5975000000000000311, 0.6300000000000000044, 0.6624999999999999778, 0.6949999999999999512, 0.7275000000000000355, 0.7600000000000000089, 0.7924999999999999822, 0.8249999999999999556, 0.8575000000000000400, 0.8900000000000000133, 0.9224999999999999867, 0.9549999999999999600, 0.9875000000000000444, 1.020000000000000018 ),
 .UNSPECIFIED. ) ;
#5025 = VERTEX_POINT ( 'NONE', #36536 ) ;
#5026 = CARTESIAN_POINT ( 'NONE',  ( 1.392666586335999934, -82.23234125147999407, 0.4657552147452999614 ) ) ;
#5027 = CARTESIAN_POINT ( 'NONE',  ( -11.75000000000000000, -77.79999999999999716, 1.702919296826999607E-14 ) ) ;
#5028 = CARTESIAN_POINT ( 'NONE',  ( -9.309367086190000862, -77.13855160546319212, -0.1968645694141999969 ) ) ;
#5029 = CARTESIAN_POINT ( 'NONE',  ( 7.851705946354000432, -77.18019320671699290, -9.048036745432998629 ) ) ;
#5030 = CARTESIAN_POINT ( 'NONE',  ( 0.7461282319042067401, -76.94999999999998863, -9.500000001998314403 ) ) ;
#5031 = CARTESIAN_POINT ( 'NONE',  ( -11.55487901120999972, -78.03174834697500728, -3.417680896482000019 ) ) ;
#5032 = CARTESIAN_POINT ( 'NONE',  ( -8.997179024602999675, -78.97889415034599381, 3.687079342327000298 ) ) ;
#5033 = CARTESIAN_POINT ( 'NONE',  ( 7.919085842678998510, -78.97136658247099206, -5.669895566145999766 ) ) ;
#5034 = CARTESIAN_POINT ( 'NONE',  ( 4.701268039995720294, -76.04171589382065122, 10.76872600201126673 ) ) ;
#5035 = CARTESIAN_POINT ( 'NONE',  ( 8.589798209762999903, -78.65488561575499205, -6.922213596449000583 ) ) ;
#5036 = CARTESIAN_POINT ( 'NONE',  ( 3.930393413736106734, -86.02148120184399716, 0.4511457402663626159 ) ) ;
#5037 = ORIENTED_EDGE ( 'NONE', *, *, #13444, .F. ) ;
#5038 = AXIS2_PLACEMENT_3D ( 'NONE', #45735, #32697, #28268 ) ;
#5039 = EDGE_CURVE ( 'NONE', #36154, #41200, #46005, .T. ) ;
#5040 = CARTESIAN_POINT ( 'NONE',  ( 6.153863461931999623, -76.21665917695410997, -10.66140155521000032 ) ) ;
#5041 = B_SPLINE_CURVE_WITH_KNOTS ( 'NONE', 3,
 ( #14025, #14895, #9610, #32307, #46519, #32893, #10195, #27597, #45932, #10485, #5178, #54194, #5465, #45639, #23184, #13732, #23468, #1064 ),
 .UNSPECIFIED., .F., .F.,
 ( 4, 2, 2, 2, 2, 2, 2, 2, 4 ),
 ( 0.000000000000000000, 0.1250000000000000833, 0.2500000000000001110, 0.3750000000000000000, 0.4999999999999999445, 0.6249999999999998890, 0.7499999999999997780, 0.8749999999999998890, 1.000000000000000000 ),
 .UNSPECIFIED. ) ;
#5042 = CARTESIAN_POINT ( 'NONE',  ( -2.309341173333539388, -78.43735716284257364, -3.830055274395752551 ) ) ;
#5043 = ADVANCED_FACE ( 'NONE', ( #40975 ), #4959, .F. ) ;
#5045 = CARTESIAN_POINT ( 'NONE',  ( -5.692170641448433877, -76.28460817517897397, -10.28117217690509655 ) ) ;
#5044 = CARTESIAN_POINT ( 'NONE',  ( -2.813789756862300262, -77.39583333333334281, 10.47020627418438465 ) ) ;
#5046 = CARTESIAN_POINT ( 'NONE',  ( 10.71556987377000070, -79.75781129242999157, 2.374990294079000197 ) ) ;
#5047 = CARTESIAN_POINT ( 'NONE',  ( 0.000000000000000000, -9.295797029142999435, 0.000000000000000000 ) ) ;
#5048 = CARTESIAN_POINT ( 'NONE',  ( -12.47910600135000081, -76.37844759300099895, -0.7911314731844000248 ) ) ;
#5049 = DIRECTION ( 'NONE',  ( 0.000000000000000000, -1.000000000000000000, 0.000000000000000000 ) ) ;
#5050 = CARTESIAN_POINT ( 'NONE',  ( 7.606021555073000151, -18.57841460072999951, -10.52692944505000128 ) ) ;
#5051 = ORIENTED_EDGE ( 'NONE', *, *, #4039, .T. ) ;
#5052 = CARTESIAN_POINT ( 'NONE',  ( 7.942219812765999087, -79.58930274324299603, 7.984679643171000762 ) ) ;
#5053 = CARTESIAN_POINT ( 'NONE',  ( 12.72924182832020534, -18.22450359986278201, 1.930521792012820370 ) ) ;
#5054 = CARTESIAN_POINT ( 'NONE',  ( 12.50659830419106910, -53.82653389278990375, 0.3508388549139770940 ) ) ;
#5055 = CARTESIAN_POINT ( 'NONE',  ( -3.547719550341454475, -78.43735717367049176, -0.06688104799386529464 ) ) ;
#5056 = B_SPLINE_CURVE_WITH_KNOTS ( 'NONE', 3,
 ( #28202, #35965, #22688, #294, #54287, #31823 ),
 .UNSPECIFIED., .F., .F.,
 ( 4, 2, 4 ),
 ( 0.000000000000000000, 0.4999999999999998890, 1.000000000000000000 ),
 .UNSPECIFIED. ) ;
#5057 = CARTESIAN_POINT ( 'NONE',  ( 12.56594317991999965, -60.04999999381999487, 1.750000000001000089 ) ) ;
#5058 = EDGE_CURVE ( 'NONE', #47851, #17898, #47722, .T. ) ;
#5059 = CARTESIAN_POINT ( 'NONE',  ( -9.501885680564001291, -79.34955593965399601, -5.638445012646999821 ) ) ;
#5060 = CARTESIAN_POINT ( 'NONE',  ( -8.314650709467036549, -77.00000000000000000, -4.397163425340465892 ) ) ;
#5061 = CARTESIAN_POINT ( 'NONE',  ( 14.00000000000000000, -9.295797029142999435, 0.000000000000000000 ) ) ;
#5062 = B_SPLINE_CURVE_WITH_KNOTS ( 'NONE', 3,
 ( #9572, #49134, #9278, #26677, #40572, #27556, #5143, #54451, #36424, #4855, #44709, #18434, #35833, #23142, #26971, #39973, #31097, #4262 ),
 .UNSPECIFIED., .F., .F.,
 ( 4, 2, 2, 2, 2, 2, 2, 2, 4 ),
 ( 0.000000000000000000, 0.06250000000000328904, 0.1250000000000065781, 0.2500000000000031641, 0.5000000000000028866, 0.7500000000000025535, 0.8125000000000018874, 0.8750000000000012212, 1.000000000000000000 ),
 .UNSPECIFIED. ) ;
#5063 = CARTESIAN_POINT ( 'NONE',  ( 0.7554284705563509839, -81.16666666666668561, -1.310679582531385945 ) ) ;
#5064 = DIRECTION ( 'NONE',  ( 0.000000000000000000, 0.000000000000000000, -1.000000000000000000 ) ) ;
#5065 = CARTESIAN_POINT ( 'NONE',  ( -8.631516086050529779, -78.39711804219207636, 6.779730741015662865 ) ) ;
#5066 = B_SPLINE_CURVE_WITH_KNOTS ( 'NONE', 3,
 ( #5900, #10345, #11226, #23910, #1500, #55506, #33046, #24209, #20082, #51093, #28624, #46669, #42227, #29205, #1792, #19788 ),
 .UNSPECIFIED., .F., .F.,
 ( 4, 2, 2, 2, 2, 2, 2, 4 ),
 ( 0.000000000000000000, 0.2500000000000000555, 0.3750000000000001110, 0.5000000000000001110, 0.6250000000000001110, 0.6875000000000001110, 0.7500000000000002220, 1.000000000000000000 ),
 .UNSPECIFIED. ) ;
#5067 = CARTESIAN_POINT ( 'NONE',  ( -12.66319951811000166, -25.18148258132000095, 0.1455783832297000147 ) ) ;
#5068 = VERTEX_POINT ( 'NONE', #28244 ) ;
#5069 = ORIENTED_EDGE ( 'NONE', *, *, #23221, .T. ) ;
#5070 = CARTESIAN_POINT ( 'NONE',  ( 7.655285058836605039, -78.78807752846175561, -7.547175273370277715 ) ) ;
#5071 = DIRECTION ( 'NONE',  ( 0.7071067811865475727, 0.000000000000000000, -0.7071067811865475727 ) ) ;
#5072 = ORIENTED_EDGE ( 'NONE', *, *, #19257, .F. ) ;
#5073 = CARTESIAN_POINT ( 'NONE',  ( -9.250000000000000000, -78.09999999999999432, 0.000000000000000000 ) ) ;
#5074 = CARTESIAN_POINT ( 'NONE',  ( 7.606021324597999289, -23.42158946275000275, 10.52692925327000140 ) ) ;
#5075 = CIRCLE ( 'NONE', #55992, 11.70000000000000107 ) ;
#5076 = CARTESIAN_POINT ( 'NONE',  ( 6.099615176083999835, -78.31341404718699550, -9.019941877331000057 ) ) ;
#5077 = CARTESIAN_POINT ( 'NONE',  ( 10.35398566683000077, -60.20788276206999967, 7.619388279096000360 ) ) ;
#5078 = CARTESIAN_POINT ( 'NONE',  ( -13.49939038839240979, -32.88214388149999934, -0.1282931867975413143 ) ) ;
#5079 = CARTESIAN_POINT ( 'NONE',  ( -10.86803167256632463, -77.58446068609639212, -5.040424477369018774 ) ) ;
#5080 = CARTESIAN_POINT ( 'NONE',  ( -10.34326456654000026, -78.73449123692898866, 4.339929572939999147 ) ) ;
#5081 = CARTESIAN_POINT ( 'NONE',  ( 8.562542432403372317, -81.00000000000002842, 6.777005483380555084 ) ) ;
#5082 = ORIENTED_EDGE ( 'NONE', *, *, #21481, .F. ) ;
#5083 = CARTESIAN_POINT ( 'NONE',  ( 7.850076762419817555, -61.11471440997013360, -9.837736659315822862 ) ) ;
#5084 = ORIENTED_EDGE ( 'NONE', *, *, #36701, .F. ) ;
#5085 = CARTESIAN_POINT ( 'NONE',  ( -0.4327165701982794155, -77.47889716067786026, 9.240429326102006513 ) ) ;
#5086 = CARTESIAN_POINT ( 'NONE',  ( 10.90987126150000108, -77.19238596616818882, 1.690571823134000118 ) ) ;
#5087 = CARTESIAN_POINT ( 'NONE',  ( 0.000000000000000000, -0.09999999858571000100, 0.000000000000000000 ) ) ;
#5088 = ADVANCED_FACE ( 'NONE', ( #14673 ), #28088, .F. ) ;
#5089 = CARTESIAN_POINT ( 'NONE',  ( -9.446433787353997857, -78.40883546070699595, -2.221620594898999990 ) ) ;
#5090 = CARTESIAN_POINT ( 'NONE',  ( 6.292427835922000057, -76.25321726005000755, 11.33658693087999936 ) ) ;
#5091 = DIRECTION ( 'NONE',  ( 1.000000000000000000, 0.000000000000000000, 0.000000000000000000 ) ) ;
#5092 = CARTESIAN_POINT ( 'NONE',  ( -1.481905647302000029, -78.24508877014999086, -0.6727694308694001091 ) ) ;
#5093 = CARTESIAN_POINT ( 'NONE',  ( 14.00000000000000000, -32.88214388149999934, 0.000000000000000000 ) ) ;
#5094 = CARTESIAN_POINT ( 'NONE',  ( -8.032634178075001685, -78.48857205644399926, -7.427287829177999789 ) ) ;
#5095 = CARTESIAN_POINT ( 'NONE',  ( -7.758655887903000092, -24.15078616243999932, -9.996711280983999970 ) ) ;
#5096 = AXIS2_PLACEMENT_3D ( 'NONE', #4938, #4651, #50405 ) ;
#5097 = CARTESIAN_POINT ( 'NONE',  ( 12.50000000000000000, -91.29999999999999716, 2.555046452191000376E-12 ) ) ;
#5098 = CARTESIAN_POINT ( 'NONE',  ( -0.6946676981835000486, -83.34017939494499672, -3.521531175359999821 ) ) ;
#5099 = ORIENTED_EDGE ( 'NONE', *, *, #5439, .T. ) ;
#5100 = CARTESIAN_POINT ( 'NONE',  ( -9.739450257827000357, -78.99356062328099881, -7.539835367685000733 ) ) ;
#5101 = CARTESIAN_POINT ( 'NONE',  ( 0.1598674175986999901, -76.08275625893899985, 11.49285586031999884 ) ) ;
#5102 = CARTESIAN_POINT ( 'NONE',  ( 2.414752746249941406, -77.95724855646152207, 10.49752381153813907 ) ) ;
#5103 = CARTESIAN_POINT ( 'NONE',  ( 10.69384760718000038, -78.34668429937299550, -5.399785902169999652 ) ) ;
#5104 = CARTESIAN_POINT ( 'NONE',  ( 2.598917237794081014, -3.302083333333333925, 1.997276839918480373 ) ) ;
#5106 = CYLINDRICAL_SURFACE ( 'NONE', #25065, 0.5000000000000004441 ) ;
#5105 = CARTESIAN_POINT ( 'NONE',  ( 10.36935812844000004, -78.17876026662598576, -2.835297515976000327 ) ) ;
#5107 = CARTESIAN_POINT ( 'NONE',  ( 0.000000000000000000, -91.29999999999999716, 0.000000000000000000 ) ) ;
#5108 = CARTESIAN_POINT ( 'NONE',  ( 3.268028314528707678, -80.95051983432966836, 10.24357525341220132 ) ) ;
#5109 = CARTESIAN_POINT ( 'NONE',  ( -9.379486438909999890, -77.58593853670399199, -0.7977647835019999745 ) ) ;
#5110 = CARTESIAN_POINT ( 'NONE',  ( -3.241578942234993654, -85.83735717367099483, 1.443243930775013784 ) ) ;
#5111 = CARTESIAN_POINT ( 'NONE',  ( 2.958310398169000432, -77.53751179411899841, -10.74723220921999989 ) ) ;
#5112 = CARTESIAN_POINT ( 'NONE',  ( -12.17466003208999936, -76.63951734500820123, 1.612538369963999907 ) ) ;
#5113 = CARTESIAN_POINT ( 'NONE',  ( 1.937333205045999929, -80.25222754060989416, 10.97105737937000036 ) ) ;
#5114 = B_SPLINE_CURVE_WITH_KNOTS ( 'NONE', 3,
 ( #13152, #12862, #9624, #31146, #9333, #45061 ),
 .UNSPECIFIED., .F., .F.,
 ( 4, 1, 1, 4 ),
 ( 0.000000000000000000, 0.3333333311589000147, 0.6666666623179000606, 0.9999999934768000198 ),
 .UNSPECIFIED. ) ;
#5115 = VERTEX_POINT ( 'NONE', #22671 ) ;
#5116 = CIRCLE ( 'NONE', #39063, 9.000000000000000000 ) ;
#5117 = DIRECTION ( 'NONE',  ( 0.000000000000000000, -1.000000000000000000, 0.000000000000000000 ) ) ;
#5118 = CARTESIAN_POINT ( 'NONE',  ( -2.205007487985999770, -77.04364903538302656, 9.235565851336001941 ) ) ;
#5119 = CARTESIAN_POINT ( 'NONE',  ( -2.536595847992999975, -3.375401880086999817, -3.049063006156000011 ) ) ;
#5120 = EDGE_CURVE ( 'NONE', #44860, #1033, #13413, .T. ) ;
#5121 = CARTESIAN_POINT ( 'NONE',  ( 7.155101792066000499, -78.44746208375599394, -8.354909834651998324 ) ) ;
#5122 = CARTESIAN_POINT ( 'NONE',  ( 0.000000000000000000, -76.00000000000000000, 0.000000000000000000 ) ) ;
#5123 = CYLINDRICAL_SURFACE ( 'NONE', #36612, 9.250000000000000000 ) ;
#5124 = CARTESIAN_POINT ( 'NONE',  ( 4.008581223418561379, -82.43854164688262642, -0.1919510447721787250 ) ) ;
#5125 = CARTESIAN_POINT ( 'NONE',  ( 3.042547531669000271, -78.64783470746900207, -10.31045122763999977 ) ) ;
#5126 = DIRECTION ( 'NONE',  ( 0.000000000000000000, 0.000000000000000000, 1.000000000000000000 ) ) ;
#5127 = FACE_OUTER_BOUND ( 'NONE', #23722, .T. ) ;
#5128 = CARTESIAN_POINT ( 'NONE',  ( -1.500000000000000222, -79.51041666666668561, -0.1963495408493622085 ) ) ;
#5129 = CARTESIAN_POINT ( 'NONE',  ( 9.029856014839001688, -53.46737842902999915, -9.038878718651000455 ) ) ;
#5130 = EDGE_CURVE ( 'NONE', #33417, #3715, #16755, .T. ) ;
#5131 = CARTESIAN_POINT ( 'NONE',  ( -10.71960490440000058, -78.15429499344598696, 3.466843673432000283 ) ) ;
#5132 = CARTESIAN_POINT ( 'NONE',  ( 0.5818457612699999837, -80.92378407665999873, -1.560998038830999857 ) ) ;
#5133 = CARTESIAN_POINT ( 'NONE',  ( -1.275974813924000140, -78.99934084733999384, 0.3384762398118000282 ) ) ;
#5134 = CARTESIAN_POINT ( 'NONE',  ( -0.8898229089110474277, -61.82324531153690828, 12.70296869049124311 ) ) ;
#5135 = CARTESIAN_POINT ( 'NONE',  ( 0.1237032920003742348, -83.11841830185345259, 1.505458275059794460 ) ) ;
#5136 = CARTESIAN_POINT ( 'NONE',  ( -12.43641409355999983, -61.71801033862000452, -0.03481937293210000256 ) ) ;
#5137 = CARTESIAN_POINT ( 'NONE',  ( -4.100000000000000533, -77.49999999999998579, 0.000000000000000000 ) ) ;
#5138 = DIRECTION ( 'NONE',  ( 0.7071067811865475727, 0.000000000000000000, 0.7071067811865475727 ) ) ;
#5139 = VERTEX_POINT ( 'NONE', #49750 ) ;
#5140 = CARTESIAN_POINT ( 'NONE',  ( 1.184538586134731508, -81.82436935641939613, -0.3988734786993729520 ) ) ;
#5141 = CARTESIAN_POINT ( 'NONE',  ( -0.8338927961505636643, -61.60053577702783656, 12.50366901606069447 ) ) ;
#5142 = CARTESIAN_POINT ( 'NONE',  ( 10.63213186872000016, -78.54666782993099616, -3.713725309742000213 ) ) ;
#5143 = CARTESIAN_POINT ( 'NONE',  ( 8.111636311586917003, -55.28385402669261595, 7.429974109814975414 ) ) ;
#5144 = VERTEX_POINT ( 'NONE', #30545 ) ;
#5145 = ORIENTED_EDGE ( 'NONE', *, *, #32666, .T. ) ;
#5146 = DIRECTION ( 'NONE',  ( 0.000000000000000000, 0.000000000000000000, -1.000000000000000000 ) ) ;
#5147 = ORIENTED_EDGE ( 'NONE', *, *, #55170, .T. ) ;
#5148 = ORIENTED_EDGE ( 'NONE', *, *, #14702, .T. ) ;
#5149 = DIRECTION ( 'NONE',  ( -1.000000000000000000, 0.000000000000000000, 0.000000000000000000 ) ) ;
#5150 = CARTESIAN_POINT ( 'NONE',  ( -4.017143116098000455, -80.25404428795494027, 10.51352533724000082 ) ) ;
#5151 = CARTESIAN_POINT ( 'NONE',  ( 1.750000000000000000, -57.04935285922000077, 12.65372179284000076 ) ) ;
#5152 = CARTESIAN_POINT ( 'NONE',  ( -10.48543666025109111, -76.34166666662416389, -6.043427764450793660 ) ) ;
#5153 = CARTESIAN_POINT ( 'NONE',  ( 0.5992844399098999908, -82.41796443320698984, -3.708392236748999871 ) ) ;
#5154 = LINE ( 'NONE', #23155, #35243 ) ;
#5155 = CARTESIAN_POINT ( 'NONE',  ( 9.995119889681001624, -79.03418329856999947, -6.751676457494999894 ) ) ;
#5156 = ORIENTED_EDGE ( 'NONE', *, *, #30225, .F. ) ;
#5157 = EDGE_LOOP ( 'NONE', ( #11690, #54004, #49135, #2070 ) ) ;
#5158 = FACE_OUTER_BOUND ( 'NONE', #50892, .T. ) ;
#5159 = DIRECTION ( 'NONE',  ( 0.000000000000000000, -1.000000000000000000, 0.000000000000000000 ) ) ;
#5160 = EDGE_CURVE ( 'NONE', #29817, #45005, #45317, .T. ) ;
#5161 = CARTESIAN_POINT ( 'NONE',  ( 0.8898229090076987813, -61.82324531144395507, -12.70296869049792932 ) ) ;
#5162 = CARTESIAN_POINT ( 'NONE',  ( 9.583411031200000707, -77.97211222153399035, 1.526087275887999972 ) ) ;
#5163 = CARTESIAN_POINT ( 'NONE',  ( 9.750000000000000000, -76.19999999999998863, 0.000000000000000000 ) ) ;
#5164 = CARTESIAN_POINT ( 'NONE',  ( 3.047808061981939876, -85.85448694835680783, 2.394986058418032471 ) ) ;
#5165 = CARTESIAN_POINT ( 'NONE',  ( -10.55245342185999924, -77.36928380272000538, 7.517205849611000801 ) ) ;
#5166 = EDGE_CURVE ( 'NONE', #39794, #27203, #45020, .T. ) ;
#5167 = CARTESIAN_POINT ( 'NONE',  ( 0.5128916439544000117, -80.79673389420999285, -1.376005298375999830 ) ) ;
#5168 = CARTESIAN_POINT ( 'NONE',  ( 7.630512808711405803, -77.35002193750341348, 5.569571266600500614 ) ) ;
#5169 = FACE_OUTER_BOUND ( 'NONE', #24018, .T. ) ;
#5170 = CARTESIAN_POINT ( 'NONE',  ( -2.067188713461000305, -79.93618638030199008, 3.624472860286000131 ) ) ;
#5171 = CARTESIAN_POINT ( 'NONE',  ( -8.418594644163000851, -80.82394357426177578, -7.485750452785000064 ) ) ;
#5172 = CARTESIAN_POINT ( 'NONE',  ( 7.890654042133999901, -77.86386001420198966, 4.760698198672999482 ) ) ;
#5173 = FACE_OUTER_BOUND ( 'NONE', #51889, .T. ) ;
#5174 = CARTESIAN_POINT ( 'NONE',  ( 3.440741359840000069, -82.45273712795798815, -0.2267907360308999976 ) ) ;
#5175 = CARTESIAN_POINT ( 'NONE',  ( 0.9384621721472999889, -78.53477076110999633, 0.9475573338641000154 ) ) ;
#5176 = CARTESIAN_POINT ( 'NONE',  ( 7.189039685305539606, -77.47583944371665154, -9.673072753243907584 ) ) ;
#5177 = CARTESIAN_POINT ( 'NONE',  ( -8.485281374238999419, 0.000000000000000000, 8.485281374238999419 ) ) ;
#5178 = CARTESIAN_POINT ( 'NONE',  ( -0.3271848554490991434, -79.10416666666665719, -1.217465845835395299 ) ) ;
#5179 = ORIENTED_EDGE ( 'NONE', *, *, #6097, .F. ) ;
#5180 = DIRECTION ( 'NONE',  ( 0.000000000000000000, -1.000000000000000000, 0.000000000000000000 ) ) ;
#5181 = CARTESIAN_POINT ( 'NONE',  ( -0.1610657711543910797, -18.25053022707189854, -10.99997582743960223 ) ) ;
#5182 = CARTESIAN_POINT ( 'NONE',  ( 11.00000000000000000, -78.94999999999998863, -1.064824513673000067E-14 ) ) ;
#5183 = CIRCLE ( 'NONE', #19305, 5.000000000000000000 ) ;
#5184 = EDGE_CURVE ( 'NONE', #13151, #31999, #27297, .T. ) ;
#5185 = VECTOR ( 'NONE', #29673, 1000.000000000000000 ) ;
#5186 = CARTESIAN_POINT ( 'NONE',  ( 9.434081066526999848, -79.55882968926798071, -2.467387813727000001 ) ) ;
#5187 = CARTESIAN_POINT ( 'NONE',  ( -12.97295173694999981, -77.48891468547999750, -1.020668466325000079 ) ) ;
#5188 = CARTESIAN_POINT ( 'NONE',  ( -6.313152452412044369, -79.52497619356374514, 8.700938145767349141 ) ) ;
#5189 = CARTESIAN_POINT ( 'NONE',  ( -8.266617305365361545, -61.77234527411153664, -9.697375114849947408 ) ) ;
#5190 = CARTESIAN_POINT ( 'NONE',  ( 10.12290050256999940, -18.75000002239000096, 7.648026768411000376 ) ) ;
#5191 = ORIENTED_EDGE ( 'NONE', *, *, #55612, .F. ) ;
#5192 = VECTOR ( 'NONE', #25207, 1000.000000000000000 ) ;
#5193 = CARTESIAN_POINT ( 'NONE',  ( -9.621717086601071500, -24.62064477554104869, -8.060172378189184528 ) ) ;
#5194 = CARTESIAN_POINT ( 'NONE',  ( 10.85646270852000050, -77.97987769867899033, -1.809030205320999896 ) ) ;
#5195 = EDGE_CURVE ( 'NONE', #47936, #891, #39400, .T. ) ;
#5196 = CARTESIAN_POINT ( 'NONE',  ( 0.1847432000700000021, -81.43278215430200362, -1.396303359803000133 ) ) ;
#5197 = CARTESIAN_POINT ( 'NONE',  ( 7.718346056127999510, -20.25111654322000021, -10.07719973196000041 ) ) ;
#5198 = CARTESIAN_POINT ( 'NONE',  ( -2.142155038640999987, -77.84999470175499425, 9.278014228403000274 ) ) ;
#5199 = EDGE_CURVE ( 'NONE', #33222, #10301, #17262, .T. ) ;
#5201 = CARTESIAN_POINT ( 'NONE',  ( -3.249661007175000282, -0.6980864414130000251, 2.357191814219000037 ) ) ;
#5200 = CARTESIAN_POINT ( 'NONE',  ( -1.832953822565000168, -85.87701485180299699, 3.751014218058000171 ) ) ;
#5202 = CARTESIAN_POINT ( 'NONE',  ( -2.062502994258999856, -58.55648180022999583, -12.92181194095999963 ) ) ;
#5203 = CARTESIAN_POINT ( 'NONE',  ( -1.460959015002474937, -81.47916666666665719, 0.3926218265389144757 ) ) ;
#5204 = VERTEX_POINT ( 'NONE', #26402 ) ;
#5205 = CARTESIAN_POINT ( 'NONE',  ( -3.395352835590720098, -77.19953567266439620, -10.19974753772885201 ) ) ;
#5206 = CARTESIAN_POINT ( 'NONE',  ( -1.500000000000000222, -78.91041666666666288, -0.1963495408493622363 ) ) ;
#5207 = ORIENTED_EDGE ( 'NONE', *, *, #1611, .F. ) ;
#5208 = ORIENTED_EDGE ( 'NONE', *, *, #24516, .T. ) ;
#5209 = DIRECTION ( 'NONE',  ( 0.000000000000000000, -1.000000000000000000, 0.000000000000000000 ) ) ;
#5210 = CARTESIAN_POINT ( 'NONE',  ( 0.5999999999999999778, -5.200000000000000178, -4.000000000000000000 ) ) ;
#5211 = ORIENTED_EDGE ( 'NONE', *, *, #27920, .T. ) ;
#5212 = CARTESIAN_POINT ( 'NONE',  ( 1.730980777285999972, -77.32779697871899316, -11.76800180821999930 ) ) ;
#5213 = ORIENTED_EDGE ( 'NONE', *, *, #56640, .F. ) ;
#5214 = EDGE_LOOP ( 'NONE', ( #2152, #51199, #1850, #46746, #43398 ) ) ;
#5215 = CARTESIAN_POINT ( 'NONE',  ( -2.748921057787184541, -2.646192902617848564, -1.734975443660489169 ) ) ;
#5216 = EDGE_CURVE ( 'NONE', #52133, #469, #10006, .T. ) ;
#5217 = B_SPLINE_CURVE_WITH_KNOTS ( 'NONE', 3,
 ( #46347, #55475, #14722, #4718, #41311, #40730, #9437, #13856, #321, #18298, #5006, #36293, #54315, #31851, #50474, #27716, #5294, #49893 ),
 .UNSPECIFIED., .F., .F.,
 ( 4, 2, 2, 2, 2, 2, 2, 2, 4 ),
 ( 0.000000000000000000, 0.1250000000000000000, 0.2500000000000000000, 0.3750000000000000000, 0.5000000000000000000, 0.6250000000000000000, 0.7500000000000000000, 0.8750000000000000000, 1.000000000000000000 ),
 .UNSPECIFIED. ) ;
#5218 = CARTESIAN_POINT ( 'NONE',  ( -9.596002108778193929, -78.74791666666664014, 7.374560639698935383 ) ) ;
#5219 = CARTESIAN_POINT ( 'NONE',  ( 9.319018100775748437, -79.16524970259979455, 1.846458293751403135 ) ) ;
#5220 = ORIENTED_EDGE ( 'NONE', *, *, #39281, .F. ) ;
#5221 = CARTESIAN_POINT ( 'NONE',  ( 0.8840402821807384903, -82.78818478153729643, -0.8831652403929096673 ) ) ;
#5222 = ORIENTED_EDGE ( 'NONE', *, *, #6014, .T. ) ;
#5223 = CARTESIAN_POINT ( 'NONE',  ( -7.396672774822746987, -79.15237237872500486, -5.684931589052010459 ) ) ;
#5224 = CARTESIAN_POINT ( 'NONE',  ( -6.473154694944447840, -78.28301520904093991, 7.229944404031765082 ) ) ;
#5225 = CARTESIAN_POINT ( 'NONE',  ( -0.03769889196560047978, -78.72610001270986402, -3.999822345247734834 ) ) ;
#5226 = ADVANCED_FACE ( 'NONE', ( #35550 ), #6312, .F. ) ;
#5227 = DIRECTION ( 'NONE',  ( 1.000000000000000000, 0.000000000000000000, 0.000000000000000000 ) ) ;
#5228 = CARTESIAN_POINT ( 'NONE',  ( -8.075725583014000009, -76.32689981197398765, -7.736700848913999451 ) ) ;
#5229 = CARTESIAN_POINT ( 'NONE',  ( -9.298485322487321625, -24.88812323703229268, 8.385852789306289523 ) ) ;
#5230 = EDGE_CURVE ( 'NONE', #32124, #47573, #32202, .T. ) ;
#5231 = CARTESIAN_POINT ( 'NONE',  ( 0.000000000000000000, -77.50000000000000000, 0.000000000000000000 ) ) ;
#5232 = CARTESIAN_POINT ( 'NONE',  ( -9.871315929017001167, -76.28387572403700290, 5.351714737855999715 ) ) ;
#5233 = CARTESIAN_POINT ( 'NONE',  ( 6.769093727302936792, -78.79047469916130808, -6.304424132926785163 ) ) ;
#5234 = CARTESIAN_POINT ( 'NONE',  ( 8.924962326551000302, -77.79496001420199036, -2.986943611218999983 ) ) ;
#5235 = DIRECTION ( 'NONE',  ( 0.000000000000000000, 1.000000000000000000, 0.000000000000000000 ) ) ;
#5236 = CARTESIAN_POINT ( 'NONE',  ( -4.186946963469314831, -80.19418132811986766, -10.17752948135066049 ) ) ;
#5237 = CARTESIAN_POINT ( 'NONE',  ( -12.01673236380376686, -77.95062490049402015, 0.3580987964395272449 ) ) ;
#5238 = CARTESIAN_POINT ( 'NONE',  ( -3.523827339823000226, -79.88067549782599031, 2.154331540686999613 ) ) ;
#5239 = CARTESIAN_POINT ( 'NONE',  ( -9.632028597164000061, -77.19831332859899931, -0.6303035207593999933 ) ) ;
#5240 = CARTESIAN_POINT ( 'NONE',  ( 0.000000000000000000, -75.15999999999999659, 0.000000000000000000 ) ) ;
#5241 = CARTESIAN_POINT ( 'NONE',  ( 1.750000000001000089, -18.74999999009000007, -12.56594317857000043 ) ) ;
#5242 = CARTESIAN_POINT ( 'NONE',  ( -2.065394024360999836, -23.42161432646000208, 12.82193048528000112 ) ) ;
#5243 = CARTESIAN_POINT ( 'NONE',  ( -9.500000000000000000, -91.89999999999999147, 0.000000000000000000 ) ) ;
#5244 = CARTESIAN_POINT ( 'NONE',  ( 8.760175664411535834, -79.99999999999998579, 3.616861466383621160 ) ) ;
#5245 = CARTESIAN_POINT ( 'NONE',  ( -0.1136598462024999839, -0.8462797842361000633, 3.300476129822000004 ) ) ;
#5246 = CARTESIAN_POINT ( 'NONE',  ( 1.250000000000000000, -80.74999999999998579, 0.000000000000000000 ) ) ;
#5247 = DIRECTION ( 'NONE',  ( 0.000000000000000000, 1.000000000000000000, 0.000000000000000000 ) ) ;
#5248 = CARTESIAN_POINT ( 'NONE',  ( 10.59551070212999946, -58.55648180022999583, 7.678690995210999404 ) ) ;
#5249 = CARTESIAN_POINT ( 'NONE',  ( 0.5327588397318764324, -79.50310756622292274, -1.415177852321873209 ) ) ;
#5250 = CARTESIAN_POINT ( 'NONE',  ( -7.624341764906000130, -55.53514850498000044, -10.42531124851000079 ) ) ;
#5251 = CARTESIAN_POINT ( 'NONE',  ( 2.866048672220999904, -2.746200577026000289, -1.983677989232000227 ) ) ;
#5252 = CARTESIAN_POINT ( 'NONE',  ( 6.768882593647018275, -77.27178109534467865, 8.462659279992045924 ) ) ;
#5253 = DIRECTION ( 'NONE',  ( 1.674928520677000026E-10, 1.000000000000000000, -2.004067147595000089E-09 ) ) ;
#5255 = CARTESIAN_POINT ( 'NONE',  ( -1.317826160292999926, -77.82215499870639519, 0.5319603796220000458 ) ) ;
#5254 = DIRECTION ( 'NONE',  ( 0.000000000000000000, 1.000000000000000000, 0.000000000000000000 ) ) ;
#5256 = CARTESIAN_POINT ( 'NONE',  ( -1.623947472758999977, -83.24568302734098779, 0.5113958356693000251 ) ) ;
#5257 = ORIENTED_EDGE ( 'NONE', *, *, #17405, .F. ) ;
#5258 = CARTESIAN_POINT ( 'NONE',  ( 3.170434149039000005, -82.75482450217398878, 1.682927666644999931 ) ) ;
#5259 = CARTESIAN_POINT ( 'NONE',  ( 5.125497890974998860, -79.28376034395300564, -10.76871041769000037 ) ) ;
#5260 = VECTOR ( 'NONE', #1062, 1000.000000000000000 ) ;
#5261 = CARTESIAN_POINT ( 'NONE',  ( -10.83119716622999995, -80.18612266303370006, 3.182336190940000087 ) ) ;
#5262 = FACE_BOUND ( 'NONE', #43467, .T. ) ;
#5263 = CARTESIAN_POINT ( 'NONE',  ( 0.9218200799623742503, -81.67708333333332860, -1.199500263597268912 ) ) ;
#5264 = CARTESIAN_POINT ( 'NONE',  ( 12.43647099676999979, -53.88193128055999637, 0.03491583288326000067 ) ) ;
#5265 = CARTESIAN_POINT ( 'NONE',  ( -1.335477334469999862E-14, -72.70000000000000284, 0.000000000000000000 ) ) ;
#5266 = CARTESIAN_POINT ( 'NONE',  ( 11.48986902082000050, -77.53985072955998703, 5.271442771914999881 ) ) ;
#5267 = CARTESIAN_POINT ( 'NONE',  ( -8.556275607134224970, -76.36061857273500664, -8.153994206733470307 ) ) ;
#5268 = CARTESIAN_POINT ( 'NONE',  ( -3.778637972659712574, -77.00000000000000000, 8.499186437672962668 ) ) ;
#5269 = EDGE_LOOP ( 'NONE', ( #13481, #29954, #12026, #28950 ) ) ;
#5270 = AXIS2_PLACEMENT_3D ( 'NONE', #30124, #2995, #49837 ) ;
#5271 = CARTESIAN_POINT ( 'NONE',  ( 0.5135400118779288592, -53.62131466105113020, -12.70453250094157660 ) ) ;
#5272 = CARTESIAN_POINT ( 'NONE',  ( 2.166634614239063377E-07, -77.01246206852036380, -9.437473063691797392 ) ) ;
#5273 = CARTESIAN_POINT ( 'NONE',  ( 2.749590660225081251, -75.84330483478258600, -11.46114634323648396 ) ) ;
#5274 = CARTESIAN_POINT ( 'NONE',  ( -1.256362333281000110, -77.62034566960160475, 0.2270125678640999844 ) ) ;
#5275 = CARTESIAN_POINT ( 'NONE',  ( -12.00000000000000000, -18.75000000000000000, 1.250000000000000000 ) ) ;
#5276 = CARTESIAN_POINT ( 'NONE',  ( -13.94827586207000003, -33.10361340872000113, -8.082385102019000922E-06 ) ) ;
#5277 = ORIENTED_EDGE ( 'NONE', *, *, #7186, .T. ) ;
#5278 = CARTESIAN_POINT ( 'NONE',  ( 8.274772994052357333, -61.77888614391775235, -9.689268730118849149 ) ) ;
#5279 = VERTEX_POINT ( 'NONE', #10759 ) ;
#5280 = EDGE_LOOP ( 'NONE', ( #16907, #43622, #39884 ) ) ;
#5281 = EDGE_CURVE ( 'NONE', #58211, #26037, #1041, .T. ) ;
#5282 = CARTESIAN_POINT ( 'NONE',  ( -1.189861610678828008, -80.57546913605862926, 0.3832792502281296421 ) ) ;
#5283 = EDGE_CURVE ( 'NONE', #44413, #56422, #1324, .T. ) ;
#5284 = CARTESIAN_POINT ( 'NONE',  ( 9.767191983224998708, -79.76072787413951914, 0.05162932631433000269 ) ) ;
#5285 = ORIENTED_EDGE ( 'NONE', *, *, #47801, .F. ) ;
#5286 = CARTESIAN_POINT ( 'NONE',  ( -1.977101394398999679, -76.01185016949999351, 11.71119668716000106 ) ) ;
#5287 = LINE ( 'NONE', #23295, #4178 ) ;
#5288 = CARTESIAN_POINT ( 'NONE',  ( -0.6796159160043999670, -78.61816101900998888, 1.376191089724000172 ) ) ;
#5289 = ORIENTED_EDGE ( 'NONE', *, *, #4889, .T. ) ;
#5290 = CARTESIAN_POINT ( 'NONE',  ( -9.391369684923001060, -77.11827694988500070, 1.399863080762999923 ) ) ;
#5291 = DIRECTION ( 'NONE',  ( 0.000000000000000000, 0.000000000000000000, -1.000000000000000000 ) ) ;
#5292 = CARTESIAN_POINT ( 'NONE',  ( 10.42531124905999995, -18.73514851523999880, -7.624341765453999997 ) ) ;
#5293 = CARTESIAN_POINT ( 'NONE',  ( 1.930860503546800500, -18.22582494088415928, -12.72930866331970279 ) ) ;
#5294 = CARTESIAN_POINT ( 'NONE',  ( 12.00000000000000888, -79.03958333333332575, -1.570796326794872577 ) ) ;
#5295 = EDGE_CURVE ( 'NONE', #14174, #22264, #22535, .T. ) ;
#5296 = CARTESIAN_POINT ( 'NONE',  ( 9.116782980790521407, -79.86451097818435585, 1.648924484312454419 ) ) ;
#5297 = CARTESIAN_POINT ( 'NONE',  ( 1.990533724726763820, -79.70208332345784186, 3.529387283865522473 ) ) ;
#5298 = EDGE_LOOP ( 'NONE', ( #6954, #18723, #25174, #2641, #39990, #4018 ) ) ;
#5299 = CARTESIAN_POINT ( 'NONE',  ( -1.750000000000000000, -18.75000000240999753, 12.50000000000000000 ) ) ;
#5300 = CARTESIAN_POINT ( 'NONE',  ( 9.754023262367999436, -76.21512124563000157, -7.509630405475999915 ) ) ;
#5301 = CARTESIAN_POINT ( 'NONE',  ( -0.3603946542032999689, -79.80096993136200467, 1.573953487139999829 ) ) ;
#5302 = VECTOR ( 'NONE', #58176, 1000.000000000000000 ) ;
#5303 = CARTESIAN_POINT ( 'NONE',  ( 3.490340410772612145, -2.109536202225938073, 0.4540853053036469911 ) ) ;
#5304 = CARTESIAN_POINT ( 'NONE',  ( 10.12290050124000018, -18.75000000007999645, -7.648026767085999822 ) ) ;
#5306 = ADVANCED_FACE ( 'NONE', ( #14288 ), #10280, .T. ) ;
#5305 = CARTESIAN_POINT ( 'NONE',  ( -7.421655993048999811, -78.44405766871000196, 9.763070719336001346 ) ) ;
#5307 = DIRECTION ( 'NONE',  ( 0.000000000000000000, -1.000000000000000000, 0.000000000000000000 ) ) ;
#5308 = CIRCLE ( 'NONE', #25073, 0.5000000000000000000 ) ;
#5309 = CARTESIAN_POINT ( 'NONE',  ( -10.18496935386999880, -57.04935285362000030, -7.710095619715000126 ) ) ;
#5310 = CIRCLE ( 'NONE', #27966, 2.299999999999999822 ) ;
#5311 = CARTESIAN_POINT ( 'NONE',  ( 10.58947069987000056, -78.34309102680099102, -3.845989281283999528 ) ) ;
#5312 = DIRECTION ( 'NONE',  ( 0.000000000000000000, 1.000000000000000000, 0.000000000000000000 ) ) ;
#5313 = CARTESIAN_POINT ( 'NONE',  ( -11.97720891572606128, -77.06026423996446795, -1.545522828243951929 ) ) ;
#5314 = CARTESIAN_POINT ( 'NONE',  ( -10.34326456654000026, -78.71838589773552997, 4.339929572939999147 ) ) ;
#5315 = AXIS2_PLACEMENT_3D ( 'NONE', #56725, #2418, #16283 ) ;
#5316 = ORIENTED_EDGE ( 'NONE', *, *, #38954, .F. ) ;
#5317 = CARTESIAN_POINT ( 'NONE',  ( -0.5331523304941999664, -82.92725009134899494, 1.241660107034999960 ) ) ;
#5318 = CARTESIAN_POINT ( 'NONE',  ( -1.091933803201964315, -78.64189527190625029, -0.6291797731469532806 ) ) ;
#5319 = CARTESIAN_POINT ( 'NONE',  ( -1.750000000001000089, -59.55077028460999600, -12.60356226396000068 ) ) ;
#5320 = CARTESIAN_POINT ( 'NONE',  ( 1.092232985442820992, -82.79166666666665719, 0.6295237254636267821 ) ) ;
#5321 = CARTESIAN_POINT ( 'NONE',  ( 7.685661446562000343, -77.00000000000000000, -5.583959896779000509 ) ) ;
#5322 = CARTESIAN_POINT ( 'NONE',  ( -1.519662023741000123, -82.80398532648199250, -0.6825586799200999977 ) ) ;
#5323 = CARTESIAN_POINT ( 'NONE',  ( -11.93030759001999996, -78.52007602460300006, -1.692197530282999907 ) ) ;
#5324 = CARTESIAN_POINT ( 'NONE',  ( 8.982692273745001899, -77.48629938523899341, 3.473391639513999429 ) ) ;
#5325 = CARTESIAN_POINT ( 'NONE',  ( 0.1978932475499107502, -76.07339481969196981, 11.74839477131042820 ) ) ;
#5326 = CARTESIAN_POINT ( 'NONE',  ( 11.03163745116999905, -78.70935830175899639, 0.06858965353743999571 ) ) ;
#5327 = CARTESIAN_POINT ( 'NONE',  ( 3.106054555984665289, -86.07390000031791999, -1.382904586457468943 ) ) ;
#5328 = ORIENTED_EDGE ( 'NONE', *, *, #23650, .T. ) ;
#5329 = DIRECTION ( 'NONE',  ( 0.000000000000000000, 0.000000000000000000, 1.000000000000000000 ) ) ;
#5330 = CARTESIAN_POINT ( 'NONE',  ( -0.03344221497652981323, -78.43735717367049176, -3.548192314505119960 ) ) ;
#5331 = CARTESIAN_POINT ( 'NONE',  ( -2.928603948516999900, -78.88694830811698466, 10.57767911662999971 ) ) ;
#5332 = CARTESIAN_POINT ( 'NONE',  ( 0.000000000000000000, -80.59999999999999432, 0.000000000000000000 ) ) ;
#5333 = CARTESIAN_POINT ( 'NONE',  ( 12.16540687204999927, -76.60484402282999383, -2.890821896307000038 ) ) ;
#5334 = DIRECTION ( 'NONE',  ( 0.000000000000000000, -1.000000000000000000, 0.000000000000000000 ) ) ;
#5335 = CARTESIAN_POINT ( 'NONE',  ( 8.790679651960999763, -17.06186536190000069, -8.797972003296999688 ) ) ;
#5336 = LINE ( 'NONE', #55514, #41904 ) ;
#5337 = EDGE_LOOP ( 'NONE', ( #38765, #37194, #29093, #6430 ) ) ;
#5338 = CARTESIAN_POINT ( 'NONE',  ( -10.97184146967999929, -79.19473956280799598, 1.968068935562000243 ) ) ;
#5339 = CARTESIAN_POINT ( 'NONE',  ( 12.70455814331302768, -54.23992875941878822, 1.489882837217631595 ) ) ;
#5340 = CARTESIAN_POINT ( 'NONE',  ( 5.413904038987143785, -79.83333333333334281, 9.393203674808290771 ) ) ;
#5341 = CARTESIAN_POINT ( 'NONE',  ( 3.548349909811000291, -78.43735717367052018, 2.094141616746843404 ) ) ;
#5342 = CARTESIAN_POINT ( 'NONE',  ( -0.5388325380043634816, -81.51077761135140065, 1.127735728752304656 ) ) ;
#5343 = CARTESIAN_POINT ( 'NONE',  ( -3.571993175857000491, -79.40574064831898227, -10.45556112308999985 ) ) ;
#5344 = CARTESIAN_POINT ( 'NONE',  ( -8.944216015804251185, -77.00000000000000000, -2.811381416889873197 ) ) ;
#5345 = CARTESIAN_POINT ( 'NONE',  ( 13.89248035986000041, -9.608407476587998985, 2.632528379384000019E-05 ) ) ;
#5346 = AXIS2_PLACEMENT_3D ( 'NONE', #35964, #1153, #14690 ) ;
#5347 = CARTESIAN_POINT ( 'NONE',  ( 1.310679582531387943, -81.20833333333331439, -0.7554284705563468760 ) ) ;
#5348 = CARTESIAN_POINT ( 'NONE',  ( -9.000000000000000000, -91.89999999999999147, -2.445120494964999949E-12 ) ) ;
#5349 = AXIS2_PLACEMENT_3D ( 'NONE', #5818, #32664, #50717 ) ;
#5350 = CARTESIAN_POINT ( 'NONE',  ( 10.36935812844000004, -78.17876026662598576, -2.835297515976000327 ) ) ;
#5351 = CARTESIAN_POINT ( 'NONE',  ( -9.307291666739137881, -79.69270833332970483, -0.9752027189503162941 ) ) ;
#5352 = ORIENTED_EDGE ( 'NONE', *, *, #56248, .F. ) ;
#5353 = AXIS2_PLACEMENT_3D ( 'NONE', #19626, #10193, #28173 ) ;
#5354 = ORIENTED_EDGE ( 'NONE', *, *, #9210, .T. ) ;
#5355 = CARTESIAN_POINT ( 'NONE',  ( -5.610847844242282001, -77.82499999999998863, 7.718163323371708628 ) ) ;
#5356 = CARTESIAN_POINT ( 'NONE',  ( 9.234857099017842685, -78.80734080730690039, -5.504304055585024003 ) ) ;
#5357 = CIRCLE ( 'NONE', #35509, 13.86363636363999952 ) ;
#5358 = ORIENTED_EDGE ( 'NONE', *, *, #49358, .T. ) ;
#5359 = CARTESIAN_POINT ( 'NONE',  ( -1.750000000001000089, -23.24999998674999802, 12.56594318051000059 ) ) ;
#5360 = CARTESIAN_POINT ( 'NONE',  ( 0.01567759588933310619, -82.82395834925023337, 3.411067620805362299 ) ) ;
#5361 = CARTESIAN_POINT ( 'NONE',  ( 8.220407391966000787, -61.61950084198999633, 9.523310056136001123 ) ) ;
#5363 = EDGE_CURVE ( 'NONE', #25542, #22170, #32865, .T. ) ;
#5362 = DIRECTION ( 'NONE',  ( 0.000000000000000000, 1.000000000000000000, 0.000000000000000000 ) ) ;
#5364 = CARTESIAN_POINT ( 'NONE',  ( 11.95265301635149946, -78.80527988016636698, 0.8087635557727725910 ) ) ;
#5365 = CARTESIAN_POINT ( 'NONE',  ( 3.632329907060999563, -80.18225450229719797, 10.45854222826000068 ) ) ;
#5366 = CARTESIAN_POINT ( 'NONE',  ( 10.44969936162916646, -81.00000000000000000, 3.411603317218904863 ) ) ;
#5367 = ORIENTED_EDGE ( 'NONE', *, *, #37753, .T. ) ;
#5368 = CARTESIAN_POINT ( 'NONE',  ( 10.61050599188999932, -77.92876026662598576, -2.901234667509999809 ) ) ;
#5369 = ORIENTED_EDGE ( 'NONE', *, *, #6783, .T. ) ;
#5370 = CARTESIAN_POINT ( 'NONE',  ( 8.392153346702146521, -77.38471673975136866, 3.904227155189466725 ) ) ;
#5371 = CARTESIAN_POINT ( 'NONE',  ( 5.341789944771999643, -77.70465779647399529, 9.661750877468000098 ) ) ;
#5372 = DIRECTION ( 'NONE',  ( 0.000000000000000000, -1.000000000000000000, 0.000000000000000000 ) ) ;
#5373 = CARTESIAN_POINT ( 'NONE',  ( 1.577356090230000119, -77.75908736353699169, 0.3451975780249000314 ) ) ;
#5374 = CARTESIAN_POINT ( 'NONE',  ( -10.03847181070773331, -18.20634590497699179, -7.678636148852304721 ) ) ;
#5375 = CARTESIAN_POINT ( 'NONE',  ( -8.596418555780466875, -80.94791666666665719, 6.606377239730298001 ) ) ;
#5376 = CARTESIAN_POINT ( 'NONE',  ( 0.4102083068199999794, -78.35645190970998897, -1.574926093281000083 ) ) ;
#5377 = CARTESIAN_POINT ( 'NONE',  ( 11.10498291493000167, -80.22745348979398727, -1.830582403018000015 ) ) ;
#5378 = CARTESIAN_POINT ( 'NONE',  ( 0.2605153439964000284, -79.55608152108499098, -10.93709047653000077 ) ) ;
#5379 = CARTESIAN_POINT ( 'NONE',  ( -7.634438871657000192, -23.74781730700000182, -10.30764054782000017 ) ) ;
#5380 = EDGE_CURVE ( 'NONE', #36499, #34323, #14580, .T. ) ;
#5381 = CARTESIAN_POINT ( 'NONE',  ( 12.71658872082999814, -55.48415267986000288, -1.931087888240000217 ) ) ;
#5382 = CARTESIAN_POINT ( 'NONE',  ( -3.559158646470999887, -84.54268354761398996, -0.4649029617932999847 ) ) ;
#5383 = ORIENTED_EDGE ( 'NONE', *, *, #1617, .F. ) ;
#5384 = B_SPLINE_CURVE_WITH_KNOTS ( 'NONE', 3,
 ( #54333, #4436, #45185, #4735, #58160, #13873, #31567, #31867, #32157, #17726, #49909, #40451, #54037, #35714, #32445, #26855, #53743, #23320, #49616, #50196, #13576, #14159, #5313, #8863, #22733, #44886, #27732, #13279, #40744, #50489, #18896, #913, #9163, #9456, #36887, #23025, #31271, #14450, #49313, #22436, #10043, #337, #18317, #45478, #46069, #28024, #43, #5591, #23604, #41037, #18019, #5021, #36308, #27442, #628, #18611, #19770, #51662, #20346, #11499, #33901, #11210, #10625, #24774, #42209, #19186, #6765, #29473, #47528, #1775, #15337, #15037, #37766, #24483, #33328, #55787, #47236, #38343, #20067, #38055, #56365, #51077, #37181, #56078, #6180, #29188, #37468, #55194, #15915, #7057, #19475, #42787, #24192, #51365, #41616, #51943, #33618, #10329, #50784, #10920, #41911, #15624, #1196, #14737, #32736, #28901, #28309, #6472, #55489, #46360, #2351, #46947, #5885, #42498, #33031, #23892, #46653, #1484, #28607, #2066, #52792, #12631, #7628, #20915, #35339, #17065, #21776, #30044, #38918 ),
 .UNSPECIFIED., .F., .F.,
 ( 4, 2, 2, 2, 2, 2, 1, 2, 2, 2, 2, 2, 2, 2, 2, 2, 2, 1, 2, 2, 1, 1, 2, 2, 1, 2, 2, 1, 2, 2, 2, 2, 2, 2, 2, 1, 2, 2, 2, 2, 2, 2, 2, 1, 2, 2, 1, 2, 2, 1, 1, 2, 2, 1, 2, 2, 2, 2, 2, 2, 2, 2, 2, 2, 1, 2, 2, 2, 2, 2, 4 ),
 ( 0.000000000000000000, 0.01562500000000000000, 0.03125000000000000000, 0.04687500000000000000, 0.06250000000000000000, 0.07812500000000000000, 0.09375000000000000000, 0.1093750000000000000, 0.1250000000000000000, 0.1406250000000000000, 0.1562500000000000000, 0.1718750000000000278, 0.1875000000000000555, 0.2031250000000000833, 0.2187500000000001110, 0.2343750000000001388, 0.2421875000000001388, 0.2500000000000001665, 0.2656250000000001665, 0.2734375000000001665, 0.2812500000000001665, 0.2968750000000001665, 0.3046875000000001665, 0.3125000000000001665, 0.3281250000000001665, 0.3359375000000001665, 0.3437500000000001665, 0.3593750000000001665, 0.3671875000000001665, 0.3750000000000001665, 0.3906250000000001665, 0.4062500000000001665, 0.4218750000000001665, 0.4375000000000001665, 0.4687500000000001665, 0.5000000000000001110, 0.5312500000000001110, 0.5625000000000001110, 0.5781250000000001110, 0.5937500000000001110, 0.6093750000000001110, 0.6250000000000001110, 0.6328125000000001110, 0.6406250000000001110, 0.6562500000000001110, 0.6640625000000001110, 0.6718750000000001110, 0.6875000000000001110, 0.6953125000000001110, 0.7031250000000001110, 0.7187500000000001110, 0.7265625000000001110, 0.7343750000000001110, 0.7500000000000001110, 0.7578125000000001110, 0.7656250000000001110, 0.7812500000000001110, 0.7968750000000001110, 0.8125000000000001110, 0.8281250000000001110, 0.8437500000000001110, 0.8593750000000001110, 0.8750000000000001110, 0.8906250000000001110, 0.9062500000000001110, 0.9218750000000001110, 0.9375000000000001110, 0.9531250000000001110, 0.9687500000000001110, 0.9843750000000001110, 1.000000000000000000 ),
 .UNSPECIFIED. ) ;
#5385 = DIRECTION ( 'NONE',  ( -0.7071067811865475727, 0.000000000000000000, -0.7071067811865475727 ) ) ;
#5386 = CARTESIAN_POINT ( 'NONE',  ( 9.562223978213696185, -77.88793088717281421, 4.911682316942298065 ) ) ;
#5387 = CARTESIAN_POINT ( 'NONE',  ( 3.999999999993000266, -77.30000000000720206, -8.632702228606999814E-11 ) ) ;
#5388 = AXIS2_PLACEMENT_3D ( 'NONE', #12129, #52578, #58376 ) ;
#5390 = CARTESIAN_POINT ( 'NONE',  ( -1.250000000000000000, -60.04999999966999980, -12.00000000000000000 ) ) ;
#5389 = DIRECTION ( 'NONE',  ( -0.7071067811865475727, 0.000000000000000000, -0.7071067811865475727 ) ) ;
#5391 = CARTESIAN_POINT ( 'NONE',  ( 3.518011427261086954, -3.002431050661036327, 0.1098636256542055017 ) ) ;
#5392 = CARTESIAN_POINT ( 'NONE',  ( 4.409055568808000203, -77.41539556192998361, 8.316935944130001701 ) ) ;
#5393 = CARTESIAN_POINT ( 'NONE',  ( 3.647699722740940675, -86.02148118236289065, -1.624060551956039822 ) ) ;
#5394 = CARTESIAN_POINT ( 'NONE',  ( 10.22699339414000086, -77.67369350912798609, 4.434321446068000050 ) ) ;
#5395 = CARTESIAN_POINT ( 'NONE',  ( 0.000000000000000000, -60.04999999966999980, 12.00000000000000000 ) ) ;
#5396 = CARTESIAN_POINT ( 'NONE',  ( -10.73991933103999941, -80.86972431869342870, 2.961644346888999912 ) ) ;
#5397 = CIRCLE ( 'NONE', #42995, 1.750000000000000000 ) ;
#5398 = ORIENTED_EDGE ( 'NONE', *, *, #10186, .F. ) ;
#5399 = FACE_OUTER_BOUND ( 'NONE', #18724, .T. ) ;
#5400 = CARTESIAN_POINT ( 'NONE',  ( -3.388689987348999733, -2.762137290292000280, 2.061041899425999802 ) ) ;
#5401 = CARTESIAN_POINT ( 'NONE',  ( -7.803863155890000236, -78.20233499673999233, 8.057160196619001624 ) ) ;
#5402 = CARTESIAN_POINT ( 'NONE',  ( 10.28103400416999946, -78.14831066145598015, 3.842432268884000024 ) ) ;
#5403 = CARTESIAN_POINT ( 'NONE',  ( 9.038948602518001252, -25.33262223864999640, -9.029786144013998594 ) ) ;
#5404 = CARTESIAN_POINT ( 'NONE',  ( -10.31421052434999908, -76.72175206120299151, 3.823226550887000030 ) ) ;
#5405 = EDGE_CURVE ( 'NONE', #56093, #1567, #54741, .T. ) ;
#5406 = CARTESIAN_POINT ( 'NONE',  ( 6.559824298179475655, -79.75000000000000000, -6.561935513396097264 ) ) ;
#5407 = LINE ( 'NONE', #1576, #14491 ) ;
#5408 = CARTESIAN_POINT ( 'NONE',  ( -3.362425624285000136, -84.83242953870899328, -2.469947173108999916 ) ) ;
#5409 = CARTESIAN_POINT ( 'NONE',  ( -0.3926218265389190276, -79.60416666666668561, -1.460959015002473826 ) ) ;
#5410 = CARTESIAN_POINT ( 'NONE',  ( 1.250000000000000000, -23.44678171330999916, -12.50000000000000000 ) ) ;
#5411 = CARTESIAN_POINT ( 'NONE',  ( 10.58947069987000056, -77.90146380445199270, -3.845989281283999528 ) ) ;
#5412 = CARTESIAN_POINT ( 'NONE',  ( 1.551146335801999898, -80.99088618300999087, 0.6076261867840000441 ) ) ;
#5413 = CARTESIAN_POINT ( 'NONE',  ( -0.7268831363637999754, -77.94139102152999499, 1.101817922911999981 ) ) ;
#5414 = CARTESIAN_POINT ( 'NONE',  ( -11.68767212001979061, -79.32083333333332575, -3.140974612311365988 ) ) ;
#5415 = CARTESIAN_POINT ( 'NONE',  ( -1.549803789708370738, -82.27831976753381582, -0.5760661418227226438 ) ) ;
#5416 = DIRECTION ( 'NONE',  ( 0.000000000000000000, -1.000000000000000000, 0.000000000000000000 ) ) ;
#5417 = CARTESIAN_POINT ( 'NONE',  ( -10.75000000000000000, -80.09999999999999432, -1.711887504597999906E-14 ) ) ;
#5418 = DIRECTION ( 'NONE',  ( -0.6489586469534679436, -0.04890178980860759861, 0.7592504787603620020 ) ) ;
#5419 = CARTESIAN_POINT ( 'NONE',  ( 12.50409217853026078, -54.27871355468435866, -1.233808106764433532 ) ) ;
#5420 = VERTEX_POINT ( 'NONE', #37308 ) ;
#5421 = CARTESIAN_POINT ( 'NONE',  ( -1.249786646214342989, -81.60930685382331262, -0.1405899892054735811 ) ) ;
#5422 = CARTESIAN_POINT ( 'NONE',  ( 11.14673908614000020, -78.64163123734599026, 0.06930530262389000828 ) ) ;
#5423 = CARTESIAN_POINT ( 'NONE',  ( -9.549999999999998934, -76.89999999999999147, 0.000000000000000000 ) ) ;
#5424 = VERTEX_POINT ( 'NONE', #1610 ) ;
#5425 = VERTEX_POINT ( 'NONE', #50038 ) ;
#5426 = CARTESIAN_POINT ( 'NONE',  ( 0.1605656202615999839, -81.46865411194299611, 1.408644050778000034 ) ) ;
#5427 = VERTEX_POINT ( 'NONE', #55324 ) ;
#5428 = DIRECTION ( 'NONE',  ( 0.000000000000000000, -1.000000000000000000, 0.000000000000000000 ) ) ;
#5429 = VERTEX_POINT ( 'NONE', #37602 ) ;
#5430 = CARTESIAN_POINT ( 'NONE',  ( -1.669849926071999890, -18.62771399582999976, 12.48404299553000030 ) ) ;
#5431 = SHAPE_REPRESENTATION_RELATIONSHIP ( 'NONE' , 'NONE' ,  #13452, #35529 ) ;
#5432 = CARTESIAN_POINT ( 'NONE',  ( -3.277886346742791890, -80.12604165830404668, 1.054380925102407218 ) ) ;
#5434 = ADVANCED_FACE ( 'NONE', ( #14868 ), #55618, .F. ) ;
#5433 = CARTESIAN_POINT ( 'NONE',  ( -0.8742025125545000996, -79.20261001420199420, 9.984153739810000872 ) ) ;
#5435 = CARTESIAN_POINT ( 'NONE',  ( 5.154876033940102964, -78.27220474274599837, -7.680359545439894298 ) ) ;
#5436 = DIRECTION ( 'NONE',  ( 0.000000000000000000, -1.000000000000000000, 0.000000000000000000 ) ) ;
#5437 = AXIS2_PLACEMENT_3D ( 'NONE', #11614, #2466, #21320 ) ;
#5438 = ORIENTED_EDGE ( 'NONE', *, *, #51508, .F. ) ;
#5440 = ORIENTED_EDGE ( 'NONE', *, *, #37309, .T. ) ;
#5439 = EDGE_CURVE ( 'NONE', #35786, #46363, #9585, .T. ) ;
#5441 = CARTESIAN_POINT ( 'NONE',  ( 0.000000000000000000, -78.69999999999998863, 0.000000000000000000 ) ) ;
#5442 = CARTESIAN_POINT ( 'NONE',  ( 0.000000000000000000, -82.50000000000000000, 0.000000000000000000 ) ) ;
#5443 = CARTESIAN_POINT ( 'NONE',  ( -0.1636246173744726473, -81.38541666666664298, 1.249999999999999112 ) ) ;
#5444 = VECTOR ( 'NONE', #10860, 1000.000000000000000 ) ;
#5445 = CARTESIAN_POINT ( 'NONE',  ( 1.722320550013656915, -61.03663688784501318, -12.71171904440563161 ) ) ;
#5446 = CARTESIAN_POINT ( 'NONE',  ( 2.260091721765999928, -78.91355385020298741, -9.437303113984999214 ) ) ;
#5447 = CIRCLE ( 'NONE', #39369, 13.94827586206999825 ) ;
#5448 = B_SPLINE_CURVE_WITH_KNOTS ( 'NONE', 3,
 ( #12344, #48657, #43935, #35934, #13500, #4056 ),
 .UNSPECIFIED., .F., .F.,
 ( 4, 1, 1, 4 ),
 ( 0.000000000000000000, 0.3333333333333000081, 0.6666666666667000474, 1.000000000000000000 ),
 .UNSPECIFIED. ) ;
#5449 = CARTESIAN_POINT ( 'NONE',  ( 10.36597333715451263, -60.57522428980394125, 7.635925938732074592 ) ) ;
#5450 = CARTESIAN_POINT ( 'NONE',  ( 3.586328456911428653, -85.81453820040007940, 1.233688378895768434 ) ) ;
#5451 = CARTESIAN_POINT ( 'NONE',  ( 11.66345872527999994, -77.61523079875999542, 5.269998857220999255 ) ) ;
#5452 = CARTESIAN_POINT ( 'NONE',  ( -0.2789364955927000067, -79.53354959200999019, 1.441751320050999929 ) ) ;
#5453 = CARTESIAN_POINT ( 'NONE',  ( -12.58335110161999815, -21.74888345808999901, -1.667961430005999945 ) ) ;
#5454 = EDGE_CURVE ( 'NONE', #52467, #34093, #5154, .T. ) ;
#5455 = CARTESIAN_POINT ( 'NONE',  ( 0.1120494588183876261, -76.57414459540065366, 11.74947323293256574 ) ) ;
#5456 = CARTESIAN_POINT ( 'NONE',  ( -4.005627318223000444, -81.61969232303898991, 1.168341821262999902 ) ) ;
#5457 = CARTESIAN_POINT ( 'NONE',  ( -11.03620408507000050, -80.28218522619640396, -2.260839449595000161 ) ) ;
#5458 = CARTESIAN_POINT ( 'NONE',  ( 8.449950666592000559, -78.71463667140099574, -4.961522297560000183 ) ) ;
#5459 = FACE_OUTER_BOUND ( 'NONE', #37962, .T. ) ;
#5460 = CARTESIAN_POINT ( 'NONE',  ( 2.185735370214000106, -82.24605496681199668, -2.793614180511000189 ) ) ;
#5461 = CARTESIAN_POINT ( 'NONE',  ( 1.315129997485000146, -78.52893215530700388, 0.2213803045116000123 ) ) ;
#5462 = CARTESIAN_POINT ( 'NONE',  ( -6.043427764450833628, -78.31666666666667709, 10.48543666025107335 ) ) ;
#5463 = PLANE ( 'NONE',  #45815 ) ;
#5464 = CARTESIAN_POINT ( 'NONE',  ( 3.383845406481000406, -2.529494972095000183, -1.742318191517000070 ) ) ;
#5465 = CARTESIAN_POINT ( 'NONE',  ( -0.7681833999686432657, -79.07291666666668561, -0.9995835529977258327 ) ) ;
#5466 = ORIENTED_EDGE ( 'NONE', *, *, #32095, .T. ) ;
#5467 = CARTESIAN_POINT ( 'NONE',  ( -11.75000000000000000, -78.79999999999999716, 1.318041981624000073E-14 ) ) ;
#5468 = CARTESIAN_POINT ( 'NONE',  ( 8.838834764832000701, -60.04999999966999980, -8.838834764832000701 ) ) ;
#5469 = DIRECTION ( 'NONE',  ( 0.7071067811865475727, 0.000000000000000000, 0.7071067811865475727 ) ) ;
#5470 = CARTESIAN_POINT ( 'NONE',  ( 1.930989179114000143, -57.04546192861999998, 12.80896991328000034 ) ) ;
#5471 = CARTESIAN_POINT ( 'NONE',  ( -9.339950055924999717, -78.00929442844000050, -9.061158367717998985 ) ) ;
#5472 = CARTESIAN_POINT ( 'NONE',  ( -1.200332545804832840, -79.48406602089589512, 10.68275685977173950 ) ) ;
#5473 = CARTESIAN_POINT ( 'NONE',  ( 5.818877114584999788, -79.20403998579800486, 7.945831408065000545 ) ) ;
#5474 = CARTESIAN_POINT ( 'NONE',  ( 9.729416038176543324, -78.49535593849341808, 6.585780853366507870 ) ) ;
#5475 = DIRECTION ( 'NONE',  ( 0.7071067811864970576, -3.534294796762985261E-08, 0.7071067811865970887 ) ) ;
#5476 = CARTESIAN_POINT ( 'NONE',  ( -2.009571257635000219, -77.19648208238979237, 10.87244111694000104 ) ) ;
#5477 = CARTESIAN_POINT ( 'NONE',  ( -0.6678841138425000157, -81.44112908879199608, -1.350122867467000054 ) ) ;
#5478 = LINE ( 'NONE', #1081, #15371 ) ;
#5479 = CARTESIAN_POINT ( 'NONE',  ( -7.476203163627999970, -77.57278449298998169, -5.719923538308999689 ) ) ;
#5481 = DIRECTION ( 'NONE',  ( 0.000000000000000000, -1.000000000000000000, 0.000000000000000000 ) ) ;
#5480 = CARTESIAN_POINT ( 'NONE',  ( -1.715416423673999935, -82.73892731861099037, 3.757107549244000033 ) ) ;
#5482 = CARTESIAN_POINT ( 'NONE',  ( 1.861092857305999937, -79.71054805011500832, -9.371850619045000386 ) ) ;
#5483 = CARTESIAN_POINT ( 'NONE',  ( 5.246383657897999875, -77.06100733245999379, -10.79237965019999912 ) ) ;
#5484 = FACE_BOUND ( 'NONE', #26744, .T. ) ;
#5485 = EDGE_CURVE ( 'NONE', #7824, #41164, #27858, .T. ) ;
#5486 = CARTESIAN_POINT ( 'NONE',  ( -7.264472637402048960, -77.16596736302702197, -7.925599033090998446 ) ) ;
#5487 = CARTESIAN_POINT ( 'NONE',  ( 10.98749645531832542, -79.08354319426250356, 4.929334125397528688 ) ) ;
#5488 = CARTESIAN_POINT ( 'NONE',  ( 3.962812355711001544, -78.85171438276199751, 7.925624711422035062 ) ) ;
#5489 = ORIENTED_EDGE ( 'NONE', *, *, #8464, .T. ) ;
#5490 = CARTESIAN_POINT ( 'NONE',  ( -8.850953919802000414, -79.69309878738100394, -8.146641040006999290 ) ) ;
#5491 = CARTESIAN_POINT ( 'NONE',  ( -6.525519130240628130, -80.42663223072267442, 8.600139951612055356 ) ) ;
#5492 = ORIENTED_EDGE ( 'NONE', *, *, #41895, .T. ) ;
#5493 = CARTESIAN_POINT ( 'NONE',  ( 0.000000000000000000, -0.1000000007601000024, 0.000000000000000000 ) ) ;
#5494 = ORIENTED_EDGE ( 'NONE', *, *, #52565, .F. ) ;
#5495 = EDGE_LOOP ( 'NONE', ( #15599, #35180, #19449, #12572 ) ) ;
#5496 = CARTESIAN_POINT ( 'NONE',  ( -3.066878322771222631, -2.627509113554599374, -1.087878959322058581 ) ) ;
#5497 = ORIENTED_EDGE ( 'NONE', *, *, #3738, .F. ) ;
#5498 = CARTESIAN_POINT ( 'NONE',  ( 3.225040040299000044, -79.33493425789589537, -1.476714839321999984 ) ) ;
#5499 = CARTESIAN_POINT ( 'NONE',  ( 14.00000000000000000, -80.90000000000000568, 0.000000000000000000 ) ) ;
#5500 = B_SPLINE_SURFACE_WITH_KNOTS ( 'NONE', 3, 3, ( 
 ( #15776, #46808, #20217, #25208 ),
 ( #33768, #10780, #7206, #52091 ),
 ( #47385, #47095, #38206, #42362 ),
 ( #43227, #42066, #19924, #55939 ),
 ( #42942, #11076, #20783, #15489 ),
 ( #38784, #33479, #42649, #19625 ),
 ( #15191, #56802, #16362, #34342 ),
 ( #28758, #1635, #37622, #55641 ),
 ( #33182, #57375, #21069, #39075 ),
 ( #31062, #43514, #58245, #48524 ),
 ( #30495, #12213, #35794, #22221 ),
 ( #3923, #57950, #57655, #3640 ),
 ( #8068, #8354, #26065, #16648 ),
 ( #17504, #40233, #17807, #8650 ),
 ( #52947, #34632, #11932, #52660 ),
 ( #47962, #44670, #48810, #49100 ),
 ( #21643, #26636, #29909, #44371 ) ),
 .UNSPECIFIED., .F., .F., .F.,
 ( 4, 1, 1, 1, 1, 1, 1, 1, 1, 1, 1, 1, 1, 1, 4 ),
 ( 4, 4 ),
 ( -0.01011408452870000106, 0.000000000000000000, 0.08333333333333001192, 0.1666666666667000196, 0.2500000000000000000, 0.3333333333333000081, 0.4166666666666999919, 0.5000000000000000000, 0.5833333333333000637, 0.6666666666667000474, 0.7500000000000000000, 0.8333333333333000637, 0.9166666666667000474, 1.000000000000000000, 1.010362559107000013 ),
 ( -0.3559705546268999710, 1.357612419602000076 ),
 .UNSPECIFIED. ) ;
#5501 = ORIENTED_EDGE ( 'NONE', *, *, #25525, .T. ) ;
#5502 = DIRECTION ( 'NONE',  ( 1.000000000000000000, 0.000000000000000000, 0.000000000000000000 ) ) ;
#5504 = EDGE_CURVE ( 'NONE', #3819, #56496, #27179, .T. ) ;
#5503 = ORIENTED_EDGE ( 'NONE', *, *, #26459, .F. ) ;
#5505 = CARTESIAN_POINT ( 'NONE',  ( 10.75000000000000000, -80.75000000000000000, 3.489821576044999869E-14 ) ) ;
#5506 = CARTESIAN_POINT ( 'NONE',  ( -1.959727320071604773, -77.45872416430094631, -9.504382773771103743 ) ) ;
#5507 = CARTESIAN_POINT ( 'NONE',  ( -11.13124813254851198, -79.79999999999998295, -4.350558907888798288 ) ) ;
#5508 = CARTESIAN_POINT ( 'NONE',  ( -12.50728313516488832, -17.00024825485232682, 0.1773838730325038027 ) ) ;
#5509 = CARTESIAN_POINT ( 'NONE',  ( -12.51072239526000196, -15.69705297114000331, -0.7871079366006996647 ) ) ;
#5510 = CARTESIAN_POINT ( 'NONE',  ( -10.99972769911000015, -76.25165398600699973, 2.019869862886000345 ) ) ;
#5511 = CARTESIAN_POINT ( 'NONE',  ( -9.549999999953000085, -76.40000000004698677, 5.125988344190999543E-10 ) ) ;
#5512 = CARTESIAN_POINT ( 'NONE',  ( -4.819527309429000539, -76.23371184005799250, 10.14178905882999970 ) ) ;
#5513 = EDGE_CURVE ( 'NONE', #40202, #31102, #11338, .T. ) ;
#5514 = CARTESIAN_POINT ( 'NONE',  ( 1.565620768230334470, -78.73876823178706275, -9.127934873522015380 ) ) ;
#5515 = CARTESIAN_POINT ( 'NONE',  ( -0.5392637480173118059, -23.41532333361683982, -10.98678411023716883 ) ) ;
#5516 = CARTESIAN_POINT ( 'NONE',  ( 1.313995274498999999, -80.37066597088099229, -0.2280190045613000038 ) ) ;
#5517 = ADVANCED_FACE ( 'NONE', ( #52071 ), #43580, .T. ) ;
#5518 = FACE_OUTER_BOUND ( 'NONE', #22852, .T. ) ;
#5519 = CARTESIAN_POINT ( 'NONE',  ( -0.7823459921530014904, -78.33311419357939087, 12.04988513590113897 ) ) ;
#5520 = CARTESIAN_POINT ( 'NONE',  ( 3.755321587697000307, -79.15917549782629692, -1.719320632020000073 ) ) ;
#5521 = CARTESIAN_POINT ( 'NONE',  ( 9.576515689347999682, -77.45311332859900233, 1.209795274715000257 ) ) ;
#5522 = CARTESIAN_POINT ( 'NONE',  ( -12.78037507862999966, -17.70670131430000183, 1.812742845510000089 ) ) ;
#5523 = CARTESIAN_POINT ( 'NONE',  ( -1.156432516341094896, -83.06912217221712069, 0.4743574928646153710 ) ) ;
#5524 = CARTESIAN_POINT ( 'NONE',  ( 9.500000000000005329, -77.14374999999998295, -0.7461282552275557700 ) ) ;
#5525 = CARTESIAN_POINT ( 'NONE',  ( -0.4635254915625000027, -82.00000000000000000, -1.426584774443000025 ) ) ;
#5526 = CARTESIAN_POINT ( 'NONE',  ( 1.247385801072999900, -24.47722256257999973, 12.50301438876999960 ) ) ;
#5527 = CARTESIAN_POINT ( 'NONE',  ( 10.01234990226999955, -55.50150862742999891, 7.653559502261000347 ) ) ;
#5528 = CARTESIAN_POINT ( 'NONE',  ( 1.510215997576003222, -79.60432664446625495, 0.09564393186081109055 ) ) ;
#5529 = CARTESIAN_POINT ( 'NONE',  ( 10.36935812844000004, -78.17876026662598576, -2.835297515976000327 ) ) ;
#5530 = PLANE ( 'NONE',  #3146 ) ;
#5531 = CARTESIAN_POINT ( 'NONE',  ( 12.46165725306000027, -23.67155322522999938, 1.631637378453000053 ) ) ;
#5532 = CARTESIAN_POINT ( 'NONE',  ( -10.56885402377634797, -77.43492478567101500, 2.086924253389536243 ) ) ;
#5533 = DIRECTION ( 'NONE',  ( -4.529352715887982601E-09, -0.9999999999999983347, 5.940771866771979903E-08 ) ) ;
#5534 = EDGE_CURVE ( 'NONE', #54221, #5753, #42921, .T. ) ;
#5536 = CARTESIAN_POINT ( 'NONE',  ( -1.980584515756000030, -23.26485150094000076, -12.76303204340999997 ) ) ;
#5535 = CARTESIAN_POINT ( 'NONE',  ( 1.500000000000000000, -80.25000000000000000, 0.000000000000000000 ) ) ;
#5537 = CARTESIAN_POINT ( 'NONE',  ( 8.455103393227000552, -75.85439764561999709, -8.811608351744000700 ) ) ;
#5538 = ORIENTED_EDGE ( 'NONE', *, *, #6928, .T. ) ;
#5539 = CARTESIAN_POINT ( 'NONE',  ( 3.126065026453999973, -82.63071544543198854, -1.787417263702000048 ) ) ;
#5540 = CARTESIAN_POINT ( 'NONE',  ( -4.697326221550000014, -81.11872762313059582, 9.999795703097998256 ) ) ;
#5541 = CARTESIAN_POINT ( 'NONE',  ( 8.333454457512889491, -78.31429970678456698, -4.014433121081317779 ) ) ;
#5542 = CARTESIAN_POINT ( 'NONE',  ( 10.04568514500116372, -54.24913840229667983, 7.921286339673507371 ) ) ;
#5543 = CARTESIAN_POINT ( 'NONE',  ( -8.649885944100999424, -77.95660330126699478, -7.141259254888000285 ) ) ;
#5544 = FACE_OUTER_BOUND ( 'NONE', #24892, .T. ) ;
#5545 = CARTESIAN_POINT ( 'NONE',  ( 2.243017272178000177, -79.03676744264699039, -9.366006557871001448 ) ) ;
#5546 = CARTESIAN_POINT ( 'NONE',  ( -3.693777716050999693, -1.773066864578999979, 1.600481400925999997 ) ) ;
#5547 = CARTESIAN_POINT ( 'NONE',  ( -8.141768944221999149, -79.22275767078099307, 5.616688595088000113 ) ) ;
#5548 = CARTESIAN_POINT ( 'NONE',  ( -1.931087888049999979, -55.48415522678000400, 12.71658889739000031 ) ) ;
#5549 = EDGE_LOOP ( 'NONE', ( #7465, #28790, #49499, #535, #12184, #37449, #17548, #17218, #35107 ) ) ;
#5550 = EDGE_CURVE ( 'NONE', #32631, #53612, #22841, .T. ) ;
#5551 = CARTESIAN_POINT ( 'NONE',  ( -4.299999999999999822, -81.99999999999998579, 0.000000000000000000 ) ) ;
#5552 = CARTESIAN_POINT ( 'NONE',  ( -1.782734487936610934, -54.67754631409817279, -12.71547286922772457 ) ) ;
#5553 = CARTESIAN_POINT ( 'NONE',  ( 4.024324870012000233, -79.29007331913099677, -8.363631784355000320 ) ) ;
#5554 = VECTOR ( 'NONE', #35121, 1000.000000000000000 ) ;
#5555 = DIRECTION ( 'NONE',  ( 0.000000000000000000, 0.7071067811866525998, -0.7071067811864425456 ) ) ;
#5556 = ORIENTED_EDGE ( 'NONE', *, *, #2903, .F. ) ;
#5557 = EDGE_CURVE ( 'NONE', #37074, #54955, #30731, .T. ) ;
#5558 = CARTESIAN_POINT ( 'NONE',  ( -1.460959015002473826, -81.42083333333336270, -0.3926218265389207485 ) ) ;
#5559 = LINE ( 'NONE', #41581, #18050 ) ;
#5560 = ORIENTED_EDGE ( 'NONE', *, *, #43215, .T. ) ;
#5561 = CARTESIAN_POINT ( 'NONE',  ( -10.52667135666000142, -78.78354445816799512, 6.323366929881999887 ) ) ;
#5562 = CARTESIAN_POINT ( 'NONE',  ( -7.298419138992000121, -77.99709831745698807, -8.365328406272000805 ) ) ;
#5563 = CARTESIAN_POINT ( 'NONE',  ( -1.799490220168999954, -19.22870851082999977, 12.64502302238000020 ) ) ;
#5564 = EDGE_LOOP ( 'NONE', ( #42174, #13484, #45606, #15517, #9399 ) ) ;
#5565 = CIRCLE ( 'NONE', #7473, 0.6000000000000008660 ) ;
#5566 = CARTESIAN_POINT ( 'NONE',  ( -1.242201279478839959, -80.59188204877600015, 0.1373445331278350945 ) ) ;
#5567 = B_SPLINE_CURVE_WITH_KNOTS ( 'NONE', 3,
 ( #15630, #30340, #39211, #57226 ),
 .UNSPECIFIED., .F., .F.,
 ( 4, 4 ),
 ( 0.000000000000000000, 1.000000000000000000 ),
 .UNSPECIFIED. ) ;
#5568 = CARTESIAN_POINT ( 'NONE',  ( 9.767191983224998708, -79.64087503069099228, 0.05162932631433000269 ) ) ;
#5569 = ORIENTED_EDGE ( 'NONE', *, *, #2704, .T. ) ;
#5570 = CARTESIAN_POINT ( 'NONE',  ( 12.78015286808999917, -54.49674784847999831, 1.806262579044999983 ) ) ;
#5571 = FACE_OUTER_BOUND ( 'NONE', #42476, .T. ) ;
#5572 = CARTESIAN_POINT ( 'NONE',  ( -12.54715528150999937, -24.53180535391000205, -1.292252957172000061 ) ) ;
#5573 = CARTESIAN_POINT ( 'NONE',  ( -7.591316436381999821, -77.18132694988500475, -5.703451837412999659 ) ) ;
#5574 = PLANE ( 'NONE',  #42337 ) ;
#5575 = CARTESIAN_POINT ( 'NONE',  ( -0.7905733931407377124, -80.17088946056077248, -0.9685879666675529798 ) ) ;
#5576 = CARTESIAN_POINT ( 'NONE',  ( -7.648026766753000416, -60.05000000550000294, 10.12290050090999927 ) ) ;
#5577 = CARTESIAN_POINT ( 'NONE',  ( -1.276771495430000038E-14, -69.50420297070000686, 0.000000000000000000 ) ) ;
#5578 = CARTESIAN_POINT ( 'NONE',  ( -9.160649592606999292, -77.23931109735399048, 3.828331730729000348 ) ) ;
#5579 = CARTESIAN_POINT ( 'NONE',  ( 1.343421608112092658, -78.06192807433161818, -0.6881263894564929595 ) ) ;
#5580 = CARTESIAN_POINT ( 'NONE',  ( 8.485281374238999419, -23.25000000000000000, -8.485281374238999419 ) ) ;
#5581 = ORIENTED_EDGE ( 'NONE', *, *, #5283, .T. ) ;
#5582 = CARTESIAN_POINT ( 'NONE',  ( 10.69843650790000034, -76.30851016852000157, 6.089250768039999429 ) ) ;
#5583 = CARTESIAN_POINT ( 'NONE',  ( -2.692194317453766139, -1.904912773971035422, -2.265922085054583146 ) ) ;
#5584 = TOROIDAL_SURFACE ( 'NONE', #17842, 13.50000000000000000, 0.5000000000000000000 ) ;
#5585 = CARTESIAN_POINT ( 'NONE',  ( 0.000000000000000000, -5.000000000000000000, 0.000000000000000000 ) ) ;
#5586 = CARTESIAN_POINT ( 'NONE',  ( -10.61911868076999887, -78.55902054102001841, -6.134606423928000041 ) ) ;
#5587 = CARTESIAN_POINT ( 'NONE',  ( 4.297951556683999641, -76.71955760450698847, -11.50435740523999861 ) ) ;
#5588 = LINE ( 'NONE', #9454, #38341 ) ;
#5589 = CARTESIAN_POINT ( 'NONE',  ( -0.6622892437428000711, -79.93666419164598835, 11.13790800686000004 ) ) ;
#5590 = CARTESIAN_POINT ( 'NONE',  ( 3.249343497640856615, -2.845515713985523831, -0.2278308301013699799 ) ) ;
#5591 = CARTESIAN_POINT ( 'NONE',  ( 10.49839420453927197, -77.34045593712866662, 5.848571948716326574 ) ) ;
#5592 = CARTESIAN_POINT ( 'NONE',  ( 6.085790774524467928, -78.42088135606610422, -9.367230124943132452 ) ) ;
#5593 = ORIENTED_EDGE ( 'NONE', *, *, #23115, .T. ) ;
#5595 = B_SPLINE_CURVE_WITH_KNOTS ( 'NONE', 3,
 ( #28308, #41910, #46652, #36886, #37180, #54898, #14449, #1483 ),
 .UNSPECIFIED., .F., .F.,
 ( 4, 2, 2, 4 ),
 ( 0.000000000000000000, 0.5000000000000009992, 0.7500000000000004441, 1.000000000000000000 ),
 .UNSPECIFIED. ) ;
#5594 = CARTESIAN_POINT ( 'NONE',  ( 0.4072933538588000002, -82.16933951002999947, -1.288442219433000080 ) ) ;
#5596 = CARTESIAN_POINT ( 'NONE',  ( -9.395951288910000088, -77.37666898275598726, 1.963411011382999893 ) ) ;
#5597 = CARTESIAN_POINT ( 'NONE',  ( 7.000000000000000000, -81.19999999999998863, 0.000000000000000000 ) ) ;
#5598 = CIRCLE ( 'NONE', #48969, 1.199999999999999956 ) ;
#5599 = LINE ( 'NONE', #23610, #50349 ) ;
#5600 = CARTESIAN_POINT ( 'NONE',  ( 2.151784307624999837, -2.466290364169000604, -3.217165252942999931 ) ) ;
#5601 = AXIS2_PLACEMENT_3D ( 'NONE', #36146, #40871, #4270 ) ;
#5602 = CARTESIAN_POINT ( 'NONE',  ( 9.201871282504999527, -77.81471382358499511, 7.779546039068999441 ) ) ;
#5603 = CARTESIAN_POINT ( 'NONE',  ( -9.612747958823000261, -77.20206109394898419, 0.5898851805584000019 ) ) ;
#5604 = ADVANCED_FACE ( 'NONE', ( #33460 ), #2669, .F. ) ;
#5605 = CARTESIAN_POINT ( 'NONE',  ( 5.917544427059681311, -76.03248552931820825, 10.15932382542081669 ) ) ;
#5606 = B_SPLINE_CURVE_WITH_KNOTS ( 'NONE', 3,
 ( #32112, #51027, #14688, #28559, #54284, #50153, #14400, #6133 ),
 .UNSPECIFIED., .F., .F.,
 ( 4, 2, 2, 4 ),
 ( 0.000000000000000000, 0.4999999999999977796, 0.7499999999999988898, 1.000000000000000000 ),
 .UNSPECIFIED. ) ;
#5607 = CARTESIAN_POINT ( 'NONE',  ( 2.253937565478000060, -78.66813999416500280, -10.68151722998999986 ) ) ;
#5608 = CARTESIAN_POINT ( 'NONE',  ( -0.5084075448453283519, -85.83735717367099483, 4.088733110535459403 ) ) ;
#5609 = ORIENTED_EDGE ( 'NONE', *, *, #876, .F. ) ;
#5610 = DIRECTION ( 'NONE',  ( 0.000000000000000000, 0.000000000000000000, -1.000000000000000000 ) ) ;
#5611 = ADVANCED_FACE ( 'NONE', ( #43711 ), #57682, .F. ) ;
#5612 = CARTESIAN_POINT ( 'NONE',  ( -5.684974983678790394, -78.02723969034931883, 7.397314429064029362 ) ) ;
#5613 = CARTESIAN_POINT ( 'NONE',  ( 12.56594317991999965, -60.04999999381999487, 1.750000000001000089 ) ) ;
#5614 = CARTESIAN_POINT ( 'NONE',  ( -6.405050160242000246, -78.91504066244898752, 8.912875463421000788 ) ) ;
#5615 = CARTESIAN_POINT ( 'NONE',  ( 2.879226727952061360, -79.24583333333333712, -10.71369944335147828 ) ) ;
#5616 = CARTESIAN_POINT ( 'NONE',  ( -11.46357413472999909, -76.34071485469600304, 4.994040814626000468 ) ) ;
#5617 = CARTESIAN_POINT ( 'NONE',  ( 0.000000000000000000, -63.73717104351998586, 0.000000000000000000 ) ) ;
#5618 = CARTESIAN_POINT ( 'NONE',  ( 7.645391692608000334, -18.78469634161999835, -10.18949678827999961 ) ) ;
#5619 = CARTESIAN_POINT ( 'NONE',  ( 9.019406119853890402, -17.00707871055414344, 8.666949039025178436 ) ) ;
#5620 = VERTEX_POINT ( 'NONE', #48717 ) ;
#5621 = CARTESIAN_POINT ( 'NONE',  ( -1.463640999337999959, -78.32317658674999450, -10.83301059047000159 ) ) ;
#5622 = CARTESIAN_POINT ( 'NONE',  ( -4.849178099734126057, -77.41866321790520544, 7.910227586308292480 ) ) ;
#5623 = CARTESIAN_POINT ( 'NONE',  ( 10.49303003107499421, -79.76163707075535569, -5.474388617415005598 ) ) ;
#5624 = CARTESIAN_POINT ( 'NONE',  ( 3.914500761937000028, -78.48547955770028750, -4.793880828366022505E-16 ) ) ;
#5625 = CARTESIAN_POINT ( 'NONE',  ( 7.723332765951321122, -77.77272290370588337, 9.278744632980441054 ) ) ;
#5626 = EDGE_CURVE ( 'NONE', #54609, #44143, #16839, .T. ) ;
#5627 = CARTESIAN_POINT ( 'NONE',  ( 12.54435915808562108, -60.32412882177209212, 1.733925320397567305 ) ) ;
#5628 = DIRECTION ( 'NONE',  ( 0.000000000000000000, 1.000000000000000000, 0.000000000000000000 ) ) ;
#5629 = DIRECTION ( 'NONE',  ( 1.140590214241074934E-08, -0.7071067811865474617, -0.7071067811865474617 ) ) ;
#5630 = CARTESIAN_POINT ( 'NONE',  ( -1.266141431829999942, -77.60019095522000043, -0.3277948212408000050 ) ) ;
#5631 =( BOUNDED_SURFACE ( )  B_SPLINE_SURFACE ( 3, 3, ( 
 ( #43413, #56706, #20970, #2971, #52563, #20402, #16263 ),
 ( #43709, #11832, #34241, #46998, #33384, #16548, #52277 ),
 ( #24538, #4421, #21548, #22421, #44867, #35697, #17712 ),
 ( #40433, #24, #21830, #35390, #9147, #35103, #54020 ),
 ( #13560, #18004, #35995, #30677, #22122, #12402, #57850 ),
 ( #31552, #16838, #53726, #12685, #25968, #26261, #4719 ),
 ( #53137, #17408, #27131, #49599, #45169, #22718, #8848 ),
 ( #39552, #40731, #34821, #58145, #52849, #53421, #30393 ),
 ( #43994, #48429, #7971, #17118, #3545, #57557, #48716 ),
 ( #8261, #44274, #3831, #39836, #12965, #30964, #49001 ),
 ( #13265, #8549, #26540, #31256, #44567, #49297, #4121 ),
 ( #26839, #40132, #51063, #32719, #9728, #23880, #46054 ),
 ( #322, #37167, #31852, #41602, #55180, #25195, #42929 ),
 ( #56501, #48508, #3623, #20771, #21629, #2484, #38772 ),
 ( #47952, #43798, #38483, #56790, #43213, #21057, #16056 ) ),
 .UNSPECIFIED., .F., .F., .T. ) 
 B_SPLINE_SURFACE_WITH_KNOTS ( ( 4, 1, 1, 1, 1, 1, 1, 1, 1, 1, 1, 1, 4 ),
 ( 4, 3, 4 ),
 ( 0.009836358961777999163, 0.09153385889397000486, 0.1732268882812000033, 0.2549245844128000260, 0.3366128623372000028, 0.4183102317861999708, 0.5000049915032999115, 0.5816997502458999270, 0.6633970872647999562, 0.7450853589770999319, 0.8267830756728000718, 0.9084760833474000430, 0.9901736252444659492 ),
 ( 0.000000000000000000, 0.5000000000000000000, 1.000000000000000000 ),
 .UNSPECIFIED. ) 
 GEOMETRIC_REPRESENTATION_ITEM ( )  RATIONAL_B_SPLINE_SURFACE ( (
 ( 1.000000000000000000, 0.8025111637939407183, 0.8025111637939407183, 1.000000000000000000, 0.8025111637939407183, 0.8025111637939407183, 1.000000000000000000),
 ( 1.000000000000000000, 0.8025111637939407183, 0.8025111637939407183, 1.000000000000000000, 0.8025111637939407183, 0.8025111637939407183, 1.000000000000000000),
 ( 1.000000000000000000, 0.8025111637939407183, 0.8025111637939407183, 1.000000000000000000, 0.8025111637939407183, 0.8025111637939407183, 1.000000000000000000),
 ( 1.000000000000000000, 0.8025111637939407183, 0.8025111637939407183, 1.000000000000000000, 0.8025111637939407183, 0.8025111637939407183, 1.000000000000000000),
 ( 1.000000000000000000, 0.8025111637939407183, 0.8025111637939407183, 1.000000000000000000, 0.8025111637939407183, 0.8025111637939407183, 1.000000000000000000),
 ( 1.000000000000000000, 0.8025111637939407183, 0.8025111637939407183, 1.000000000000000000, 0.8025111637939407183, 0.8025111637939407183, 1.000000000000000000),
 ( 1.000000000000000000, 0.8025111637939407183, 0.8025111637939407183, 1.000000000000000000, 0.8025111637939407183, 0.8025111637939407183, 1.000000000000000000),
 ( 1.000000000000000000, 0.8025111637939407183, 0.8025111637939407183, 1.000000000000000000, 0.8025111637939407183, 0.8025111637939407183, 1.000000000000000000),
 ( 1.000000000000000000, 0.8025111637939407183, 0.8025111637939407183, 1.000000000000000000, 0.8025111637939407183, 0.8025111637939407183, 1.000000000000000000),
 ( 1.000000000000000000, 0.8025111637939407183, 0.8025111637939407183, 1.000000000000000000, 0.8025111637939407183, 0.8025111637939407183, 1.000000000000000000),
 ( 1.000000000000000000, 0.8025111637939407183, 0.8025111637939407183, 1.000000000000000000, 0.8025111637939407183, 0.8025111637939407183, 1.000000000000000000),
 ( 1.000000000000000000, 0.8025111637939407183, 0.8025111637939407183, 1.000000000000000000, 0.8025111637939407183, 0.8025111637939407183, 1.000000000000000000),
 ( 1.000000000000000000, 0.8025111637939407183, 0.8025111637939407183, 1.000000000000000000, 0.8025111637939407183, 0.8025111637939407183, 1.000000000000000000),
 ( 1.000000000000000000, 0.8025111637939407183, 0.8025111637939407183, 1.000000000000000000, 0.8025111637939407183, 0.8025111637939407183, 1.000000000000000000),
 ( 1.000000000000000000, 0.8025111637939407183, 0.8025111637939407183, 1.000000000000000000, 0.8025111637939407183, 0.8025111637939407183, 1.000000000000000000) ) ) 
 REPRESENTATION_ITEM ( '' )  SURFACE ( )  );
#5632 = CARTESIAN_POINT ( 'NONE',  ( 9.250000000000000000, -79.74999999999998579, 1.907449677260999760E-14 ) ) ;
#5633 = DIRECTION ( 'NONE',  ( -0.7071067811865475727, 0.000000000000000000, 0.7071067811865475727 ) ) ;
#5634 = EDGE_CURVE ( 'NONE', #8440, #38434, #38491, .T. ) ;
#5635 = CARTESIAN_POINT ( 'NONE',  ( -12.50386483995777809, -61.58505343581191482, 0.8574420495993835267 ) ) ;
#5636 = EDGE_LOOP ( 'NONE', ( #30724, #42187, #30547, #46852 ) ) ;
#5637 = EDGE_LOOP ( 'NONE', ( #14200, #52764, #4231, #5593 ) ) ;
#5638 = CARTESIAN_POINT ( 'NONE',  ( -2.370458031814262068, -77.79499999999998749, 9.242975026304343089 ) ) ;
#5639 = CARTESIAN_POINT ( 'NONE',  ( 8.425244479088499716, -78.79682508674252972, -6.676653465681916977 ) ) ;
#5640 = CIRCLE ( 'NONE', #13173, 9.599999999999999645 ) ;
#5641 = EDGE_LOOP ( 'NONE', ( #19344, #6143, #56917, #53309 ) ) ;
#5642 = CARTESIAN_POINT ( 'NONE',  ( 0.000000000000000000, -74.64999999999999147, 0.000000000000000000 ) ) ;
#5643 = CARTESIAN_POINT ( 'NONE',  ( 2.297158073433503755, -83.74895834637031555, -2.566498985648576703 ) ) ;
#5644 = AXIS2_PLACEMENT_3D ( 'NONE', #10167, #46196, #5721 ) ;
#5645 = CARTESIAN_POINT ( 'NONE',  ( 0.3926218265389159745, -80.25416666666666288, 1.460959015002474493 ) ) ;
#5646 = CARTESIAN_POINT ( 'NONE',  ( 7.657745562928999661, -60.46920625093000012, 9.966193613345000202 ) ) ;
#5647 = CARTESIAN_POINT ( 'NONE',  ( -2.472186688656227371, -77.15814173843004653, -11.94662027503587076 ) ) ;
#5648 = CARTESIAN_POINT ( 'NONE',  ( -1.360231837983352676, -77.66584863236742819, -11.90251068871223339 ) ) ;
#5649 = CARTESIAN_POINT ( 'NONE',  ( -11.19989528650999944, -78.76172757993099083, 0.6168112860373000661 ) ) ;
#5650 = B_SPLINE_CURVE_WITH_KNOTS ( 'NONE', 3,
 ( #13598, #18632, #50511, #934, #13894, #31888 ),
 .UNSPECIFIED., .F., .F.,
 ( 4, 2, 4 ),
 ( 0.000000000000000000, 0.5000000000000001110, 1.000000000000000000 ),
 .UNSPECIFIED. ) ;
#5651 = ORIENTED_EDGE ( 'NONE', *, *, #51191, .F. ) ;
#5652 = CARTESIAN_POINT ( 'NONE',  ( 0.000000000000000000, -39.30476017083000073, 0.000000000000000000 ) ) ;
#5653 = ORIENTED_EDGE ( 'NONE', *, *, #41879, .F. ) ;
#5654 = CARTESIAN_POINT ( 'NONE',  ( 8.217637274874787678, -77.38807705323522157, 4.246385049674642254 ) ) ;
#5655 = CARTESIAN_POINT ( 'NONE',  ( -1.235017835984000056, -79.23795388112999660, 0.06195353447049999768 ) ) ;
#5656 = CARTESIAN_POINT ( 'NONE',  ( 0.9218200799623694763, -77.82291666666667140, 1.199500263597272465 ) ) ;
#5657 = CARTESIAN_POINT ( 'NONE',  ( -7.954951288349001004, -23.25000000000000000, -9.722718241315000398 ) ) ;
#5658 = CARTESIAN_POINT ( 'NONE',  ( -1.570796326794884790, -77.51458333333334849, -12.00000000000000355 ) ) ;
#5659 = CARTESIAN_POINT ( 'NONE',  ( 1.063278045107967973, -2.151263346416249167, -3.097506788382764498 ) ) ;
#5660 = CARTESIAN_POINT ( 'NONE',  ( -1.560595261880000084, -77.68827307234998614, 0.4619550309703999713 ) ) ;
#5661 = B_SPLINE_CURVE_WITH_KNOTS ( 'NONE', 3,
 ( #1154, #51030, #10283, #2025, #42457, #19140, #37134, #10579, #46610, #55145, #14691, #6136, #32693, #28264, #24143 ),
 .UNSPECIFIED., .F., .F.,
 ( 4, 1, 1, 1, 1, 1, 1, 1, 1, 1, 1, 1, 4 ),
 ( 0.000000000000000000, 0.08333615748455000527, 0.1666676910119000155, 0.2500040280097000078, 0.3333307305850000124, 0.4166666802908000067, 0.5000000000075000006, 0.5833333207182000990, 0.6666693035046000748, 0.7499960124165999664, 0.8333323284379000606, 0.9166638841133999405, 1.000000000000000000 ),
 .UNSPECIFIED. ) ;
#5662 = CARTESIAN_POINT ( 'NONE',  ( -4.094444587552000137, -78.75880496681158149, -0.8031955627257999497 ) ) ;
#5663 = CARTESIAN_POINT ( 'NONE',  ( 9.203868716350999790, -79.72463564708098716, 5.914103205931999341 ) ) ;
#5664 = CARTESIAN_POINT ( 'NONE',  ( 12.70228857843095227, -61.62190589586192857, 1.213561371183882187 ) ) ;
#5665 = CARTESIAN_POINT ( 'NONE',  ( 9.500517569907307447, -79.06045223105810749, 1.242907163946308069 ) ) ;
#5666 = CARTESIAN_POINT ( 'NONE',  ( 0.1846283042134000130, -85.50854634175698266, 3.751963089900000270 ) ) ;
#5667 = AXIS2_PLACEMENT_3D ( 'NONE', #4193, #57917, #35464 ) ;
#5668 = ORIENTED_EDGE ( 'NONE', *, *, #16533, .T. ) ;
#5669 = CARTESIAN_POINT ( 'NONE',  ( 0.6999999999999999556, -21.00000000000000000, -11.90000000000000036 ) ) ;
#5670 = CARTESIAN_POINT ( 'NONE',  ( 8.411888842866000360, -76.58712216313399779, 8.005707060120000662 ) ) ;
#5671 = CARTESIAN_POINT ( 'NONE',  ( -0.1701304685956719354, -77.97633532982500526, 10.74867621670826878 ) ) ;
#5672 = CARTESIAN_POINT ( 'NONE',  ( 10.46934363224000109, -77.42428757496500680, 5.823135730235999397 ) ) ;
#5673 = CARTESIAN_POINT ( 'NONE',  ( 0.4254240051736068451, -3.364583333333333481, 3.250000000000001776 ) ) ;
#5674 = LINE ( 'NONE', #36386, #44044 ) ;
#5675 = CARTESIAN_POINT ( 'NONE',  ( -1.344596514747811611, -3.156225089547542328, 3.253962609497633718 ) ) ;
#5676 = CARTESIAN_POINT ( 'NONE',  ( 9.574567190152320606, -80.88771002875691352, 4.887542694105030172 ) ) ;
#5677 = CARTESIAN_POINT ( 'NONE',  ( 4.061470846528000500, -78.23968660667100039, -8.492093326754000415 ) ) ;
#5679 = EDGE_CURVE ( 'NONE', #32058, #54228, #41317, .T. ) ;
#5678 = CARTESIAN_POINT ( 'NONE',  ( -6.389969351467987835, -85.79678895079197787, -5.255310806705900006 ) ) ;
#5680 = CARTESIAN_POINT ( 'NONE',  ( -9.244881144060999034, -76.93831224807900071, -6.227904302768000555 ) ) ;
#5681 = CARTESIAN_POINT ( 'NONE',  ( 2.083499196047589042, -0.8606770703554429414, -2.709727116747193687 ) ) ;
#5682 = CARTESIAN_POINT ( 'NONE',  ( 7.291278940103000039, -80.77636526708458575, 8.270696028970998981 ) ) ;
#5683 = ORIENTED_EDGE ( 'NONE', *, *, #5166, .T. ) ;
#5684 = B_SPLINE_CURVE_WITH_KNOTS ( 'NONE', 3,
 ( #28235, #46286, #35116, #553, #45405, #45106, #53150, #36230, #12697, #36812, #14087, #30692, #9080, #4659, #13786, #31786, #4946, #49830 ),
 .UNSPECIFIED., .F., .F.,
 ( 4, 2, 2, 2, 2, 2, 2, 2, 4 ),
 ( 0.000000000000000000, 0.1250000000000000833, 0.2500000000000001665, 0.3750000000000001110, 0.5000000000000001110, 0.6250000000000001110, 0.7500000000000000000, 0.8750000000000000000, 1.000000000000000000 ),
 .UNSPECIFIED. ) ;
#5685 = CARTESIAN_POINT ( 'NONE',  ( 9.426477049435000310, -77.39042403538302040, -1.139727483088999849 ) ) ;
#5686 = CARTESIAN_POINT ( 'NONE',  ( 2.787169241930258057, -80.45429007894077245, 10.40602097193850817 ) ) ;
#5687 = CARTESIAN_POINT ( 'NONE',  ( 11.01642476345000077, -76.96338369438498717, 2.111041454437999842 ) ) ;
#5688 = CARTESIAN_POINT ( 'NONE',  ( -9.505686244346000180, -79.26788661775799483, 5.486888517706000279 ) ) ;
#5689 = CARTESIAN_POINT ( 'NONE',  ( 7.659225027811000786, -23.68266641665999828, -9.963489011784998794 ) ) ;
#5690 = CARTESIAN_POINT ( 'NONE',  ( 0.6616348183234056490, -82.78541665061636934, 3.958011967683783716 ) ) ;
#5691 = CARTESIAN_POINT ( 'NONE',  ( -0.2428027759546764197, -78.62319558955745435, -10.77942311248712315 ) ) ;
#5692 = CARTESIAN_POINT ( 'NONE',  ( -7.764220096216667422, -54.54399029303478841, -10.21028322253899923 ) ) ;
#5693 = COLOUR_RGB ( '', 0.08235294, 0.09019608, 0.10196078) ;
#5694 = CARTESIAN_POINT ( 'NONE',  ( -0.8075922533534999337, -83.51594503318798957, -4.093636164257000054 ) ) ;
#5695 = CARTESIAN_POINT ( 'NONE',  ( 0.000000000000000000, -75.15999999999999659, 0.000000000000000000 ) ) ;
#5696 = ADVANCED_FACE ( 'NONE', ( #38261 ), #12463, .F. ) ;
#5697 = CARTESIAN_POINT ( 'NONE',  ( 10.36221646771999971, -55.57876216348000042, -7.631895822728999690 ) ) ;
#5698 = CARTESIAN_POINT ( 'NONE',  ( -12.76303204513999923, -55.53514852210999919, 1.980584515753000208 ) ) ;
#5699 = CARTESIAN_POINT ( 'NONE',  ( -1.529754383668999962, -81.24352304346000153, -0.6588408878327000062 ) ) ;
#5700 = CARTESIAN_POINT ( 'NONE',  ( -0.5850755440913000260, -78.10843573086999925, -1.183371315974999893 ) ) ;
#5701 = CARTESIAN_POINT ( 'NONE',  ( 1.500000000000000000, -78.75000000000000000, 0.000000000000000000 ) ) ;
#5702 = CARTESIAN_POINT ( 'NONE',  ( 1.518408311387865917, -81.48882957865839671, -0.2150362242269064084 ) ) ;
#5703 = CARTESIAN_POINT ( 'NONE',  ( 0.1237567301189053115, -83.21780190041201308, 1.506540253472085755 ) ) ;
#5704 = CARTESIAN_POINT ( 'NONE',  ( -7.598611126932110160, -80.16299070835863461, -7.603773876929224684 ) ) ;
#5705 = CARTESIAN_POINT ( 'NONE',  ( 2.486604901413172364, -77.94583333333333997, -9.252740428348998236 ) ) ;
#5706 = CARTESIAN_POINT ( 'NONE',  ( -1.218468010184407202, -81.07986474255089604, 0.3279021448883003842 ) ) ;
#5707 = ADVANCED_FACE ( 'NONE', ( #38553 ), #18061, .F. ) ;
#5708 = EDGE_LOOP ( 'NONE', ( #19589, #23469, #13835 ) ) ;
#5709 = CARTESIAN_POINT ( 'NONE',  ( 13.97864847851000114, -45.76668425569999954, 0.0001086640162475999876 ) ) ;
#5710 =( LENGTH_UNIT ( ) NAMED_UNIT ( * ) SI_UNIT ( .MILLI., .METRE. ) );
#5711 = ADVANCED_FACE ( 'NONE', ( #4877 ), #49761, .F. ) ;
#5712 = CARTESIAN_POINT ( 'NONE',  ( 9.221778727104000595, -79.66263030682299018, -6.054794091447999627 ) ) ;
#5713 = CARTESIAN_POINT ( 'NONE',  ( 0.000000000000000000, 4.040000000000000036, 0.000000000000000000 ) ) ;
#5714 = ORIENTED_EDGE ( 'NONE', *, *, #4110, .F. ) ;
#5715 = ORIENTED_EDGE ( 'NONE', *, *, #167, .T. ) ;
#5716 = CARTESIAN_POINT ( 'NONE',  ( 1.002739805183000099, -81.91516772237299904, 1.002283400281000159 ) ) ;
#5717 = B_SPLINE_CURVE_WITH_KNOTS ( 'NONE', 3,
 ( #56424, #11557, #42558, #56135, #15974, #33966 ),
 .UNSPECIFIED., .F., .F.,
 ( 4, 2, 4 ),
 ( 0.000000000000000000, 0.5000000000000000000, 1.000000000000000000 ),
 .UNSPECIFIED. ) ;
#5718 = EDGE_LOOP ( 'NONE', ( #56477, #25652, #27852, #49998 ) ) ;
#5719 = EDGE_LOOP ( 'NONE', ( #47994, #31456, #30315 ) ) ;
#5720 = CARTESIAN_POINT ( 'NONE',  ( -0.5045596072232000351, -16.86471086961999788, 12.66210649709999991 ) ) ;
#5721 = DIRECTION ( 'NONE',  ( -0.9999380042107527400, 0.000000000000000000, 0.01113497799803945566 ) ) ;
#5722 = PRODUCT_CONTEXT ( 'NONE', #14927, 'mechanical' ) ;
#5723 = CARTESIAN_POINT ( 'NONE',  ( -1.432607641878103744, -80.47291665695050256, -3.131646614799266537 ) ) ;
#5724 = CARTESIAN_POINT ( 'NONE',  ( 3.903619169069028949, -78.25971142198206110, -8.387417762067762794 ) ) ;
#5725 = CARTESIAN_POINT ( 'NONE',  ( 5.413904038987179312, -78.16666666666662877, -9.393203674808262349 ) ) ;
#5726 = ORIENTED_EDGE ( 'NONE', *, *, #52089, .F. ) ;
#5727 = ORIENTED_EDGE ( 'NONE', *, *, #33780, .T. ) ;
#5728 = CARTESIAN_POINT ( 'NONE',  ( -8.325424899317864558, -77.56401563986393910, 4.046370920615864009 ) ) ;
#5729 = AXIS2_PLACEMENT_3D ( 'NONE', #44908, #46091, #36039 ) ;
#5730 = CARTESIAN_POINT ( 'NONE',  ( 0.3704480450335023711, -77.02746413819750160, -12.03686759590603650 ) ) ;
#5731 = CARTESIAN_POINT ( 'NONE',  ( 1.500000000000000000, -79.26041666666669983, 0.1963495408493652339 ) ) ;
#5732 = ADVANCED_FACE ( 'NONE', ( #53586, #40883 ), #40596, .F. ) ;
#5733 = CARTESIAN_POINT ( 'NONE',  ( -1.308715794653438680, -61.54404499166313514, -12.70256747361121796 ) ) ;
#5734 = CIRCLE ( 'NONE', #22714, 1.199999999999999956 ) ;
#5735 = CARTESIAN_POINT ( 'NONE',  ( -9.157500079073999544, -78.74301087542899324, 3.211059275314999795 ) ) ;
#5736 = DIRECTION ( 'NONE',  ( -1.000000000000000000, 0.000000000000000000, 0.000000000000000000 ) ) ;
#5737 = CARTESIAN_POINT ( 'NONE',  ( -10.18589226631999978, -23.28917723430000208, 7.641012305222999679 ) ) ;
#5738 = CARTESIAN_POINT ( 'NONE',  ( -10.00716890277074356, -77.34696047196747770, -6.699252482692385158 ) ) ;
#5739 = CARTESIAN_POINT ( 'NONE',  ( 0.7658660592953000501, -79.40707368812999789, 1.113292320107999833 ) ) ;
#5740 = CARTESIAN_POINT ( 'NONE',  ( -8.539484132404522754, -77.01652175453601501, 3.808411293863636971 ) ) ;
#5741 = CARTESIAN_POINT ( 'NONE',  ( -9.160327239603146765, -76.64595974771152953, 7.362753168639923018 ) ) ;
#5742 = CARTESIAN_POINT ( 'NONE',  ( 3.934691878955999922, -81.01844020063299467, 1.388622521904000040 ) ) ;
#5743 = CARTESIAN_POINT ( 'NONE',  ( 7.551392188974999975, -80.08153398617218954, 8.117862728809001283 ) ) ;
#5744 = CARTESIAN_POINT ( 'NONE',  ( 1.570796326794857478, -76.66458333333332575, 12.00000000000000533 ) ) ;
#5745 = CARTESIAN_POINT ( 'NONE',  ( 1.407187316041068392, -76.73555785001855156, -10.75055512959062121 ) ) ;
#5746 = CARTESIAN_POINT ( 'NONE',  ( -0.05200678273669999407, -79.84732046129099103, 3.547090062506000230 ) ) ;
#5748 = CARTESIAN_POINT ( 'NONE',  ( 1.302799686710000016, -77.98903190391820317, 0.2851120931344000020 ) ) ;
#5747 = LINE ( 'NONE', #18753, #48561 ) ;
#5749 = CARTESIAN_POINT ( 'NONE',  ( -9.250000000000000000, -79.59999999999999432, 0.000000000000000000 ) ) ;
#5750 = CARTESIAN_POINT ( 'NONE',  ( 9.708203932494999577, -79.25000000000000000, 7.053423027515000499 ) ) ;
#5751 = CARTESIAN_POINT ( 'NONE',  ( 1.432628882339999965, -2.473043513114999925, -3.526139092948999743 ) ) ;
#5752 = CARTESIAN_POINT ( 'NONE',  ( 2.854661674668000058E-14, -82.00000000000000000, 0.000000000000000000 ) ) ;
#5753 = VERTEX_POINT ( 'NONE', #41464 ) ;
#5754 = CARTESIAN_POINT ( 'NONE',  ( -11.74999999999999645, -78.80833333333335133, -1.230457122656147373 ) ) ;
#5755 = CARTESIAN_POINT ( 'NONE',  ( -0.5245219981418175470, -18.54839576653561650, -10.98753021428655963 ) ) ;
#5756 = CARTESIAN_POINT ( 'NONE',  ( 5.539808784079903070, -79.03333333333333144, 9.611650271896831299 ) ) ;
#5757 = VECTOR ( 'NONE', #19083, 1000.000000000000114 ) ;
#5758 = CARTESIAN_POINT ( 'NONE',  ( -3.587367123708000261, -79.73416563881599473, 9.067562258818998799 ) ) ;
#5759 = CARTESIAN_POINT ( 'NONE',  ( 1.750000000000000000, -20.25022860793999868, -12.65375411744000012 ) ) ;
#5760 = CARTESIAN_POINT ( 'NONE',  ( -2.508531238560355092, -79.49373965571280110, 10.45321017623470716 ) ) ;
#5761 = DIRECTION ( 'NONE',  ( 0.000000000000000000, 1.000000000000000000, 0.000000000000000000 ) ) ;
#5762 = EDGE_CURVE ( 'NONE', #56208, #800, #6321, .T. ) ;
#5763 = FACE_OUTER_BOUND ( 'NONE', #43493, .T. ) ;
#5764 = CARTESIAN_POINT ( 'NONE',  ( 11.06229936814999881, -77.50388255425598061, 1.513518412900999977 ) ) ;
#5765 = ADVANCED_FACE ( 'NONE', ( #37611 ), #28477, .T. ) ;
#5766 = CARTESIAN_POINT ( 'NONE',  ( -0.3614649557311000461, -81.95840137440799822, -1.462273585377000140 ) ) ;
#5767 = FACE_OUTER_BOUND ( 'NONE', #25602, .T. ) ;
#5768 = AXIS2_PLACEMENT_3D ( 'NONE', #27204, #30257, #35258 ) ;
#5769 = CARTESIAN_POINT ( 'NONE',  ( 4.409055568808000203, -77.85702278427999090, 8.316935944130001701 ) ) ;
#5771 = FACE_OUTER_BOUND ( 'NONE', #47647, .T. ) ;
#5770 = CARTESIAN_POINT ( 'NONE',  ( -2.532643299141000170, -84.18579177382198964, 3.048230288908000407 ) ) ;
#5772 = DIRECTION ( 'NONE',  ( 0.000000000000000000, 1.000000000000000000, 4.440892098500000122E-14 ) ) ;
#5773 = CARTESIAN_POINT ( 'NONE',  ( -1.750000000001000089, -18.75000001325000198, -12.56594318051000059 ) ) ;
#5774 = CARTESIAN_POINT ( 'NONE',  ( -0.6144861720749000833, -80.74167289250799229, -1.073086222052999972 ) ) ;
#5775 = CARTESIAN_POINT ( 'NONE',  ( -9.722718241315000398, -18.75000000000000000, 7.954951288349001004 ) ) ;
#5776 = CARTESIAN_POINT ( 'NONE',  ( -5.838193839761721016, -77.32708333333333428, 7.596835002782687418 ) ) ;
#5777 = CONICAL_SURFACE ( 'NONE', #38770, 10.09999999997999964, 0.7853981633972997312 ) ;
#5778 = CARTESIAN_POINT ( 'NONE',  ( 3.999999999999816147, -78.72610001270986402, 7.999999999999665157 ) ) ;
#5779 = EDGE_LOOP ( 'NONE', ( #25005, #32198, #38244, #35085, #57341, #43560 ) ) ;
#5780 = ORIENTED_EDGE ( 'NONE', *, *, #30745, .T. ) ;
#5781 = CARTESIAN_POINT ( 'NONE',  ( -5.092641036025000290, -79.54368063314299775, 10.89826376711000044 ) ) ;
#5782 = DIRECTION ( 'NONE',  ( 1.000000000000000000, 0.000000000000000000, 0.000000000000000000 ) ) ;
#5783 = EDGE_CURVE ( 'NONE', #8187, #26499, #56773, .T. ) ;
#5784 = DIRECTION ( 'NONE',  ( 0.000000000000000000, 1.000000000000000000, 0.000000000000000000 ) ) ;
#5785 = VERTEX_POINT ( 'NONE', #55334 ) ;
#5786 = CARTESIAN_POINT ( 'NONE',  ( -8.852102014390000662, -78.06490627187800158, 8.004735621704000437 ) ) ;
#5787 = ORIENTED_EDGE ( 'NONE', *, *, #54972, .T. ) ;
#5788 = ORIENTED_EDGE ( 'NONE', *, *, #29018, .F. ) ;
#5789 = ORIENTED_EDGE ( 'NONE', *, *, #55973, .F. ) ;
#5790 = B_SPLINE_CURVE_WITH_KNOTS ( 'NONE', 3,
 ( #18494, #4917, #54515, #45368, #5487, #40637, #31160, #53931, #18785, #37065 ),
 .UNSPECIFIED., .F., .F.,
 ( 4, 2, 2, 2, 4 ),
 ( 0.000000000000000000, 0.2500000000000000000, 0.5000000000000000000, 0.7500000000000000000, 1.000000000000000000 ),
 .UNSPECIFIED. ) ;
#5791 = CARTESIAN_POINT ( 'NONE',  ( -1.757305424856000053, -79.93618638030199008, 3.081143863716000464 ) ) ;
#5792 = CARTESIAN_POINT ( 'NONE',  ( -10.50000000000000000, -73.00000000000001421, 0.000000000000000000 ) ) ;
#5793 = ORIENTED_EDGE ( 'NONE', *, *, #3738, .T. ) ;
#5794 = DIRECTION ( 'NONE',  ( 0.000000000000000000, -1.000000000000000000, 0.000000000000000000 ) ) ;
#5795 = CARTESIAN_POINT ( 'NONE',  ( -7.642147947524999374, -56.01514526721999943, 10.55910102243999837 ) ) ;
#5796 = ORIENTED_EDGE ( 'NONE', *, *, #40776, .T. ) ;
#5797 = DIRECTION ( 'NONE',  ( -1.000000000000000000, 0.000000000000000000, 0.000000000000000000 ) ) ;
#5798 = CARTESIAN_POINT ( 'NONE',  ( 4.746119756384775457, -77.51557182255893963, -8.464524489953728192 ) ) ;
#5799 = CARTESIAN_POINT ( 'NONE',  ( -9.760280716455657313, -79.79999999999999716, -6.845562419370476270 ) ) ;
#5800 = DIRECTION ( 'NONE',  ( -0.7071067811865475727, 0.000000000000000000, -0.7071067811865475727 ) ) ;
#5801 = CARTESIAN_POINT ( 'NONE',  ( -12.26179901070890566, -78.95175067907904065, -0.2371216807744343236 ) ) ;
#5802 = CARTESIAN_POINT ( 'NONE',  ( 6.983565664416999219, -78.43892452229077605, -6.737990796766999857 ) ) ;
#5803 = CARTESIAN_POINT ( 'NONE',  ( 5.380788203752000065, -76.10116233407198649, 9.804131929786001010 ) ) ;
#5804 = DIRECTION ( 'NONE',  ( 0.000000000000000000, -1.000000000000000000, 0.000000000000000000 ) ) ;
#5805 = CARTESIAN_POINT ( 'NONE',  ( -7.691893942725999800, -58.55453807205000061, -10.42272502862000039 ) ) ;
#5806 = CARTESIAN_POINT ( 'NONE',  ( 2.087132440259329424, -78.74332257418703307, -9.032315042655973514 ) ) ;
#5807 = CARTESIAN_POINT ( 'NONE',  ( -4.354206273205999622, -77.48393501420198959, 8.343719559825000687 ) ) ;
#5808 = CARTESIAN_POINT ( 'NONE',  ( 0.000000000000000000, -79.65000000003199432, 0.000000000000000000 ) ) ;
#5809 = CYLINDRICAL_SURFACE ( 'NONE', #31753, 1.250000000000000000 ) ;
#5810 = CARTESIAN_POINT ( 'NONE',  ( 0.6454797250853000490, -61.68806512111272156, -12.50471521371631312 ) ) ;
#5811 = CARTESIAN_POINT ( 'NONE',  ( -4.126007527045000067, -80.00092549782598894, 0.1859177100975999974 ) ) ;
#5812 = EDGE_CURVE ( 'NONE', #42334, #15713, #15477, .T. ) ;
#5813 = VECTOR ( 'NONE', #19084, 1000.000000000000000 ) ;
#5814 = CARTESIAN_POINT ( 'NONE',  ( 4.153738564337000838, -77.85351332859899287, -8.713191203520999295 ) ) ;
#5815 = CARTESIAN_POINT ( 'NONE',  ( -12.72558083409999874, -18.79866855842000106, 1.930284430576000076 ) ) ;
#5816 = CARTESIAN_POINT ( 'NONE',  ( 1.115776411654021860, -82.88725312741937046, 0.5639269211292178285 ) ) ;
#5817 = PLANE ( 'NONE',  #38665 ) ;
#5818 = CARTESIAN_POINT ( 'NONE',  ( 0.000000000000000000, -87.09999999999999432, 0.000000000000000000 ) ) ;
#5819 = CARTESIAN_POINT ( 'NONE',  ( 7.650805994261745901, -79.99999999999998579, 5.540479312588552752 ) ) ;
#5820 = FACE_OUTER_BOUND ( 'NONE', #57311, .T. ) ;
#5821 = FACE_OUTER_BOUND ( 'NONE', #35757, .T. ) ;
#5822 = CARTESIAN_POINT ( 'NONE',  ( -1.798336774608999988, -23.19644498052000259, -12.61277771566000006 ) ) ;
#5823 = DIRECTION ( 'NONE',  ( 0.000000000000000000, 0.000000000000000000, -1.000000000000000000 ) ) ;
#5824 = CARTESIAN_POINT ( 'NONE',  ( -1.898295385589999995, -2.623547659066999937, -2.923300871422000125 ) ) ;
#5825 = CARTESIAN_POINT ( 'NONE',  ( 12.54673765596000123, -24.82199238237999950, 0.9174244429638999110 ) ) ;
#5826 = CARTESIAN_POINT ( 'NONE',  ( -1.394284273676999808, -77.48935448679299043, -12.20048157021999913 ) ) ;
#5827 = DIRECTION ( 'NONE',  ( 0.000000000000000000, 0.000000000000000000, -1.000000000000000000 ) ) ;
#5829 = CARTESIAN_POINT ( 'NONE',  ( -1.495357591793033514, -24.55876337360558281, -12.70444646759402119 ) ) ;
#5828 = CARTESIAN_POINT ( 'NONE',  ( 1.758095523364999968, -60.52291663846999370, 12.57362173518999882 ) ) ;
#5830 = CARTESIAN_POINT ( 'NONE',  ( -4.573833614540000703, -76.66157131458999174, 11.16101939607000126 ) ) ;
#5831 = ORIENTED_EDGE ( 'NONE', *, *, #40673, .T. ) ;
#5832 = CARTESIAN_POINT ( 'NONE',  ( 1.204906488280999888, -83.95346544543099299, -3.775470985156000214 ) ) ;
#5833 = CARTESIAN_POINT ( 'NONE',  ( 0.3732109351705000244, -80.01347754060989814, 11.16625220509000016 ) ) ;
#5834 = STYLED_ITEM ( 'NONE', ( #54305 ), #11003 ) ;
#5835 = EDGE_CURVE ( 'NONE', #45319, #27414, #3950, .T. ) ;
#5836 = CARTESIAN_POINT ( 'NONE',  ( 7.585176102898188333, -78.30167758068601813, -5.294072734977127048 ) ) ;
#5837 = DIRECTION ( 'NONE',  ( 0.000000000000000000, 0.000000000000000000, 1.000000000000000000 ) ) ;
#5838 = CARTESIAN_POINT ( 'NONE',  ( -10.17713110909000029, -76.86714958119398489, 4.716330562529999604 ) ) ;
#5839 = CARTESIAN_POINT ( 'NONE',  ( 0.000000000000000000, -75.15999999999999659, 0.000000000000000000 ) ) ;
#5840 = CARTESIAN_POINT ( 'NONE',  ( -4.778484498315999751, -78.80937680961498870, 8.361775879827998637 ) ) ;
#5841 = CARTESIAN_POINT ( 'NONE',  ( 0.7311670807272000472, -82.22766660800999716, 1.496881327486000002 ) ) ;
#5842 = DIRECTION ( 'NONE',  ( -0.7071067811865475727, 0.000000000000000000, 0.7071067811865475727 ) ) ;
#5843 = CARTESIAN_POINT ( 'NONE',  ( -7.483407197968000801, -77.00000000000000000, 5.437013583706000297 ) ) ;
#5844 = EDGE_LOOP ( 'NONE', ( #47249, #20049, #54096, #24145 ) ) ;
#5845 = CARTESIAN_POINT ( 'NONE',  ( -1.741532119305578830, -0.7916666666665673757, 3.009437940290339064 ) ) ;
#5846 = CARTESIAN_POINT ( 'NONE',  ( 11.22355342542000045, -80.45517816094930197, 0.9700744431168999427 ) ) ;
#5847 = CARTESIAN_POINT ( 'NONE',  ( -1.250000000000000000, -76.50000000000000000, 0.000000000000000000 ) ) ;
#5848 = ORIENTED_EDGE ( 'NONE', *, *, #55863, .F. ) ;
#5849 = CARTESIAN_POINT ( 'NONE',  ( -1.112801787005999854, -79.17487453554200272, -0.6258220204580999813 ) ) ;
#5850 = ADVANCED_FACE ( 'NONE', ( #1917 ), #14879, .F. ) ;
#5851 = CARTESIAN_POINT ( 'NONE',  ( -10.83547269566999915, -79.70737966341999936, -4.008037460590999856 ) ) ;
#5852 = EDGE_LOOP ( 'NONE', ( #33994, #24458, #41513, #38254 ) ) ;
#5853 = CARTESIAN_POINT ( 'NONE',  ( 12.13705548371000020, -79.01423986341698935, 0.8212409526314999875 ) ) ;
#5854 = CARTESIAN_POINT ( 'NONE',  ( 5.497693353104999403, -77.32727988493299165, 9.771496850480000163 ) ) ;
#5855 = CARTESIAN_POINT ( 'NONE',  ( 8.894916816534065518, -62.02809132899625411, -9.073484344827472015 ) ) ;
#5856 = AXIS2_PLACEMENT_3D ( 'NONE', #50630, #41171, #9887 ) ;
#5857 = ORIENTED_EDGE ( 'NONE', *, *, #49509, .T. ) ;
#5858 = ORIENTED_EDGE ( 'NONE', *, *, #29337, .T. ) ;
#5859 = CARTESIAN_POINT ( 'NONE',  ( -10.53562613913000057, -55.59442116235999976, -7.620013630307000518 ) ) ;
#5860 = CARTESIAN_POINT ( 'NONE',  ( 5.496668217546000434, -80.06301958804498042, -8.073860231047000013 ) ) ;
#5861 = ORIENTED_EDGE ( 'NONE', *, *, #18056, .T. ) ;
#5862 = CARTESIAN_POINT ( 'NONE',  ( 12.43410192427999839, -54.35868879854000113, 1.192687910178000132 ) ) ;
#5863 = CARTESIAN_POINT ( 'NONE',  ( 8.803747447820532201, -25.21568152340251601, -9.164340453613974091 ) ) ;
#5864 = EDGE_LOOP ( 'NONE', ( #27262, #37310, #20014 ) ) ;
#5865 = CARTESIAN_POINT ( 'NONE',  ( -12.48409101788000086, -23.36970703835000052, -1.669510252625999946 ) ) ;
#5866 = CARTESIAN_POINT ( 'NONE',  ( 8.666912951388480835, -24.99291380871280310, 9.019442093124220960 ) ) ;
#5867 = PLANE ( 'NONE',  #33836 ) ;
#5868 = VECTOR ( 'NONE', #12097, 1000.000000000000000 ) ;
#5869 = FACE_OUTER_BOUND ( 'NONE', #30671, .T. ) ;
#5870 = CARTESIAN_POINT ( 'NONE',  ( 8.130813118010999929, -17.31476110167000115, -9.546856411651999608 ) ) ;
#5871 = CARTESIAN_POINT ( 'NONE',  ( -10.23602088258210152, -76.67184350084455957, 3.794244288828453993 ) ) ;
#5872 = CARTESIAN_POINT ( 'NONE',  ( -12.70228549161442544, -17.17187149261430079, -1.205357499388056475 ) ) ;
#5873 = CARTESIAN_POINT ( 'NONE',  ( 1.210448961617198282, -79.15058965391948220, 0.9017437205617973017 ) ) ;
#5874 = CARTESIAN_POINT ( 'NONE',  ( 10.36746145411186149, -18.23400545010334284, 7.635225828759837796 ) ) ;
#5875 = VERTEX_POINT ( 'NONE', #46209 ) ;
#5876 = CARTESIAN_POINT ( 'NONE',  ( -3.151328970204000157, -76.12173232274999179, -11.89977497056000111 ) ) ;
#5877 = ADVANCED_FACE ( 'NONE', ( #45623 ), #27547, .F. ) ;
#5878 = CARTESIAN_POINT ( 'NONE',  ( 0.000000000000000000, -76.75499999999999545, 0.000000000000000000 ) ) ;
#5879 = CARTESIAN_POINT ( 'NONE',  ( 7.760939450761999758, -61.03085356300000086, -10.15321588361999972 ) ) ;
#5880 = CARTESIAN_POINT ( 'NONE',  ( 4.750030159171999777, -78.63931674665001026, -11.30647155123999958 ) ) ;
#5881 = CARTESIAN_POINT ( 'NONE',  ( -3.164411967817999827, -77.17036772586099858, -11.86639179494000018 ) ) ;
#5882 = CARTESIAN_POINT ( 'NONE',  ( -10.14948852603999896, -56.04899164556000102, -7.674614791885000287 ) ) ;
#5883 = ADVANCED_FACE ( 'NONE', ( #10468 ), #14318, .F. ) ;
#5884 = CARTESIAN_POINT ( 'NONE',  ( 12.50385649908071173, -24.78436723039533263, 0.8579675316851195221 ) ) ;
#5885 = CARTESIAN_POINT ( 'NONE',  ( 9.134039069024126434, -78.24329585021101252, -7.883706473441567830 ) ) ;
#5886 = DIRECTION ( 'NONE',  ( 0.000000000000000000, -1.000000000000000000, 0.000000000000000000 ) ) ;
#5887 = VERTEX_POINT ( 'NONE', #32582 ) ;
#5888 = LINE ( 'NONE', #23896, #496 ) ;
#5889 = CARTESIAN_POINT ( 'NONE',  ( -0.5083718267365000543, -77.20835577409998507, 9.693975953357998776 ) ) ;
#5890 = DIRECTION ( 'NONE',  ( 0.000000000000000000, -1.000000000000000000, 0.000000000000000000 ) ) ;
#5891 = AXIS2_PLACEMENT_3D ( 'NONE', #45702, #41839, #36815 ) ;
#5892 = DIRECTION ( 'NONE',  ( 0.000000000000000000, 0.7071067811866525998, -0.7071067811864425456 ) ) ;
#5893 = CARTESIAN_POINT ( 'NONE',  ( 2.011257834211999995, -2.625894741107999586, 3.306836841438999919 ) ) ;
#5894 = CARTESIAN_POINT ( 'NONE',  ( 0.9683650813416999625, -78.14026560866999205, -12.01074688531000056 ) ) ;
#5895 = CARTESIAN_POINT ( 'NONE',  ( 9.401690036064000111, -78.99979041159998872, -2.543243121375000193 ) ) ;
#5896 = CARTESIAN_POINT ( 'NONE',  ( -10.84963681563615800, -76.16850844397271203, 4.510596736791835148 ) ) ;
#5897 = CARTESIAN_POINT ( 'NONE',  ( 10.26057445098000187, -78.80432170917399048, 3.727731092327000173 ) ) ;
#5898 = CARTESIAN_POINT ( 'NONE',  ( -0.5188809666119423847, -85.80681307385597734, 4.172962832911210285 ) ) ;
#5899 = VERTEX_POINT ( 'NONE', #19911 ) ;
#5900 = CARTESIAN_POINT ( 'NONE',  ( 12.70556836347999941, -25.22772277227999993, 2.424222353299999887E-09 ) ) ;
#5901 = AXIS2_PLACEMENT_3D ( 'NONE', #56671, #53384, #2659 ) ;
#5902 = CARTESIAN_POINT ( 'NONE',  ( 11.71941206009442205, -79.16681733756954031, 2.493429747108907968 ) ) ;
#5903 = EDGE_CURVE ( 'NONE', #3955, #31290, #3045, .T. ) ;
#5904 = CARTESIAN_POINT ( 'NONE',  ( 3.250000000000000444, -2.260416666666666075, 0.4254240051736248862 ) ) ;
#5905 = CARTESIAN_POINT ( 'NONE',  ( 8.867070753125000593, -78.69030182778799087, -6.468312982590000537 ) ) ;
#5906 = CARTESIAN_POINT ( 'NONE',  ( -0.3070260000256299082, -79.20550685558696102, -1.218020810600508153 ) ) ;
#5907 = CARTESIAN_POINT ( 'NONE',  ( 9.596002108778145967, -77.70208333333330586, 7.374560639699002884 ) ) ;
#5908 = CARTESIAN_POINT ( 'NONE',  ( 1.654508304067999980, -79.28174448050398837, -9.527719980787999532 ) ) ;
#5909 = CARTESIAN_POINT ( 'NONE',  ( 9.516265623875000301, -17.17460635740999919, -8.227505979428000771 ) ) ;
#5910 = CARTESIAN_POINT ( 'NONE',  ( 13.13047446164998711, -59.58578169018999660, 0.8260994316375004365 ) ) ;
#5911 = ORIENTED_EDGE ( 'NONE', *, *, #32682, .F. ) ;
#5913 = AXIS2_PLACEMENT_3D ( 'NONE', #42949, #2506, #20510 ) ;
#5912 = CARTESIAN_POINT ( 'NONE',  ( 6.907293935673000540, -79.09904856920998384, 8.895125352942999442 ) ) ;
#5914 = CARTESIAN_POINT ( 'NONE',  ( 12.70228549161202380, -17.17187149263573431, 1.205357499442098357 ) ) ;
#5915 = CARTESIAN_POINT ( 'NONE',  ( 12.50240633875000107, -54.11762602111000575, 1.005381409374000112 ) ) ;
#5916 = CARTESIAN_POINT ( 'NONE',  ( -3.437217181655167320, -78.70000000000000284, 1.942148107221286724 ) ) ;
#5917 = CARTESIAN_POINT ( 'NONE',  ( -9.191912067484826920, -77.89725430145915652, 7.750011545041279426 ) ) ;
#5918 = AXIS2_PLACEMENT_3D ( 'NONE', #15638, #28916, #29203 ) ;
#5919 = CARTESIAN_POINT ( 'NONE',  ( -0.8842298993840882471, -81.53809034327093741, 0.8830699700463247037 ) ) ;
#5920 = ADVANCED_FACE ( 'NONE', ( #55926 ), #23743, .F. ) ;
#5921 = CARTESIAN_POINT ( 'NONE',  ( -9.805777851055321293, -79.39025696075076155, -5.446864207918929779 ) ) ;
#5922 = CARTESIAN_POINT ( 'NONE',  ( -9.340210362350283901, -76.99999999999998579, 0.02720789100463689644 ) ) ;
#5923 = CARTESIAN_POINT ( 'NONE',  ( -3.453171399369999950, -1.763032031398999999, -0.5706200895263999762 ) ) ;
#5924 = EDGE_CURVE ( 'NONE', #49174, #48925, #44490, .T. ) ;
#5925 = CARTESIAN_POINT ( 'NONE',  ( -10.75000000000000000, -81.00000000000000000, 2.851355842494999902E-13 ) ) ;
#5926 = CARTESIAN_POINT ( 'NONE',  ( 1.980464439859999981, -21.75472017459999918, 12.85144117154000121 ) ) ;
#5927 = CARTESIAN_POINT ( 'NONE',  ( 4.634636847927953163, -78.79041100284936761, 9.949269327501806259 ) ) ;
#5928 = B_SPLINE_CURVE_WITH_KNOTS ( 'NONE', 3,
 ( #46361, #41329, #18897, #36888, #23605, #19187 ),
 .UNSPECIFIED., .F., .F.,
 ( 4, 2, 4 ),
 ( 0.000000000000000000, 0.5000000000000000000, 1.000000000000000000 ),
 .UNSPECIFIED. ) ;
#5929 = CARTESIAN_POINT ( 'NONE',  ( -12.50240681836000078, -61.48234730679999416, 1.005418944265999981 ) ) ;
#5930 = VERTEX_POINT ( 'NONE', #19326 ) ;
#5931 = EDGE_LOOP ( 'NONE', ( #45682, #29591, #161, #5653 ) ) ;
#5932 = CARTESIAN_POINT ( 'NONE',  ( -0.6017968039497372246, -77.78000000000000114, 9.523103445003338052 ) ) ;
#5933 = CARTESIAN_POINT ( 'NONE',  ( 9.931997526924730479, -78.81882101904967897, -4.113022196682803333 ) ) ;
#5934 = EDGE_LOOP ( 'NONE', ( #36366, #42448, #44872, #50823 ) ) ;
#5935 = DIRECTION ( 'NONE',  ( 0.000000000000000000, -1.000000000000000000, 0.000000000000000000 ) ) ;
#5936 = ADVANCED_FACE ( 'NONE', ( #51215 ), #10767, .F. ) ;
#5937 = CARTESIAN_POINT ( 'NONE',  ( -8.997332162609597006, -79.37373539064718386, 3.050007033374654508 ) ) ;
#5938 = B_SPLINE_CURVE_WITH_KNOTS ( 'NONE', 3,
 ( #48859, #13112, #18154, #5152, #39984, #23153, #17258, #3971, #17554, #49147, #8697, #26688, #19600, #27856, #42340, #51205, #6310, #28443 ),
 .UNSPECIFIED., .F., .F.,
 ( 4, 2, 2, 2, 2, 2, 2, 2, 4 ),
 ( 0.000000000000000000, 0.1250000000000000000, 0.2500000000000000000, 0.3750000000000000000, 0.5000000000000000000, 0.6250000000000000000, 0.7500000000000000000, 0.8750000000000000000, 1.000000000000000000 ),
 .UNSPECIFIED. ) ;
#5939 = CARTESIAN_POINT ( 'NONE',  ( 7.633478499842999199, -60.00098177563999968, 10.36292345936000103 ) ) ;
#5940 = CARTESIAN_POINT ( 'NONE',  ( 8.196408543750321130, -76.36575423402705098, 9.036094815919039291 ) ) ;
#5941 = CARTESIAN_POINT ( 'NONE',  ( 7.103502425096676731, -78.87345073205365509, 9.415326140932604559 ) ) ;
#5942 = AXIS2_PLACEMENT_3D ( 'NONE', #27349, #9358, #4928 ) ;
#5943 = CARTESIAN_POINT ( 'NONE',  ( 8.645668071321999548, -78.57107317891799880, 7.146365085715999044 ) ) ;
#5944 = EDGE_LOOP ( 'NONE', ( #49107, #34783, #6236, #11329, #6594 ) ) ;
#5945 = CARTESIAN_POINT ( 'NONE',  ( -8.620921567869039848, -25.16528830419391838, 9.346042574068809117 ) ) ;
#5946 = ORIENTED_EDGE ( 'NONE', *, *, #2953, .T. ) ;
#5947 = CARTESIAN_POINT ( 'NONE',  ( 8.729031720696649899, -77.37686029687922940, 3.060862442712833698 ) ) ;
#5948 = CARTESIAN_POINT ( 'NONE',  ( -0.2944660333051000167, -79.63485486817799597, 1.286023070983999927 ) ) ;
#5949 = PLANE ( 'NONE',  #24379 ) ;
#5950 = CARTESIAN_POINT ( 'NONE',  ( -1.607511835558000035, -78.99940294806400232, -0.1512538100690999920 ) ) ;
#5951 = VECTOR ( 'NONE', #16160, 1000.000000000000114 ) ;
#5952 = CARTESIAN_POINT ( 'NONE',  ( 2.500000000000000000, -80.69999999999998863, 0.000000000000000000 ) ) ;
#5953 = FACE_OUTER_BOUND ( 'NONE', #21749, .T. ) ;
#5954 = CARTESIAN_POINT ( 'NONE',  ( -0.1732310466989999687, -77.59547045605000903, 1.530487294790999986 ) ) ;
#5955 = CARTESIAN_POINT ( 'NONE',  ( -1.507531252938999922, -78.99930496681159298, -3.890673863795999665 ) ) ;
#5956 = EDGE_CURVE ( 'NONE', #39914, #22868, #25101, .T. ) ;
#5957 =( GEOMETRIC_REPRESENTATION_CONTEXT ( 3 ) GLOBAL_UNCERTAINTY_ASSIGNED_CONTEXT ( ( #37827 ) ) GLOBAL_UNIT_ASSIGNED_CONTEXT ( ( #56019, #10567, #24720 ) ) REPRESENTATION_CONTEXT ( 'NONE', 'WORKASPACE' ) );
#5958 = CARTESIAN_POINT ( 'NONE',  ( 3.902863791433999641, -79.27515797775897965, 10.22034591202999820 ) ) ;
#5959 = CARTESIAN_POINT ( 'NONE',  ( 12.71536556660652728, -60.92544729019407157, 1.781281568951020411 ) ) ;
#5960 = CARTESIAN_POINT ( 'NONE',  ( 8.538006731470160204, -79.08654938339437024, 4.209831911330708110 ) ) ;
#5961 = CARTESIAN_POINT ( 'NONE',  ( -1.556282511482000253, -85.87701485180299699, 3.184825365493999527 ) ) ;
#5962 = VERTEX_POINT ( 'NONE', #5163 ) ;
#5963 = CARTESIAN_POINT ( 'NONE',  ( 12.00000000000000000, -79.65000000000000568, 0.000000000000000000 ) ) ;
#5964 = CARTESIAN_POINT ( 'NONE',  ( -1.494795747725999879, -80.92041546398999685, -0.5291335979940999801 ) ) ;
#5965 = CARTESIAN_POINT ( 'NONE',  ( 9.769349281881931191, -77.88441593596398604, 4.488065258493001863 ) ) ;
#5966 = CARTESIAN_POINT ( 'NONE',  ( 7.919842512016999514, -77.45141689038899813, 8.988445846368000147 ) ) ;
#5967 = DIRECTION ( 'NONE',  ( -1.000000000000000000, 0.000000000000000000, 0.000000000000000000 ) ) ;
#5968 = CARTESIAN_POINT ( 'NONE',  ( 0.4989225658573747113, -78.59297769293915792, 1.172947819115397916 ) ) ;
#5969 = CARTESIAN_POINT ( 'NONE',  ( 2.908337012396843946, -3.047664591510003795, 1.983095937705898537 ) ) ;
#5970 = CARTESIAN_POINT ( 'NONE',  ( 9.648882615658788353, -80.88645074276622893, 4.741768800263339578 ) ) ;
#5971 = CARTESIAN_POINT ( 'NONE',  ( -8.508571376020000798, -77.61436236583298864, -4.026835934908000070 ) ) ;
#5972 = CARTESIAN_POINT ( 'NONE',  ( 0.4002886859631615835, -86.09999999999999432, -8.935310233444422323 ) ) ;
#5973 = CARTESIAN_POINT ( 'NONE',  ( 10.12138908678999982, -77.74142057354099222, 4.388532480841000449 ) ) ;
#5974 = CARTESIAN_POINT ( 'NONE',  ( 0.8930464934706795477, -0.8411458150437891579, -3.319805051666669726 ) ) ;
#5975 = CARTESIAN_POINT ( 'NONE',  ( -12.00000000000000178, -78.31041666666665435, -1.570796326794897890 ) ) ;
#5976 = EDGE_LOOP ( 'NONE', ( #20885, #35365, #38386, #29389 ) ) ;
#5977 = DIRECTION ( 'NONE',  ( -1.000000000000000000, 0.000000000000000000, 0.000000000000000000 ) ) ;
#5978 = CARTESIAN_POINT ( 'NONE',  ( -2.015551294784000191, -60.60347704811000824, -12.79857978897999971 ) ) ;
#5979 = CARTESIAN_POINT ( 'NONE',  ( 8.098288960089517374, -80.40744867782952099, 7.103106135035865520 ) ) ;
#5980 = CARTESIAN_POINT ( 'NONE',  ( -6.984027423104000043, -77.19459030567298896, 8.777327129872999123 ) ) ;
#5981 = CARTESIAN_POINT ( 'NONE',  ( 5.330173052271000245, -78.20449537012198959, 9.594439332582000546 ) ) ;
#5982 = CARTESIAN_POINT ( 'NONE',  ( 7.765022563360999719, -24.09093562100999719, -9.830785949113998612 ) ) ;
#5983 = CARTESIAN_POINT ( 'NONE',  ( -0.4114167394185317961, -85.84947918359929986, 3.991239199179264840 ) ) ;
#5984 = DIRECTION ( 'NONE',  ( -0.7071067811865474617, 0.000000000000000000, -0.7071067811865474617 ) ) ;
#5985 = CYLINDRICAL_SURFACE ( 'NONE', #28649, 1.750000000000001332 ) ;
#5986 = CARTESIAN_POINT ( 'NONE',  ( 0.2052812982897999905, -85.80069503318799207, 4.167475636592000932 ) ) ;
#5987 = CARTESIAN_POINT ( 'NONE',  ( -0.7554284705563480973, -79.58333333333334281, -1.310679582531387277 ) ) ;
#5988 = AXIS2_PLACEMENT_3D ( 'NONE', #52225, #15916, #35047 ) ;
#5989 = CARTESIAN_POINT ( 'NONE',  ( 10.47513558171999826, -54.99636614397000045, -7.624778817986999968 ) ) ;
#5990 = B_SPLINE_CURVE_WITH_KNOTS ( 'NONE', 3,
 ( #24471, #28003, #46052, #23301, #15320, #5576 ),
 .UNSPECIFIED., .F., .F.,
 ( 4, 1, 1, 4 ),
 ( 0.000000000000000000, 0.3333333333333000081, 0.6666666666667000474, 1.000000000000000000 ),
 .UNSPECIFIED. ) ;
#5991 = CARTESIAN_POINT ( 'NONE',  ( 7.538328940028000247, -76.95994809191398645, -8.367052130149000178 ) ) ;
#5992 = CARTESIAN_POINT ( 'NONE',  ( -1.542698325316999908, -81.29879647607999971, 0.6290719308543000210 ) ) ;
#5993 = CARTESIAN_POINT ( 'NONE',  ( 1.031014977102000074, -78.26784532121999405, 0.9975409193212999570 ) ) ;
#5994 = CARTESIAN_POINT ( 'NONE',  ( -10.42531125074000009, -18.73514854687000053, -7.624341767140999870 ) ) ;
#5995 = CARTESIAN_POINT ( 'NONE',  ( 2.935661446561999899, -79.99999999999998579, -9.035036904803998681 ) ) ;
#5996 = CARTESIAN_POINT ( 'NONE',  ( -1.500000000000000000, -83.34999999999999432, 0.000000000000000000 ) ) ;
#5997 = EDGE_LOOP ( 'NONE', ( #1864, #4904, #21685, #10220, #28201, #44556, #40343, #37595, #14059, #25029, #29160 ) ) ;
#5998 = CARTESIAN_POINT ( 'NONE',  ( 1.249651984936067439, -79.84628556922963583, -0.06748478051193507188 ) ) ;
#5999 = VECTOR ( 'NONE', #55637, 1000.000000000000000 ) ;
#6000 = CARTESIAN_POINT ( 'NONE',  ( 0.3926218265389221362, -78.04583333333334849, -1.460959015002473160 ) ) ;
#6001 = ORIENTED_EDGE ( 'NONE', *, *, #26106, .T. ) ;
#6002 = CIRCLE ( 'NONE', #47503, 1.750000000000001332 ) ;
#6003 = CARTESIAN_POINT ( 'NONE',  ( 0.3134647746052411921, -81.74538725804720229, -1.211105577459558269 ) ) ;
#6004 = CARTESIAN_POINT ( 'NONE',  ( -10.85854583389000005, -79.44473956280799598, 1.947746583844000012 ) ) ;
#6005 = FACE_OUTER_BOUND ( 'NONE', #29861, .T. ) ;
#6006 = ORIENTED_EDGE ( 'NONE', *, *, #25191, .F. ) ;
#6007 = EDGE_LOOP ( 'NONE', ( #41524, #49854, #14002, #10084, #38176, #29632, #12360 ) ) ;
#6008 = CARTESIAN_POINT ( 'NONE',  ( -1.284296857402999814, -81.56787935870499950, 0.6005338976478999946 ) ) ;
#6009 = ORIENTED_EDGE ( 'NONE', *, *, #32194, .F. ) ;
#6010 = ORIENTED_EDGE ( 'NONE', *, *, #14252, .T. ) ;
#6011 = CYLINDRICAL_SURFACE ( 'NONE', #47197, 1.750000000000001332 ) ;
#6012 = DIRECTION ( 'NONE',  ( -1.000000000000000000, 0.000000000000000000, 0.000000000000000000 ) ) ;
#6013 =( NAMED_UNIT ( * ) PLANE_ANGLE_UNIT ( ) SI_UNIT ( $, .RADIAN. ) );
#6014 = EDGE_CURVE ( 'NONE', #16529, #515, #54870, .T. ) ;
#6015 = CARTESIAN_POINT ( 'NONE',  ( -3.384237465907204534, -81.74479165198742692, -0.6379114951690191271 ) ) ;
#6016 = CARTESIAN_POINT ( 'NONE',  ( -5.773189589619000195, -78.24451001420199248, 8.192511063987998554 ) ) ;
#6017 = CARTESIAN_POINT ( 'NONE',  ( 3.540263149936455633, -78.25629661996973141, -8.545667284253724461 ) ) ;
#6018 = CARTESIAN_POINT ( 'NONE',  ( 0.000000000000000000, -86.29999999996098836, 0.000000000000000000 ) ) ;
#6019 = ORIENTED_EDGE ( 'NONE', *, *, #28429, .T. ) ;
#6020 = EDGE_LOOP ( 'NONE', ( #53272, #45084, #32049 ) ) ;
#6021 = CARTESIAN_POINT ( 'NONE',  ( -7.544460730989308139, -77.55089713445312327, 5.352097458047992973 ) ) ;
#6022 = CARTESIAN_POINT ( 'NONE',  ( -12.70395504299446188, -24.60679290123326268, 1.447100708826857263 ) ) ;
#6023 = DIRECTION ( 'NONE',  ( 0.000000000000000000, 1.000000000000000000, 0.000000000000000000 ) ) ;
#6024 = FACE_OUTER_BOUND ( 'NONE', #26761, .T. ) ;
#6025 = CARTESIAN_POINT ( 'NONE',  ( -3.536681740116999872, -78.17453429284898903, 9.036735673663999435 ) ) ;
#6026 = DIRECTION ( 'NONE',  ( 0.000000000000000000, 1.000000000000000000, 0.000000000000000000 ) ) ;
#6027 = CARTESIAN_POINT ( 'NONE',  ( -10.01234990228999955, -23.29849137228000444, 7.653559502275999016 ) ) ;
#6028 = CARTESIAN_POINT ( 'NONE',  ( 9.596002108778145967, -76.70208333333333428, 7.374560639699002884 ) ) ;
#6029 = EDGE_CURVE ( 'NONE', #36474, #35786, #56796, .T. ) ;
#6030 = CARTESIAN_POINT ( 'NONE',  ( -0.3737996561424999920, -80.03882331289000263, 1.420113360969999849 ) ) ;
#6031 = AXIS2_PLACEMENT_3D ( 'NONE', #34867, #3310, #30443 ) ;
#6032 = CARTESIAN_POINT ( 'NONE',  ( -1.184016694733479591, -77.43484693750340853, 9.372457216979636740 ) ) ;
#6033 = CARTESIAN_POINT ( 'NONE',  ( -0.4365072073316000334, -80.60649082017198452, -4.151996103213000389 ) ) ;
#6034 = CARTESIAN_POINT ( 'NONE',  ( 0.1623090455760520801, -79.38352240831720508, -1.503739187786481191 ) ) ;
#6035 = CARTESIAN_POINT ( 'NONE',  ( 9.342221983604002133, -78.29936001420199432, -2.562053005734000077 ) ) ;
#6036 = CARTESIAN_POINT ( 'NONE',  ( -10.74950085534044852, -76.61052573971902291, -1.407179153412859929 ) ) ;
#6037 = CARTESIAN_POINT ( 'NONE',  ( -7.619389775686000732, -18.59213701582999789, -10.35398629635000134 ) ) ;
#6039 = CARTESIAN_POINT ( 'NONE',  ( 13.89248034750000116, -32.39159251014999796, 2.632538495369999938E-05 ) ) ;
#6038 = CARTESIAN_POINT ( 'NONE',  ( 1.500000000000000000, -78.64999999999999147, 0.000000000000000000 ) ) ;
#6040 = CARTESIAN_POINT ( 'NONE',  ( -1.570796326794937636, -78.28541666666666288, 11.99999999999999467 ) ) ;
#6041 = CARTESIAN_POINT ( 'NONE',  ( 4.769507551644696974, -80.00000000000000000, -8.276756506782131595 ) ) ;
#6042 = ADVANCED_FACE ( 'NONE', ( #25482 ), #47374, .F. ) ;
#6043 = CARTESIAN_POINT ( 'NONE',  ( -1.135826688880000157, -81.30663953507000485, -0.9797437077257000748 ) ) ;
#6044 = CARTESIAN_POINT ( 'NONE',  ( 9.802742422367249020, -77.20000000000000284, -4.551162862351648464 ) ) ;
#6045 = VERTEX_POINT ( 'NONE', #29613 ) ;
#6046 = CARTESIAN_POINT ( 'NONE',  ( -2.895491044260078528, -3.500000000000000000, -1.620397986153582437 ) ) ;
#6047 = LINE ( 'NONE', #15198, #36080 ) ;
#6048 = EDGE_CURVE ( 'NONE', #16887, #43630, #43401, .T. ) ;
#6049 = DIRECTION ( 'NONE',  ( 1.000000000000000000, 0.000000000000000000, 0.000000000000000000 ) ) ;
#6050 = CARTESIAN_POINT ( 'NONE',  ( 12.43641409355999983, -61.71801033862000452, 0.03481937293210000256 ) ) ;
#6051 = CARTESIAN_POINT ( 'NONE',  ( -3.547312378341000549, -79.79804137959898469, 8.966318398112001375 ) ) ;
#6052 = CARTESIAN_POINT ( 'NONE',  ( -8.048032176077001054, -78.37932536818000528, 9.328081102756000220 ) ) ;
#6053 = CARTESIAN_POINT ( 'NONE',  ( -0.007641576831010176221, -79.47517447817466518, 10.74992670947085571 ) ) ;
#6054 = CARTESIAN_POINT ( 'NONE',  ( 4.145750262472000180, -79.10401332859899526, -8.580453259755000062 ) ) ;
#6055 = FACE_OUTER_BOUND ( 'NONE', #12407, .T. ) ;
#6056 = CARTESIAN_POINT ( 'NONE',  ( -7.421505610835000155, -77.61136506546499447, 8.486883608244999877 ) ) ;
#6057 = CIRCLE ( 'NONE', #46628, 0.5000000000000000000 ) ;
#6058 = CARTESIAN_POINT ( 'NONE',  ( 0.7766715314972000295, -81.07327799737899454, -1.403532576748999894 ) ) ;
#6059 = CARTESIAN_POINT ( 'NONE',  ( -8.997179024602999675, -79.11904514476064776, 3.687079342326999853 ) ) ;
#6060 = CARTESIAN_POINT ( 'NONE',  ( -12.00000000000000000, -18.75000000000000000, 0.000000000000000000 ) ) ;
#6062 = CARTESIAN_POINT ( 'NONE',  ( -3.250000000000001776, -2.989583333333332593, 0.4254240051736045136 ) ) ;
#6061 = CARTESIAN_POINT ( 'NONE',  ( -3.707226347175000214, -85.82921411580198878, 1.046803743307999968 ) ) ;
#6063 = CARTESIAN_POINT ( 'NONE',  ( -8.630067035710000667, -79.72545584965399712, -4.100810385846999750 ) ) ;
#6064 = CARTESIAN_POINT ( 'NONE',  ( -7.648026768036999989, -60.04999998387000204, -10.12290050219000115 ) ) ;
#6065 = FACE_OUTER_BOUND ( 'NONE', #41707, .T. ) ;
#6066 = ADVANCED_FACE ( 'NONE', ( #11063 ), #7752, .T. ) ;
#6067 = VECTOR ( 'NONE', #25506, 1000.000000000000000 ) ;
#6068 = CARTESIAN_POINT ( 'NONE',  ( -9.390656772802731922, -77.14192976238929589, -5.419584780083640752 ) ) ;
#6069 = CARTESIAN_POINT ( 'NONE',  ( 1.243547092045927949, -77.26458333333334849, 9.500000000000003553 ) ) ;
#6070 = DIRECTION ( 'NONE',  ( 1.000000000000000000, 0.000000000000000000, 0.000000000000000000 ) ) ;
#6071 = ORIENTED_EDGE ( 'NONE', *, *, #55507, .F. ) ;
#6072 = ORIENTED_EDGE ( 'NONE', *, *, #10519, .F. ) ;
#6073 = CARTESIAN_POINT ( 'NONE',  ( -2.112861425255000203, -79.31263287794399730, -11.84242215301999934 ) ) ;
#6074 = AXIS2_PLACEMENT_3D ( 'NONE', #30668, #26251, #8839 ) ;
#6075 = CARTESIAN_POINT ( 'NONE',  ( 1.249471583050132839, -78.32919795546139596, -0.3269302217491961149 ) ) ;
#6076 = CARTESIAN_POINT ( 'NONE',  ( 3.250000000000000000, -2.750000000000000000, 0.000000000000000000 ) ) ;
#6077 = VERTEX_POINT ( 'NONE', #3346 ) ;
#6078 = CARTESIAN_POINT ( 'NONE',  ( 7.455335830631999450, -78.44471668781000062, 9.319520915745998835 ) ) ;
#6079 = ORIENTED_EDGE ( 'NONE', *, *, #20325, .T. ) ;
#6080 = ORIENTED_EDGE ( 'NONE', *, *, #6297, .F. ) ;
#6081 = CARTESIAN_POINT ( 'NONE',  ( 10.74999999999999645, -78.76041666666667140, 1.407171709420451666 ) ) ;
#6082 = ORIENTED_EDGE ( 'NONE', *, *, #54858, .T. ) ;
#6083 = CARTESIAN_POINT ( 'NONE',  ( 2.359654807561999856, -81.13869062511399477, 2.648320043780999722 ) ) ;
#6084 = CARTESIAN_POINT ( 'NONE',  ( 12.00000000000000000, -79.65000000000000568, 0.000000000000000000 ) ) ;
#6085 = EDGE_LOOP ( 'NONE', ( #13756, #45817, #13416 ) ) ;
#6086 = CARTESIAN_POINT ( 'NONE',  ( 1.186068794074434996, -82.82441975421146196, -0.3952336422712977027 ) ) ;
#6087 = CARTESIAN_POINT ( 'NONE',  ( -7.642160924878999673, -59.58461666436000570, 10.55911395187000146 ) ) ;
#6088 = ORIENTED_EDGE ( 'NONE', *, *, #38472, .F. ) ;
#6089 = CARTESIAN_POINT ( 'NONE',  ( 1.749899258077703301, -18.61283151237005740, 12.55433901290730603 ) ) ;
#6090 = CARTESIAN_POINT ( 'NONE',  ( -1.521427883520144686, -78.25414970944238746, -0.07951690128473563879 ) ) ;
#6091 = CARTESIAN_POINT ( 'NONE',  ( -10.99392646372974092, -79.79999999999999716, -4.674613442768594140 ) ) ;
#6092 = DIRECTION ( 'NONE',  ( 0.000000000000000000, -1.000000000000000000, 0.000000000000000000 ) ) ;
#6093 = CARTESIAN_POINT ( 'NONE',  ( 9.889722810339758752, -78.75056565254401164, 7.252677050776306089 ) ) ;
#6094 = CARTESIAN_POINT ( 'NONE',  ( -6.473047519705999342, -78.18311006013023245, 7.229824698717000508 ) ) ;
#6095 = CARTESIAN_POINT ( 'NONE',  ( -1.660522255173999984, -76.58517650455699766, 11.05968181062000077 ) ) ;
#6096 = CARTESIAN_POINT ( 'NONE',  ( -0.8307515566936579665, -76.48212377155830666, 10.82435606304636799 ) ) ;
#6097 = EDGE_CURVE ( 'NONE', #9880, #16336, #56791, .T. ) ;
#6098 = FACE_BOUND ( 'NONE', #10057, .T. ) ;
#6099 = CIRCLE ( 'NONE', #29644, 14.00000000000000355 ) ;
#6100 = CARTESIAN_POINT ( 'NONE',  ( -7.655542440085000067, -59.57819125629999490, -10.38645071868999992 ) ) ;
#6101 = CARTESIAN_POINT ( 'NONE',  ( -6.480567632827825442, -78.66327994001753154, -6.600377077318754004 ) ) ;
#6102 = CARTESIAN_POINT ( 'NONE',  ( 3.194637145771936027, -76.55251996074613885, 11.30859510570057402 ) ) ;
#6103 = CARTESIAN_POINT ( 'NONE',  ( 1.980464439859999981, -20.24527982672000093, -12.85144117157999943 ) ) ;
#6104 = DIRECTION ( 'NONE',  ( 0.000000000000000000, 1.000000000000000000, 0.000000000000000000 ) ) ;
#6105 = VECTOR ( 'NONE', #58216, 1000.000000000000114 ) ;
#6106 = CARTESIAN_POINT ( 'NONE',  ( -5.531057285270385648, -80.18318348377982829, -9.508306399520915164 ) ) ;
#6107 = CARTESIAN_POINT ( 'NONE',  ( -3.137524286708853971, -3.080320021855812662, 0.8496376415343023236 ) ) ;
#6108 = CARTESIAN_POINT ( 'NONE',  ( 1.539579185250999904, -80.36553455456798645, -3.651804586294000288 ) ) ;
#6109 = CARTESIAN_POINT ( 'NONE',  ( -10.05357165398491759, -78.07129154303414964, 3.808089728372485272 ) ) ;
#6110 = CARTESIAN_POINT ( 'NONE',  ( 0.8734639515568026757, -82.91404585606140643, 0.8936271339499843869 ) ) ;
#6111 = CARTESIAN_POINT ( 'NONE',  ( -3.437187628289000152, -78.85171435493609238, -1.442231121412212840E-14 ) ) ;
#6112 = CARTESIAN_POINT ( 'NONE',  ( -7.159979337456084281, -76.27258029778182902, -9.317074303591205364 ) ) ;
#6113 = CARTESIAN_POINT ( 'NONE',  ( 9.025284355001986114, -80.00000000000000000, 2.926013110658441274 ) ) ;
#6114 = DIRECTION ( 'NONE',  ( -0.7071067811865474617, 0.000000000000000000, 0.7071067811865474617 ) ) ;
#6115 = CIRCLE ( 'NONE', #57027, 14.00000000000000000 ) ;
#6116 = CARTESIAN_POINT ( 'NONE',  ( 0.2218469911736734856, -3.500000000000000888, 3.293143398893245699 ) ) ;
#6117 = ADVANCED_FACE ( 'NONE', ( #12202 ), #11918, .F. ) ;
#6118 = CARTESIAN_POINT ( 'NONE',  ( 10.53101990617999917, -55.49360215019999742, 7.613962745591999592 ) ) ;
#6119 = CARTESIAN_POINT ( 'NONE',  ( -1.493074398910679834, -79.83713052442533353, 0.2323495900538211922 ) ) ;
#6120 = PLANE ( 'NONE',  #51241 ) ;
#6121 = CARTESIAN_POINT ( 'NONE',  ( -3.339615680726000235, -78.47284805011499031, 9.131854552393999569 ) ) ;
#6122 = CARTESIAN_POINT ( 'NONE',  ( 12.77651047016999897, -25.30895689136000115, -0.04321256188106999824 ) ) ;
#6123 = CARTESIAN_POINT ( 'NONE',  ( -8.771511755855000203, -77.43509585594499356, -8.593972346821999508 ) ) ;
#6124 = DIRECTION ( 'NONE',  ( 0.000000000000000000, 0.000000000000000000, -1.000000000000000000 ) ) ;
#6125 = CARTESIAN_POINT ( 'NONE',  ( 4.634563706678000550, -78.69030876264459096, 9.949112313689999709 ) ) ;
#6126 = CARTESIAN_POINT ( 'NONE',  ( 11.65748953279999967, -76.39446726005000698, -3.638198820018999857 ) ) ;
#6127 = ORIENTED_EDGE ( 'NONE', *, *, #51212, .T. ) ;
#6128 = CARTESIAN_POINT ( 'NONE',  ( 0.2633489006888999895, -85.39646544543099083, -3.747266932773000381 ) ) ;
#6129 = CARTESIAN_POINT ( 'NONE',  ( 11.39554093367000043, -81.02324881952658586, -0.4788264379577999996 ) ) ;
#6130 = CARTESIAN_POINT ( 'NONE',  ( 0.000000000000000000, -75.67500000000001137, 0.000000000000000000 ) ) ;
#6131 = CARTESIAN_POINT ( 'NONE',  ( -0.7554284705563480973, -81.58333333333332860, -1.310679582531387277 ) ) ;
#6132 = CARTESIAN_POINT ( 'NONE',  ( 1.025029370886000101E-14, -0.2000000000000005107, 0.000000000000000000 ) ) ;
#6133 = CARTESIAN_POINT ( 'NONE',  ( 10.12290050253000118, -23.24999997822999731, -7.648026768374000639 ) ) ;
#6134 = CARTESIAN_POINT ( 'NONE',  ( -9.316314781052998484, -77.35273344151198671, -2.840095070410999956 ) ) ;
#6135 = CARTESIAN_POINT ( 'NONE',  ( -0.5790013745696001024, -82.98557718933099636, -1.562055304842999925 ) ) ;
#6136 = CARTESIAN_POINT ( 'NONE',  ( 3.437187628289000152, -78.85171435493609238, 0.000000000000000000 ) ) ;
#6137 = CARTESIAN_POINT ( 'NONE',  ( -6.722422115750747551, -77.00000000000001421, 6.387398339048315776 ) ) ;
#6138 = EDGE_CURVE ( 'NONE', #56909, #1239, #29045, .T. ) ;
#6139 = ORIENTED_EDGE ( 'NONE', *, *, #28890, .T. ) ;
#6140 = CARTESIAN_POINT ( 'NONE',  ( 0.000000000000000000, -55.54999999966999980, -12.00000000000000000 ) ) ;
#6141 = DIRECTION ( 'NONE',  ( 4.529347781562982494E-09, -0.9999999999999983347, -5.940771729776980447E-08 ) ) ;
#6142 = CARTESIAN_POINT ( 'NONE',  ( 2.682229413215286851, -78.98086027728551528, -2.699476886104560158 ) ) ;
#6143 = ORIENTED_EDGE ( 'NONE', *, *, #25630, .F. ) ;
#6144 = CARTESIAN_POINT ( 'NONE',  ( -0.9151233253627000241, -78.19915960904749852, -0.9701162038759999495 ) ) ;
#6145 = CARTESIAN_POINT ( 'NONE',  ( 9.012516225103091472, -77.72930688072841576, -2.404885370045733772 ) ) ;
#6146 = VECTOR ( 'NONE', #19354, 1000.000000000000114 ) ;
#6147 = CARTESIAN_POINT ( 'NONE',  ( 0.6294848425788325263, -80.76745373571634445, -1.093351163505755341 ) ) ;
#6148 = ORIENTED_EDGE ( 'NONE', *, *, #38393, .F. ) ;
#6149 = CARTESIAN_POINT ( 'NONE',  ( -4.817132589604000259, -78.85146397087400771, -11.17039677886999982 ) ) ;
#6150 = AXIS2_PLACEMENT_3D ( 'NONE', #13127, #16420, #58011 ) ;
#6151 = CARTESIAN_POINT ( 'NONE',  ( 9.697372265369082811, -61.77233735005967219, -8.266620275728030265 ) ) ;
#6152 = EDGE_LOOP ( 'NONE', ( #45299, #47353, #24603 ) ) ;
#6153 = EDGE_CURVE ( 'NONE', #49275, #27979, #47954, .T. ) ;
#6154 = VERTEX_POINT ( 'NONE', #38194 ) ;
#6155 = CARTESIAN_POINT ( 'NONE',  ( -1.055666910258088231, -80.55513841626326155, 0.6698640694703560383 ) ) ;
#6156 = AXIS2_PLACEMENT_3D ( 'NONE', #18102, #40232, #41408 ) ;
#6157 = CARTESIAN_POINT ( 'NONE',  ( 3.140974612311327796, -79.65416666666664014, 11.68767212001979594 ) ) ;
#6158 = CARTESIAN_POINT ( 'NONE',  ( -7.479908383216000267, -79.44603908114399360, -6.281056869080000382 ) ) ;
#6159 = EDGE_LOOP ( 'NONE', ( #19027, #42909, #14269, #13943, #41729, #1093, #49408, #56851, #13957, #46261, #3889, #27054 ) ) ;
#6160 = CARTESIAN_POINT ( 'NONE',  ( 12.65989785476000051, -53.85665906507999523, 0.9744897697748999832 ) ) ;
#6161 = CARTESIAN_POINT ( 'NONE',  ( 7.610436523679670273, -23.52540704710936126, -10.41144397132592836 ) ) ;
#6162 = ORIENTED_EDGE ( 'NONE', *, *, #36908, .F. ) ;
#6163 = CARTESIAN_POINT ( 'NONE',  ( -12.61277705613999878, -23.19666672528000007, -1.798399175679999740 ) ) ;
#6164 = CARTESIAN_POINT ( 'NONE',  ( 4.897371265365999982, -76.84044415034598785, 7.847181321287999722 ) ) ;
#6165 = CARTESIAN_POINT ( 'NONE',  ( -0.3490198212478526907, -80.20286839885675079, -1.200175596027631908 ) ) ;
#6166 = CARTESIAN_POINT ( 'NONE',  ( 1.980584515756000030, -18.73514849905999924, -12.76303204340999997 ) ) ;
#6167 = CARTESIAN_POINT ( 'NONE',  ( 2.853743189566999534E-14, -82.00000000000000000, -10.34999999999597797 ) ) ;
#6168 = EDGE_CURVE ( 'NONE', #49068, #11615, #56213, .T. ) ;
#6169 = DIRECTION ( 'NONE',  ( -0.7026410690473250398, 0.1122098755728047209, 0.7026410690473250398 ) ) ;
#6170 = CARTESIAN_POINT ( 'NONE',  ( 0.5445062389433608097, -78.69549341983497470, 1.437445382695913487 ) ) ;
#6171 = DIRECTION ( 'NONE',  ( 0.000000000000000000, -1.000000000000000000, 0.000000000000000000 ) ) ;
#6172 = ADVANCED_FACE ( 'NONE', ( #25774 ), #53011, .F. ) ;
#6173 = CARTESIAN_POINT ( 'NONE',  ( 5.894077591580000330, -76.68206586006000691, -10.80721126921000064 ) ) ;
#6174 = CARTESIAN_POINT ( 'NONE',  ( 0.3280756968000912988, -1.981646559566586419, -3.506079728219933411 ) ) ;
#6175 = CARTESIAN_POINT ( 'NONE',  ( -13.86363625866319715, -9.638971321655001034, -0.001706075946107427034 ) ) ;
#6176 = CARTESIAN_POINT ( 'NONE',  ( -12.10179013622999911, -78.53027982294000253, -1.986401539992999954 ) ) ;
#6177 = CARTESIAN_POINT ( 'NONE',  ( 5.459501886381000091, -76.22776474484699349, -11.00074850082999767 ) ) ;
#6178 = CARTESIAN_POINT ( 'NONE',  ( 12.76303204517000012, -18.73514852243999940, -1.980584515753000208 ) ) ;
#6179 = CARTESIAN_POINT ( 'NONE',  ( 3.160362247288924564, -2.832624405079319452, -0.7606606948156037218 ) ) ;
#6180 = CARTESIAN_POINT ( 'NONE',  ( 2.319020911157693821, -77.90973430596969251, 11.89852370548304172 ) ) ;
#6181 = CARTESIAN_POINT ( 'NONE',  ( -7.408849624938999234, -79.31758544377551345, -8.421820339245000397 ) ) ;
#6182 = EDGE_CURVE ( 'NONE', #6658, #11325, #42218, .T. ) ;
#6183 = ORIENTED_EDGE ( 'NONE', *, *, #48931, .T. ) ;
#6184 = CARTESIAN_POINT ( 'NONE',  ( -1.357301787716079788, -81.28639619689411688, -0.6673137404722703225 ) ) ;
#6185 = CARTESIAN_POINT ( 'NONE',  ( 5.231719136747999599, -76.99948083835489854, -8.176838819753999843 ) ) ;
#6186 = CARTESIAN_POINT ( 'NONE',  ( 10.21026636380264740, -24.25606635949579371, 7.764233071689755405 ) ) ;
#6187 = CARTESIAN_POINT ( 'NONE',  ( 0.000000000000000000, -77.69999999999998863, 0.000000000000000000 ) ) ;
#6188 = CARTESIAN_POINT ( 'NONE',  ( 3.108770384767000294, -3.085385803691999662, -2.032239610727000212 ) ) ;
#6189 = CARTESIAN_POINT ( 'NONE',  ( 11.60231809276000092, -78.73711054799299802, -3.252995651540999678 ) ) ;
#6190 = CARTESIAN_POINT ( 'NONE',  ( -0.5568870975076999352, -77.89126107556998591, -9.723660445896001647 ) ) ;
#6192 = CARTESIAN_POINT ( 'NONE',  ( 10.28236248476030390, -76.80731616818275143, -6.022669235425634149 ) ) ;
#6191 = CARTESIAN_POINT ( 'NONE',  ( -7.980753701116782395, -76.13439855002184231, 8.624097217009085270 ) ) ;
#6193 = CARTESIAN_POINT ( 'NONE',  ( -0.5331523304941999664, -82.48730002504399295, 1.241660107034999960 ) ) ;
#6194 = CARTESIAN_POINT ( 'NONE',  ( 4.268285239867494418, -85.79678895079199208, 0.4899302694423579019 ) ) ;
#6195 = ORIENTED_EDGE ( 'NONE', *, *, #54364, .T. ) ;
#6196 = CARTESIAN_POINT ( 'NONE',  ( 10.04991969245749672, -76.75384563621365430, -6.584037273805950718 ) ) ;
#6197 = CARTESIAN_POINT ( 'NONE',  ( 9.008910651542503700, -77.87100497140035316, 2.420997400874941974 ) ) ;
#6198 = CARTESIAN_POINT ( 'NONE',  ( -3.075537641221531615, -76.90416666666666856, -11.44417895085270942 ) ) ;
#6199 = CARTESIAN_POINT ( 'NONE',  ( 6.083963560182000130, -78.66220947345499326, -9.135064530700001129 ) ) ;
#6200 = CYLINDRICAL_SURFACE ( 'NONE', #20452, 0.5000000000000006661 ) ;
#6201 = CARTESIAN_POINT ( 'NONE',  ( 5.642630579966001036, -79.46848277179400100, 7.853379265792000297 ) ) ;
#6202 = CARTESIAN_POINT ( 'NONE',  ( 10.52682159591000044, -18.57432398260000284, -7.605688676868000542 ) ) ;
#6203 = CARTESIAN_POINT ( 'NONE',  ( 0.000000000000000000, -63.10294702885996543, -12.53545825868000207 ) ) ;
#6204 = EDGE_LOOP ( 'NONE', ( #41155, #40324, #6266, #38099 ) ) ;
#6205 = CARTESIAN_POINT ( 'NONE',  ( 4.671862542492999815, -78.93563051119899399, -10.24732477002999964 ) ) ;
#6206 = CARTESIAN_POINT ( 'NONE',  ( 2.076511064785050653, -76.21002604798447067, 10.98936983701634418 ) ) ;
#6207 = CARTESIAN_POINT ( 'NONE',  ( 2.885036932590493652, -79.69456034571689429, -11.47827798692048873 ) ) ;
#6208 = LINE ( 'NONE', #47264, #32498 ) ;
#6209 = CARTESIAN_POINT ( 'NONE',  ( -11.89252178239981994, -77.93728225073550675, 2.372833624312832956 ) ) ;
#6210 = CARTESIAN_POINT ( 'NONE',  ( 0.9272193457273129047, -81.40918307165384249, 0.8400180975224862401 ) ) ;
#6211 = CARTESIAN_POINT ( 'NONE',  ( 0.7276880389500910429, -78.47687705635108557, 1.046751526124253262 ) ) ;
#6212 = CARTESIAN_POINT ( 'NONE',  ( -12.50000000000000000, -54.11762331445000029, -1.005384021965999963 ) ) ;
#6213 = CARTESIAN_POINT ( 'NONE',  ( 2.113064247614999669, -3.419836441412999584, -3.165785623842000351 ) ) ;
#6214 = EDGE_CURVE ( 'NONE', #40639, #56888, #21802, .T. ) ;
#6215 = CARTESIAN_POINT ( 'NONE',  ( -1.140778876102999995, -79.12070647882998742, -0.6399209788899999918 ) ) ;
#6216 = FACE_OUTER_BOUND ( 'NONE', #31158, .T. ) ;
#6217 = B_SPLINE_SURFACE_WITH_KNOTS ( 'NONE', 3, 3, ( 
 ( #43224, #44087, #35196, #3072, #57372, #16931, #7782, #30492, #11646, #8065, #38781, #30772, #53228, #34912, #52944, #44367, #12494, #52375, #48521, #56799, #34629, #3919, #26060, #21922, #3353, #7493, #29905, #47677, #3637, #16358, #34339, #21350, #30197, #56511, #11928, #25490, #47960, #52655, #39645, #43511, #39071, #16644, #39365, #12210, #29623, #48245, #57652, #17208, #45854, #49692, #49396, #35790, #31943, #9239, #27224, #22218, #8647, #13654, #44963, #8945, #40529, #49987, #31649, #44667, #14235, #4811, #13060 ),
 ( #27516, #4518, #17501, #414, #40822, #50275, #17804, #35490, #9823, #40229, #9532, #22520, #36383, #27807, #39931, #45557, #57947, #18100, #123, #58242, #53519, #53821, #31059, #54409, #36096, #5103, #23102, #41112, #13357, #26932, #54113, #49096, #18392, #45264, #26632, #703, #31355, #22811, #10707, #11285, #10997, #28098, #28981, #51445, #6256, #51736, #41989, #38130, #46147, #32520, #41406, #47022, #23682, #2141, #29264, #15702, #28684, #19265, #5966, #5672, #20143, #6552, #50564, #24561, #55862, #37256, #42578 ),
 ( #33407, #10118, #56153, #33696, #1854, #19849, #47312, #37843, #55268, #15414, #41695, #1557, #23394, #24270, #989, #46736, #32813, #14816, #14527, #42287, #50860, #10405, #33109, #55563, #18974, #28390, #46437, #23970, #19548, #36965, #37546, #15112, #51152, #54979, #11574, #35130, #3002, #12141, #34271, #12711, #16574, #16292, #2716, #39290, #34559, #52591, #29554, #33983, #39003, #11862, #52306, #7422, #16864, #57012, #47609, #21574, #30129, #38422, #7710, #53162, #7133, #52876, #29839, #42867, #25712, #48178, #7997 ),
 ( #47891, #56733, #43738, #25134, #30704, #20998, #3290, #25426, #6841, #21283, #43441, #20713, #57302, #34845, #12429, #43159, #52020, #30422, #48455, #25994, #44018, #3570, #39579, #38713, #57582, #17144, #56441, #24852, #2425, #20428, #15996, #13288, #26286, #9170, #49623, #23031, #18324, #54340, #53751, #8871, #41046, #635, #44893, #18617, #36019, #22445, #13879, #17433, #53448, #44300, #31281, #36606, #9463, #48740, #27152, #44594, #57876, #58169, #54629, #49323, #26563, #26865, #14166, #5029, #31874, #8284, #40751 ) ),
 .UNSPECIFIED., .F., .F., .F.,
 ( 4, 4 ),
 ( 4, 1, 1, 1, 1, 1, 1, 1, 1, 1, 1, 1, 1, 1, 1, 1, 1, 1, 1, 1, 1, 1, 1, 1, 1, 1, 1, 1, 1, 1, 1, 1, 1, 1, 1, 1, 1, 1, 1, 1, 1, 1, 1, 1, 1, 1, 1, 1, 1, 1, 1, 1, 1, 1, 1, 1, 1, 1, 1, 1, 1, 1, 1, 1, 4 ),
 ( -0.5168282991433000850, 1.516828299142999992 ),
 ( -0.02000000000000000042, -0.003749999999999999861, 0.01250000000000000069, 0.02875000000000000125, 0.04499999999999999833, 0.06124999999999999889, 0.07749999999999999944, 0.09375000000000000000, 0.1100000000000000006, 0.1262500000000000011, 0.1424999999999999878, 0.1587500000000000022, 0.1749999999999999889, 0.1912500000000000033, 0.2074999999999999900, 0.2237500000000000044, 0.2399999999999999911, 0.2562499999999999778, 0.2725000000000000200, 0.2887500000000000067, 0.3049999999999999933, 0.3212499999999999800, 0.3375000000000000222, 0.3537500000000000089, 0.3699999999999999956, 0.3862499999999999822, 0.4025000000000000244, 0.4187500000000000111, 0.4349999999999999978, 0.4512499999999999845, 0.4675000000000000266, 0.4837500000000000133, 0.5000000000000000000, 0.5162499999999999867, 0.5324999999999999734, 0.5487499999999999600, 0.5649999999999999467, 0.5812500000000000444, 0.5975000000000000311, 0.6137500000000000178, 0.6300000000000000044, 0.6462499999999999911, 0.6624999999999999778, 0.6787499999999999645, 0.6949999999999999512, 0.7112500000000000488, 0.7275000000000000355, 0.7437500000000000222, 0.7600000000000000089, 0.7762499999999999956, 0.7924999999999999822, 0.8087499999999999689, 0.8249999999999999556, 0.8412500000000000533, 0.8575000000000000400, 0.8737500000000000266, 0.8900000000000000133, 0.9062500000000000000, 0.9224999999999999867, 0.9387499999999999734, 0.9549999999999999600, 0.9712499999999999467, 0.9875000000000000444, 1.003749999999999920, 1.020000000000000018 ),
 .UNSPECIFIED. ) ;
#6218 = CARTESIAN_POINT ( 'NONE',  ( 10.62559031388325614, -78.18606552174667002, -1.896613003017499244 ) ) ;
#6219 = VECTOR ( 'NONE', #18548, 1000.000000000000000 ) ;
#6220 = DIRECTION ( 'NONE',  ( 0.7071067811865475727, 0.000000000000000000, 0.7071067811865475727 ) ) ;
#6221 = ORIENTED_EDGE ( 'NONE', *, *, #49369, .T. ) ;
#6222 = ORIENTED_EDGE ( 'NONE', *, *, #35877, .T. ) ;
#6223 = CARTESIAN_POINT ( 'NONE',  ( -0.8742025125545000996, -78.76128998579800111, 9.984153739810000872 ) ) ;
#6224 = CARTESIAN_POINT ( 'NONE',  ( 8.943349029703989927, -78.80334685903174829, -5.964646307384620094 ) ) ;
#6225 = ORIENTED_EDGE ( 'NONE', *, *, #2262, .F. ) ;
#6226 = CARTESIAN_POINT ( 'NONE',  ( 7.620037552712999762, -18.79433113555000290, 10.53559761427999852 ) ) ;
#6227 = CIRCLE ( 'NONE', #50588, 14.00000000000000000 ) ;
#6228 = CARTESIAN_POINT ( 'NONE',  ( -9.034604909256527705, -79.37471052910895253, 2.936440201109655312 ) ) ;
#6229 = CARTESIAN_POINT ( 'NONE',  ( 6.497627649074000367, -78.57347311384999955, 9.985601457511998902 ) ) ;
#6230 = CARTESIAN_POINT ( 'NONE',  ( 10.18948929999999997, -60.01532694310999716, 7.645397820753000673 ) ) ;
#6231 = CARTESIAN_POINT ( 'NONE',  ( 5.137083998358000336, -77.21100733245999947, -10.56753840748999984 ) ) ;
#6232 = CARTESIAN_POINT ( 'NONE',  ( 9.450616389032896691, -77.74723657863938797, -7.362461627428266375 ) ) ;
#6233 = CARTESIAN_POINT ( 'NONE',  ( -8.286771986066998608, -78.77504344720300367, 7.559597915363999832 ) ) ;
#6234 = VERTEX_POINT ( 'NONE', #18674 ) ;
#6235 = DIRECTION ( 'NONE',  ( 0.000000000000000000, 0.000000000000000000, 1.000000000000000000 ) ) ;
#6236 = ORIENTED_EDGE ( 'NONE', *, *, #6888, .F. ) ;
#6237 = ADVANCED_FACE ( 'NONE', ( #5953 ), #28085, .F. ) ;
#6238 = CARTESIAN_POINT ( 'NONE',  ( 9.097059317135745005, -77.36466295629431045, 1.675254618218271263 ) ) ;
#6239 = DIRECTION ( 'NONE',  ( 0.000000000000000000, 1.000000000000000000, -4.899618830983999950E-14 ) ) ;
#6240 = CARTESIAN_POINT ( 'NONE',  ( -1.049525737143000015, -77.56063687001267226, -1.227116502697000122 ) ) ;
#6241 = CARTESIAN_POINT ( 'NONE',  ( 0.000000000000000000, -75.15999999999999659, 0.000000000000000000 ) ) ;
#6242 = CARTESIAN_POINT ( 'NONE',  ( 11.68767212001979239, -78.62916666666666288, -3.140974612311342451 ) ) ;
#6243 = CARTESIAN_POINT ( 'NONE',  ( 0.4326115402657000342, -78.97601868546000503, -1.568920109259999807 ) ) ;
#6244 = CARTESIAN_POINT ( 'NONE',  ( -0.9428654619097610601, -79.15721871088541661, -0.8204702594945776362 ) ) ;
#6245 = CARTESIAN_POINT ( 'NONE',  ( -10.66249531825000041, -79.92128212740999516, 1.062579819291000094 ) ) ;
#6246 = LINE ( 'NONE', #47014, #56474 ) ;
#6247 = CARTESIAN_POINT ( 'NONE',  ( -7.619712170649999727, -23.40404510063000032, -10.35409959310000083 ) ) ;
#6248 = CARTESIAN_POINT ( 'NONE',  ( 7.156381309732353202, -79.10742710526332644, 6.276394420187332734 ) ) ;
#6249 = ADVANCED_FACE ( 'NONE', ( #45546 ), #19249, .T. ) ;
#6250 = CARTESIAN_POINT ( 'NONE',  ( 0.2488026545057999972, -85.10431426239898656, -3.538314140727000456 ) ) ;
#6251 = EDGE_LOOP ( 'NONE', ( #44053, #35015, #49209, #17164, #46921 ) ) ;
#6252 = CARTESIAN_POINT ( 'NONE',  ( -10.17160039975009767, -77.19999999999998863, 4.054394401284254101 ) ) ;
#6253 = CARTESIAN_POINT ( 'NONE',  ( 7.919595949288999570, -55.64999999965999677, -8.768124086712999699 ) ) ;
#6254 = CARTESIAN_POINT ( 'NONE',  ( 10.69076134079912777, -77.86011180829753187, 1.345938505392821005 ) ) ;
#6255 = ADVANCED_FACE ( 'NONE', ( #23669 ), #29402, .F. ) ;
#6256 = CARTESIAN_POINT ( 'NONE',  ( 9.450487096927000508, -77.83122730632099717, -7.362360902974999455 ) ) ;
#6257 = CARTESIAN_POINT ( 'NONE',  ( -9.929695104603000644, -17.36901065046999904, 7.973993995755001229 ) ) ;
#6258 = CARTESIAN_POINT ( 'NONE',  ( -0.2498055603741706487, -78.64068256608658203, 1.249787055701736316 ) ) ;
#6259 = CARTESIAN_POINT ( 'NONE',  ( -2.356642558701290024, -3.183365214057053194, 2.616017292610900657 ) ) ;
#6260 = CARTESIAN_POINT ( 'NONE',  ( 6.482950081930999531, -79.37695584965399576, -6.598019266050999754 ) ) ;
#6261 = CARTESIAN_POINT ( 'NONE',  ( 8.631984821280999753, -78.29653426492899371, -3.755001005681000148 ) ) ;
#6262 = CARTESIAN_POINT ( 'NONE',  ( 0.3965672376479022487, -85.94828561723799965, -8.852239448800926169 ) ) ;
#6263 = CARTESIAN_POINT ( 'NONE',  ( -7.675142533464999417, -78.39509280558399951, 7.924261572595001191 ) ) ;
#6264 = FACE_OUTER_BOUND ( 'NONE', #44535, .T. ) ;
#6265 = CARTESIAN_POINT ( 'NONE',  ( 5.403345834808000347, -80.29310691901919483, 9.610968446100999429 ) ) ;
#6266 = ORIENTED_EDGE ( 'NONE', *, *, #1740, .F. ) ;
#6267 = CARTESIAN_POINT ( 'NONE',  ( 0.2153359604882000011, -82.12775552825800673, 1.316133176457000120 ) ) ;
#6268 = CARTESIAN_POINT ( 'NONE',  ( -1.886823409074000146, -60.56319684329000097, -12.68610076208999971 ) ) ;
#6269 = CARTESIAN_POINT ( 'NONE',  ( 10.46898001190309735, -80.37101647696528062, 2.813233871471190195 ) ) ;
#6270 = CARTESIAN_POINT ( 'NONE',  ( 6.433795189870999742, -77.43971739268899057, -9.188274595716000803 ) ) ;
#6271 = CARTESIAN_POINT ( 'NONE',  ( -10.79326785783000098, -79.32407132642299530, -1.992331681952000055 ) ) ;
#6272 = CARTESIAN_POINT ( 'NONE',  ( 7.986976573804001056, -24.72634345633999686, -10.07613380457000041 ) ) ;
#6273 = CARTESIAN_POINT ( 'NONE',  ( 4.012235213810621204, -85.44479167924301066, -0.08669540122018622175 ) ) ;
#6274 = CARTESIAN_POINT ( 'NONE',  ( -12.12824626824999896, -76.58162878623900838, -0.7688881989071000289 ) ) ;
#6275 = DIRECTION ( 'NONE',  ( 0.000000000000000000, 0.000000000000000000, -1.000000000000000000 ) ) ;
#6276 = ORIENTED_EDGE ( 'NONE', *, *, #34608, .T. ) ;
#6277 = AXIS2_PLACEMENT_3D ( 'NONE', #19494, #29776, #47832 ) ;
#6278 = CARTESIAN_POINT ( 'NONE',  ( -0.6492849177312852715, -80.01898409060812867, 1.068617496498147856 ) ) ;
#6279 = EDGE_CURVE ( 'NONE', #46546, #9748, #45044, .T. ) ;
#6280 = CARTESIAN_POINT ( 'NONE',  ( -7.686918321215999939, -57.04439829094999936, 10.48771805383000100 ) ) ;
#6281 = CIRCLE ( 'NONE', #58100, 10.40000000000000036 ) ;
#6282 = VECTOR ( 'NONE', #14181, 1000.000000000000000 ) ;
#6283 = CARTESIAN_POINT ( 'NONE',  ( 7.758650587924000419, -54.64922688096000059, -9.996717134825001239 ) ) ;
#6284 = CIRCLE ( 'NONE', #11028, 11.00000000000000000 ) ;
#6285 = CARTESIAN_POINT ( 'NONE',  ( -10.91036644271999911, -76.79653003390299659, -2.792455208340000272 ) ) ;
#6286 = CARTESIAN_POINT ( 'NONE',  ( 0.2617232932829000047, -79.40796291402000406, -1.644907507304999905 ) ) ;
#6287 = CARTESIAN_POINT ( 'NONE',  ( -0.7581747471680000405, -78.94365927756000190, 1.080670598843999963 ) ) ;
#6288 = CARTESIAN_POINT ( 'NONE',  ( -7.374560639699022424, -77.72708333333333997, 9.596002108778135309 ) ) ;
#6289 = CARTESIAN_POINT ( 'NONE',  ( 1.205168758126570427, -81.44834290230591023, -0.9133787470919593199 ) ) ;
#6290 = VECTOR ( 'NONE', #43408, 1000.000000000000000 ) ;
#6291 = DIRECTION ( 'NONE',  ( 0.000000000000000000, -1.000000000000000000, 1.360822088842000019E-13 ) ) ;
#6292 = ORIENTED_EDGE ( 'NONE', *, *, #36664, .T. ) ;
#6293 = CARTESIAN_POINT ( 'NONE',  ( -7.601397897754999633, -18.75000000000000000, 9.369164850722000892 ) ) ;
#6294 = EDGE_CURVE ( 'NONE', #822, #39513, #52765, .T. ) ;
#6295 = CARTESIAN_POINT ( 'NONE',  ( 0.9994933351473022087, -80.90274815551298104, 0.7676091254557989574 ) ) ;
#6296 = ORIENTED_EDGE ( 'NONE', *, *, #38342, .T. ) ;
#6297 = EDGE_CURVE ( 'NONE', #47034, #33163, #19060, .T. ) ;
#6298 = CARTESIAN_POINT ( 'NONE',  ( 0.1446683541241534920, -81.73463977978825312, -1.242005837416781056 ) ) ;
#6299 = CARTESIAN_POINT ( 'NONE',  ( 10.32003611956000100, -80.18012082385709505, -3.898536120860000231 ) ) ;
#6300 = CARTESIAN_POINT ( 'NONE',  ( 6.002077433942410778, -78.07088160286059519, 7.255254208431503038 ) ) ;
#6301 = ORIENTED_EDGE ( 'NONE', *, *, #18720, .T. ) ;
#6302 = ORIENTED_EDGE ( 'NONE', *, *, #8905, .F. ) ;
#6303 = CARTESIAN_POINT ( 'NONE',  ( 1.072377845517999972, -81.85979603464500087, 1.071889744314999948 ) ) ;
#6304 = ORIENTED_EDGE ( 'NONE', *, *, #15217, .F. ) ;
#6305 = ORIENTED_EDGE ( 'NONE', *, *, #40249, .T. ) ;
#6306 = CARTESIAN_POINT ( 'NONE',  ( -1.288488638074000159, -17.46435060632000003, 12.54709296483000003 ) ) ;
#6307 = DIRECTION ( 'NONE',  ( 1.000000000000000000, 0.000000000000000000, 0.000000000000000000 ) ) ;
#6308 = APPLICATION_PROTOCOL_DEFINITION ( 'draft international standard', 'automotive_design', 1998, #42101 ) ;
#6309 = FACE_OUTER_BOUND ( 'NONE', #54453, .T. ) ;
#6310 = CARTESIAN_POINT ( 'NONE',  ( 12.00000000000000888, -76.53958333333119413, -1.570796326794872577 ) ) ;
#6311 = CARTESIAN_POINT ( 'NONE',  ( 5.769691659566330344, -78.27875186636556748, -7.231031389465585768 ) ) ;
#6312 = CYLINDRICAL_SURFACE ( 'NONE', #30696, 11.75000000000000000 ) ;
#6313 = EDGE_LOOP ( 'NONE', ( #57135, #7382, #12668, #33373, #9623, #7992, #52043 ) ) ;
#6314 = ORIENTED_EDGE ( 'NONE', *, *, #18893, .T. ) ;
#6315 = CARTESIAN_POINT ( 'NONE',  ( 0.000000000000000000, -80.79999999999999716, 0.000000000000000000 ) ) ;
#6316 = DIRECTION ( 'NONE',  ( 0.000000000000000000, 1.000000000000000000, 0.000000000000000000 ) ) ;
#6317 = CARTESIAN_POINT ( 'NONE',  ( 1.217465845835393967, -81.27083333333332860, 0.3271848554491025851 ) ) ;
#6318 = AXIS2_PLACEMENT_3D ( 'NONE', #31785, #31488, #35930 ) ;
#6319 = CARTESIAN_POINT ( 'NONE',  ( 1.003693376153260264, -61.76223992066808677, -12.70247752669052232 ) ) ;
#6320 = CARTESIAN_POINT ( 'NONE',  ( -8.680270256945998852, -77.17624500592239656, 3.860428508128000313 ) ) ;
#6321 = LINE ( 'NONE', #1621, #30356 ) ;
#6322 = CARTESIAN_POINT ( 'NONE',  ( -0.6295237254636286695, -79.91666666666665719, 1.092232985442819881 ) ) ;
#6323 = AXIS2_PLACEMENT_3D ( 'NONE', #56364, #33617, #24481 ) ;
#6324 = CARTESIAN_POINT ( 'NONE',  ( 7.000000000000000000, -81.19999999999998863, 0.000000000000000000 ) ) ;
#6325 = CARTESIAN_POINT ( 'NONE',  ( -1.321122997307999869, -79.66002549588999671, 0.8769429413327000100 ) ) ;
#6326 = FACE_OUTER_BOUND ( 'NONE', #32501, .T. ) ;
#6327 = AXIS2_PLACEMENT_3D ( 'NONE', #56218, #56795, #6618 ) ;
#6328 = CARTESIAN_POINT ( 'NONE',  ( -2.943907793430999842, -81.49317640407899432, 2.956342729591999952 ) ) ;
#6329 = CONICAL_SURFACE ( 'NONE', #58199, 8.899999998586000771, 0.7853981633972997312 ) ;
#6330 = CARTESIAN_POINT ( 'NONE',  ( -10.47513558171999826, -54.99636614397000045, 7.624778817986999968 ) ) ;
#6331 = CARTESIAN_POINT ( 'NONE',  ( -7.575359187103000380, -78.51711001420200375, 6.037810896484000267 ) ) ;
#6332 = CARTESIAN_POINT ( 'NONE',  ( -1.750000000001000089, -18.75000001325000198, -12.56594318051000059 ) ) ;
#6333 = DIRECTION ( 'NONE',  ( -2.708260965908999685E-12, 1.000000000000000000, -1.232643895471000067E-11 ) ) ;
#6335 = CARTESIAN_POINT ( 'NONE',  ( 0.5704417986824000808, -78.92583314235599801, -1.205475954488999912 ) ) ;
#6334 = LINE ( 'NONE', #2215, #39150 ) ;
#6336 = LINE ( 'NONE', #56229, #18558 ) ;
#6337 = FACE_OUTER_BOUND ( 'NONE', #52329, .T. ) ;
#6338 = FACE_OUTER_BOUND ( 'NONE', #6898, .T. ) ;
#6339 = CARTESIAN_POINT ( 'NONE',  ( 1.388126973326925473, -1.594193359475267524, 3.339128716332707469 ) ) ;
#6340 = EDGE_LOOP ( 'NONE', ( #49186, #39748, #38658, #23948 ) ) ;
#6341 = CARTESIAN_POINT ( 'NONE',  ( -0.2306306439467533664, -3.500000000000000000, -3.452531048248814294 ) ) ;
#6342 = DIRECTION ( 'NONE',  ( 0.000000000000000000, 0.000000000000000000, -1.000000000000000000 ) ) ;
#6343 = CARTESIAN_POINT ( 'NONE',  ( 3.077551880085030778, -77.55205857829017191, 11.44362783114953253 ) ) ;
#6344 = CARTESIAN_POINT ( 'NONE',  ( -0.004472651058881748666, -78.47550862917535142, 1.249857563130390981 ) ) ;
#6345 = CARTESIAN_POINT ( 'NONE',  ( 5.288697200961000711, -79.56426011353597971, -8.062752175145998734 ) ) ;
#6346 = CARTESIAN_POINT ( 'NONE',  ( 11.88928085110999966, -78.23131299228001012, 5.289737169833999886 ) ) ;
#6347 = CARTESIAN_POINT ( 'NONE',  ( -0.4536591235910606423, -79.47852630003501417, 10.74087249166092306 ) ) ;
#6348 = EDGE_CURVE ( 'NONE', #45667, #15896, #16228, .T. ) ;
#6349 = CARTESIAN_POINT ( 'NONE',  ( 8.557689913033998508, -79.23271332859899019, 4.648766890461000223 ) ) ;
#6350 = DIRECTION ( 'NONE',  ( -0.9999999999995751176, 0.000000000000000000, -9.217554819261769351E-07 ) ) ;
#6351 = EDGE_CURVE ( 'NONE', #13102, #43717, #11559, .T. ) ;
#6352 = CARTESIAN_POINT ( 'NONE',  ( -2.029340489805000036, -77.13260634160660345, 10.97939916177999997 ) ) ;
#6353 = CARTESIAN_POINT ( 'NONE',  ( -0.1369841977586999937, -81.02625324414100305, -1.598267016032999921 ) ) ;
#6354 = CARTESIAN_POINT ( 'NONE',  ( 1.899930039692999895, -78.50934514476064408, 9.535935523283001203 ) ) ;
#6356 = CARTESIAN_POINT ( 'NONE',  ( 0.000000000000000000, -82.09999999999999432, 0.000000000000000000 ) ) ;
#6355 = CARTESIAN_POINT ( 'NONE',  ( 1.142167996899000171, -83.34403886695498898, -3.578662123773000303 ) ) ;
#6357 = CARTESIAN_POINT ( 'NONE',  ( 8.395992668097999712, -79.47975584965399776, 4.560928606276999808 ) ) ;
#6358 = LINE ( 'NONE', #41795, #37424 ) ;
#6359 = CARTESIAN_POINT ( 'NONE',  ( 4.692082659980980175, -80.26118559034645727, -9.672370880052689301 ) ) ;
#6360 = AXIS2_PLACEMENT_3D ( 'NONE', #27352, #28212, #5502 ) ;
#6361 = CARTESIAN_POINT ( 'NONE',  ( -6.926502605637190335, -77.16933908148428145, -8.221045740255387813 ) ) ;
#6362 = CARTESIAN_POINT ( 'NONE',  ( -2.486604901413195901, -77.29583333333334849, 9.252740428348989354 ) ) ;
#6363 = EDGE_LOOP ( 'NONE', ( #7478, #53760, #28858 ) ) ;
#6365 = EDGE_CURVE ( 'NONE', #15288, #47432, #40856, .T. ) ;
#6364 = VERTEX_POINT ( 'NONE', #23087 ) ;
#6366 = CARTESIAN_POINT ( 'NONE',  ( -3.970056213021999625, -79.03565890873500166, 11.35542513096999961 ) ) ;
#6367 = DIRECTION ( 'NONE',  ( 0.000000000000000000, 0.000000000000000000, 1.000000000000000000 ) ) ;
#6368 = LINE ( 'NONE', #42975, #35981 ) ;
#6369 = VECTOR ( 'NONE', #6442, 1000.000000000000000 ) ;
#6370 = ORIENTED_EDGE ( 'NONE', *, *, #57467, .F. ) ;
#6371 = CARTESIAN_POINT ( 'NONE',  ( 10.38571723084000098, -77.33241475543599108, -5.879822389739000066 ) ) ;
#6372 = VECTOR ( 'NONE', #38567, 1000.000000000000000 ) ;
#6373 = ORIENTED_EDGE ( 'NONE', *, *, #35099, .T. ) ;
#6374 = ORIENTED_EDGE ( 'NONE', *, *, #14831, .T. ) ;
#6375 = AXIS2_PLACEMENT_3D ( 'NONE', #48406, #7943, #18279 ) ;
#6376 = EDGE_LOOP ( 'NONE', ( #18160, #56694, #21293, #30665 ) ) ;
#6377 = CARTESIAN_POINT ( 'NONE',  ( -1.281711091423999971, -78.97418298445228402, -3.307376133738999968 ) ) ;
#6378 = CARTESIAN_POINT ( 'NONE',  ( 7.552177422520572669, -79.20153084570749513, 5.764790892576884929 ) ) ;
#6379 = ADVANCED_FACE ( 'NONE', ( #29827 ), #49261, .T. ) ;
#6380 = ORIENTED_EDGE ( 'NONE', *, *, #48957, .F. ) ;
#6381 = CARTESIAN_POINT ( 'NONE',  ( -10.48771805367000098, -57.04439828530000511, -7.686918321054999836 ) ) ;
#6382 = DIRECTION ( 'NONE',  ( 0.000000000000000000, -1.000000000000000000, 3.788556036780999566E-11 ) ) ;
#6383 = ORIENTED_EDGE ( 'NONE', *, *, #12073, .F. ) ;
#6384 = CARTESIAN_POINT ( 'NONE',  ( 3.561977969011698608, -79.25638847529646114, -8.599364659723994109 ) ) ;
#6385 = CARTESIAN_POINT ( 'NONE',  ( 0.9916361112363957231, -78.06929481599125609, 1.169919221591249503 ) ) ;
#6386 = CARTESIAN_POINT ( 'NONE',  ( 10.90226209911854127, -79.80000000000003979, 4.526743382750034961 ) ) ;
#6387 = CARTESIAN_POINT ( 'NONE',  ( -12.50239399164999909, -17.31640749886000208, 1.003653729363000124 ) ) ;
#6388 = DIRECTION ( 'NONE',  ( 1.000000000000000000, 0.000000000000000000, 0.000000000000000000 ) ) ;
#6389 = CARTESIAN_POINT ( 'NONE',  ( -9.702231720816998362, -78.75158664270975351, -0.1934140619087000024 ) ) ;
#6390 = CARTESIAN_POINT ( 'NONE',  ( 7.778176538613999824, -76.45230952192000018, -8.035785801754000701 ) ) ;
#6391 = CARTESIAN_POINT ( 'NONE',  ( 2.935661446561999899, -79.99999999999998579, -9.035036904803998681 ) ) ;
#6392 = CYLINDRICAL_SURFACE ( 'NONE', #1454, 14.00000000000000000 ) ;
#6393 = CARTESIAN_POINT ( 'NONE',  ( -5.027353609631000531, -76.73535067984099101, 10.04038870902000014 ) ) ;
#6394 = CARTESIAN_POINT ( 'NONE',  ( -6.420806408779561103, -78.66401051080144669, -6.658731949244796056 ) ) ;
#6395 = CARTESIAN_POINT ( 'NONE',  ( 8.313499432590312210, -76.51190516819144705, 8.303026597870685421 ) ) ;
#6396 = CARTESIAN_POINT ( 'NONE',  ( -0.4872545538094000261, -79.31712366827299832, -1.241463230931000084 ) ) ;
#6397 = CARTESIAN_POINT ( 'NONE',  ( -7.554596112399141639, -80.16517684970969526, -7.995309787463595441 ) ) ;
#6398 = CARTESIAN_POINT ( 'NONE',  ( 0.000000000000000000, -82.25000000001401190, 0.000000000000000000 ) ) ;
#6399 = CARTESIAN_POINT ( 'NONE',  ( -3.218396486835000125, -80.12117549782598758, -1.589233011689999975 ) ) ;
#6400 = CARTESIAN_POINT ( 'NONE',  ( -8.246369313880999030, -79.51135969142900706, 8.832712023146999769 ) ) ;
#6401 = CARTESIAN_POINT ( 'NONE',  ( -8.746972750979978173, -78.05079177105272947, 6.251516341120114006 ) ) ;
#6402 = CARTESIAN_POINT ( 'NONE',  ( 0.9188661267636154539, -82.90988150905879195, 0.8478900103341754368 ) ) ;
#6403 = CARTESIAN_POINT ( 'NONE',  ( -13.63885489310999510, -59.58578169018998949, 7.254376133916000668 ) ) ;
#6404 = DIRECTION ( 'NONE',  ( 0.000000000000000000, -1.000000000000000000, 0.000000000000000000 ) ) ;
#6405 = CARTESIAN_POINT ( 'NONE',  ( 0.6295237254636211199, -80.33333333333334281, 1.092232985442824322 ) ) ;
#6406 = CARTESIAN_POINT ( 'NONE',  ( 10.35747145892000098, -18.68415268018999953, 7.626500777237000150 ) ) ;
#6407 = B_SPLINE_SURFACE_WITH_KNOTS ( 'NONE', 3, 3, ( 
 ( #21197, #39198, #31194, #49234 ),
 ( #26776, #4357, #44806, #22359 ),
 ( #17942, #58380, #48093, #7624 ),
 ( #43648, #57213, #16780, #21488 ),
 ( #34762, #52788, #12343, #7910 ),
 ( #3483, #39495, #14663, #40965 ),
 ( #5522, #41543, #45408, #36526 ),
 ( #35933, #9084, #53962, #32374 ),
 ( #27070, #23530, #50415, #13790 ),
 ( #4949, #19113, #54548, #13499 ),
 ( #23821, #5815, #14089, #9670 ) ),
 .UNSPECIFIED., .F., .F., .F.,
 ( 4, 1, 1, 1, 1, 1, 1, 1, 4 ),
 ( 4, 4 ),
 ( -0.01994574723509000280, 0.000000000000000000, 0.1666666666667000196, 0.3333333333333000081, 0.5000000000000000000, 0.6666666666667000474, 0.8333333333333000637, 1.000000000000000000, 1.020511277925000071 ),
 ( -0.3582002740325999635, 1.358574366096999997 ),
 .UNSPECIFIED. ) ;
#6408 = CARTESIAN_POINT ( 'NONE',  ( -9.992017125402000488, -60.96084086979999483, -7.762968460695000239 ) ) ;
#6409 = CARTESIAN_POINT ( 'NONE',  ( -1.210642416637526475, -79.71502597872630247, -9.250941057579437299 ) ) ;
#6410 = AXIS2_PLACEMENT_3D ( 'NONE', #4773, #22184, #44333 ) ;
#6411 = CARTESIAN_POINT ( 'NONE',  ( -0.8218343019581000330, -80.70650526761399135, -1.050237832603999832 ) ) ;
#6412 = CARTESIAN_POINT ( 'NONE',  ( 12.50686284812396210, -54.49510763085826426, 1.423064270604161630 ) ) ;
#6414 = CARTESIAN_POINT ( 'NONE',  ( 12.77562710766000009, -25.26233677660999888, 0.5428386295906000303 ) ) ;
#6413 = B_SPLINE_CURVE_WITH_KNOTS ( 'NONE', 3,
 ( #33206, #42091, #52405, #6944, #57404, #34081, #20807, #21383, #34659, #24948 ),
 .UNSPECIFIED., .F., .F.,
 ( 4, 2, 2, 2, 4 ),
 ( 0.000000000000000000, 0.1249999656550738053, 0.2499999313101476106, 0.3749998969652214020, 0.4999998626202952212 ),
 .UNSPECIFIED. ) ;
#6415 = CARTESIAN_POINT ( 'NONE',  ( -10.26045602449772964, -77.92435585664894404, 3.486900230140368873 ) ) ;
#6416 = SURFACE_STYLE_FILL_AREA ( #10867 ) ;
#6417 = CARTESIAN_POINT ( 'NONE',  ( 0.1291013223160000223, -79.22406349496543498, 10.97485077030000333 ) ) ;
#6418 = CARTESIAN_POINT ( 'NONE',  ( 6.478953145441000316, -76.08549705920000861, 10.17405887424000177 ) ) ;
#6419 = ORIENTED_EDGE ( 'NONE', *, *, #51017, .F. ) ;
#6420 = CARTESIAN_POINT ( 'NONE',  ( -3.776500157906000243, -86.47871544543099276, 0.4129270166134999531 ) ) ;
#6421 = CARTESIAN_POINT ( 'NONE',  ( -1.632746748298000039, -81.09541249912808780, 11.17026117058999901 ) ) ;
#6422 = CARTESIAN_POINT ( 'NONE',  ( 7.537139175769687505, -78.30095851910974147, -5.362098310969546588 ) ) ;
#6423 = DIRECTION ( 'NONE',  ( 0.000000000000000000, -1.000000000000000000, 0.000000000000000000 ) ) ;
#6424 = CARTESIAN_POINT ( 'NONE',  ( -10.54491486739000017, -77.92936695826499260, -3.823987582478999947 ) ) ;
#6425 = CARTESIAN_POINT ( 'NONE',  ( 12.54715396797999993, -54.26815137240999576, -1.292200816717000045 ) ) ;
#6426 = CARTESIAN_POINT ( 'NONE',  ( 9.164371241867000251, -77.55170024541499174, -3.297574176498999865 ) ) ;
#6427 = CARTESIAN_POINT ( 'NONE',  ( 0.7076411874954000591, -83.04873640444098726, -1.508144869335000138 ) ) ;
#6428 = FACE_OUTER_BOUND ( 'NONE', #15461, .T. ) ;
#6429 = CARTESIAN_POINT ( 'NONE',  ( -1.158153954042000056, -79.93059372536998808, 1.125119257983999921 ) ) ;
#6430 = ORIENTED_EDGE ( 'NONE', *, *, #7238, .F. ) ;
#6431 = CARTESIAN_POINT ( 'NONE',  ( -7.919595949288999570, -59.94999999040999938, 9.050966798898000931 ) ) ;
#6432 = DIRECTION ( 'NONE',  ( 0.000000000000000000, 0.000000000000000000, -1.000000000000000000 ) ) ;
#6433 = CARTESIAN_POINT ( 'NONE',  ( 2.592083719635297712, -78.97662554493233245, -2.800471138597825149 ) ) ;
#6434 = ORIENTED_EDGE ( 'NONE', *, *, #55014, .F. ) ;
#6435 = ADVANCED_FACE ( 'NONE', ( #25413 ), #48164, .F. ) ;
#6436 = CARTESIAN_POINT ( 'NONE',  ( 0.8912423865758999364, -77.99487050972069824, 0.9921004264782997684 ) ) ;
#6437 = CARTESIAN_POINT ( 'NONE',  ( 12.83044027763000017, -60.10639784916000394, 2.062670899361999766 ) ) ;
#6438 = CARTESIAN_POINT ( 'NONE',  ( -7.369179516270000008, -79.74914082875798726, -8.897431359219000413 ) ) ;
#6439 = ORIENTED_EDGE ( 'NONE', *, *, #36346, .F. ) ;
#6440 = CARTESIAN_POINT ( 'NONE',  ( 1.659836960048000076, -79.12275712511198833, 11.81542141165000004 ) ) ;
#6441 = CARTESIAN_POINT ( 'NONE',  ( -4.507968364102000081, -77.46452504304699005, 10.38607047735999878 ) ) ;
#6442 = DIRECTION ( 'NONE',  ( -1.776356839400000238E-14, -1.000000000000000000, 3.019806626979999679E-13 ) ) ;
#6443 = ORIENTED_EDGE ( 'NONE', *, *, #49719, .F. ) ;
#6444 = CARTESIAN_POINT ( 'NONE',  ( -0.6282371225189693487, -80.51721610571219401, 1.080583994657213998 ) ) ;
#6445 = B_SPLINE_CURVE_WITH_KNOTS ( 'NONE', 3,
 ( #14651, #37383, #14944, #50985, #28519, #42121, #28811, #1687, #46859, #34972, #15832, #16125, #11989, #30551, #42996, #12553, #57140, #7551, #43569, #21123, #16705, #34103, #52716, #48017, #25550, #2553, #47443, #12269, #29678, #20554, #30258, #24974, #48583, #11704, #26129, #3133, #51858, #39128, #8128, #34687, #44150, #47728, #38550, #56565, #56282, #53002, #11413, #16415, #39424, #43282, #16991, #52144, #57430, #7263, #29967, #29393, #33819, #20267, #38259, #6971, #25264, #2837, #7837, #20833, #38840, #48298, #3414, #25839, #56857, #43866, #21414, #12869, #3733, #35294, #3447, #21453, #39741, #39460, #20874, #57464, #52184, #53042, #38877, #20594, #21734, #11740, #57751, #53324, #48619, #3170, #56606, #30004, #34144, #30872, #43034, #17308, #7874, #26168, #17025, #48907, #38591, #16454, #52752, #29717, #25013, #21160, #30296, #52465, #2596, #34722, #34436, #56897, #35009, #12306, #48335, #47765, #7300, #12589, #12024, #25302, #30588, #8166, #16166 ),
 .UNSPECIFIED., .F., .F.,
 ( 4, 2, 1, 2, 2, 1, 2, 2, 2, 2, 1, 2, 2, 1, 1, 1, 2, 2, 2, 2, 2, 2, 2, 2, 2, 2, 2, 2, 1, 1, 1, 2, 2, 2, 2, 1, 1, 1, 1, 2, 2, 2, 2, 2, 2, 2, 2, 2, 2, 1, 1, 2, 2, 2, 2, 2, 2, 1, 1, 2, 2, 2, 1, 2, 2, 1, 1, 1, 2, 2, 2, 4 ),
 ( 0.000000000000000000, 0.06250000000001762479, 0.07031250000001984524, 0.07128906250002013667, 0.07226562500002041423, 0.07421875000002099709, 0.07812500000002214895, 0.09375000000002668699, 0.1250000000000358602, 0.1406250000000404121, 0.1425781250000410227, 0.1428222656250410227, 0.1430664062500410505, 0.1435546875000410227, 0.1445312500000409672, 0.1484375000000408562, 0.1562500000000406342, 0.1875000000000399125, 0.2500000000000383582, 0.2812500000000378031, 0.2851562500000378031, 0.2890625000000377476, 0.2968750000000377476, 0.3125000000000378031, 0.3750000000000384137, 0.3906250000000385803, 0.3925781250000386358, 0.3930664062500386913, 0.3935546875000386913, 0.3945312500000385803, 0.3984375000000378031, 0.4062500000000363043, 0.4375000000000301426, 0.4687500000000240363, 0.4843750000000209832, 0.4921875000000193734, 0.4960937500000185407, 0.4980468750000181521, 0.4990234375000179301, 0.4995117187500178746, 0.5000000000000177636, 0.5625000000000000000, 0.5703124999999977796, 0.5781249999999954481, 0.5937499999999908962, 0.6249999999999816813, 0.6406249999999771294, 0.6425781249999765743, 0.6435546874999763522, 0.6445312499999760192, 0.6484374999999749090, 0.6562499999999727995, 0.6874999999999640288, 0.7499999999999467093, 0.7812499999999379385, 0.7851562499999369393, 0.7871093749999364952, 0.7890624999999360512, 0.7968749999999341638, 0.8124999999999303890, 0.8749999999999151790, 0.8906249999999114042, 0.8925781249999109601, 0.8928222656249110711, 0.8930664062499110711, 0.8935546874999115152, 0.8945312499999122924, 0.8984374999999158451, 0.9062499999999222844, 0.9374999999999481526, 0.9687499999999741318, 1.000000000000000000 ),
 .UNSPECIFIED. ) ;
#6446 = CARTESIAN_POINT ( 'NONE',  ( 8.540261029602000065, -76.91613998579799727, 4.257270096473000365 ) ) ;
#6447 = CARTESIAN_POINT ( 'NONE',  ( 9.202039358297998461, -80.51999609317051920, 2.360608321670000453 ) ) ;
#6448 = EDGE_CURVE ( 'NONE', #54221, #5425, #51183, .T. ) ;
#6449 = EDGE_LOOP ( 'NONE', ( #1746, #16754, #44944 ) ) ;
#6450 = CARTESIAN_POINT ( 'NONE',  ( -3.163647801558190586, -2.580206749503648922, 0.8517472837491544269 ) ) ;
#6451 = CARTESIAN_POINT ( 'NONE',  ( 10.91653581620999880, -78.32390417293299834, 0.06787400445098999702 ) ) ;
#6452 = EDGE_LOOP ( 'NONE', ( #14409, #27788, #21595 ) ) ;
#6453 = CARTESIAN_POINT ( 'NONE',  ( -12.77562710766000009, -25.26233677660999888, -0.5428386295906000303 ) ) ;
#6454 = CARTESIAN_POINT ( 'NONE',  ( 3.399999999999724576, -78.69999999999998863, -2.006589542798634440 ) ) ;
#6455 = DIRECTION ( 'NONE',  ( 0.000000000000000000, 1.000000000000000000, 0.000000000000000000 ) ) ;
#6456 = LINE ( 'NONE', #46930, #44004 ) ;
#6457 = CARTESIAN_POINT ( 'NONE',  ( -1.583004792629327806, -17.54790758840184139, -12.70616254410899515 ) ) ;
#6458 = B_SPLINE_CURVE_WITH_KNOTS ( 'NONE', 3,
 ( #18405, #13960, #1283, #45865, #36688, #50000, #9546, #54424, #27529, #54703, #55281, #54991, #13666, #14540, #31662, #23407, #32533, #36978, #4825, #4533, #5685, #36396, #40834, #138, #27819, #54125, #27237, #18694, #41122, #26945, #45571, #5118, #428, #23114, #41417 ),
 .UNSPECIFIED., .F., .F.,
 ( 4, 1, 1, 1, 1, 1, 1, 1, 1, 1, 1, 1, 1, 1, 1, 1, 1, 1, 1, 1, 1, 1, 1, 1, 1, 1, 1, 1, 1, 1, 1, 1, 4 ),
 ( 0.000000000000000000, 0.01250096958943576128, 0.04500090495504436433, 0.07750084032066266448, 0.1100007756862671354, 0.1425007110518439757, 0.1750006464174760634, 0.2075005817831081512, 0.2400005171487402389, 0.2725004525143723266, 0.3050003878800044421, 0.3375003232454983904, 0.3700002586111305614, 0.4025001939767626213, 0.4350001293423947368, 0.4675000647080267968, 0.5000000000736588568, 0.5324999354391528605, 0.5649998708047848650, 0.5974998061704170915, 0.6299997415360490960, 0.6624996769016813225, 0.6949996122673132160, 0.7274995476329454425, 0.7599994829984393352, 0.7924994183640715617, 0.8249993537297034552, 0.8574992890953355706, 0.8899992244609679082, 0.9224991598265999126, 0.9549990951922320281, 0.9874990305577258098, 1.000000000000000000 ),
 .UNSPECIFIED. ) ;
#6459 = CARTESIAN_POINT ( 'NONE',  ( -5.601841361836865651, -77.97297913613843434, 7.949357391288894625 ) ) ;
#6460 = CARTESIAN_POINT ( 'NONE',  ( -9.380723093181000394, -77.11069873435108946, 0.6187074708012999524 ) ) ;
#6461 = CARTESIAN_POINT ( 'NONE',  ( 0.7804427332109117321, -79.01673782036979787, -1.323298261115681385 ) ) ;
#6462 = CARTESIAN_POINT ( 'NONE',  ( -1.615392861586334883, -81.97604168214044762, -3.673578837756669824 ) ) ;
#6463 = CARTESIAN_POINT ( 'NONE',  ( 12.17088485526999975, -75.74463960549999797, 1.845041276493999849 ) ) ;
#6464 = CARTESIAN_POINT ( 'NONE',  ( -0.6744830649036911430, -82.23641784909204944, -1.051876958025935949 ) ) ;
#6465 = ADVANCED_FACE ( 'NONE', ( #29253 ), #27588, .F. ) ;
#6466 = DIRECTION ( 'NONE',  ( -1.000000000000000000, 0.000000000000000000, 0.000000000000000000 ) ) ;
#6467 = CARTESIAN_POINT ( 'NONE',  ( 9.788011744299998540, -61.32881292732000134, -7.956359616248999345 ) ) ;
#6468 = CARTESIAN_POINT ( 'NONE',  ( 11.93255069029000026, -79.17946444151000662, -2.830763026309000008 ) ) ;
#6469 = CARTESIAN_POINT ( 'NONE',  ( -6.018890980713000438, -76.04965686829399374, 10.70471907396000155 ) ) ;
#6470 = PLANE ( 'NONE',  #31757 ) ;
#6471 = CARTESIAN_POINT ( 'NONE',  ( 1.614622833403325686, -2.767753323799579501, -2.821287581134315658 ) ) ;
#6472 = CARTESIAN_POINT ( 'NONE',  ( 0.9078743877195619705, -78.18103102862099263, -12.03646258193789897 ) ) ;
#6473 = CARTESIAN_POINT ( 'NONE',  ( 7.808618912244999599, -78.93627664175009784, -8.052551227705000869 ) ) ;
#6474 = B_SPLINE_SURFACE_WITH_KNOTS ( 'NONE', 3, 3, ( 
 ( #12840, #34402, #30556, #48587, #44434, #35562, #17273, #35263, #53588, #53294, #16709, #29971, #48022, #44154, #25554, #39709, #34691, #3701, #48302, #12273, #30262, #57716, #25843, #3420, #21704, #30840, #48874, #21419, #8415, #26413, #3987, #21989, #39998, #17573, #31122 ),
 ( #45033, #9302, #18456, #31423, #23454, #193, #45329, #45916, #767, #49466, #41466, #14298, #9889, #9596, #14011, #5165, #36447, #18744, #54476, #26999, #27292, #27869, #32584, #50633, #19036, #53891, #4879, #4585, #46211, #22585, #18168, #58311, #55043, #40598, #54753 ),
 ( #14592, #10182, #32008, #28160, #27582, #9013, #22876, #36161, #50338, #17873, #49763, #31715, #54181, #1052, #40885, #35863, #23165, #477, #50050, #13718, #32292, #5451, #22285, #45625, #41174, #13422, #36737, #37029, #40302, #21705, #21421, #22586, #12559, #40599, #36162 ),
 ( #30557, #44156, #35563, #58013, #17574, #26135, #49161, #3988, #21990, #58312, #16997, #12841, #17274, #53589, #48588, #54182, #57436, #13719, #39999, #39710, #44435, #3702, #49764, #31716, #13128, #31124, #8134, #53007, #8714, #30841, #53295, #26414, #43871, #48875, #40303 ) ),
 .UNSPECIFIED., .F., .F., .F.,
 ( 4, 4 ),
 ( 4, 1, 1, 1, 1, 1, 1, 1, 1, 1, 1, 1, 1, 1, 1, 1, 1, 1, 1, 1, 1, 1, 1, 1, 1, 1, 1, 1, 1, 1, 1, 1, 4 ),
 ( -0.3708084972812999980, 1.370808497280999960 ),
 ( -0.02000000000000000042, 0.01250000000000000069, 0.04499999999999999833, 0.07749999999999999944, 0.1100000000000000006, 0.1424999999999999878, 0.1749999999999999889, 0.2074999999999999900, 0.2399999999999999911, 0.2725000000000000200, 0.3049999999999999933, 0.3375000000000000222, 0.3699999999999999956, 0.4025000000000000244, 0.4349999999999999978, 0.4675000000000000266, 0.5000000000000000000, 0.5324999999999999734, 0.5649999999999999467, 0.5975000000000000311, 0.6300000000000000044, 0.6624999999999999778, 0.6949999999999999512, 0.7275000000000000355, 0.7600000000000000089, 0.7924999999999999822, 0.8249999999999999556, 0.8575000000000000400, 0.8900000000000000133, 0.9224999999999999867, 0.9549999999999999600, 0.9875000000000000444, 1.020000000000000018 ),
 .UNSPECIFIED. ) ;
#6475 = VERTEX_POINT ( 'NONE', #56999 ) ;
#6476 = CARTESIAN_POINT ( 'NONE',  ( 0.5739952604901000788, -83.17988695178998171, -1.223314898041000021 ) ) ;
#6477 = CARTESIAN_POINT ( 'NONE',  ( 9.031968385043001035, -77.11557531307438751, -3.250018536810999947 ) ) ;
#6478 = DIRECTION ( 'NONE',  ( 0.000000000000000000, 1.000000000000000000, 0.000000000000000000 ) ) ;
#6479 = DIRECTION ( 'NONE',  ( 0.000000000000000000, 1.000000000000000000, 0.000000000000000000 ) ) ;
#6480 = CARTESIAN_POINT ( 'NONE',  ( 1.179839603460000053, -3.032184344713000357, -3.521708340803999970 ) ) ;
#6481 = CARTESIAN_POINT ( 'NONE',  ( 4.400069678882000623, -77.16361025341399227, -11.21761009915999985 ) ) ;
#6482 = CARTESIAN_POINT ( 'NONE',  ( 7.686826547751000938, -78.57343297466498200, 5.981002702827999506 ) ) ;
#6483 = AXIS2_PLACEMENT_3D ( 'NONE', #22006, #27599, #9612 ) ;
#6485 = CARTESIAN_POINT ( 'NONE',  ( -13.86363636363000218, -32.36102867817999851, -1.277888278874999896E-05 ) ) ;
#6484 = CARTESIAN_POINT ( 'NONE',  ( -10.85510852219592337, -76.16860941111713146, 4.497416836951729557 ) ) ;
#6486 = CARTESIAN_POINT ( 'NONE',  ( -6.155296265070999695, -79.10392148219399644, -9.015968826447998907 ) ) ;
#6487 = CARTESIAN_POINT ( 'NONE',  ( 0.000000000000000000, -32.88214388149999934, 0.000000000000000000 ) ) ;
#6488 = VERTEX_POINT ( 'NONE', #7123 ) ;
#6489 = CARTESIAN_POINT ( 'NONE',  ( 1.250000000000000222, -82.23958333333330017, -0.1636246173744659582 ) ) ;
#6490 = CARTESIAN_POINT ( 'NONE',  ( -10.75000000000000000, -77.50000000000000000, 0.000000000000000000 ) ) ;
#6491 = B_SPLINE_CURVE_WITH_KNOTS ( 'NONE', 3,
 ( #47026, #19552, #1560, #33410, #28688, #15417, #23400, #41699, #14240, #11000, #55273, #28985, #46441, #9829, #46151, #45858, #46739, #54696, #1275, #51448, #19852, #23974, #54983, #6259, #10123, #5675, #6556, #37550, #28394, #19268, #37259, #23686, #14819, #5969, #24564, #24274, #5391, #42292, #1857, #41992, #32817, #41410, #55567, #992, #18688, #15116, #33114, #50279, #37847, #51155, #36970, #10710, #28101, #55867, #50863, #36679, #708, #18978, #14532, #10409, #32525, #50568, #2145, #25429, #43163, #16297, #20431, #34562, #52594, #42581, #15999, #52025, #38133, #21001, #7136, #12145, #38426, #56156, #39293, #30426, #56444, #15705, #16868, #29268, #2428, #52309, #34274, #11865, #42871, #7426, #48458, #20716, #33986, #2720, #11578, #8001, #52879, #29842, #47894, #6845, #11288, #43444, #3005, #38716, #39007, #56737, #47316, #29557, #48181, #12433, #20146 ),
 .UNSPECIFIED., .F., .F.,
 ( 4, 2, 2, 2, 2, 2, 1, 2, 2, 2, 2, 2, 2, 2, 2, 2, 2, 2, 2, 2, 2, 2, 2, 2, 2, 2, 2, 2, 1, 2, 2, 2, 2, 2, 2, 2, 2, 2, 2, 2, 2, 2, 2, 2, 2, 2, 2, 2, 2, 2, 1, 2, 2, 2, 2, 2, 4 ),
 ( 0.000000000000000000, 0.01562500000000000347, 0.03125000000000000694, 0.04687500000000000000, 0.06250000000000000000, 0.07812499999999998612, 0.09374999999999997224, 0.1093749999999999722, 0.1249999999999999584, 0.1406249999999999445, 0.1562499999999999167, 0.1718749999999998890, 0.1874999999999998612, 0.2031249999999998890, 0.2187499999999998890, 0.2343749999999998890, 0.2499999999999998890, 0.2656249999999998890, 0.2812499999999998890, 0.2968749999999998890, 0.3124999999999998890, 0.3281249999999998890, 0.3437499999999998890, 0.3593749999999998890, 0.3749999999999998890, 0.4062499999999999445, 0.4374999999999999445, 0.4687499999999999445, 0.4999999999999999445, 0.5312499999999998890, 0.5624999999999998890, 0.5937499999999998890, 0.6249999999999998890, 0.6406249999999998890, 0.6562499999999998890, 0.6718749999999998890, 0.6874999999999998890, 0.7031249999999998890, 0.7187499999999998890, 0.7343749999999998890, 0.7499999999999998890, 0.7656250000000000000, 0.7812500000000000000, 0.7968750000000000000, 0.8125000000000000000, 0.8281250000000000000, 0.8437500000000000000, 0.8593750000000000000, 0.8750000000000000000, 0.8906250000000000000, 0.9062500000000000000, 0.9218750000000000000, 0.9375000000000000000, 0.9531250000000000000, 0.9687500000000000000, 0.9843750000000000000, 1.000000000000000000 ),
 .UNSPECIFIED. ) ;
#6492 = CARTESIAN_POINT ( 'NONE',  ( -2.098469896607999926E-14, 0.000000000000000000, 0.000000000000000000 ) ) ;
#6493 = CARTESIAN_POINT ( 'NONE',  ( -7.658900562732000594, -60.00940503048000352, 10.01676248783999945 ) ) ;
#6494 = LINE ( 'NONE', #29497, #51556 ) ;
#6495 = CARTESIAN_POINT ( 'NONE',  ( 6.891029062618999390, -79.89012658836398373, 6.626049502339999897 ) ) ;
#6496 = CARTESIAN_POINT ( 'NONE',  ( 3.248132008022913020, -3.329261903070285022, -0.8492709327984924172 ) ) ;
#6497 = CARTESIAN_POINT ( 'NONE',  ( 8.060167320302427996, -17.37936585541044821, 9.621722526392044728 ) ) ;
#6498 = ORIENTED_EDGE ( 'NONE', *, *, #17624, .T. ) ;
#6499 = CARTESIAN_POINT ( 'NONE',  ( -9.774834661796999669, -79.23523028421899994, 5.593440076811999617 ) ) ;
#6500 = CARTESIAN_POINT ( 'NONE',  ( 7.655984445824144835, -23.70337239446406841, -10.06694410249365568 ) ) ;
#6501 = AXIS2_PLACEMENT_3D ( 'NONE', #46049, #9725, #45460 ) ;
#6502 = CARTESIAN_POINT ( 'NONE',  ( 0.000000000000000000, -90.29999999999999716, -9.699999999999990408 ) ) ;
#6503 = CARTESIAN_POINT ( 'NONE',  ( 1.996052162998995350, -78.54828564506389910, 3.456153249904594382 ) ) ;
#6504 = CARTESIAN_POINT ( 'NONE',  ( 1.173556370041068053, -77.58592580708349828, -12.24706281916396655 ) ) ;
#6505 = EDGE_CURVE ( 'NONE', #45641, #50158, #44530, .T. ) ;
#6506 = CARTESIAN_POINT ( 'NONE',  ( 1.250000000000000000, -81.34999999999999432, 0.000000000000000000 ) ) ;
#6507 = EDGE_CURVE ( 'NONE', #31243, #50285, #34448, .T. ) ;
#6508 = LINE ( 'NONE', #20099, #21910 ) ;
#6509 = CARTESIAN_POINT ( 'NONE',  ( 0.6295189948058200757, -82.26732208686871672, -1.093239786954644410 ) ) ;
#6510 = CARTESIAN_POINT ( 'NONE',  ( -7.648026768019999366, -23.24999998419999869, -10.12290050217000115 ) ) ;
#6511 = DIRECTION ( 'NONE',  ( 0.000000000000000000, 0.7071067811866525998, -0.7071067811864425456 ) ) ;
#6512 = CARTESIAN_POINT ( 'NONE',  ( -1.407249236881253918, -78.48544456714265038, 10.74983227778450257 ) ) ;
#6513 = DIRECTION ( 'NONE',  ( 0.000000000000000000, 1.000000000000000000, 0.000000000000000000 ) ) ;
#6514 = ORIENTED_EDGE ( 'NONE', *, *, #28980, .T. ) ;
#6515 = ADVANCED_FACE ( 'NONE', ( #43147 ), #11275, .T. ) ;
#6516 = EDGE_LOOP ( 'NONE', ( #2728, #28800, #9166, #4919 ) ) ;
#6517 = CARTESIAN_POINT ( 'NONE',  ( 8.163677614451000153, -77.67253998579799656, 4.925422544966999716 ) ) ;
#6518 = CARTESIAN_POINT ( 'NONE',  ( 5.788238289111504287, -78.77040165266161864, -9.060210061007026638 ) ) ;
#6519 = PRODUCT_DEFINITION_FORMATION_WITH_SPECIFIED_SOURCE ( 'ANY', '', #8796, .NOT_KNOWN. ) ;
#6520 = ORIENTED_EDGE ( 'NONE', *, *, #40836, .T. ) ;
#6521 = CARTESIAN_POINT ( 'NONE',  ( 8.878349648294999952, -16.93036913510000119, 8.870329531829000302 ) ) ;
#6522 = AXIS2_PLACEMENT_3D ( 'NONE', #48710, #38969, #30094 ) ;
#6523 = CARTESIAN_POINT ( 'NONE',  ( -12.00000000000000000, -77.89999999999999147, -2.795183092923000262E-14 ) ) ;
#6524 = CARTESIAN_POINT ( 'NONE',  ( 11.61968134756000026, -78.60307252743000106, 3.235820271459000086 ) ) ;
#6525 = CARTESIAN_POINT ( 'NONE',  ( 0.000000000000000000, -91.89999999999999147, 0.000000000000000000 ) ) ;
#6526 = CARTESIAN_POINT ( 'NONE',  ( 10.14948852604999985, -19.24899164588000389, 7.674614791898999755 ) ) ;
#6527 = CARTESIAN_POINT ( 'NONE',  ( 10.58946819037999987, -78.55715270318900423, -3.698823201301000285 ) ) ;
#6528 = ORIENTED_EDGE ( 'NONE', *, *, #28761, .T. ) ;
#6529 = DIRECTION ( 'NONE',  ( -1.000000000000000000, 0.000000000000000000, 0.000000000000000000 ) ) ;
#6530 = ORIENTED_EDGE ( 'NONE', *, *, #25865, .T. ) ;
#6531 = CARTESIAN_POINT ( 'NONE',  ( 9.123750851018394670, -77.36332806067234458, 1.522676030713496331 ) ) ;
#6532 = CARTESIAN_POINT ( 'NONE',  ( -9.808193611224998776, -77.95250248247700142, 5.067887917229000116 ) ) ;
#6533 = CONICAL_SURFACE ( 'NONE', #48028, 1.099999997148999986, 0.7853981633972997312 ) ;
#6534 = CARTESIAN_POINT ( 'NONE',  ( -7.712802233773871308, -77.41457454146333816, -8.144586586592856392 ) ) ;
#6535 = B_SPLINE_CURVE_WITH_KNOTS ( 'NONE', 3,
 ( #25853, #53015, #3711, #53305, #35272, #43882, #20568, #48035, #3428, #38853 ),
 .UNSPECIFIED., .F., .F.,
 ( 4, 2, 2, 2, 4 ),
 ( 0.000000000000000000, 0.2500000000000000000, 0.5000000000000000000, 0.7500000000000000000, 1.000000000000000000 ),
 .UNSPECIFIED. ) ;
#6536 = UNCERTAINTY_MEASURE_WITH_UNIT (LENGTH_MEASURE( 1.000000000000000082E-05 ), #21532, 'distance_accuracy_value', 'NONE');
#6537 = CARTESIAN_POINT ( 'NONE',  ( 9.549999999953000085, -76.40000000004698677, -5.125981083096999748E-10 ) ) ;
#6538 = CARTESIAN_POINT ( 'NONE',  ( -10.11462645681450034, -18.61287635839325461, -7.639895286233333138 ) ) ;
#6539 = TOROIDAL_SURFACE ( 'NONE', #43333, 1.250000000000000000, 0.5000000000000000000 ) ;
#6540 = CARTESIAN_POINT ( 'NONE',  ( 17.50000000000000000, -57.79999999999999716, 0.000000000000000000 ) ) ;
#6541 = CARTESIAN_POINT ( 'NONE',  ( 0.4102083068199999794, -78.53410088132000055, -1.574926093281000083 ) ) ;
#6542 = CARTESIAN_POINT ( 'NONE',  ( -5.869402599192000025, -78.46567021303999923, 10.46661899222999992 ) ) ;
#6543 = CARTESIAN_POINT ( 'NONE',  ( -11.03994916103999913, -78.49626308856198875, -0.4443153950920000206 ) ) ;
#6544 = CARTESIAN_POINT ( 'NONE',  ( 7.674614791501999989, -59.55100836074000625, 10.14948852566000070 ) ) ;
#6545 = LINE ( 'NONE', #28971, #46939 ) ;
#6546 = DIRECTION ( 'NONE',  ( -1.044282756598000039E-09, -1.000000000000000000, 6.141137129051000072E-09 ) ) ;
#6547 = CARTESIAN_POINT ( 'NONE',  ( -2.847654145493000222, -83.06005720286400162, 2.114813391968999756 ) ) ;
#6548 = VERTEX_POINT ( 'NONE', #56430 ) ;
#6549 = CARTESIAN_POINT ( 'NONE',  ( 11.68767212001979239, -79.62916666666666288, -3.140974612311342451 ) ) ;
#6550 = CARTESIAN_POINT ( 'NONE',  ( 0.9651418585498000580, -79.65707368812999789, 1.402967275931999769 ) ) ;
#6551 = CARTESIAN_POINT ( 'NONE',  ( 9.662219778377666657, -79.31367287321590709, -4.763839899825916824 ) ) ;
#6552 = CARTESIAN_POINT ( 'NONE',  ( 11.79843486695000010, -77.37002894411699572, -2.076781258317999868 ) ) ;
#6553 = CARTESIAN_POINT ( 'NONE',  ( -8.478741751137999216, -17.12187496603999648, 9.108230428607001272 ) ) ;
#6554 = EDGE_CURVE ( 'NONE', #34267, #8613, #40787, .T. ) ;
#6555 = CARTESIAN_POINT ( 'NONE',  ( -0.9821332843717349714, -78.19543708337666033, 0.8118240402714035353 ) ) ;
#6556 = CARTESIAN_POINT ( 'NONE',  ( -0.5809223153592418809, -3.138131673207912087, 3.474841036571488129 ) ) ;
#6557 = CARTESIAN_POINT ( 'NONE',  ( 9.722066209057999231, -78.94145584965399109, 0.1588365413100999990 ) ) ;
#6558 = CARTESIAN_POINT ( 'NONE',  ( 2.217690073412000196, -78.78676744264699039, -9.260249588150999855 ) ) ;
#6559 = CARTESIAN_POINT ( 'NONE',  ( 0.7369231997792153877, -81.27577443587277628, -1.011343237770755632 ) ) ;
#6560 = CARTESIAN_POINT ( 'NONE',  ( 7.384237969039999072, -77.14222102750099452, -8.196021229627000082 ) ) ;
#6561 = DIRECTION ( 'NONE',  ( 0.000000000000000000, 0.000000000000000000, -1.000000000000000000 ) ) ;
#6562 = CARTESIAN_POINT ( 'NONE',  ( -11.68767212001979061, -78.32083333333333997, -3.140974612311365988 ) ) ;
#6563 = CARTESIAN_POINT ( 'NONE',  ( 0.7435827448538506745, -81.97520306399145795, 1.034501988448051968 ) ) ;
#6564 = ORIENTED_EDGE ( 'NONE', *, *, #46709, .F. ) ;
#6565 = CARTESIAN_POINT ( 'NONE',  ( 0.8471236057751000414, -81.08589043725500289, 1.030027924806000028 ) ) ;
#6566 = CARTESIAN_POINT ( 'NONE',  ( -1.576170184330999868, -60.96086967183000382, -12.55466896108000086 ) ) ;
#6567 = CARTESIAN_POINT ( 'NONE',  ( 0.7038322923064118664, -80.46990387931118960, 10.74953000798084624 ) ) ;
#6568 = CARTESIAN_POINT ( 'NONE',  ( -11.14038684213999986, -78.32459623601998544, 1.307628137226999998 ) ) ;
#6569 = CARTESIAN_POINT ( 'NONE',  ( 0.2613587267741000475, -79.43644074375399100, -10.97249781033000104 ) ) ;
#6570 = CARTESIAN_POINT ( 'NONE',  ( 10.08161778466999969, -24.71855282893000094, -7.981584069265998949 ) ) ;
#6571 = CARTESIAN_POINT ( 'NONE',  ( 1.791187267989293064, -85.71458334881383223, 3.590998125927075790 ) ) ;
#6572 = CARTESIAN_POINT ( 'NONE',  ( 3.274231746039999891, -77.15535827300999472, -11.82472670181999952 ) ) ;
#6573 = CARTESIAN_POINT ( 'NONE',  ( 6.306936360652213303, -78.52899687234631187, 9.913378331859004078 ) ) ;
#6574 = FACE_OUTER_BOUND ( 'NONE', #23980, .T. ) ;
#6575 = ORIENTED_EDGE ( 'NONE', *, *, #46924, .T. ) ;
#6576 = CARTESIAN_POINT ( 'NONE',  ( -1.250000000000000000, -77.68333333333332291, 0.000000000000000000 ) ) ;
#6577 = CARTESIAN_POINT ( 'NONE',  ( 2.879226727952050258, -78.05416666666666003, 10.71369944335148361 ) ) ;
#6578 = CARTESIAN_POINT ( 'NONE',  ( 7.622784390041999814, -55.01288991740999990, -10.47836615824999917 ) ) ;
#6579 = CARTESIAN_POINT ( 'NONE',  ( 3.390474011741000382, -78.82851149742998587, -10.74400392503999946 ) ) ;
#6580 = EDGE_CURVE ( 'NONE', #33154, #37266, #11848, .T. ) ;
#6581 = DIRECTION ( 'NONE',  ( 0.000000000000000000, -1.000000000000000000, 0.000000000000000000 ) ) ;
#6582 = CARTESIAN_POINT ( 'NONE',  ( -7.634645133843775078, -23.47584427336687440, 10.10912661253024503 ) ) ;
#6583 = CARTESIAN_POINT ( 'NONE',  ( -1.192863218486718724, -81.80260132039094856, -0.9258880463762395596 ) ) ;
#6584 = AXIS2_PLACEMENT_3D ( 'NONE', #27253, #53552, #17532 ) ;
#6585 = CARTESIAN_POINT ( 'NONE',  ( -0.02827822798232390578, -81.97280723801726765, -1.511008595699627532 ) ) ;
#6586 = CARTESIAN_POINT ( 'NONE',  ( -0.8768947901867296668, -79.66348982473350304, -0.8905431139892215908 ) ) ;
#6587 = CONICAL_SURFACE ( 'NONE', #39566, 13.94999999937999924, 0.7853981633972997312 ) ;
#6588 = CARTESIAN_POINT ( 'NONE',  ( -9.433537730344784933, -53.67202052640185883, 8.532653828180887245 ) ) ;
#6589 = ORIENTED_EDGE ( 'NONE', *, *, #8047, .T. ) ;
#6590 = CARTESIAN_POINT ( 'NONE',  ( -1.151942055393958553, -81.63187234693144489, -0.4850639606811199545 ) ) ;
#6591 = CARTESIAN_POINT ( 'NONE',  ( 1.199999999999999956, -80.99999999999998579, 7.000000000000000000 ) ) ;
#6592 = ORIENTED_EDGE ( 'NONE', *, *, #9898, .F. ) ;
#6593 = ADVANCED_FACE ( 'NONE', ( #51723 ), #29541, .F. ) ;
#6594 = ORIENTED_EDGE ( 'NONE', *, *, #25162, .F. ) ;
#6595 = CARTESIAN_POINT ( 'NONE',  ( -0.9269474863677999998, -81.17097837165700014, -1.072766394601999851 ) ) ;
#6596 = EDGE_CURVE ( 'NONE', #34348, #12597, #57058, .T. ) ;
#6597 = EDGE_LOOP ( 'NONE', ( #57057, #23113, #45745, #17773 ) ) ;
#6598 = ORIENTED_EDGE ( 'NONE', *, *, #11428, .T. ) ;
#6599 = CARTESIAN_POINT ( 'NONE',  ( 1.666727925315000025, -18.80825518223999993, 12.50018462903999961 ) ) ;
#6600 = CARTESIAN_POINT ( 'NONE',  ( 12.69999999929000012, 7.140943757287000156E-10, 6.699859664396000284E-09 ) ) ;
#6601 = CARTESIAN_POINT ( 'NONE',  ( -12.99510751537000353, -52.49705297113997204, -6.911973076623003642 ) ) ;
#6602 = CARTESIAN_POINT ( 'NONE',  ( 9.633138876124000660, -78.59291001420200473, 2.765897569310999948 ) ) ;
#6603 = CARTESIAN_POINT ( 'NONE',  ( 6.550831367461507071, -78.28762608587432226, -6.530619802353137437 ) ) ;
#6604 = CARTESIAN_POINT ( 'NONE',  ( 1.099819419251000019, -79.56550200271298934, 11.16281809564999961 ) ) ;
#6605 = EDGE_LOOP ( 'NONE', ( #30821, #8062, #25259, #28652 ) ) ;
#6606 = AXIS2_PLACEMENT_3D ( 'NONE', #37594, #33153, #14279 ) ;
#6607 = EDGE_LOOP ( 'NONE', ( #26105, #44296 ) ) ;
#6608 = B_SPLINE_CURVE_WITH_KNOTS ( 'NONE', 3,
 ( #57726, #7276, #48313, #25278, #43010, #21429 ),
 .UNSPECIFIED., .F., .F.,
 ( 4, 1, 1, 4 ),
 ( 0.000000000000000000, 0.3333333333333000081, 0.6666666666667000474, 0.9999998688569219363 ),
 .UNSPECIFIED. ) ;
#6609 = FACE_BOUND ( 'NONE', #20185, .T. ) ;
#6610 = CARTESIAN_POINT ( 'NONE',  ( -12.70619440579224246, -24.46151788317378006, 1.571771935825063915 ) ) ;
#6611 = FILL_AREA_STYLE ('',( #33465 ) ) ;
#6612 = CARTESIAN_POINT ( 'NONE',  ( -12.43571054531000186, -61.67980566386000163, -0.4385525234350999835 ) ) ;
#6613 = CARTESIAN_POINT ( 'NONE',  ( 8.444976262095000408, -78.06083897633399715, 4.780490068936999570 ) ) ;
#6614 = CARTESIAN_POINT ( 'NONE',  ( -9.247932426686000795, -77.50168256874098915, -0.1955654147372000162 ) ) ;
#6615 = CARTESIAN_POINT ( 'NONE',  ( -2.813789756862251856, -76.60416666666665719, -10.47020627418439709 ) ) ;
#6616 = CARTESIAN_POINT ( 'NONE',  ( -1.937158916668030528, -79.75000000000000000, -9.096604487445336673 ) ) ;
#6617 = CARTESIAN_POINT ( 'NONE',  ( 0.4877854313978999268, -80.41809355086999744, -1.631527605715999973 ) ) ;
#6618 = DIRECTION ( 'NONE',  ( 0.000000000000000000, 1.000000000000000000, 0.000000000000000000 ) ) ;
#6619 = B_SPLINE_CURVE_WITH_KNOTS ( 'NONE', 3,
 ( #7895, #31177, #25896, #8468, #3467, #53059, #17044, #35027, #48642, #3755 ),
 .UNSPECIFIED., .F., .F.,
 ( 4, 2, 2, 2, 4 ),
 ( 0.000000000000000000, 0.5000000000000001110, 0.6250000000000000000, 0.7500000000000000000, 1.000000000000000000 ),
 .UNSPECIFIED. ) ;
#6620 = CARTESIAN_POINT ( 'NONE',  ( 7.067261237832259013, -79.23437499043450316, -9.724484250782996497 ) ) ;
#6621 = CARTESIAN_POINT ( 'NONE',  ( -10.19019671030999952, -55.60356357307000508, 7.646965722228999951 ) ) ;
#6622 = CARTESIAN_POINT ( 'NONE',  ( 9.525749612248999298, -78.21536332859899687, 2.735063621234999687 ) ) ;
#6623 = CARTESIAN_POINT ( 'NONE',  ( 10.40619348602752048, -76.82933193274368477, -2.787222590573924297 ) ) ;
#6624 = CARTESIAN_POINT ( 'NONE',  ( 1.799502287691000069, -18.69283319134000010, -12.60413670420000010 ) ) ;
#6625 = EDGE_CURVE ( 'NONE', #47968, #27284, #53988, .T. ) ;
#6626 = VECTOR ( 'NONE', #31313, 1000.000000000000000 ) ;
#6627 = VECTOR ( 'NONE', #7890, 1000.000000000000000 ) ;
#6629 = DIRECTION ( 'NONE',  ( 0.000000000000000000, 1.000000000000000000, 0.000000000000000000 ) ) ;
#6628 = CARTESIAN_POINT ( 'NONE',  ( -1.250000000000000000, -80.99999999999998579, 0.000000000000000000 ) ) ;
#6630 = CARTESIAN_POINT ( 'NONE',  ( -10.48543666025111776, -78.35833333333332007, 6.043427764450754580 ) ) ;
#6631 = CARTESIAN_POINT ( 'NONE',  ( 10.90030694484000051, -80.19320782078999343, 1.940743536767000066 ) ) ;
#6632 = CARTESIAN_POINT ( 'NONE',  ( 4.000000000000000000, -5.000000000000000000, 0.5999999999999999778 ) ) ;
#6633 = DIRECTION ( 'NONE',  ( 1.000000000000000000, 0.000000000000000000, 0.000000000000000000 ) ) ;
#6634 = CARTESIAN_POINT ( 'NONE',  ( -2.888768896543007614, -1.298725683607843351, -2.022024471902001519 ) ) ;
#6635 = EDGE_CURVE ( 'NONE', #42830, #44850, #55599, .T. ) ;
#6636 = ORIENTED_EDGE ( 'NONE', *, *, #8883, .F. ) ;
#6637 = CARTESIAN_POINT ( 'NONE',  ( -1.560639837747103131, -3.499999999999999556, -3.021350444604665508 ) ) ;
#6638 = DIRECTION ( 'NONE',  ( 0.000000000000000000, -1.000000000000000000, 0.000000000000000000 ) ) ;
#6639 = CARTESIAN_POINT ( 'NONE',  ( 0.3401359493934584810, -78.45311654837766469, 1.203085218402039525 ) ) ;
#6640 = CARTESIAN_POINT ( 'NONE',  ( -7.635222642325999232, -80.00803041167199581, -5.709097800406000012 ) ) ;
#6641 = CARTESIAN_POINT ( 'NONE',  ( 7.411516475408999050, -77.12122017304999133, -10.69619859711000132 ) ) ;
#6642 = CARTESIAN_POINT ( 'NONE',  ( -4.837304822058766440, -79.43335073634851540, -8.426485034531916440 ) ) ;
#6643 = CARTESIAN_POINT ( 'NONE',  ( -2.308100210809882036, -79.49222366784911742, 10.49994118944253785 ) ) ;
#6644 = CARTESIAN_POINT ( 'NONE',  ( 9.723265251863999481, -79.19761332859899028, 0.5504220888713000637 ) ) ;
#6645 = CARTESIAN_POINT ( 'NONE',  ( 0.000000000000000000, -80.74999999986198418, 0.000000000000000000 ) ) ;
#6646 = CARTESIAN_POINT ( 'NONE',  ( -9.228378915705999219, -77.85335538169299241, -6.089758258776999611 ) ) ;
#6647 = CARTESIAN_POINT ( 'NONE',  ( -0.2424364941441000121, -82.24054989383500924, 1.486642543718000198 ) ) ;
#6648 = CARTESIAN_POINT ( 'NONE',  ( -1.249549403371825740, -82.09031365513524747, 0.1639824843638148233 ) ) ;
#6649 = CARTESIAN_POINT ( 'NONE',  ( -6.279067761433998918, -78.45392319598897757, 7.013166371532999932 ) ) ;
#6651 = CARTESIAN_POINT ( 'NONE',  ( 17.50000000000000000, -21.00000000000000000, 0.000000000000000000 ) ) ;
#6650 = CARTESIAN_POINT ( 'NONE',  ( -2.548432965028000208, -83.10353803642099990, -3.035041914084000148 ) ) ;
#6652 = DIRECTION ( 'NONE',  ( 0.000000000000000000, -1.000000000000000000, 0.000000000000000000 ) ) ;
#6653 = DIRECTION ( 'NONE',  ( -0.7071067811865475727, 0.000000000000000000, 0.7071067811865475727 ) ) ;
#6654 = CARTESIAN_POINT ( 'NONE',  ( 10.74987231437827084, -80.34986571895258578, -0.04688819721409577534 ) ) ;
#6655 = CYLINDRICAL_SURFACE ( 'NONE', #11732, 3.250000000000000000 ) ;
#6656 = CYLINDRICAL_SURFACE ( 'NONE', #49233, 0.5000000000000006661 ) ;
#6657 = EDGE_LOOP ( 'NONE', ( #42369, #16118, #3633, #58366, #31617 ) ) ;
#6658 = VERTEX_POINT ( 'NONE', #21559 ) ;
#6659 = CARTESIAN_POINT ( 'NONE',  ( 11.92746894621999942, -79.46205103218200350, 1.562891678063999867 ) ) ;
#6660 = DIRECTION ( 'NONE',  ( 0.4045602622694902117, 0.8201597334573811349, -0.4045602622694902117 ) ) ;
#6661 = CARTESIAN_POINT ( 'NONE',  ( 7.655983890243021506, -18.29663439994899221, 10.06694524887558551 ) ) ;
#6662 = EDGE_LOOP ( 'NONE', ( #12706, #4613, #36143 ) ) ;
#6663 = EDGE_CURVE ( 'NONE', #45005, #9948, #21086, .T. ) ;
#6664 = CARTESIAN_POINT ( 'NONE',  ( 0.3849455888886000321, -77.25102680916499764, -11.69935108946000035 ) ) ;
#6665 = CIRCLE ( 'NONE', #47229, 4.799999999999999822 ) ;
#6666 = EDGE_CURVE ( 'NONE', #49070, #11684, #16180, .T. ) ;
#6667 = EDGE_LOOP ( 'NONE', ( #42072, #30105, #57122, #15532 ) ) ;
#6668 = EDGE_LOOP ( 'NONE', ( #12088, #1901, #6221 ) ) ;
#6669 = AXIS2_PLACEMENT_3D ( 'NONE', #20384, #38380, #55824 ) ;
#6670 = CARTESIAN_POINT ( 'NONE',  ( -1.750000000000000000, -60.04999999725999515, -12.50000000000000000 ) ) ;
#6671 = ORIENTED_EDGE ( 'NONE', *, *, #29229, .F. ) ;
#6672 = CARTESIAN_POINT ( 'NONE',  ( -0.9789553397924000144, -81.37292597959698526, 3.409722363132999590 ) ) ;
#6673 = CARTESIAN_POINT ( 'NONE',  ( 6.169502046027795394, -79.21861551698380310, 7.223965119394421208 ) ) ;
#6674 = EDGE_LOOP ( 'NONE', ( #10672, #25130, #14230, #3182 ) ) ;
#6675 = DIRECTION ( 'NONE',  ( 0.7071067811814920612, -1.249158819818986152E-07, -0.7071067811915919821 ) ) ;
#6676 = ORIENTED_EDGE ( 'NONE', *, *, #23431, .F. ) ;
#6677 = CARTESIAN_POINT ( 'NONE',  ( -3.104418684490000135, -2.089115405599000219, -1.389370826391999936 ) ) ;
#6678 = ORIENTED_EDGE ( 'NONE', *, *, #15474, .T. ) ;
#6679 = CARTESIAN_POINT ( 'NONE',  ( 0.000000000000000000, -23.25000000000000000, 12.00000000000000000 ) ) ;
#6680 = CARTESIAN_POINT ( 'NONE',  ( -1.499313493251033913, -78.74149442853628500, 0.1614851097358912524 ) ) ;
#6681 = CARTESIAN_POINT ( 'NONE',  ( 0.8532591808235191477, -79.79999999999998295, -11.75147895264783493 ) ) ;
#6682 = DIRECTION ( 'NONE',  ( -0.5000000000000744960, -0.7071067811864422126, 0.5000000000000744960 ) ) ;
#6683 = CARTESIAN_POINT ( 'NONE',  ( 2.624903909527706247, -78.80804708869507635, 11.97989236737772778 ) ) ;
#6684 = ADVANCED_FACE ( 'NONE', ( #39276 ), #35111, .T. ) ;
#6685 = CARTESIAN_POINT ( 'NONE',  ( -9.157500079073999544, -78.72316281358077106, 3.211059275314999795 ) ) ;
#6686 = CARTESIAN_POINT ( 'NONE',  ( -10.07624512687999996, -76.36960642326199888, -4.852130239470000106 ) ) ;
#6687 = CARTESIAN_POINT ( 'NONE',  ( 8.696932689530999738, -76.29999999999999716, -6.318691462144000681 ) ) ;
#6688 = CARTESIAN_POINT ( 'NONE',  ( 0.3918244861196526485, -81.20358808071422629, 1.461319962763056868 ) ) ;
#6689 = CARTESIAN_POINT ( 'NONE',  ( -5.192466827641999849, -76.54473956280799030, -9.696398534197001595 ) ) ;
#6690 = CARTESIAN_POINT ( 'NONE',  ( -7.239079175163887214, -78.65352817696454224, -5.758258266944833892 ) ) ;
#6691 = CARTESIAN_POINT ( 'NONE',  ( 5.333565260656944140, -76.53737489142297079, 10.47213728794457310 ) ) ;
#6692 = AXIS2_PLACEMENT_3D ( 'NONE', #33216, #51261, #28199 ) ;
#6693 = CARTESIAN_POINT ( 'NONE',  ( 1.199918086393000127, -80.46405261184000324, 0.5820416783086000967 ) ) ;
#6694 = FACE_OUTER_BOUND ( 'NONE', #20596, .T. ) ;
#6695 = DIRECTION ( 'NONE',  ( 0.000000000000000000, 0.000000000000000000, -1.000000000000000000 ) ) ;
#6696 = CARTESIAN_POINT ( 'NONE',  ( -2.532762364124999888, -81.32367549782598815, 2.543393847634999538 ) ) ;
#6697 = CARTESIAN_POINT ( 'NONE',  ( 11.09871289063999988, -79.85894599990470510, 4.778917828262999379 ) ) ;
#6698 = CARTESIAN_POINT ( 'NONE',  ( -10.60148741414840856, -78.08680037169739308, 1.782181226894791193 ) ) ;
#6699 = CARTESIAN_POINT ( 'NONE',  ( 0.8515782275871298657, -82.91596154203972446, 0.9145198330317436675 ) ) ;
#6700 = CARTESIAN_POINT ( 'NONE',  ( 11.65000000000000036, -76.00000000000000000, 0.000000000000000000 ) ) ;
#6701 = CARTESIAN_POINT ( 'NONE',  ( -1.217465845835396188, -80.47916666666668561, 0.3271848554490955907 ) ) ;
#6702 = CYLINDRICAL_SURFACE ( 'NONE', #588, 0.5000000000000004441 ) ;
#6703 = ADVANCED_FACE ( 'NONE', ( #34832 ), #1707, .F. ) ;
#6704 = CARTESIAN_POINT ( 'NONE',  ( -10.07616267223999884, -61.52631138996999738, -7.986947465035998839 ) ) ;
#6705 = CARTESIAN_POINT ( 'NONE',  ( -0.1832406609208000192, -81.74837035861699519, -1.320984106490000087 ) ) ;
#6706 = CONICAL_SURFACE ( 'NONE', #27422, 1.099999997157999232, 0.7853981633972997312 ) ;
#6707 = CARTESIAN_POINT ( 'NONE',  ( 12.50240633875000107, -54.11762602111000575, 1.005381409374000112 ) ) ;
#6708 = CARTESIAN_POINT ( 'NONE',  ( 12.44210192979000063, -24.08432059816999882, 1.464837683472000052 ) ) ;
#6709 = VECTOR ( 'NONE', #44029, 1000.000000000000114 ) ;
#6710 = CARTESIAN_POINT ( 'NONE',  ( 8.244337278279383341, -77.75611392600042393, 6.933698818737298986 ) ) ;
#6711 = CARTESIAN_POINT ( 'NONE',  ( -3.783525742921558521, -78.29734542223856408, -11.14657560477560061 ) ) ;
#6712 = LINE ( 'NONE', #19420, #33954 ) ;
#6713 = CARTESIAN_POINT ( 'NONE',  ( -5.681140472451000178, -76.84159451939000007, -10.64016158193000017 ) ) ;
#6714 = VERTEX_POINT ( 'NONE', #49904 ) ;
#6715 = B_SPLINE_SURFACE_WITH_KNOTS ( 'NONE', 3, 3, ( 
 ( #34505, #38948, #3519, #12375, #39235, #48405, #29783, #7942, #17679, #25944, #35074, #43386, #12659, #35666, #12091, #47839, #21519, #7370, #30653 ),
 ( #25371, #2945, #56963, #39526, #17091, #52534, #30074, #53111, #25655, #48687, #43684, #3239, #21231, #23280, #49268, #36269, #27982, #14407, #53698 ),
 ( #49574, #4395, #4696, #41577, #54293, #31526, #22395, #23564, #13830, #10003, #2, #40406, #13235, #18856, #53995, #32406, #1158, #46030, #40998 ),
 ( #31229, #9121, #49870, #19146, #54583, #36561, #45736, #14123, #4980, #27693, #8821, #45438, #31828, #869, #50450, #32119, #50160, #5553, #9703 ) ),
 .UNSPECIFIED., .F., .F., .F.,
 ( 4, 4 ),
 ( 4, 1, 1, 1, 1, 1, 1, 1, 1, 1, 1, 1, 1, 1, 1, 1, 4 ),
 ( -0.1377334280162000046, 1.137733428016000081 ),
 ( 0.6650746268656999582, 0.6864179104477999838, 0.7077611940298000892, 0.7291044776119000037, 0.7504477611940000292, 0.7717910447760999437, 0.7931343283582000803, 0.8144776119402999948, 0.8358208955224000203, 0.8571641791044999348, 0.8785074626865999603, 0.8998507462686999858, 0.9211940298506999802, 0.9425373134328000058, 0.9638805970148999203, 0.9852238805970000568, 1.006567164178999940 ),
 .UNSPECIFIED. ) ;
#6716 = CARTESIAN_POINT ( 'NONE',  ( 3.500502033605999763, -82.87121544543099105, 1.858134073305999889 ) ) ;
#6717 = CARTESIAN_POINT ( 'NONE',  ( 0.000000000000000000, -3.500000000000000000, 0.000000000000000000 ) ) ;
#6718 = CARTESIAN_POINT ( 'NONE',  ( 9.250000492344584657, -78.34738994167214798, -0.3032949936654210643 ) ) ;
#6719 = CARTESIAN_POINT ( 'NONE',  ( 7.764220096253753312, -54.54399029293954726, 10.21028322249942022 ) ) ;
#6720 = CARTESIAN_POINT ( 'NONE',  ( -2.309466437479000156, -77.79318524325600492, 10.97654204954999990 ) ) ;
#6721 = CARTESIAN_POINT ( 'NONE',  ( 12.48408657656000109, -55.43026141536999774, -1.669508654504999967 ) ) ;
#6722 = CARTESIAN_POINT ( 'NONE',  ( -0.5568870975076999352, -77.94963385321997862, -9.723660445896001647 ) ) ;
#6723 = CARTESIAN_POINT ( 'NONE',  ( -7.342331066867000544, -59.94999999967000548, -8.190859204290999784 ) ) ;
#6724 = DIRECTION ( 'NONE',  ( 0.000000000000000000, -1.000000000000000000, 0.000000000000000000 ) ) ;
#6725 = CARTESIAN_POINT ( 'NONE',  ( -0.5539667471886999817, -79.14255081561999816, -1.411437496924000001 ) ) ;
#6726 = ORIENTED_EDGE ( 'NONE', *, *, #50366, .T. ) ;
#6727 = CARTESIAN_POINT ( 'NONE',  ( -2.299491490204544242, -0.8333333333332290094, 2.552553896037383474 ) ) ;
#6728 = CARTESIAN_POINT ( 'NONE',  ( 2.215346327408018734, -78.96753941592319848, -2.793036654489012616 ) ) ;
#6729 = VERTEX_POINT ( 'NONE', #14730 ) ;
#6730 = CARTESIAN_POINT ( 'NONE',  ( -1.309352690804000074, -78.19332100324500345, -0.2533212985548999874 ) ) ;
#6731 = CARTESIAN_POINT ( 'NONE',  ( -6.447812191272999982, -78.73152414433498336, 8.972380486426999369 ) ) ;
#6732 = CARTESIAN_POINT ( 'NONE',  ( 12.49306752636999995, -60.08056692637000396, 1.667917367010000040 ) ) ;
#6733 = CARTESIAN_POINT ( 'NONE',  ( 3.250000000000000000, -3.250000000000000000, 0.000000000000000000 ) ) ;
#6734 = ORIENTED_EDGE ( 'NONE', *, *, #25417, .F. ) ;
#6735 = AXIS2_PLACEMENT_3D ( 'NONE', #43548, #3113, #39682 ) ;
#6736 = CARTESIAN_POINT ( 'NONE',  ( -9.022824479474000015, -78.20036040070399963, 8.159115699504999597 ) ) ;
#6737 = ORIENTED_EDGE ( 'NONE', *, *, #39116, .F. ) ;
#6738 = VERTEX_POINT ( 'NONE', #5304 ) ;
#6739 = CARTESIAN_POINT ( 'NONE',  ( 0.6898300185143996233, -80.42861775785651446, 1.042310243182293483 ) ) ;
#6740 = CARTESIAN_POINT ( 'NONE',  ( 11.68767212001977995, -79.57083333333332575, 3.140974612311385972 ) ) ;
#6741 = CARTESIAN_POINT ( 'NONE',  ( 1.841371367509999857, -80.39010546013851410, -9.592189096167999196 ) ) ;
#6742 = VERTEX_POINT ( 'NONE', #18605 ) ;
#6743 = CARTESIAN_POINT ( 'NONE',  ( -12.70228857838970704, -24.82190589609123776, -1.213561371311159487 ) ) ;
#6744 = CARTESIAN_POINT ( 'NONE',  ( -10.46946769381999864, -78.59626760295098791, -3.092832390908999862 ) ) ;
#6745 = EDGE_LOOP ( 'NONE', ( #49802, #49662, #36189, #42813, #40102 ) ) ;
#6746 = VECTOR ( 'NONE', #43139, 1000.000000000000000 ) ;
#6747 = CARTESIAN_POINT ( 'NONE',  ( 6.557594696296815684, -80.77712964829170517, -8.547591727114575377 ) ) ;
#6748 = CARTESIAN_POINT ( 'NONE',  ( 5.102724688570000389, -77.83873581701298860, 7.811319209985999379 ) ) ;
#6749 = CARTESIAN_POINT ( 'NONE',  ( -1.500000000000000000, -77.50000000000000000, 0.000000000000000000 ) ) ;
#6750 = AXIS2_PLACEMENT_3D ( 'NONE', #2269, #36800, #55397 ) ;
#6751 = EDGE_CURVE ( 'NONE', #39806, #40044, #57765, .T. ) ;
#6752 = CARTESIAN_POINT ( 'NONE',  ( 9.850513605848957965, -54.49492088415036761, 7.836738268828630893 ) ) ;
#6753 = CARTESIAN_POINT ( 'NONE',  ( -0.3926218265389256890, -81.29583333333334849, 1.460959015002472050 ) ) ;
#6754 = CARTESIAN_POINT ( 'NONE',  ( -8.920205756585657397, -78.01652913613843054, 3.873438468320558936 ) ) ;
#6755 = CARTESIAN_POINT ( 'NONE',  ( 7.097510073754000004, -77.08243616160899592, 6.942687883724000919 ) ) ;
#6756 = LINE ( 'NONE', #24766, #32846 ) ;
#6757 = CARTESIAN_POINT ( 'NONE',  ( 2.879226727952094222, -79.74583333333333712, -10.71369944335146940 ) ) ;
#6758 = CARTESIAN_POINT ( 'NONE',  ( -7.765022563360999719, -24.09093562100999719, 9.830785949113998612 ) ) ;
#6759 = CARTESIAN_POINT ( 'NONE',  ( 0.7412195098092654311, -77.02812499985410000, -9.421875000738944905 ) ) ;
#6760 = CARTESIAN_POINT ( 'NONE',  ( 10.52693147742000157, -60.22153431716999705, -7.606024891127000309 ) ) ;
#6761 = CARTESIAN_POINT ( 'NONE',  ( -7.421655993048999811, -78.37472433538000871, 9.763070719336001346 ) ) ;
#6762 = CARTESIAN_POINT ( 'NONE',  ( -1.925872869407999843, -76.67857486620199836, -12.12904120624999926 ) ) ;
#6763 = DIRECTION ( 'NONE',  ( -1.000000000000000000, 0.000000000000000000, 0.000000000000000000 ) ) ;
#6764 = EDGE_CURVE ( 'NONE', #22013, #36179, #4730, .T. ) ;
#6765 = CARTESIAN_POINT ( 'NONE',  ( 1.173085220040108290, -77.68291245588305571, -12.24193935082051965 ) ) ;
#6766 = CARTESIAN_POINT ( 'NONE',  ( 0.1636246173744697330, -78.63541666666665719, -1.249999999999999778 ) ) ;
#6767 =( GEOMETRIC_REPRESENTATION_CONTEXT ( 3 ) GLOBAL_UNCERTAINTY_ASSIGNED_CONTEXT ( ( #6536 ) ) GLOBAL_UNIT_ASSIGNED_CONTEXT ( ( #21532, #57543, #35683 ) ) REPRESENTATION_CONTEXT ( 'NONE', 'WORKASPACE' ) );
#6768 = ORIENTED_EDGE ( 'NONE', *, *, #4068, .F. ) ;
#6769 = CARTESIAN_POINT ( 'NONE',  ( 1.497208609717835648, -80.01106589178321826, 0.2087373732156078132 ) ) ;
#6770 = CARTESIAN_POINT ( 'NONE',  ( -6.317187036472000194, -77.26057450803698146, 7.370530927706999691 ) ) ;
#6771 = CARTESIAN_POINT ( 'NONE',  ( 2.062312494845999655, -23.22715659892999795, 12.83634740209000036 ) ) ;
#6772 = CARTESIAN_POINT ( 'NONE',  ( -0.9218200799623716968, -78.57291666666667140, -1.199500263597270910 ) ) ;
#6773 = CARTESIAN_POINT ( 'NONE',  ( 2.064858460238000237, -2.553371213896999947, -3.087201104211000136 ) ) ;
#6774 = CARTESIAN_POINT ( 'NONE',  ( 8.905881360917000222, -78.75077142985099954, 8.286615985300000986 ) ) ;
#6775 = CARTESIAN_POINT ( 'NONE',  ( 8.270224399031000928, -77.97653256295699009, -5.144228231339999624 ) ) ;
#6776 = ADVANCED_FACE ( 'NONE', ( #23887 ), #22729, .T. ) ;
#6778 = CARTESIAN_POINT ( 'NONE',  ( -10.76076152244900364, -77.71906335555217993, -2.634765227118816444 ) ) ;
#6777 = CARTESIAN_POINT ( 'NONE',  ( -9.885937566445212710, -76.15396054158379968, 6.353414232468484357 ) ) ;
#6779 = CARTESIAN_POINT ( 'NONE',  ( 1.250322495222000008, -82.36098159482000369, 0.5125084194436000384 ) ) ;
#6780 = CARTESIAN_POINT ( 'NONE',  ( -10.37577574274595804, -79.57882527228287017, 2.833895236981160082 ) ) ;
#6781 = ORIENTED_EDGE ( 'NONE', *, *, #52656, .T. ) ;
#6782 = CARTESIAN_POINT ( 'NONE',  ( 1.328206530128999807, -76.68360379137467930, -12.23810562210000086 ) ) ;
#6783 = EDGE_CURVE ( 'NONE', #24608, #29213, #47398, .T. ) ;
#6784 = CARTESIAN_POINT ( 'NONE',  ( -8.082941148289398470, -78.05848663413912902, 4.658681804407654781 ) ) ;
#6785 = PLANE ( 'NONE',  #37248 ) ;
#6786 = CARTESIAN_POINT ( 'NONE',  ( -9.523353692561999040, -61.61947015589999666, 8.220363114712000652 ) ) ;
#6787 = AXIS2_PLACEMENT_3D ( 'NONE', #33468, #37318, #50919 ) ;
#6788 = CARTESIAN_POINT ( 'NONE',  ( -9.469606800734000629, -80.05752053325198858, 5.597012331546999953 ) ) ;
#6789 = CARTESIAN_POINT ( 'NONE',  ( -4.409065846835999558, -79.66604063881599984, -8.482405482233000171 ) ) ;
#6790 = DIRECTION ( 'NONE',  ( 0.000000000000000000, -1.000000000000000000, 0.000000000000000000 ) ) ;
#6791 = DIRECTION ( 'NONE',  ( 0.000000000000000000, 1.000000000000000000, 0.000000000000000000 ) ) ;
#6792 = VERTEX_POINT ( 'NONE', #54327 ) ;
#6793 = CIRCLE ( 'NONE', #39764, 10.69999999999999929 ) ;
#6794 = CARTESIAN_POINT ( 'NONE',  ( -1.478754609759999950, -78.39090365116300063, -10.94487265352999827 ) ) ;
#6795 = CARTESIAN_POINT ( 'NONE',  ( -9.513123067637545560, -76.80684774649085966, 5.706940836106007886 ) ) ;
#6796 = LINE ( 'NONE', #24803, #4688 ) ;
#6797 = CARTESIAN_POINT ( 'NONE',  ( -0.7620226540494657863, -81.98338008206076211, -1.329091872049480427 ) ) ;
#6798 = CARTESIAN_POINT ( 'NONE',  ( -0.2725461282999930845, -81.49265652800838211, 1.220870497201928639 ) ) ;
#6799 = CARTESIAN_POINT ( 'NONE',  ( 0.8552014154741368612, -78.33376371967493412, -0.9447217733863905176 ) ) ;
#6800 = CARTESIAN_POINT ( 'NONE',  ( -1.250000000000000000, -80.99999999999998579, 0.000000000000000000 ) ) ;
#6801 = CARTESIAN_POINT ( 'NONE',  ( 1.799490220168999954, -56.02870851050000311, -12.64502302235999842 ) ) ;
#6802 = ADVANCED_FACE ( 'NONE', ( #10324 ), #24323, .F. ) ;
#6803 = CARTESIAN_POINT ( 'NONE',  ( -1.118058248199999882, -77.54775938543998848, 0.4799216473306999742 ) ) ;
#6804 = PLANE ( 'NONE',  #24587 ) ;
#6805 = CARTESIAN_POINT ( 'NONE',  ( 10.75000000000000000, -78.35000000000000853, 1.923335087985999915E-14 ) ) ;
#6806 = CARTESIAN_POINT ( 'NONE',  ( 0.000000000000000000, -74.64999999999999147, 0.000000000000000000 ) ) ;
#6807 = ORIENTED_EDGE ( 'NONE', *, *, #15995, .F. ) ;
#6808 = ORIENTED_EDGE ( 'NONE', *, *, #50924, .F. ) ;
#6809 = CARTESIAN_POINT ( 'NONE',  ( -12.12838880425000099, -77.24017731979098755, 2.901490023383999972 ) ) ;
#6810 = CARTESIAN_POINT ( 'NONE',  ( 5.117680542276197286, -78.76455040800591689, -9.453633761533124513 ) ) ;
#6811 = ORIENTED_EDGE ( 'NONE', *, *, #26192, .T. ) ;
#6812 = CARTESIAN_POINT ( 'NONE',  ( 8.227509542990000924, -17.17460508872999725, 9.516261809269000338 ) ) ;
#6813 = CARTESIAN_POINT ( 'NONE',  ( 10.26699006316253637, -76.00833333333331154, -5.917523019358050362 ) ) ;
#6814 = CARTESIAN_POINT ( 'NONE',  ( -3.799640087458000082, -78.34354736923999951, -11.29133014407999980 ) ) ;
#6815 = CARTESIAN_POINT ( 'NONE',  ( -1.407207572180206867, -79.71460441629234595, -10.68085486824220887 ) ) ;
#6816 = DIRECTION ( 'NONE',  ( -0.7071067811865475727, 0.000000000000000000, -0.7071067811865475727 ) ) ;
#6817 = CARTESIAN_POINT ( 'NONE',  ( 1.500000000000000000, -79.76041666666669983, 0.1963495408493652339 ) ) ;
#6818 = CARTESIAN_POINT ( 'NONE',  ( -4.019809786096000259, -79.23806127823398526, 10.47183077952999852 ) ) ;
#6819 = ORIENTED_EDGE ( 'NONE', *, *, #3245, .T. ) ;
#6820 = CARTESIAN_POINT ( 'NONE',  ( 10.70099950850357118, -78.08451462771667195, 4.958828595142525941 ) ) ;
#6821 = EDGE_LOOP ( 'NONE', ( #24831, #13161, #44726, #3605 ) ) ;
#6822 = CARTESIAN_POINT ( 'NONE',  ( 4.865965793551021434, -77.26911405462628579, -7.870456092190766917 ) ) ;
#6823 = LINE ( 'NONE', #56715, #45582 ) ;
#6824 = CIRCLE ( 'NONE', #32298, 5.000000000000000888 ) ;
#6825 = CARTESIAN_POINT ( 'NONE',  ( -11.14054172028253475, -78.34061020352532978, 1.307646316399887265 ) ) ;
#6826 = CARTESIAN_POINT ( 'NONE',  ( 0.7144648680787000217, -78.21136003831350081, -1.337341431498000111 ) ) ;
#6827 = DIRECTION ( 'NONE',  ( 0.000000000000000000, 0.000000000000000000, 1.000000000000000000 ) ) ;
#6828 = CARTESIAN_POINT ( 'NONE',  ( 6.606377239730313988, -80.82291666666665719, 8.596418555780454440 ) ) ;
#6829 = CARTESIAN_POINT ( 'NONE',  ( -1.491326706514000122, -77.92160361373998967, -0.6515838025032999470 ) ) ;
#6830 = CARTESIAN_POINT ( 'NONE',  ( -7.641012386039999882, -23.28917565320000094, 10.18589234708000113 ) ) ;
#6831 = CARTESIAN_POINT ( 'NONE',  ( 9.759566573192998362, -79.70423432486698800, -5.179648052473000419 ) ) ;
#6832 = EDGE_CURVE ( 'NONE', #13366, #1523, #32261, .T. ) ;
#6833 = CARTESIAN_POINT ( 'NONE',  ( 3.714552462503000640, -79.50001896804056400, 11.44155784251000085 ) ) ;
#6834 = AXIS2_PLACEMENT_3D ( 'NONE', #17669, #4081, #35959 ) ;
#6835 = CARTESIAN_POINT ( 'NONE',  ( 1.862677531273999820, -85.70556633873299290, 3.018611295180000376 ) ) ;
#6836 = ORIENTED_EDGE ( 'NONE', *, *, #11428, .F. ) ;
#6837 = EDGE_CURVE ( 'NONE', #1677, #18184, #39801, .T. ) ;
#6838 = CARTESIAN_POINT ( 'NONE',  ( 1.529418508686999800, -83.11625531570498993, 0.7487957062819000642 ) ) ;
#6839 = CARTESIAN_POINT ( 'NONE',  ( -0.6027184710183000060, -81.29937075464998486, 1.466649853462000053 ) ) ;
#6840 = CARTESIAN_POINT ( 'NONE',  ( 5.413682326552444302, -79.26680726287403900, -9.392823994831353218 ) ) ;
#6841 = CARTESIAN_POINT ( 'NONE',  ( 6.917788961650999546, -78.67230555502499101, -9.780606322222999083 ) ) ;
#6842 = CARTESIAN_POINT ( 'NONE',  ( -8.284626357352999904, -16.95139346842000094, 9.778502130864000108 ) ) ;
#6843 = AXIS2_PLACEMENT_3D ( 'NONE', #25951, #30658, #12381 ) ;
#6844 = CARTESIAN_POINT ( 'NONE',  ( -1.407139030276307157, -78.98557530161406248, 10.75050469601710645 ) ) ;
#6845 = CARTESIAN_POINT ( 'NONE',  ( 1.407444721559201417, -1.907779362115657573, -3.228803909804078831 ) ) ;
#6846 = CARTESIAN_POINT ( 'NONE',  ( 10.02077320556693785, -80.87969032288694393, 3.898277874299578727 ) ) ;
#6847 = CARTESIAN_POINT ( 'NONE',  ( 7.515172033767000492, -78.44568149309900207, 5.847440938983000436 ) ) ;
#6848 = CARTESIAN_POINT ( 'NONE',  ( 2.015551294784000191, -54.99652295122999845, -12.79857978891999970 ) ) ;
#6849 = CARTESIAN_POINT ( 'NONE',  ( 1.483539930421000186, -77.82312960254598977, 10.93164414240999882 ) ) ;
#6850 = CARTESIAN_POINT ( 'NONE',  ( -13.99999999961999819, -72.70000000038000110, 1.691901337660000028E-09 ) ) ;
#6851 = CARTESIAN_POINT ( 'NONE',  ( 4.292187240357000277, -81.18416302087679526, -9.881207810293000549 ) ) ;
#6852 = CARTESIAN_POINT ( 'NONE',  ( 0.9169854298989832397, -81.33914378987525140, -0.8846736303925517575 ) ) ;
#6853 = ORIENTED_EDGE ( 'NONE', *, *, #666, .T. ) ;
#6854 = VECTOR ( 'NONE', #55885, 1000.000000000000000 ) ;
#6855 = CARTESIAN_POINT ( 'NONE',  ( 10.98465012826175169, -18.69514063119935088, -0.5809631169955021823 ) ) ;
#6856 = CARTESIAN_POINT ( 'NONE',  ( 0.005928781627365999583, -62.00113050230000056, -12.66336824422999996 ) ) ;
#6857 = ADVANCED_FACE ( 'NONE', ( #24478 ), #11495, .F. ) ;
#6858 = CARTESIAN_POINT ( 'NONE',  ( -7.664266801483091918, -55.05053022673563135, 7.892048199458214341 ) ) ;
#6859 = CARTESIAN_POINT ( 'NONE',  ( -4.531904799951000484, -77.35800836368299827, -10.26060180864999971 ) ) ;
#6860 = CARTESIAN_POINT ( 'NONE',  ( 10.71556987377000070, -79.63720544108798549, 2.374990294079000197 ) ) ;
#6861 = CARTESIAN_POINT ( 'NONE',  ( 10.15831671671000080, -24.21991983044000207, -7.756223511073000232 ) ) ;
#6862 = CARTESIAN_POINT ( 'NONE',  ( 2.171690589435127716, -83.71041666057348607, -3.419483144129718877 ) ) ;
#6863 = CARTESIAN_POINT ( 'NONE',  ( -10.03846658019334193, -60.59367507117082852, 7.678639819092132335 ) ) ;
#6864 = DIRECTION ( 'NONE',  ( 0.000000000000000000, -1.000000000000000000, 0.000000000000000000 ) ) ;
#6865 = CARTESIAN_POINT ( 'NONE',  ( -10.41172477450676581, -60.32013115014467530, 7.610718073431628206 ) ) ;
#6866 = ORIENTED_EDGE ( 'NONE', *, *, #37206, .T. ) ;
#6867 = CARTESIAN_POINT ( 'NONE',  ( -0.8943305861287761394, -80.03894847689588232, 0.8728967361965981331 ) ) ;
#6868 = DIRECTION ( 'NONE',  ( -0.9805806756909162258, 0.1961161351382035567, 2.366670532390040672E-11 ) ) ;
#6869 = CARTESIAN_POINT ( 'NONE',  ( 11.14483649738000004, -78.94088091476099578, 1.649713251514000056 ) ) ;
#6870 = CARTESIAN_POINT ( 'NONE',  ( 0.000000000000000000, -77.69999999999998863, -2.500000000003963496 ) ) ;
#6871 = DIRECTION ( 'NONE',  ( 0.000000000000000000, 1.000000000000000000, 0.000000000000000000 ) ) ;
#6872 = CARTESIAN_POINT ( 'NONE',  ( 1.250000000000000000, -78.85000000000000853, 0.000000000000000000 ) ) ;
#6873 = AXIS2_PLACEMENT_3D ( 'NONE', #34481, #38640, #20071 ) ;
#6874 = CARTESIAN_POINT ( 'NONE',  ( 0.8231928634769288822, -82.51939026053260307, -1.312852273108907397 ) ) ;
#6875 = CARTESIAN_POINT ( 'NONE',  ( -1.211605918170402196, -79.62183856433064477, -0.3412175572405004020 ) ) ;
#6876 = CARTESIAN_POINT ( 'NONE',  ( -7.864797288573664780, -54.34877151149995456, 10.10445166985919840 ) ) ;
#6877 = VERTEX_POINT ( 'NONE', #6175 ) ;
#6878 = CARTESIAN_POINT ( 'NONE',  ( 1.667961445601999992, -21.74800977511999989, 12.58338334669999981 ) ) ;
#6879 = CONICAL_SURFACE ( 'NONE', #46524, 10.84999999997999964, 0.7853981633972997312 ) ;
#6880 =( NAMED_UNIT ( * ) SI_UNIT ( $, .STERADIAN. ) SOLID_ANGLE_UNIT ( ) );
#6881 = CARTESIAN_POINT ( 'NONE',  ( -12.48375848564000101, -23.37270426058999817, 1.669543623995999981 ) ) ;
#6882 = ORIENTED_EDGE ( 'NONE', *, *, #41832, .F. ) ;
#6883 = VERTEX_POINT ( 'NONE', #33322 ) ;
#6884 = CARTESIAN_POINT ( 'NONE',  ( -12.57354471034999932, -55.07622323954000620, -1.757967544833999973 ) ) ;
#6885 = ORIENTED_EDGE ( 'NONE', *, *, #5216, .T. ) ;
#6886 = CARTESIAN_POINT ( 'NONE',  ( -1.168698982885748139, -79.86530793566201680, -9.494534496902526044 ) ) ;
#6888 = EDGE_CURVE ( 'NONE', #47936, #37628, #29468, .T. ) ;
#6887 = ORIENTED_EDGE ( 'NONE', *, *, #42765, .F. ) ;
#6889 = CARTESIAN_POINT ( 'NONE',  ( 0.7554284705563453217, -81.83333333333801818, 1.310679582531389276 ) ) ;
#6890 = VECTOR ( 'NONE', #35642, 1000.000000000000114 ) ;
#6891 = CARTESIAN_POINT ( 'NONE',  ( -4.410648470793000264, -77.16531204370200214, -9.986067597275999574 ) ) ;
#6892 = DIRECTION ( 'NONE',  ( 0.000000000000000000, 1.000000000000000000, 0.000000000000000000 ) ) ;
#6893 = B_SPLINE_SURFACE_WITH_KNOTS ( 'NONE', 3, 3, ( 
 ( #48898, #53315, #45058, #12859, #54204, #8438, #40620, #36472, #22011, #40019, #9621, #31739, #58034, #14037, #4611, #217, #53610, #18193, #49783 ),
 ( #9330, #17594, #22307, #13149, #31143, #27320, #32032, #22901, #503, #49184, #50076, #27607, #8735, #26728, #44755, #58333, #17896, #35885, #19641 ),
 ( #23770, #46237, #19353, #9913, #41488, #33498, #46823, #51535, #29071, #28776, #41785, #1650, #50658, #6349, #6644, #32317, #37929, #6054, #19064 ),
 ( #24365, #24653, #10496, #27894, #42377, #1946, #1075, #37640, #42663, #11091, #37346, #45941, #5473, #19940, #18768, #55656, #14616, #14906, #55954 ) ),
 .UNSPECIFIED., .F., .F., .F.,
 ( 4, 4 ),
 ( 4, 1, 1, 1, 1, 1, 1, 1, 1, 1, 1, 1, 1, 1, 1, 1, 4 ),
 ( -0.1377334280162000046, 1.137733428016000081 ),
 ( 0.5889552238806000650, 0.6151492537313000275, 0.6413432835821000211, 0.6675373134327999836, 0.6937313432835999771, 0.7199253731343000506, 0.7461194029851000442, 0.7723134328358000067, 0.7985074626866000003, 0.8247014925372999627, 0.8508955223880999563, 0.8770895522388000298, 0.9032835820896000234, 0.9294776119402999859, 0.9556716417910000594, 0.9818656716417999419, 1.008059701493000171 ),
 .UNSPECIFIED. ) ;
#6894 = AXIS2_PLACEMENT_3D ( 'NONE', #10576, #50739, #55442 ) ;
#6895 = CARTESIAN_POINT ( 'NONE',  ( -3.403932870613000095, -78.65978667140099390, 9.307723658127001087 ) ) ;
#6896 = CARTESIAN_POINT ( 'NONE',  ( 1.157835957478192457, -79.36503902903432106, 9.256249544534666640 ) ) ;
#6897 = ORIENTED_EDGE ( 'NONE', *, *, #3634, .F. ) ;
#6898 = EDGE_LOOP ( 'NONE', ( #23795, #18909, #40759, #48072 ) ) ;
#6899 = CARTESIAN_POINT ( 'NONE',  ( -9.143293663829377138, -77.58804731730369042, 1.400502067634492365 ) ) ;
#6900 = DIRECTION ( 'NONE',  ( -0.7071067811865475727, 0.000000000000000000, 0.7071067811865475727 ) ) ;
#6901 = CARTESIAN_POINT ( 'NONE',  ( -12.49997170193999985, -59.99201514515999634, -1.666513530428000101 ) ) ;
#6902 = CARTESIAN_POINT ( 'NONE',  ( -9.282419925074000489, -77.29339558985098790, -2.829762163499999872 ) ) ;
#6903 = CARTESIAN_POINT ( 'NONE',  ( 7.626500902215000544, -18.68415522710999710, 10.35747158362999976 ) ) ;
#6904 = CARTESIAN_POINT ( 'NONE',  ( -9.500228589985420413, -79.40182418455218283, -0.2334504967788087748 ) ) ;
#6905 = CARTESIAN_POINT ( 'NONE',  ( -9.393203674808267678, -76.54166666666665719, -5.413904038987171319 ) ) ;
#6906 = CARTESIAN_POINT ( 'NONE',  ( 2.997885520263000370, -78.88962101269000016, -11.53013814508000046 ) ) ;
#6907 = CARTESIAN_POINT ( 'NONE',  ( 1.505228744355000092, -80.48125276597998834, -0.7963060858757999849 ) ) ;
#6908 = EDGE_CURVE ( 'NONE', #29025, #20424, #10631, .T. ) ;
#6909 = CARTESIAN_POINT ( 'NONE',  ( -0.4980389805768000167, -82.22048152020499856, -1.194395492011000037 ) ) ;
#6910 = ADVANCED_FACE ( 'NONE', ( #1770 ), #56817, .F. ) ;
#6912 = CONICAL_SURFACE ( 'NONE', #49306, 10.59999999997999787, 0.7853981633972997312 ) ;
#6911 = CARTESIAN_POINT ( 'NONE',  ( -9.963464501270999918, -55.11723479348000154, 7.659241807016999637 ) ) ;
#6913 = CARTESIAN_POINT ( 'NONE',  ( -5.875581754031000692, -78.86861332859899676, 7.981103691720999649 ) ) ;
#6914 = CARTESIAN_POINT ( 'NONE',  ( -10.99999999999000089, -80.20000000002698926, -2.639066790267999940E-09 ) ) ;
#6915 = CARTESIAN_POINT ( 'NONE',  ( 1.667916687244999974, -23.29849137228000444, -12.49168433579000137 ) ) ;
#6917 = CARTESIAN_POINT ( 'NONE',  ( -1.327706488546999797, -79.27312150602399754, -0.1249263990498000187 ) ) ;
#6916 = CARTESIAN_POINT ( 'NONE',  ( 0.9218200799623692543, -78.72291666666667709, 1.199500263597272687 ) ) ;
#6918 = CARTESIAN_POINT ( 'NONE',  ( -2.897260861154202338, -1.143336016975180058, -1.695352622819430444 ) ) ;
#6919 = CARTESIAN_POINT ( 'NONE',  ( -10.72134522692999958, -80.50391171894298736, -1.470872915343000020 ) ) ;
#6920 = CARTESIAN_POINT ( 'NONE',  ( 10.12290050122000018, -55.54999999974999980, -7.648026767069000087 ) ) ;
#6921 = CARTESIAN_POINT ( 'NONE',  ( 3.450547804646586059, -1.024362841730831697, 1.065430366115255323 ) ) ;
#6922 = ORIENTED_EDGE ( 'NONE', *, *, #31610, .T. ) ;
#6923 = FACE_OUTER_BOUND ( 'NONE', #43058, .T. ) ;
#6924 = DIRECTION ( 'NONE',  ( 0.000000000000000000, 0.000000000000000000, 1.000000000000000000 ) ) ;
#6925 = MECHANICAL_DESIGN_GEOMETRIC_PRESENTATION_REPRESENTATION (  '', ( #38679 ), #50950 ) ;
#6926 = CARTESIAN_POINT ( 'NONE',  ( -12.50240681836000078, -61.48234730679999416, 1.005418944265999981 ) ) ;
#6927 = CARTESIAN_POINT ( 'NONE',  ( 0.3711240750354344864, -78.45108290871590384, 1.193600970463786881 ) ) ;
#6928 = EDGE_CURVE ( 'NONE', #25833, #52807, #55782, .T. ) ;
#6929 = CARTESIAN_POINT ( 'NONE',  ( -0.09064084131274000034, -79.83269446212499076, 9.533214929259999693 ) ) ;
#6930 = CARTESIAN_POINT ( 'NONE',  ( -9.662326572316155548, -77.06369712772568903, 4.763895543093616070 ) ) ;
#6931 = DIRECTION ( 'NONE',  ( 0.000000000000000000, -1.000000000000000000, 0.000000000000000000 ) ) ;
#6932 = CARTESIAN_POINT ( 'NONE',  ( 0.7554284705563509839, -80.16666666666667140, -1.310679582531385945 ) ) ;
#6933 = DIRECTION ( 'NONE',  ( 0.000000000000000000, 1.000000000000000000, 0.000000000000000000 ) ) ;
#6934 = VECTOR ( 'NONE', #11012, 1000.000000000000000 ) ;
#6935 = FACE_OUTER_BOUND ( 'NONE', #35276, .T. ) ;
#6936 = VECTOR ( 'NONE', #15509, 1000.000000000000000 ) ;
#6937 = DIRECTION ( 'NONE',  ( 0.000000000000000000, 1.000000000000000000, 0.000000000000000000 ) ) ;
#6938 = CARTESIAN_POINT ( 'NONE',  ( -4.775172515662999828, -77.39640004304698095, -9.972254548579000399 ) ) ;
#6939 = CARTESIAN_POINT ( 'NONE',  ( 8.325345585179579899, -76.38763475635133204, -8.291621564338084838 ) ) ;
#6940 = CARTESIAN_POINT ( 'NONE',  ( 5.230327773973000305, -77.87272937556599572, -9.843691987646998598 ) ) ;
#6941 = CARTESIAN_POINT ( 'NONE',  ( -9.646692012709998210, -78.63999514476064689, 1.218660606027000215 ) ) ;
#6942 = CARTESIAN_POINT ( 'NONE',  ( -7.601397897754999633, -60.04999999657000131, -10.07627163191000008 ) ) ;
#6943 = CARTESIAN_POINT ( 'NONE',  ( 4.658475568430826108, -78.33333333333332860, 8.082524092276882399 ) ) ;
#6944 = CARTESIAN_POINT ( 'NONE',  ( -3.035171633316387396, -0.7760416592923815582, -1.750338234017642769 ) ) ;
#6945 = CARTESIAN_POINT ( 'NONE',  ( 6.063733907601372763, -80.27314283314856880, -8.876350182253380794 ) ) ;
#6946 = CARTESIAN_POINT ( 'NONE',  ( 6.436424241555000592, -79.92391735373439587, 8.610165096135999008 ) ) ;
#6947 = FACE_OUTER_BOUND ( 'NONE', #5495, .T. ) ;
#6948 = ORIENTED_EDGE ( 'NONE', *, *, #56456, .T. ) ;
#6949 = CARTESIAN_POINT ( 'NONE',  ( -7.858171174022000827, -78.99775398630599454, 9.108036400545000077 ) ) ;
#6950 = CARTESIAN_POINT ( 'NONE',  ( -1.250013176831791695, -78.10006463709670754, 4.053087819277079897E-06 ) ) ;
#6951 = DIRECTION ( 'NONE',  ( 0.000000000000000000, 0.000000000000000000, -1.000000000000000000 ) ) ;
#6952 = ORIENTED_EDGE ( 'NONE', *, *, #18774, .F. ) ;
#6953 = CARTESIAN_POINT ( 'NONE',  ( -1.980610890452893624, -23.52073889483701308, 12.74374574607051258 ) ) ;
#6954 = ORIENTED_EDGE ( 'NONE', *, *, #36938, .F. ) ;
#6956 = EDGE_CURVE ( 'NONE', #22441, #17800, #49325, .T. ) ;
#6955 = ORIENTED_EDGE ( 'NONE', *, *, #19142, .T. ) ;
#6957 = CARTESIAN_POINT ( 'NONE',  ( 8.090910852014772559, -60.34721902436125873, 7.452378523310778213 ) ) ;
#6958 = CARTESIAN_POINT ( 'NONE',  ( 3.075537641221555596, -77.44583333333332575, -11.44417895085270587 ) ) ;
#6959 = EDGE_CURVE ( 'NONE', #6475, #56949, #30906, .T. ) ;
#6960 = CARTESIAN_POINT ( 'NONE',  ( -2.717122596634000242, -78.92298487743470048, -2.276482554725000274 ) ) ;
#6961 = CARTESIAN_POINT ( 'NONE',  ( 9.052015793914058861, -79.17411443971855078, 2.882270040945727363 ) ) ;
#6962 = ORIENTED_EDGE ( 'NONE', *, *, #10266, .F. ) ;
#6963 = FACE_OUTER_BOUND ( 'NONE', #39975, .T. ) ;
#6964 = ORIENTED_EDGE ( 'NONE', *, *, #41461, .T. ) ;
#6965 = CARTESIAN_POINT ( 'NONE',  ( -10.52189733146974326, -76.98116804080198960, 2.543646231316468054 ) ) ;
#6966 = ORIENTED_EDGE ( 'NONE', *, *, #48934, .F. ) ;
#6967 = FACE_OUTER_BOUND ( 'NONE', #1031, .T. ) ;
#6968 = CARTESIAN_POINT ( 'NONE',  ( 1.520089283902537947, -78.48941957383496515, -0.1979304151590696170 ) ) ;
#6969 = CARTESIAN_POINT ( 'NONE',  ( -0.1587686074110454537, -79.80000000000001137, -11.79452369934064571 ) ) ;
#6970 = AXIS2_PLACEMENT_3D ( 'NONE', #40309, #49168, #14306 ) ;
#6971 = CARTESIAN_POINT ( 'NONE',  ( -5.385664337791607359, -80.01701569195293473, 9.304641679316141278 ) ) ;
#6972 = CARTESIAN_POINT ( 'NONE',  ( 7.081266003839625789, -79.12419498753402536, -10.01317160224411396 ) ) ;
#6973 = CARTESIAN_POINT ( 'NONE',  ( -3.448314610046759210, -86.39318692614396866, -2.406653721002784074 ) ) ;
#6974 = CARTESIAN_POINT ( 'NONE',  ( 9.886069181790999139, -76.61296857046200159, -5.228720670581999741 ) ) ;
#6975 = CARTESIAN_POINT ( 'NONE',  ( 3.401992325571604692, -79.69635448561501789, 9.101187944220413328 ) ) ;
#6976 = CARTESIAN_POINT ( 'NONE',  ( -1.983076715186758543, -79.52083333388351605, -9.322644982774999534 ) ) ;
#6977 = CARTESIAN_POINT ( 'NONE',  ( -10.01344192488999951, -76.42684861441699695, -4.821887891087000888 ) ) ;
#6978 = CARTESIAN_POINT ( 'NONE',  ( -5.318030017779740604, -78.67642921060232197, -7.571365619617901999 ) ) ;
#6979 = EDGE_CURVE ( 'NONE', #9420, #469, #43679, .T. ) ;
#6980 = CARTESIAN_POINT ( 'NONE',  ( 0.9336649615752000697, -80.36482736507799984, -0.9522845488932000224 ) ) ;
#6981 = FACE_OUTER_BOUND ( 'NONE', #43714, .T. ) ;
#6982 = CARTESIAN_POINT ( 'NONE',  ( 9.499999999999998224, -77.06041666666666856, 1.243547092045980129 ) ) ;
#6983 = CARTESIAN_POINT ( 'NONE',  ( -3.686203466609999868, -78.44153455456849144, -0.7231120618135999933 ) ) ;
#6984 = CARTESIAN_POINT ( 'NONE',  ( 3.462695758895999898, -79.92846326159968839, 11.57713085889000126 ) ) ;
#6985 = CARTESIAN_POINT ( 'NONE',  ( 11.91015624972854425, -76.21015625001426486, 0.9351146918447083012 ) ) ;
#6986 = CARTESIAN_POINT ( 'NONE',  ( 0.6995068289773208603, -82.92824216472010335, 1.038481775461846057 ) ) ;
#6987 = CARTESIAN_POINT ( 'NONE',  ( -2.858667760471000019, -84.83869503318800298, -2.099900233581000197 ) ) ;
#6988 = CARTESIAN_POINT ( 'NONE',  ( 0.1636246173744642929, -80.36458333333335702, 1.250000000000000888 ) ) ;
#6989 = CARTESIAN_POINT ( 'NONE',  ( -1.099495439336281688, -79.29263548292873054, -0.6453601205885236558 ) ) ;
#6990 = CARTESIAN_POINT ( 'NONE',  ( 10.74999999999999645, -80.23958333333330017, -1.407171709420461436 ) ) ;
#6991 = FACE_OUTER_BOUND ( 'NONE', #13601, .T. ) ;
#6992 = AXIS2_PLACEMENT_3D ( 'NONE', #42842, #38397, #25682 ) ;
#6993 = EDGE_CURVE ( 'NONE', #15223, #24242, #57790, .T. ) ;
#6994 = CARTESIAN_POINT ( 'NONE',  ( 1.289124607492999841, -80.90495576113799814, 0.3416633729347999804 ) ) ;
#6996 = EDGE_CURVE ( 'NONE', #12208, #22441, #26713, .T. ) ;
#6995 = CARTESIAN_POINT ( 'NONE',  ( 12.56594317819999951, -55.54999998572999687, 1.750000000000000000 ) ) ;
#6997 = CARTESIAN_POINT ( 'NONE',  ( -1.338697082642999803, -78.16879906939999501, -12.94399764267999942 ) ) ;
#6998 = AXIS2_PLACEMENT_3D ( 'NONE', #15497, #10489, #6049 ) ;
#6999 = CARTESIAN_POINT ( 'NONE',  ( 6.768311862815361124, -77.77140864696846734, 8.380151698724020548 ) ) ;
#7000 = CARTESIAN_POINT ( 'NONE',  ( -9.397239103731438448, -78.25099886579246800, -7.223445203516699387 ) ) ;
#7001 = DIRECTION ( 'NONE',  ( 1.000000000000000000, 0.000000000000000000, 0.000000000000000000 ) ) ;
#7002 = CARTESIAN_POINT ( 'NONE',  ( 9.309741638652999640, -76.86252759254999489, -7.903174005480999575 ) ) ;
#7003 = EDGE_LOOP ( 'NONE', ( #21110, #17908 ) ) ;
#7004 = VECTOR ( 'NONE', #20026, 1000.000000000000000 ) ;
#7005 = LINE ( 'NONE', #34716, #8819 ) ;
#7006 = CARTESIAN_POINT ( 'NONE',  ( 1.301773871033000018, -81.00121244067099724, 0.1523335971162000091 ) ) ;
#7007 = LINE ( 'NONE', #25298, #37784 ) ;
#7008 = CARTESIAN_POINT ( 'NONE',  ( 12.57433760364000008, -55.08878254084000048, -1.760777649351999985 ) ) ;
#7009 = CARTESIAN_POINT ( 'NONE',  ( 9.191740907676001271, -79.18591467081699875, -2.486449962426000138 ) ) ;
#7010 = CARTESIAN_POINT ( 'NONE',  ( -3.891846913306999944, -83.30682352787700040, -1.503357179412999844 ) ) ;
#7011 = CARTESIAN_POINT ( 'NONE',  ( 12.50000000000000000, -18.75000000000000000, 0.000000000000000000 ) ) ;
#7012 = CARTESIAN_POINT ( 'NONE',  ( -1.511528582562000178, -78.98795388112999660, 0.07582444189424000780 ) ) ;
#7013 = EDGE_LOOP ( 'NONE', ( #29303, #57828, #58365, #1834, #35011 ) ) ;
#7014 = DIRECTION ( 'NONE',  ( 0.7071067811865474617, 0.7071067811865474617, -1.027168298793069202E-09 ) ) ;
#7015 = CARTESIAN_POINT ( 'NONE',  ( 0.000000000000000000, -81.90000000002299885, 0.000000000000000000 ) ) ;
#7016 = EDGE_CURVE ( 'NONE', #46260, #26583, #35042, .T. ) ;
#7017 = CARTESIAN_POINT ( 'NONE',  ( -12.76303204513999923, -55.53514852210999919, 1.980584515753000208 ) ) ;
#7018 = ORIENTED_EDGE ( 'NONE', *, *, #50852, .T. ) ;
#7019 = CARTESIAN_POINT ( 'NONE',  ( 10.81514082164000001, -79.04054004199397809, -2.260668630147000258 ) ) ;
#7020 = FACE_OUTER_BOUND ( 'NONE', #27551, .T. ) ;
#7021 = CARTESIAN_POINT ( 'NONE',  ( -0.9211504236885831309, -80.66021725436883116, -0.8591334638782682775 ) ) ;
#7022 = EDGE_LOOP ( 'NONE', ( #26265, #5726, #1030, #44200 ) ) ;
#7023 = CARTESIAN_POINT ( 'NONE',  ( 3.985687926398000069, -78.60730013205999001, 11.49333817212000142 ) ) ;
#7024 = CARTESIAN_POINT ( 'NONE',  ( 9.452928397550001804, -77.41834665783399316, 6.429943439921999904 ) ) ;
#7025 = EDGE_LOOP ( 'NONE', ( #31826, #55152, #4856, #55174 ) ) ;
#7027 = EDGE_CURVE ( 'NONE', #51275, #41447, #9697, .T. ) ;
#7026 = ORIENTED_EDGE ( 'NONE', *, *, #28599, .F. ) ;
#7028 = B_SPLINE_CURVE_WITH_KNOTS ( 'NONE', 3,
 ( #25401, #3548, #3269, #4425, #52852, #22424, #18007, #31259, #44277, #39267, #12688, #16842, #35998, #25687, #40438, #49004, #8852, #4125, #27 ),
 .UNSPECIFIED., .F., .F.,
 ( 4, 1, 1, 1, 1, 1, 1, 1, 1, 1, 1, 1, 1, 1, 1, 1, 4 ),
 ( 0.000000000000000000, 0.04500041259816049688, 0.1100003587311620262, 0.1750003048641954329, 0.2400002509971969622, 0.3050001971301984915, 0.3700001432631362386, 0.4350000893963608117, 0.5000000355292667509, 0.5649999816621725790, 0.6299999277953972632, 0.6949998739283032023, 0.7599998200612091415, 0.8249997661944337146, 0.8899997123273396538, 0.9549996584602455929, 1.000000000000000000 ),
 .UNSPECIFIED. ) ;
#7029 = CARTESIAN_POINT ( 'NONE',  ( -0.2496591548053319620, -80.49116606994940071, 1.224717197152575654 ) ) ;
#7030 = ADVANCED_FACE ( 'NONE', ( #40372 ), #6407, .F. ) ;
#7031 = CARTESIAN_POINT ( 'NONE',  ( -3.184161968443000479, -86.31452041982799983, 1.417680270903999951 ) ) ;
#7032 = CARTESIAN_POINT ( 'NONE',  ( 9.647254834573999460, -80.36767059146200154, -1.526580663425000095 ) ) ;
#7033 = CIRCLE ( 'NONE', #9908, 12.50000000000000000 ) ;
#7034 = ORIENTED_EDGE ( 'NONE', *, *, #56303, .T. ) ;
#7035 = CARTESIAN_POINT ( 'NONE',  ( 2.840278559734812802, -2.392921495863389758, 1.635260199181394647 ) ) ;
#7036 = CARTESIAN_POINT ( 'NONE',  ( 3.572416533754999790, -79.98949669345269342, 10.28603406935999942 ) ) ;
#7037 = ORIENTED_EDGE ( 'NONE', *, *, #28006, .T. ) ;
#7038 = CARTESIAN_POINT ( 'NONE',  ( 5.896171905175000560, -77.86999999999999034, 7.127247495676000355 ) ) ;
#7039 = CARTESIAN_POINT ( 'NONE',  ( 6.214091009702999102, -77.69161915034599986, -7.179311535719000048 ) ) ;
#7040 = CARTESIAN_POINT ( 'NONE',  ( -8.485281374238999419, -55.54999999966999980, 8.485281374238999419 ) ) ;
#7041 = CARTESIAN_POINT ( 'NONE',  ( 12.60356226362999976, -59.55077028856999988, -1.750000000000000000 ) ) ;
#7042 = CARTESIAN_POINT ( 'NONE',  ( 10.09635500651664053, -55.27627834093870973, 7.644087038098070330 ) ) ;
#7043 = CARTESIAN_POINT ( 'NONE',  ( -0.9218200799623778030, -78.32708333333337691, 1.199500263597266914 ) ) ;
#7044 = CARTESIAN_POINT ( 'NONE',  ( -9.396809191439480458, -77.25090611101180116, -7.223167806601616725 ) ) ;
#7045 = B_SPLINE_CURVE_WITH_KNOTS ( 'NONE', 3,
 ( #47479, #7582, #20298, #29711, #39455, #52459, #21444, #56891, #2587, #25007, #42738, #12017, #38290, #11448, #2870 ),
 .UNSPECIFIED., .F., .F.,
 ( 4, 1, 1, 1, 1, 1, 1, 1, 1, 1, 1, 1, 4 ),
 ( 0.000000000000000000, 0.08333615748455000527, 0.1666676910119000155, 0.2500040280097000078, 0.3333307305850000124, 0.4166666802908000067, 0.5000000000075000006, 0.5833333207182000990, 0.6666693035046000748, 0.7499960124165999664, 0.8333323284379000606, 0.9166638841133999405, 1.000000000000000000 ),
 .UNSPECIFIED. ) ;
#7046 = AXIS2_PLACEMENT_3D ( 'NONE', #2459, #20464, #34017 ) ;
#7047 = CARTESIAN_POINT ( 'NONE',  ( 12.72923908220964506, -60.57554307125821680, -1.930512971242454912 ) ) ;
#7048 = CARTESIAN_POINT ( 'NONE',  ( -0.7748888817652298533, -77.76745404050591048, 1.296322661737231874 ) ) ;
#7049 = CARTESIAN_POINT ( 'NONE',  ( -2.873766102139449163, -81.51354167698465858, 2.856429910244337123 ) ) ;
#7050 = FACE_OUTER_BOUND ( 'NONE', #36791, .T. ) ;
#7051 = CARTESIAN_POINT ( 'NONE',  ( -4.071637125700000581, -81.77132046129098342, -0.9101188877549001299 ) ) ;
#7052 = CARTESIAN_POINT ( 'NONE',  ( -4.784380313523539208, -77.98333333333332007, -8.300970689365453126 ) ) ;
#7053 = CARTESIAN_POINT ( 'NONE',  ( 0.000000000000000000, -0.2000000000000000111, 0.000000000000000000 ) ) ;
#7054 = CARTESIAN_POINT ( 'NONE',  ( -5.531768889155999958, -79.07042751779999890, -10.94525552207000096 ) ) ;
#7055 = CARTESIAN_POINT ( 'NONE',  ( 0.000000000000000000, -23.15000000000000213, -12.00000000000000000 ) ) ;
#7056 = FACE_OUTER_BOUND ( 'NONE', #56495, .T. ) ;
#7057 = CARTESIAN_POINT ( 'NONE',  ( -5.578716042954554588, -77.96310415304682806, 10.76391831645009134 ) ) ;
#7058 = FACE_OUTER_BOUND ( 'NONE', #20764, .T. ) ;
#7059 = ORIENTED_EDGE ( 'NONE', *, *, #19782, .T. ) ;
#7060 = CARTESIAN_POINT ( 'NONE',  ( 0.5006249160878237792, -80.90177277154016622, -1.427178972532155088 ) ) ;
#7061 = CARTESIAN_POINT ( 'NONE',  ( 12.49989425042000235, -59.99225390429000271, -1.666425739590000177 ) ) ;
#7062 = CARTESIAN_POINT ( 'NONE',  ( 1.930628539545000022, -23.22124444086000139, 12.72375828104000028 ) ) ;
#7063 = CARTESIAN_POINT ( 'NONE',  ( -1.310679582531386611, -78.54166666666667140, -0.7554284705563495406 ) ) ;
#7064 = CARTESIAN_POINT ( 'NONE',  ( 3.543471834705000045, -3.225668112400000176, 0.3182372728196999900 ) ) ;
#7065 = CARTESIAN_POINT ( 'NONE',  ( 10.53043183326000154, -77.29925683053299679, 5.857113494125000486 ) ) ;
#7066 = CARTESIAN_POINT ( 'NONE',  ( 1.889053048974999927, -78.63028063292298953, 9.554641504766999915 ) ) ;
#7068 = CARTESIAN_POINT ( 'NONE',  ( -12.50239399164999909, -17.31640749886000208, 1.003653729363000124 ) ) ;
#7067 = CARTESIAN_POINT ( 'NONE',  ( -8.307785421988745256, -76.13749769528703837, 8.309209506187553274 ) ) ;
#7069 = CARTESIAN_POINT ( 'NONE',  ( 1.495758047513000122, -82.92972947813200335, -0.5264119980271999566 ) ) ;
#7070 = CARTESIAN_POINT ( 'NONE',  ( -9.984422089936529687, -79.56987114508450532, 3.984396093804686512 ) ) ;
#7071 = ORIENTED_EDGE ( 'NONE', *, *, #15660, .F. ) ;
#7072 = CARTESIAN_POINT ( 'NONE',  ( -7.685416442687997396, -76.62134450945413278, -9.616126112745993382 ) ) ;
#7073 = AXIS2_PLACEMENT_3D ( 'NONE', #48613, #39454, #12016 ) ;
#7074 = CARTESIAN_POINT ( 'NONE',  ( -5.872569646762852535, -79.32220536973464675, -7.509559151335658100 ) ) ;
#7075 = CARTESIAN_POINT ( 'NONE',  ( 5.917523019358082337, -76.96666666666665435, -10.26699006316252394 ) ) ;
#7076 = CARTESIAN_POINT ( 'NONE',  ( -8.485538010685999666, -61.68067982404999583, 9.101501073510000595 ) ) ;
#7077 = VECTOR ( 'NONE', #32887, 1000.000000000000000 ) ;
#7078 = DIRECTION ( 'NONE',  ( 0.000000000000000000, -1.000000000000000000, 0.000000000000000000 ) ) ;
#7079 = CARTESIAN_POINT ( 'NONE',  ( 9.256860190652000497, -78.81949371830199880, -1.144930063865999825 ) ) ;
#7080 = CARTESIAN_POINT ( 'NONE',  ( -1.181111693982000110, -79.27654225787900089, -0.4092372983238000139 ) ) ;
#7081 = CARTESIAN_POINT ( 'NONE',  ( -12.74331394907106407, -55.27353206545080155, -1.980611464663724286 ) ) ;
#7082 = ORIENTED_EDGE ( 'NONE', *, *, #32773, .F. ) ;
#7083 = CARTESIAN_POINT ( 'NONE',  ( -9.722718241315000398, -60.24678171298000251, 7.954951288349001004 ) ) ;
#7084 = CARTESIAN_POINT ( 'NONE',  ( 6.485260017975245539, -79.37834149910659676, 9.824335988400527242 ) ) ;
#7085 = CARTESIAN_POINT ( 'NONE',  ( 9.468750000004000356, -79.53124999999600675, -6.681056941828999630E-10 ) ) ;
#7086 = EDGE_CURVE ( 'NONE', #9942, #51555, #30271, .T. ) ;
#7089 = CARTESIAN_POINT ( 'NONE',  ( 0.3808713525295242541, -81.45074787893075552, 1.190513909683055926 ) ) ;
#7088 = CARTESIAN_POINT ( 'NONE',  ( -0.6440023044164000510, -81.57363842305200308, 1.151445457756000046 ) ) ;
#7087 = AXIS2_PLACEMENT_3D ( 'NONE', #1216, #24502, #15357 ) ;
#7090 = EDGE_CURVE ( 'NONE', #42991, #2755, #15447, .T. ) ;
#7091 = CARTESIAN_POINT ( 'NONE',  ( -1.254598503050118108, -78.63589187488014431, 0.2213234496388573058 ) ) ;
#7092 = LINE ( 'NONE', #39241, #19439 ) ;
#7093 = CARTESIAN_POINT ( 'NONE',  ( 12.50657368826004046, -61.77245458960354796, 0.3553454088956558010 ) ) ;
#7094 = CARTESIAN_POINT ( 'NONE',  ( 0.000000000000000000, -76.19999999999998863, 0.000000000000000000 ) ) ;
#7095 = CARTESIAN_POINT ( 'NONE',  ( 0.1636246173744642929, -78.36458333333330017, 1.250000000000000888 ) ) ;
#7096 = ADVANCED_FACE ( 'NONE', ( #55120 ), #1414, .T. ) ;
#7097 = CARTESIAN_POINT ( 'NONE',  ( 12.70451544420807188, -54.24534321882928367, -1.498804046740677798 ) ) ;
#7098 = ORIENTED_EDGE ( 'NONE', *, *, #7725, .F. ) ;
#7099 = EDGE_LOOP ( 'NONE', ( #58304, #46547, #15012, #51467 ) ) ;
#7100 = CARTESIAN_POINT ( 'NONE',  ( -0.6836460803099999595, -76.44726687979999724, -12.57002739626000043 ) ) ;
#7101 = CARTESIAN_POINT ( 'NONE',  ( -4.675525118886041831, -78.68936016309882575, -9.679868782351919165 ) ) ;
#7102 = EDGE_LOOP ( 'NONE', ( #23494, #6520, #297, #10236 ) ) ;
#7103 = CARTESIAN_POINT ( 'NONE',  ( 7.646966891758999907, -18.80358255734000039, 10.19019756605999838 ) ) ;
#7104 = DIRECTION ( 'NONE',  ( -1.000000000000000000, 0.000000000000000000, 0.000000000000000000 ) ) ;
#7105 = CARTESIAN_POINT ( 'NONE',  ( 9.700000000000001066, -87.70000000000000284, 0.000000000000000000 ) ) ;
#7106 = ADVANCED_FACE ( 'NONE', ( #54833 ), #32661, .T. ) ;
#7107 = CARTESIAN_POINT ( 'NONE',  ( 12.17287523535000027, -77.98388785726000094, -3.409737174454000375 ) ) ;
#7108 = CARTESIAN_POINT ( 'NONE',  ( 0.000000000000000000, -0.6500000000000000222, 0.000000000000000000 ) ) ;
#7109 = LINE ( 'NONE', #16547, #9816 ) ;
#7110 = CYLINDRICAL_SURFACE ( 'NONE', #15308, 3.250000000000000000 ) ;
#7111 = CARTESIAN_POINT ( 'NONE',  ( -4.152600241220000044, -79.42871567924700571, -10.41988588363999924 ) ) ;
#7112 = EDGE_CURVE ( 'NONE', #54154, #2738, #556, .T. ) ;
#7113 = CIRCLE ( 'NONE', #36347, 12.57042253521000141 ) ;
#7114 = ORIENTED_EDGE ( 'NONE', *, *, #53523, .T. ) ;
#7115 = CARTESIAN_POINT ( 'NONE',  ( 7.970415440577865773, -54.27707676769661305, -9.713035532171977238 ) ) ;
#7116 = VERTEX_POINT ( 'NONE', #10254 ) ;
#7117 = CARTESIAN_POINT ( 'NONE',  ( 4.265386565970945121, -77.26315468739150560, -8.207862934106792352 ) ) ;
#7118 = CARTESIAN_POINT ( 'NONE',  ( -1.016909733597999965, -80.23596541309798624, 0.9879038282509999824 ) ) ;
#7119 = TOROIDAL_SURFACE ( 'NONE', #31573, 17.50000000000000000, 5.000000000000000000 ) ;
#7120 = CARTESIAN_POINT ( 'NONE',  ( -0.02522437684909708058, -78.47469668865502967, -11.17070649161864537 ) ) ;
#7121 = CARTESIAN_POINT ( 'NONE',  ( -0.7468003766476000171, -77.96329692140810153, 1.319557257415000073 ) ) ;
#7122 = FACE_OUTER_BOUND ( 'NONE', #49064, .T. ) ;
#7123 = CARTESIAN_POINT ( 'NONE',  ( -1.980584515752000119, -18.73514853375999678, -12.76303204602000108 ) ) ;
#7124 = CARTESIAN_POINT ( 'NONE',  ( -1.472167250137000005, -78.86465554589999272, -0.6938203229310999642 ) ) ;
#7125 = CARTESIAN_POINT ( 'NONE',  ( -5.866053559275163032, -78.39900354637602220, 10.46067059907391439 ) ) ;
#7126 = CARTESIAN_POINT ( 'NONE',  ( -10.51276546006999979, -78.46817073422899114, 3.399949415165999689 ) ) ;
#7127 = CARTESIAN_POINT ( 'NONE',  ( 7.624341764943999955, -60.06485149430999826, -10.42531124854999902 ) ) ;
#7128 = CARTESIAN_POINT ( 'NONE',  ( -1.488962551357000175, -84.91501152966898758, -3.216824776211999914 ) ) ;
#7129 = ORIENTED_EDGE ( 'NONE', *, *, #21214, .T. ) ;
#7130 = CARTESIAN_POINT ( 'NONE',  ( -8.937783764417927657, -77.19999999999998863, 6.271596724013802415 ) ) ;
#7131 = CARTESIAN_POINT ( 'NONE',  ( 0.8322913257134999521, -79.78370706566998649, 1.209850638715999960 ) ) ;
#7132 = DIRECTION ( 'NONE',  ( 0.000000000000000000, -1.000000000000000000, 0.000000000000000000 ) ) ;
#7133 = CARTESIAN_POINT ( 'NONE',  ( 11.81379047889000056, -77.32936970626499829, 1.987564636421000008 ) ) ;
#7134 = CARTESIAN_POINT ( 'NONE',  ( -8.188285776315000319, -17.29506253989999820, 9.395726099566001466 ) ) ;
#7135 = CARTESIAN_POINT ( 'NONE',  ( -0.2214140910157267050, -77.86150297134426523, -1.255277234743452430 ) ) ;
#7136 = CARTESIAN_POINT ( 'NONE',  ( -3.488853381481115346, -2.260600980737770271, -0.4651628758941012132 ) ) ;
#7137 = CARTESIAN_POINT ( 'NONE',  ( -5.600962501326000265, -78.11400584965400640, 7.948110234177999445 ) ) ;
#7138 = CARTESIAN_POINT ( 'NONE',  ( 9.333674174720000494, -77.87720491051898364, -1.884914489352999878 ) ) ;
#7139 = CARTESIAN_POINT ( 'NONE',  ( 0.4919046592935741868, -81.25746093831025973, -1.149158243204877472 ) ) ;
#7140 = CARTESIAN_POINT ( 'NONE',  ( 1.589707373765000042, -78.16322009697699968, -10.80037945888999928 ) ) ;
#7141 = CARTESIAN_POINT ( 'NONE',  ( 0.000000000000000000, -9.295797029142999435, 0.000000000000000000 ) ) ;
#7142 = CARTESIAN_POINT ( 'NONE',  ( 1.197531862287877891, -81.92749861843283554, 0.4345771507895428987 ) ) ;
#7143 = ORIENTED_EDGE ( 'NONE', *, *, #53765, .F. ) ;
#7144 = CARTESIAN_POINT ( 'NONE',  ( 0.000000000000000000, -49.87071424677999687, 0.000000000000000000 ) ) ;
#7145 = CARTESIAN_POINT ( 'NONE',  ( -0.9820397338569999413, -80.80308451575899653, -0.7733679338621000099 ) ) ;
#7146 = CARTESIAN_POINT ( 'NONE',  ( 1.484804496640999893, -61.51869153350000374, -12.77261165612999960 ) ) ;
#7147 = CARTESIAN_POINT ( 'NONE',  ( -0.03734840871947565227, -78.54828561723799396, -3.962636352599350875 ) ) ;
#7148 = CARTESIAN_POINT ( 'NONE',  ( -10.54491486739000017, -77.79378985171199190, -3.823987582478999947 ) ) ;
#7149 = CARTESIAN_POINT ( 'NONE',  ( -9.438868967565998247, -79.41246660642698885, -5.601050722391000214 ) ) ;
#7150 = CARTESIAN_POINT ( 'NONE',  ( 10.53495260691999924, -23.22711197486000145, -7.618387230241999930 ) ) ;
#7151 = CARTESIAN_POINT ( 'NONE',  ( 2.740721837759387824, -85.25208334383526676, -2.982738968832581605 ) ) ;
#7152 = B_SPLINE_CURVE_WITH_KNOTS ( 'NONE', 3,
 ( #3677, #26104, #21391, #39684, #19739, #15302, #16685, #42177, #48283, #11969 ),
 .UNSPECIFIED., .F., .F.,
 ( 4, 2, 2, 2, 4 ),
 ( 0.000000000000000000, 0.1249999999999990563, 0.2499999999999981126, 0.4999999999999962252, 1.000000000000000000 ),
 .UNSPECIFIED. ) ;
#7153 = CARTESIAN_POINT ( 'NONE',  ( -6.524356864576000170, -76.99668890759399176, 10.25272229717000094 ) ) ;
#7154 = FACE_OUTER_BOUND ( 'NONE', #55515, .T. ) ;
#7155 = CARTESIAN_POINT ( 'NONE',  ( -8.274772994298601247, -61.77888614401855705, 9.689268729882146047 ) ) ;
#7156 = ORIENTED_EDGE ( 'NONE', *, *, #46008, .T. ) ;
#7157 = DIRECTION ( 'NONE',  ( 0.7071067811865475727, 0.000000000000000000, 0.7071067811865475727 ) ) ;
#7158 = CARTESIAN_POINT ( 'NONE',  ( -9.250000000000000000, -77.99999999999998579, 0.000000000000000000 ) ) ;
#7159 = B_SPLINE_CURVE_WITH_KNOTS ( 'NONE', 3,
 ( #2439, #34284, #29566, #7145 ),
 .UNSPECIFIED., .F., .F.,
 ( 4, 4 ),
 ( 0.000000000000000000, 1.000000000000000000 ),
 .UNSPECIFIED. ) ;
#7160 = CARTESIAN_POINT ( 'NONE',  ( 8.456503675551001464, -78.04961660823299496, 7.278678959607000287 ) ) ;
#7161 = CARTESIAN_POINT ( 'NONE',  ( -6.007496854199997571, -79.17708331421573575, -10.42139454737465343 ) ) ;
#7162 = CARTESIAN_POINT ( 'NONE',  ( 11.44417895085270054, -77.57083333333332575, 3.075537641221564922 ) ) ;
#7163 = CARTESIAN_POINT ( 'NONE',  ( -10.14950121160999963, -56.04922972508000356, 7.674627477461999803 ) ) ;
#7164 = CARTESIAN_POINT ( 'NONE',  ( -1.506971685459099097, -82.84329131091146792, 0.1165168607353958691 ) ) ;
#7165 = CARTESIAN_POINT ( 'NONE',  ( -0.2710612067321039320, -79.70821832930488426, -1.220449725728272705 ) ) ;
#7166 = AXIS2_PLACEMENT_3D ( 'NONE', #44967, #54695, #40531 ) ;
#7167 = CARTESIAN_POINT ( 'NONE',  ( -7.610717068315568490, -55.27984996805254525, 10.41172376761247875 ) ) ;
#7168 = ORIENTED_EDGE ( 'NONE', *, *, #55708, .F. ) ;
#7169 = AXIS2_PLACEMENT_3D ( 'NONE', #43190, #81, #45218 ) ;
#7170 = DIRECTION ( 'NONE',  ( -1.000000000000000000, 0.000000000000000000, 0.000000000000000000 ) ) ;
#7171 = EDGE_CURVE ( 'NONE', #21680, #6877, #48348, .T. ) ;
#7172 = SHAPE_REPRESENTATION_RELATIONSHIP ( 'NONE' , 'NONE' ,  #46016, #42678 ) ;
#7173 = DIRECTION ( 'NONE',  ( -0.7071067811865475727, 0.000000000000000000, -0.7071067811865475727 ) ) ;
#7174 = VERTEX_POINT ( 'NONE', #41253 ) ;
#7175 = EDGE_LOOP ( 'NONE', ( #41734, #12118, #25595, #5848 ) ) ;
#7176 = CARTESIAN_POINT ( 'NONE',  ( -12.43410192427999839, -54.35868879854000113, -1.192687910178000132 ) ) ;
#7177 = ORIENTED_EDGE ( 'NONE', *, *, #5835, .T. ) ;
#7178 = ORIENTED_EDGE ( 'NONE', *, *, #54890, .T. ) ;
#7179 = DIRECTION ( 'NONE',  ( 0.7071067811865475727, 0.000000000000000000, -0.7071067811865475727 ) ) ;
#7180 = CARTESIAN_POINT ( 'NONE',  ( -9.204454400623999888, -78.11858404876599593, -5.869700187727000085 ) ) ;
#7181 = CONTEXT_DEPENDENT_SHAPE_REPRESENTATION ( #4765, #14488 ) ;
#7182 = CARTESIAN_POINT ( 'NONE',  ( -7.764010764070559567, -60.92280919712734288, 9.931043767944283118 ) ) ;
#7183 = CARTESIAN_POINT ( 'NONE',  ( -9.042797184480999562, -78.79043667140099672, -4.055650103703999143 ) ) ;
#7184 = CARTESIAN_POINT ( 'NONE',  ( -2.794094295877650680, -78.20065386029028787, -8.819927633509278664 ) ) ;
#7185 = CARTESIAN_POINT ( 'NONE',  ( 8.040680144505948590, -79.29236773697583374, 4.729291971201980971 ) ) ;
#7186 = EDGE_CURVE ( 'NONE', #33872, #17785, #24652, .T. ) ;
#7187 = EDGE_LOOP ( 'NONE', ( #10451, #45779, #14340, #24674 ) ) ;
#7188 = ORIENTED_EDGE ( 'NONE', *, *, #37559, .F. ) ;
#7189 = CARTESIAN_POINT ( 'NONE',  ( -3.808885479938491248, -77.50893336096748953, 8.432746257839983883 ) ) ;
#7190 = CARTESIAN_POINT ( 'NONE',  ( -1.500000000000000000, -79.00884741929299082, -0.1667699247263852436 ) ) ;
#7191 = CARTESIAN_POINT ( 'NONE',  ( -12.83838776462000020, -60.00596988455000513, -2.062170466182000172 ) ) ;
#7192 = CARTESIAN_POINT ( 'NONE',  ( -9.702231720816998362, -78.83173763022898584, -0.1934140619087000024 ) ) ;
#7193 = CARTESIAN_POINT ( 'NONE',  ( 7.642160924884000117, -19.21538333566000034, 10.55911395187000146 ) ) ;
#7194 = CARTESIAN_POINT ( 'NONE',  ( 7.610716808859600668, -60.32015489444223988, 10.41172350879423014 ) ) ;
#7195 = CARTESIAN_POINT ( 'NONE',  ( 0.000000000000000000, -23.15000000000000213, 11.79999999999999893 ) ) ;
#7196 = CARTESIAN_POINT ( 'NONE',  ( 7.117135278674999732, -80.13006704345897901, 8.718833803912000135 ) ) ;
#7197 = DIRECTION ( 'NONE',  ( 1.000000000000000000, 0.000000000000000000, 0.000000000000000000 ) ) ;
#7198 = CARTESIAN_POINT ( 'NONE',  ( -0.1636246173744673738, -81.11458333333331439, -1.249999999999999778 ) ) ;
#7199 = CARTESIAN_POINT ( 'NONE',  ( -10.30457855490000085, -55.03665569380999756, 7.636266480997000450 ) ) ;
#7200 = CARTESIAN_POINT ( 'NONE',  ( -9.721629130303000466, -78.49688667140098630, 1.228127365514999791 ) ) ;
#7201 = CARTESIAN_POINT ( 'NONE',  ( 1.568318300085000120E-14, 6.776263578034402713E-18, -12.89999999999698588 ) ) ;
#7202 = EDGE_CURVE ( 'NONE', #22736, #2323, #57722, .T. ) ;
#7203 = CARTESIAN_POINT ( 'NONE',  ( 1.667917367010000040, -23.28056692670000061, -12.49306752634999995 ) ) ;
#7204 = CIRCLE ( 'NONE', #12835, 12.25000000000000000 ) ;
#7206 = CARTESIAN_POINT ( 'NONE',  ( 1.798944584243999945, -18.78466771720000139, -12.61116915999999932 ) ) ;
#7205 = CARTESIAN_POINT ( 'NONE',  ( 5.799999999999999822, -80.99999999999998579, 0.000000000000000000 ) ) ;
#7207 = CARTESIAN_POINT ( 'NONE',  ( -4.999999999872000167, -80.49999999987198862, 4.857408280386999624E-10 ) ) ;
#7208 = CARTESIAN_POINT ( 'NONE',  ( -3.448863046786000197, -1.886744131007000114, -1.608907009436000068 ) ) ;
#7209 = VECTOR ( 'NONE', #49480, 1000.000000000000000 ) ;
#7210 = CARTESIAN_POINT ( 'NONE',  ( 2.227269615981378070, -0.9293910887734395665, -2.735979432117919607 ) ) ;
#7211 = CONICAL_SURFACE ( 'NONE', #11938, 4.199999999676998996, 0.7853981633972997312 ) ;
#7212 = VERTEX_POINT ( 'NONE', #47742 ) ;
#7213 = CARTESIAN_POINT ( 'NONE',  ( 10.75000000000000178, -80.25615977947786917, 0.8321152720824881444 ) ) ;
#7214 = CARTESIAN_POINT ( 'NONE',  ( 0.000000000000000000, -23.15000000000000213, -11.79999999999999893 ) ) ;
#7215 = CARTESIAN_POINT ( 'NONE',  ( -1.821913034590999979E-14, -80.69999999923000189, 0.000000000000000000 ) ) ;
#7216 = CARTESIAN_POINT ( 'NONE',  ( 1.228871970593624852, -78.36477678297961802, 0.2288398227139316898 ) ) ;
#7217 = CIRCLE ( 'NONE', #24194, 14.00000000000000533 ) ;
#7218 = CARTESIAN_POINT ( 'NONE',  ( 2.383426421432000009, -3.359465166820999826, 2.543613531316000209 ) ) ;
#7219 = CARTESIAN_POINT ( 'NONE',  ( 3.008644551092000352, -79.24281087269798718, 9.161133607876998042 ) ) ;
#7220 = CARTESIAN_POINT ( 'NONE',  ( -12.43359548531999970, -54.09290601346000216, 0.8500179128028999553 ) ) ;
#7221 = CARTESIAN_POINT ( 'NONE',  ( -7.540108831187442462, -79.40412807809049411, -6.127962695274685956 ) ) ;
#7222 = CARTESIAN_POINT ( 'NONE',  ( 1.929975092515999968, -60.00107256231000008, 12.72537404212999768 ) ) ;
#7223 = CARTESIAN_POINT ( 'NONE',  ( 8.500869906239369556, -79.11249999999999716, -4.334382246026802221 ) ) ;
#7224 = CARTESIAN_POINT ( 'NONE',  ( -11.00000000000000000, -77.19999999999998863, 5.688460190305999883E-13 ) ) ;
#7225 = CARTESIAN_POINT ( 'NONE',  ( 3.962812355710999768, -78.54828561723800817, 2.338746314310086394 ) ) ;
#7226 = CARTESIAN_POINT ( 'NONE',  ( 7.984952588555000119, -77.99615392501999622, -7.647802602006999351 ) ) ;
#7227 = CARTESIAN_POINT ( 'NONE',  ( 9.371262623183563178, -76.39810623049203286, -7.089854323050989393 ) ) ;
#7228 = CARTESIAN_POINT ( 'NONE',  ( -8.584476293286000370, -76.58844565707200047, 6.698613553322000591 ) ) ;
#7229 = DIRECTION ( 'NONE',  ( 0.000000000000000000, 1.000000000000000000, 0.000000000000000000 ) ) ;
#7230 = CARTESIAN_POINT ( 'NONE',  ( -1.607979213109999916, -78.80939078103999407, 0.4265466307092000142 ) ) ;
#7231 = CARTESIAN_POINT ( 'NONE',  ( -0.5065222552852000071, -77.08871499676898509, 9.658707080791000266 ) ) ;
#7232 = CARTESIAN_POINT ( 'NONE',  ( -6.090475762158000350, -79.43984415034599067, 7.362120511650999788 ) ) ;
#7233 = LINE ( 'NONE', #25237, #9155 ) ;
#7234 = DIRECTION ( 'NONE',  ( 0.000000000000000000, 1.000000000000000000, 0.000000000000000000 ) ) ;
#7235 = CARTESIAN_POINT ( 'NONE',  ( 7.102684642307564467, -79.91784024040764223, 8.111683265999065640 ) ) ;
#7236 = CARTESIAN_POINT ( 'NONE',  ( 2.039279229571573815, -79.98945650679056030, -11.03009289294175410 ) ) ;
#7237 = CARTESIAN_POINT ( 'NONE',  ( 3.552363299575000077, -79.64717257337099454, -11.49294985030999960 ) ) ;
#7238 = EDGE_CURVE ( 'NONE', #31099, #22708, #3517, .T. ) ;
#7239 = CARTESIAN_POINT ( 'NONE',  ( 8.485281374238999419, -23.25000000000000000, -8.485281374238999419 ) ) ;
#7240 = CARTESIAN_POINT ( 'NONE',  ( 2.417503760557000447, -80.18084841004029784, 10.77648496335999972 ) ) ;
#7241 = ORIENTED_EDGE ( 'NONE', *, *, #4965, .F. ) ;
#7242 = ADVANCED_FACE ( 'NONE', ( #19848, #988 ), #54977, .F. ) ;
#7243 = CARTESIAN_POINT ( 'NONE',  ( 1.208267226973974706, -24.82590682147949934, 12.70228502423902484 ) ) ;
#7244 = ORIENTED_EDGE ( 'NONE', *, *, #36701, .T. ) ;
#7245 = VECTOR ( 'NONE', #42889, 1000.000000000000114 ) ;
#7246 = ORIENTED_EDGE ( 'NONE', *, *, #15787, .T. ) ;
#7247 = DIRECTION ( 'NONE',  ( 0.7071067811865475727, 0.000000000000000000, -0.7071067811865475727 ) ) ;
#7248 = ORIENTED_EDGE ( 'NONE', *, *, #13867, .T. ) ;
#7249 = VECTOR ( 'NONE', #47267, 1000.000000000000000 ) ;
#7250 = CARTESIAN_POINT ( 'NONE',  ( 0.4735443828009999745, -79.16348572639719805, -3.512938801767000019 ) ) ;
#7251 = CARTESIAN_POINT ( 'NONE',  ( 2.890496000096741014, -79.25013075116083883, 9.049465696841215490 ) ) ;
#7252 = ORIENTED_EDGE ( 'NONE', *, *, #32267, .T. ) ;
#7254 = EDGE_CURVE ( 'NONE', #43183, #6714, #6824, .T. ) ;
#7253 = CARTESIAN_POINT ( 'NONE',  ( -7.478989599426999924, -78.43234560996998539, 9.838492168967000850 ) ) ;
#7255 = CIRCLE ( 'NONE', #41178, 12.50000000000000000 ) ;
#7256 = VERTEX_POINT ( 'NONE', #24560 ) ;
#7257 = CARTESIAN_POINT ( 'NONE',  ( 0.000000000000000000, -77.29999999999999716, 0.000000000000000000 ) ) ;
#7258 = ORIENTED_EDGE ( 'NONE', *, *, #19301, .F. ) ;
#7259 = CYLINDRICAL_SURFACE ( 'NONE', #29009, 1.750000000000000000 ) ;
#7260 = CARTESIAN_POINT ( 'NONE',  ( -1.215794352730352079, -78.80031189463259977, -0.8913456688967522634 ) ) ;
#7261 = CIRCLE ( 'NONE', #42119, 2.500000000000000000 ) ;
#7262 = CARTESIAN_POINT ( 'NONE',  ( 6.590460453269219698, -79.79999999999999716, 9.896017889727964700 ) ) ;
#7263 = CARTESIAN_POINT ( 'NONE',  ( -6.807492820124149802, -80.02998060238465428, 8.319674890179079796 ) ) ;
#7264 = CARTESIAN_POINT ( 'NONE',  ( -8.838834764832000701, -18.75000000000000000, -8.838834764832000701 ) ) ;
#7265 = CARTESIAN_POINT ( 'NONE',  ( -3.113118550637747894, -86.25171435493595595, 1.456966602822371559 ) ) ;
#7266 = CARTESIAN_POINT ( 'NONE',  ( -9.831705185582000794, -76.36214915056999075, 5.330239850318999828 ) ) ;
#7267 = CARTESIAN_POINT ( 'NONE',  ( 0.9440756146772367741, -79.98258690118150582, -9.563528426713427066 ) ) ;
#7268 = CARTESIAN_POINT ( 'NONE',  ( 12.76303204522000101, -23.26485147686999966, 1.980584515753000208 ) ) ;
#7269 = CARTESIAN_POINT ( 'NONE',  ( 1.838208114491000078, -76.75291386027500096, 10.96086719000000009 ) ) ;
#7270 = CARTESIAN_POINT ( 'NONE',  ( -6.009140664802340659, -78.66887010198279029, -7.034215166533324570 ) ) ;
#7271 = CARTESIAN_POINT ( 'NONE',  ( -1.213636094208999872, -80.71211572874599938, -0.5527192377158001158 ) ) ;
#7272 = DIRECTION ( 'NONE',  ( 0.000000000000000000, -1.000000000000000000, 0.000000000000000000 ) ) ;
#7273 = CARTESIAN_POINT ( 'NONE',  ( 1.980744519413613292, -2.923166175690931290, 2.579508073329230378 ) ) ;
#7274 = CARTESIAN_POINT ( 'NONE',  ( 3.455307625259000037, -82.04903455456799577, -1.473715123765999779 ) ) ;
#7275 = CARTESIAN_POINT ( 'NONE',  ( 10.20754100699015865, -76.23359375000963212, 6.252571624904344816 ) ) ;
#7276 = CARTESIAN_POINT ( 'NONE',  ( -14.00000000000000000, -32.90763690531000663, -1.352038286243999979E-05 ) ) ;
#7277 = CARTESIAN_POINT ( 'NONE',  ( -8.096452064242996016, -56.01421830980998351, 13.15643568217000769 ) ) ;
#7278 = CARTESIAN_POINT ( 'NONE',  ( 1.925627134546000097, -85.19944503318799889, -2.978845823512000113 ) ) ;
#7279 = CARTESIAN_POINT ( 'NONE',  ( -11.55907703490496985, -76.21507827338332675, -2.244914986486493902 ) ) ;
#7280 = CARTESIAN_POINT ( 'NONE',  ( 10.24998526315000014, -21.75083378359999742, 7.705142895586000407 ) ) ;
#7281 = CARTESIAN_POINT ( 'NONE',  ( -7.753906807064999462, -61.08933445950000163, -10.31979621052999896 ) ) ;
#7282 = CARTESIAN_POINT ( 'NONE',  ( -11.00000000000000000, -4.000000000000000000, 0.000000000000000000 ) ) ;
#7283 = CARTESIAN_POINT ( 'NONE',  ( 3.799999999999999822, 0.000000000000000000, 0.000000000000000000 ) ) ;
#7284 = CARTESIAN_POINT ( 'NONE',  ( -0.3926218265389189721, -80.50416666666666288, -1.460959015002473604 ) ) ;
#7285 = CARTESIAN_POINT ( 'NONE',  ( -3.129814719915999799, -78.44632227421000437, 12.62985940900000159 ) ) ;
#7286 = AXIS2_PLACEMENT_3D ( 'NONE', #52156, #7272, #25273 ) ;
#7287 = ADVANCED_FACE ( 'NONE', ( #52019 ), #43158, .F. ) ;
#7288 = CARTESIAN_POINT ( 'NONE',  ( 10.06692847398457857, -23.70343452287690056, 7.655995225931332193 ) ) ;
#7289 = CARTESIAN_POINT ( 'NONE',  ( 8.768124086712999699, -59.94999999969000015, -7.919595949288999570 ) ) ;
#7290 = CARTESIAN_POINT ( 'NONE',  ( -10.00409279782000027, -76.63142817898000203, -7.262369351941000417 ) ) ;
#7291 = ORIENTED_EDGE ( 'NONE', *, *, #48227, .F. ) ;
#7292 = CARTESIAN_POINT ( 'NONE',  ( 10.78853149093999875, -80.47676253975309635, -3.242959171380999983 ) ) ;
#7293 = FACE_BOUND ( 'NONE', #30025, .T. ) ;
#7294 = AXIS2_PLACEMENT_3D ( 'NONE', #48241, #30487, #29331 ) ;
#7295 = CARTESIAN_POINT ( 'NONE',  ( -10.99069764842704622, -18.45457471225823554, -0.4531388007107930438 ) ) ;
#7296 = CARTESIAN_POINT ( 'NONE',  ( -9.943915246433000732, -78.72146835062000036, -7.799333767171999554 ) ) ;
#7297 = DIRECTION ( 'NONE',  ( -0.7071067811865475727, 0.000000000000000000, 0.7071067811865475727 ) ) ;
#7298 = CARTESIAN_POINT ( 'NONE',  ( -2.166619587182999851, -77.78611896097199008, 9.383974079751000730 ) ) ;
#7299 = CARTESIAN_POINT ( 'NONE',  ( -1.733002789576000069, -82.93980678759699288, 3.795625233452999847 ) ) ;
#7300 = CARTESIAN_POINT ( 'NONE',  ( 4.442379490556849220, -79.94120693519379017, 9.789819061409028578 ) ) ;
#7301 = CARTESIAN_POINT ( 'NONE',  ( -0.2833792192578999947, -79.88098110198900770, 1.589625787444000071 ) ) ;
#7302 = ORIENTED_EDGE ( 'NONE', *, *, #1337, .T. ) ;
#7303 = DIRECTION ( 'NONE',  ( -0.7071067811865475727, 0.000000000000000000, 0.7071067811865475727 ) ) ;
#7304 = CIRCLE ( 'NONE', #57270, 0.5000000000000006661 ) ;
#7305 = CARTESIAN_POINT ( 'NONE',  ( 2.437122208593068162, -78.97673430672129768, -2.628241071105698712 ) ) ;
#7306 = B_SPLINE_CURVE_WITH_KNOTS ( 'NONE', 3,
 ( #45237, #26607, #44644, #54386, #13923, #53798, #31918, #13332, #57922, #31326, #8919, #26041, #22494, #32494, #24247, #10681, #49963 ),
 .UNSPECIFIED., .F., .F.,
 ( 4, 2, 2, 2, 2, 2, 1, 2, 4 ),
 ( 0.000000000000000000, 0.1250000000000000555, 0.2500000000000001110, 0.3750000000000001665, 0.5000000000000002220, 0.6250000000000002220, 0.7500000000000003331, 0.8750000000000001110, 1.000000000000000000 ),
 .UNSPECIFIED. ) ;
#7307 = VERTEX_POINT ( 'NONE', #39289 ) ;
#7308 = CARTESIAN_POINT ( 'NONE',  ( -10.06692847420048054, -60.50343452148293721, -7.655995225848112540 ) ) ;
#7309 = CARTESIAN_POINT ( 'NONE',  ( -11.05562359778000214, -79.85724572043098135, 1.903787264327999829 ) ) ;
#7310 = ORIENTED_EDGE ( 'NONE', *, *, #18821, .T. ) ;
#7311 = ADVANCED_FACE ( 'NONE', ( #47608 ), #25133, .T. ) ;
#7312 = EDGE_LOOP ( 'NONE', ( #57709, #34099, #53274, #27921, #9871, #25868 ) ) ;
#7313 = VERTEX_POINT ( 'NONE', #11284 ) ;
#7314 = CARTESIAN_POINT ( 'NONE',  ( 0.4619589256644854869, -80.44498959896617407, 1.161429065943083039 ) ) ;
#7315 = DIRECTION ( 'NONE',  ( -1.000000000000000000, 0.000000000000000000, 1.155082973713998813E-13 ) ) ;
#7316 = CARTESIAN_POINT ( 'NONE',  ( 8.985706068735000329, -79.84810805933004474, -3.828549499589000149 ) ) ;
#7317 = VERTEX_POINT ( 'NONE', #7421 ) ;
#7318 = EDGE_CURVE ( 'NONE', #13397, #30070, #2140, .T. ) ;
#7319 = ORIENTED_EDGE ( 'NONE', *, *, #21880, .F. ) ;
#7320 = CARTESIAN_POINT ( 'NONE',  ( -2.787277769084570256, -80.70420168586483101, -10.40646178475631878 ) ) ;
#7321 = EDGE_CURVE ( 'NONE', #27203, #18938, #48596, .T. ) ;
#7322 = CARTESIAN_POINT ( 'NONE',  ( -0.03284986460708162054, -78.91452042059380290, -3.485344413137181352 ) ) ;
#7323 = VECTOR ( 'NONE', #26923, 1000.000000000000000 ) ;
#7324 = CARTESIAN_POINT ( 'NONE',  ( 12.56594317825999951, -60.05000001354000005, -1.750000000000000000 ) ) ;
#7325 = CARTESIAN_POINT ( 'NONE',  ( 0.9218200799623692543, -80.72291666666664867, 1.199500263597272687 ) ) ;
#7326 = CARTESIAN_POINT ( 'NONE',  ( -1.199500263597274241, -81.34791666666666288, 0.9218200799623669228 ) ) ;
#7327 = CARTESIAN_POINT ( 'NONE',  ( 8.386131694562763528, -78.75687913613843705, -4.924049977871809425 ) ) ;
#7328 = CYLINDRICAL_SURFACE ( 'NONE', #47812, 9.500000000000000000 ) ;
#7329 = CIRCLE ( 'NONE', #50720, 1.750000000000002220 ) ;
#7330 = CARTESIAN_POINT ( 'NONE',  ( 9.789819849890999848, -78.85111807705811771, -6.904744247936999813 ) ) ;
#7331 = CARTESIAN_POINT ( 'NONE',  ( -2.448851404991599701, -81.91822918149604504, -3.178239416597233191 ) ) ;
#7332 = CARTESIAN_POINT ( 'NONE',  ( -7.624757096123999212, -23.80351363819999833, 10.47516529248999895 ) ) ;
#7333 = CARTESIAN_POINT ( 'NONE',  ( 4.161008951361999664, -79.48030496681158752, 0.3099466714955000368 ) ) ;
#7334 = CARTESIAN_POINT ( 'NONE',  ( -2.421167930323375295, -77.89583333333331439, 9.009247259181911716 ) ) ;
#7335 = EDGE_CURVE ( 'NONE', #56888, #36961, #32251, .T. ) ;
#7336 = CARTESIAN_POINT ( 'NONE',  ( 10.19022265129000004, -59.99634105610000034, -7.646946115762000673 ) ) ;
#7337 = AXIS2_PLACEMENT_3D ( 'NONE', #54988, #14536, #20151 ) ;
#7338 = CARTESIAN_POINT ( 'NONE',  ( 12.16303714866999997, -79.24287182625000980, 1.568404430622000190 ) ) ;
#7339 = CARTESIAN_POINT ( 'NONE',  ( 10.16964605767000052, -76.20095892987599484, -6.884832982024000181 ) ) ;
#7340 = CARTESIAN_POINT ( 'NONE',  ( -7.345153731672117381, -60.02841244177280089, -8.188331488387708745 ) ) ;
#7341 = CARTESIAN_POINT ( 'NONE',  ( 11.75000000000000000, -77.95000000000000284, 2.316376715183999699E-14 ) ) ;
#7342 = CARTESIAN_POINT ( 'NONE',  ( 0.9995835529977264988, -78.69791666666664298, -0.7681833999686417114 ) ) ;
#7343 = B_SPLINE_CURVE_WITH_KNOTS ( 'NONE', 3,
 ( #46269, #41523, #32640, #18512, #50692, #37670, #32067, #19385, #1107, #9361, #23799, #41815, #6086, #1390, #46562, #54532, #37376, #45389, #55689, #55391, #24095, #14937, #36506, #14069, #50978, #28512, #50107, #49815, #45681, #5221, #23226, #41230, #820, #25543, #42987, #2544, #37959, #42408, #47433, #20259, #42695, #11695, #11406, #19973, #2259, #20827, #43561, #3127, #11980, #46851, #56273, #55983, #39124, #15533, #51564, #51274, #48009, #52137, #52423, #21117, #24967, #15235, #29385, #33228, #20547, #24394, #38251, #1978, #43276, #10828, #15824, #7544, #34391, #29671 ),
 .UNSPECIFIED., .F., .F.,
 ( 4, 2, 2, 1, 2, 2, 2, 2, 1, 1, 1, 2, 2, 2, 2, 2, 1, 1, 2, 2, 2, 2, 2, 2, 2, 2, 1, 2, 2, 2, 2, 1, 2, 2, 2, 2, 2, 2, 2, 2, 4 ),
 ( 0.000000000000000000, 0.03125000000000469763, 0.04687500000000669603, 0.05468750000000768829, 0.05859375000000816708, 0.06250000000000864586, 0.09375000000000832667, 0.1093750000000081740, 0.1171875000000081185, 0.1210937500000085210, 0.1230468750000082712, 0.1240234375000081324, 0.1250000000000079936, 0.1875000000000035805, 0.2187500000000010270, 0.2343749999999996669, 0.2421874999999990286, 0.2460937499999984734, 0.2480468749999981681, 0.2499999999999978906, 0.2812499999999959477, 0.2968749999999949485, 0.3046874999999941158, 0.3124999999999932832, 0.3749999999999866218, 0.3906249999999853451, 0.3984374999999846789, 0.4023437499999846234, 0.4062499999999845124, 0.4218749999999843459, 0.4296874999999840128, 0.4335937499999837907, 0.4355468749999836797, 0.4374999999999836242, 0.4687499999999834577, 0.4843749999999837352, 0.4999999999999839573, 0.6249999999999878986, 0.7499999999999918954, 0.8749999999999960032, 1.000000000000000000 ),
 .UNSPECIFIED. ) ;
#7344 = CARTESIAN_POINT ( 'NONE',  ( -1.177014466106575785, -80.19325593536987640, 1.006209693435321739 ) ) ;
#7345 = CARTESIAN_POINT ( 'NONE',  ( -0.8153671514888000127, -77.13888932676817944, -9.346629228026998248 ) ) ;
#7346 = CARTESIAN_POINT ( 'NONE',  ( 1.250000000000000000, -79.25000000000000000, 0.000000000000000000 ) ) ;
#7347 = CARTESIAN_POINT ( 'NONE',  ( -1.500000000000000222, -78.51041666666665719, -0.1963495408493622085 ) ) ;
#7348 = CARTESIAN_POINT ( 'NONE',  ( 0.1941442403254999838, -3.685159174984999897, -3.395596365263000127 ) ) ;
#7349 = EDGE_CURVE ( 'NONE', #32986, #28865, #20712, .T. ) ;
#7350 = CARTESIAN_POINT ( 'NONE',  ( -4.148749056195000229, -78.34383169849499495, 11.43548913926000132 ) ) ;
#7351 = CARTESIAN_POINT ( 'NONE',  ( 1.492456682423999981, -77.40805598037698587, -9.624565956529000488 ) ) ;
#7353 = CARTESIAN_POINT ( 'NONE',  ( -0.9319389680074999793, -79.29901557144499691, -0.8127712196805999545 ) ) ;
#7352 = CARTESIAN_POINT ( 'NONE',  ( -10.29258502670653996, -75.80000000000002558, 5.813495078707884289 ) ) ;
#7354 = CARTESIAN_POINT ( 'NONE',  ( -0.6878774159238000285, -81.72954691737999156, -1.297410027194999982 ) ) ;
#7355 = CARTESIAN_POINT ( 'NONE',  ( -7.651160336694000641, -22.76232686216999923, 10.45205658994000153 ) ) ;
#7356 = EDGE_LOOP ( 'NONE', ( #54217, #9280, #21038, #49196 ) ) ;
#7357 = EDGE_CURVE ( 'NONE', #587, #54702, #38711, .T. ) ;
#7358 = CARTESIAN_POINT ( 'NONE',  ( -10.07722254365999959, -21.74800977511999989, -7.718368845776000242 ) ) ;
#7359 = CARTESIAN_POINT ( 'NONE',  ( -2.713839119949000178, -79.36594721108400563, -11.84948027859999975 ) ) ;
#7360 = CARTESIAN_POINT ( 'NONE',  ( -9.499053022854020867, -79.25075071779494351, -0.08961454088966377962 ) ) ;
#7361 = CARTESIAN_POINT ( 'NONE',  ( 12.00000000000000000, -79.65000000000000568, 0.000000000000000000 ) ) ;
#7362 = CARTESIAN_POINT ( 'NONE',  ( -8.227501432806000992, -61.62538814575999879, 9.516269855012000178 ) ) ;
#7363 = CARTESIAN_POINT ( 'NONE',  ( 0.008285467789246998838, -1.006281426753999897, 3.701232203711000146 ) ) ;
#7364 = CARTESIAN_POINT ( 'NONE',  ( 3.258261448710999986, -80.11910146897098173, 9.339172452763000010 ) ) ;
#7365 = FACE_OUTER_BOUND ( 'NONE', #3818, .T. ) ;
#7366 = CARTESIAN_POINT ( 'NONE',  ( -9.250000000000000000, -78.99999999999998579, 0.000000000000000000 ) ) ;
#7367 = ORIENTED_EDGE ( 'NONE', *, *, #53025, .T. ) ;
#7368 = CARTESIAN_POINT ( 'NONE',  ( 9.886237701395979016, -76.56117323583245593, -5.228809800238466643 ) ) ;
#7369 = CARTESIAN_POINT ( 'NONE',  ( 1.200560589828618463, -79.41667105627126944, 11.71043212083842455 ) ) ;
#7370 = CARTESIAN_POINT ( 'NONE',  ( 4.163570051248999704, -79.48139334753599883, -8.653020802693998093 ) ) ;
#7371 = B_SPLINE_SURFACE_WITH_KNOTS ( 'NONE', 3, 3, ( 
 ( #53107, #13530, #57527, #44837 ),
 ( #22087, #31522, #48684, #8228 ),
 ( #31226, #18793, #3798, #21800 ),
 ( #49571, #22392, #9118, #39805 ),
 ( #27104, #49265, #58114, #8816 ),
 ( #57818, #45141, #296, #17377 ),
 ( #35364, #53389, #17676, #26808 ),
 ( #40403, #5548, #55446, #19434 ) ),
 .UNSPECIFIED., .F., .F., .F.,
 ( 4, 1, 1, 1, 1, 4 ),
 ( 4, 4 ),
 ( -0.01200407347464999865, 0.000000000000000000, 0.3333333333333000081, 0.6666666666667000474, 1.000000000000000000, 1.011997855551999947 ),
 ( -0.3559705542741999906, 1.355970554273999928 ),
 .UNSPECIFIED. ) ;
#7372 = CARTESIAN_POINT ( 'NONE',  ( 11.75000000000000000, -76.05000000000001137, 0.000000000000000000 ) ) ;
#7373 = CARTESIAN_POINT ( 'NONE',  ( -1.570423240223999928, -80.91589829417999624, -0.5559045111934000083 ) ) ;
#7374 = VERTEX_POINT ( 'NONE', #42577 ) ;
#7375 = CARTESIAN_POINT ( 'NONE',  ( -0.5692623238608193192, -78.23835482855749035, -1.139807222690662147 ) ) ;
#7376 = DIRECTION ( 'NONE',  ( 0.000000000000000000, 0.000000000000000000, -1.000000000000000000 ) ) ;
#7377 = CARTESIAN_POINT ( 'NONE',  ( 3.325194823509913800, -82.39999680491617084, -0.7067916523664262707 ) ) ;
#7378 = B_SPLINE_CURVE_WITH_KNOTS ( 'NONE', 3,
 ( #49860, #27683, #13524, #45728, #22684, #5263, #32396, #31516, #55440, #19134, #37129, #6131, #29141, #41568, #56317, #46605, #23843, #28557 ),
 .UNSPECIFIED., .F., .F.,
 ( 4, 2, 2, 2, 2, 2, 2, 2, 4 ),
 ( 0.000000000000000000, 0.1250000000000000000, 0.2500000000000000000, 0.3750000000000000000, 0.5000000000000000000, 0.6250000000000000000, 0.7500000000000000000, 0.8750000000000000000, 1.000000000000000000 ),
 .UNSPECIFIED. ) ;
#7379 = CARTESIAN_POINT ( 'NONE',  ( -1.250000000000001332, -78.48958333333332860, 0.1636246173744632659 ) ) ;
#7380 = CARTESIAN_POINT ( 'NONE',  ( -4.373213035511999358, -79.29760296238899286, -8.733596771889999388 ) ) ;
#7381 = VERTEX_POINT ( 'NONE', #16573 ) ;
#7382 = ORIENTED_EDGE ( 'NONE', *, *, #25049, .F. ) ;
#7383 = CARTESIAN_POINT ( 'NONE',  ( -3.791916262795000048, -77.22593890759399926, 12.00392988483999979 ) ) ;
#7384 = CARTESIAN_POINT ( 'NONE',  ( -4.602027720686207246, -78.68996782829300685, -9.715060958940219038 ) ) ;
#7385 = EDGE_CURVE ( 'NONE', #42268, #22499, #3289, .T. ) ;
#7386 = VERTEX_POINT ( 'NONE', #3000 ) ;
#7387 = CARTESIAN_POINT ( 'NONE',  ( 8.541162059891000524, -16.99199348450000002, 9.205819316576999256 ) ) ;
#7388 = CARTESIAN_POINT ( 'NONE',  ( 5.539808784079868431, -77.53333333333331723, 9.611650271896850839 ) ) ;
#7389 = CARTESIAN_POINT ( 'NONE',  ( -3.075537641221531615, -75.90416666666669698, -11.44417895085270942 ) ) ;
#7390 = CARTESIAN_POINT ( 'NONE',  ( 5.621201030502000151, -78.50735805811000034, 11.49883638144000031 ) ) ;
#7391 = DIRECTION ( 'NONE',  ( 0.000000000000000000, -1.000000000000000000, 0.000000000000000000 ) ) ;
#7392 = FACE_OUTER_BOUND ( 'NONE', #38607, .T. ) ;
#7393 = CARTESIAN_POINT ( 'NONE',  ( -0.9218200799623775810, -79.92708333333332860, 1.199500263597266247 ) ) ;
#7394 = CARTESIAN_POINT ( 'NONE',  ( 1.099819419251000019, -79.70107910926499528, 11.16281809564999961 ) ) ;
#7395 = B_SPLINE_CURVE_WITH_KNOTS ( 'NONE', 3,
 ( #16226, #25361, #57522, #48115, #44240, #34206, #29774, #52243, #43377, #57239, #11799, #2936, #20935, #38937, #16514, #34496, #43672, #3230, #21221, #39226, #16803, #52812, #18846, #31515, #8808, #49563, #41276, #45727 ),
 .UNSPECIFIED., .F., .F.,
 ( 4, 2, 2, 2, 2, 1, 2, 2, 1, 2, 2, 2, 2, 2, 4 ),
 ( 0.000000000000000000, 0.06249999999999986122, 0.1249999999999997224, 0.2499999999999994449, 0.3749999999999991673, 0.4374999999999991118, 0.4687499999999991118, 0.4999999999999991118, 0.5624999999999994449, 0.5937499999999994449, 0.6249999999999994449, 0.7499999999999996669, 0.8124999999999997780, 0.8749999999999997780, 1.000000000000000000 ),
 .UNSPECIFIED. ) ;
#7396 = CARTESIAN_POINT ( 'NONE',  ( -0.7274841066961533764, -79.98136092145524856, 9.221286261669808582 ) ) ;
#7397 = ORIENTED_EDGE ( 'NONE', *, *, #42096, .T. ) ;
#7398 = CARTESIAN_POINT ( 'NONE',  ( 11.75000000000000000, -78.04999999999999716, 0.000000000000000000 ) ) ;
#7399 = VERTEX_POINT ( 'NONE', #39002 ) ;
#7400 = CARTESIAN_POINT ( 'NONE',  ( 9.951586773259000651, -79.83198580643298214, -5.281558014135000256 ) ) ;
#7401 = CARTESIAN_POINT ( 'NONE',  ( 9.249992181567158411, -77.35008848816909222, 0.01013385650330413286 ) ) ;
#7402 = CARTESIAN_POINT ( 'NONE',  ( 1.407029943534999994, -80.03751491957400788, -0.1741439582578000189 ) ) ;
#7403 = CARTESIAN_POINT ( 'NONE',  ( -1.217465845835394411, -83.02083333333330017, -0.3271848554491003647 ) ) ;
#7404 = CARTESIAN_POINT ( 'NONE',  ( -0.8254061940140534626, -77.46904722746734251, -11.18661314154779873 ) ) ;
#7405 = CARTESIAN_POINT ( 'NONE',  ( -0.6149910796752999786, -78.95554938902999709, 1.385894317580000035 ) ) ;
#7406 = CARTESIAN_POINT ( 'NONE',  ( -7.836764916109927093, -61.10511429613131895, -9.850487231183631565 ) ) ;
#7408 = EDGE_CURVE ( 'NONE', #10164, #42165, #45675, .T. ) ;
#7407 = CIRCLE ( 'NONE', #56429, 9.500000000000000000 ) ;
#7409 = CARTESIAN_POINT ( 'NONE',  ( 9.393203674808260573, -80.79166666666664298, 5.413904038987188194 ) ) ;
#7410 = CARTESIAN_POINT ( 'NONE',  ( -0.7213013439201000354, -77.91806885964999196, -1.458901041394999876 ) ) ;
#7411 = DIRECTION ( 'NONE',  ( 0.000000000000000000, 1.000000000000000000, 0.000000000000000000 ) ) ;
#7412 = CARTESIAN_POINT ( 'NONE',  ( -7.626500902217000721, -23.31584477285000290, 10.35747158362999976 ) ) ;
#7413 = CARTESIAN_POINT ( 'NONE',  ( 0.9151062594318000176, -78.86146369488598395, 11.01092521911999889 ) ) ;
#7414 = ADVANCED_FACE ( 'NONE', ( #344 ), #22148, .T. ) ;
#7415 = CARTESIAN_POINT ( 'NONE',  ( -9.723174505940001211, -24.47697504200000296, -7.958760297012999807 ) ) ;
#7416 =( NAMED_UNIT ( * ) SI_UNIT ( $, .STERADIAN. ) SOLID_ANGLE_UNIT ( ) );
#7417 = CARTESIAN_POINT ( 'NONE',  ( 0.2488322192806999844, -85.11057975687899102, -3.538734592273999890 ) ) ;
#7418 = ORIENTED_EDGE ( 'NONE', *, *, #36938, .T. ) ;
#7419 = CARTESIAN_POINT ( 'NONE',  ( -1.156736691641969017, -77.19999999999998863, 10.75377114862106787 ) ) ;
#7420 = CARTESIAN_POINT ( 'NONE',  ( -0.2789364955927000067, -79.84686628078000581, 1.441751320050999929 ) ) ;
#7421 = CARTESIAN_POINT ( 'NONE',  ( -13.86363636363000218, -69.16102867818000277, -1.277888281761000050E-05 ) ) ;
#7422 = CARTESIAN_POINT ( 'NONE',  ( -11.92766985523999956, -77.57353354507900178, -1.116582401450000095 ) ) ;
#7423 = DIRECTION ( 'NONE',  ( 0.000000000000000000, -1.000000000000000000, 0.000000000000000000 ) ) ;
#7424 = CARTESIAN_POINT ( 'NONE',  ( -1.561527218546999940, -82.23949528173000090, -0.5804237711334999661 ) ) ;
#7425 = CONICAL_SURFACE ( 'NONE', #38529, 1.099999997149000430, 0.7853981633972997312 ) ;
#7426 = CARTESIAN_POINT ( 'NONE',  ( 2.780473330202828386, -2.052526692832529420, 2.160620055192048472 ) ) ;
#7427 = CARTESIAN_POINT ( 'NONE',  ( -7.603664017118000551, -78.63660584965400346, 6.060370778711000384 ) ) ;
#7428 = CARTESIAN_POINT ( 'NONE',  ( -8.606866362194999454, -77.67823810661599282, -4.073355822332000109 ) ) ;
#7429 = CARTESIAN_POINT ( 'NONE',  ( 0.8922764163254073289, -81.28868091437070120, -0.8857686078441138200 ) ) ;
#7430 = CARTESIAN_POINT ( 'NONE',  ( 6.160618408503998999, -78.35387449799000592, 9.012333039518999556 ) ) ;
#7431 = DIRECTION ( 'NONE',  ( 0.7071067811865475727, 0.000000000000000000, 0.7071067811865475727 ) ) ;
#7432 = CARTESIAN_POINT ( 'NONE',  ( 11.74991234329036516, -75.95242683881967594, 0.3799060071047825060 ) ) ;
#7433 = CARTESIAN_POINT ( 'NONE',  ( 1.273953344568438784, -81.40274971728671005, 0.04755539231170149983 ) ) ;
#7434 = VERTEX_POINT ( 'NONE', #36018 ) ;
#7435 = EDGE_CURVE ( 'NONE', #24723, #43107, #21697, .T. ) ;
#7436 = CARTESIAN_POINT ( 'NONE',  ( -1.210822168571097146, -78.88541666666667140, 9.249999999999992895 ) ) ;
#7437 = CARTESIAN_POINT ( 'NONE',  ( 3.077479315212850342, -77.05195087253886754, 11.44416613010283434 ) ) ;
#7438 = CARTESIAN_POINT ( 'NONE',  ( 5.120381413209000421, -79.16733796702099824, 11.15193929233999981 ) ) ;
#7439 = SHAPE_REPRESENTATION ( 'Body', ( #43526 ), #53938 ) ;
#7440 = CARTESIAN_POINT ( 'NONE',  ( 2.273238512818713808, -78.48547955770027329, -3.936100221940973309 ) ) ;
#7441 = CARTESIAN_POINT ( 'NONE',  ( 0.7311670807272000472, -82.16845028413999330, 1.496881327486000002 ) ) ;
#7442 = CARTESIAN_POINT ( 'NONE',  ( 3.176617583302000281, -79.72148250408599779, 10.50586082162000068 ) ) ;
#7443 = CARTESIAN_POINT ( 'NONE',  ( 10.30767511322000018, -23.74763733895999707, -7.634418707049000830 ) ) ;
#7444 = CARTESIAN_POINT ( 'NONE',  ( 0.5222397221428117797, -16.83701780599038145, 12.70447686583918134 ) ) ;
#7445 = CARTESIAN_POINT ( 'NONE',  ( -10.48589328409999943, -77.03442164589898766, 6.142604583596000367 ) ) ;
#7446 = CARTESIAN_POINT ( 'NONE',  ( 4.341671546774118262, -78.54407962236030016, 10.92272608737802386 ) ) ;
#7447 = CARTESIAN_POINT ( 'NONE',  ( -9.355938762769532957, -61.97483710998693596, 8.610912454485829315 ) ) ;
#7448 = EDGE_LOOP ( 'NONE', ( #36752, #54014, #50101, #42790 ) ) ;
#7449 = CARTESIAN_POINT ( 'NONE',  ( -10.85854583389000005, -79.12701249839500406, 1.947746583844000012 ) ) ;
#7450 = CARTESIAN_POINT ( 'NONE',  ( -1.226019641078067490, -80.08489572786606914, 0.2445129742201496981 ) ) ;
#7451 = LINE ( 'NONE', #11025, #30110 ) ;
#7452 = ADVANCED_FACE ( 'NONE', ( #49322 ), #44593, .F. ) ;
#7453 = CARTESIAN_POINT ( 'NONE',  ( 6.788068531828999497, -79.50272800141398477, 8.991721824839000732 ) ) ;
#7454 = AXIS2_PLACEMENT_3D ( 'NONE', #32283, #15166, #51207 ) ;
#7455 = CARTESIAN_POINT ( 'NONE',  ( -12.83044027763000017, -60.10639784916000394, -2.062670899361999766 ) ) ;
#7456 = CARTESIAN_POINT ( 'NONE',  ( 5.917523019358037040, -77.63333333333329733, 10.26699006316254525 ) ) ;
#7457 = CARTESIAN_POINT ( 'NONE',  ( -1.250000000000000000, -79.10000000000000853, 0.000000000000000000 ) ) ;
#7458 = CARTESIAN_POINT ( 'NONE',  ( 0.6087236336976633577, -82.69146269354659751, 1.385507257417856186 ) ) ;
#7459 = CARTESIAN_POINT ( 'NONE',  ( -0.4678443571040080129, -79.69481927908104524, -1.158927088315063969 ) ) ;
#7460 = AXIS2_PLACEMENT_3D ( 'NONE', #2005, #19410, #33555 ) ;
#7461 = CARTESIAN_POINT ( 'NONE',  ( 1.931087888049999979, -23.31584477285000290, 12.71658889741999943 ) ) ;
#7462 =( NAMED_UNIT ( * ) SI_UNIT ( $, .STERADIAN. ) SOLID_ANGLE_UNIT ( ) );
#7463 = CARTESIAN_POINT ( 'NONE',  ( -11.44417895085272008, -76.27916666666668277, 3.075537641221497420 ) ) ;
#7464 = ORIENTED_EDGE ( 'NONE', *, *, #8298, .T. ) ;
#7465 = ORIENTED_EDGE ( 'NONE', *, *, #18739, .F. ) ;
#7466 = CARTESIAN_POINT ( 'NONE',  ( -12.59651451715000015, -55.40944962329000134, -1.801708894189000043 ) ) ;
#7467 = AXIS2_PLACEMENT_3D ( 'NONE', #15873, #2877, #57177 ) ;
#7468 = EDGE_CURVE ( 'NONE', #47045, #37124, #26864, .T. ) ;
#7469 = EDGE_LOOP ( 'NONE', ( #26825, #36934, #24829, #25157 ) ) ;
#7470 = ORIENTED_EDGE ( 'NONE', *, *, #55973, .T. ) ;
#7471 = CARTESIAN_POINT ( 'NONE',  ( 1.199500263597268246, -81.80208333333625603, 0.9218200799623752495 ) ) ;
#7472 = CARTESIAN_POINT ( 'NONE',  ( 6.035973157159999936, -78.24568698277398937, -8.925829823522999362 ) ) ;
#7473 = AXIS2_PLACEMENT_3D ( 'NONE', #33166, #6900, #24332 ) ;
#7474 = CARTESIAN_POINT ( 'NONE',  ( -9.786657985941999982, -79.26948667140098337, -1.562668305794999934 ) ) ;
#7475 = CARTESIAN_POINT ( 'NONE',  ( 1.142746755879123777, -78.23489730971330403, -9.184199345809689774 ) ) ;
#7476 = CARTESIAN_POINT ( 'NONE',  ( 5.986115112277999195, -80.02851983374358724, 9.486000076385000312 ) ) ;
#7477 = VERTEX_POINT ( 'NONE', #40458 ) ;
#7478 = ORIENTED_EDGE ( 'NONE', *, *, #34032, .T. ) ;
#7479 = CARTESIAN_POINT ( 'NONE',  ( -7.060961830176961662, -77.54418585273785425, 5.975330936113271818 ) ) ;
#7480 = CARTESIAN_POINT ( 'NONE',  ( 2.386167682861000117, -77.16720924082279964, 10.77916482977000001 ) ) ;
#7481 = CARTESIAN_POINT ( 'NONE',  ( 1.250000000000000000, -18.75000000000000000, 12.00000000000000000 ) ) ;
#7482 = CARTESIAN_POINT ( 'NONE',  ( 5.091895231007000255, -78.66119465545499168, 8.260951054388000259 ) ) ;
#7483 = CARTESIAN_POINT ( 'NONE',  ( 7.653559626094000201, -18.70151115557999688, 10.01235002622999914 ) ) ;
#7484 = EDGE_CURVE ( 'NONE', #23569, #56133, #54045, .T. ) ;
#7485 = CARTESIAN_POINT ( 'NONE',  ( -1.821913034590999979E-14, -80.69999999923000189, -12.14999999923000118 ) ) ;
#7486 = CARTESIAN_POINT ( 'NONE',  ( -1.250000000000000000, -80.00000000000000000, 0.000000000000000000 ) ) ;
#7487 = CARTESIAN_POINT ( 'NONE',  ( -7.054457466615000172, -80.44093696116098613, -8.769379688592000122 ) ) ;
#7488 = CARTESIAN_POINT ( 'NONE',  ( 1.561568621681000080, -79.47054785055999560, 0.2753811681071999806 ) ) ;
#7489 = CARTESIAN_POINT ( 'NONE',  ( -0.4880156322679000125, -82.23603982111399091, -1.170357530120999856 ) ) ;
#7490 = AXIS2_PLACEMENT_3D ( 'NONE', #51202, #50617, #37013 ) ;
#7491 = CARTESIAN_POINT ( 'NONE',  ( -7.969034948568999077, -54.17623147781999648, 9.934750886883000121 ) ) ;
#7492 = CARTESIAN_POINT ( 'NONE',  ( -8.940852521590000990, -78.54043667140099672, -4.009928423322000057 ) ) ;
#7493 = CARTESIAN_POINT ( 'NONE',  ( 10.69384760718000038, -78.41447285264899847, -5.399785902169999652 ) ) ;
#7494 = CARTESIAN_POINT ( 'NONE',  ( -9.835237363972000324, -17.91864156569999977, -7.760968332719999196 ) ) ;
#7496 = DIRECTION ( 'NONE',  ( 1.000000000000000000, 0.000000000000000000, 0.000000000000000000 ) ) ;
#7495 = CARTESIAN_POINT ( 'NONE',  ( 7.640030139773000606, -60.10716934574000447, 10.18491068061999982 ) ) ;
#7497 = VECTOR ( 'NONE', #20508, 1000.000000000000000 ) ;
#7498 = CARTESIAN_POINT ( 'NONE',  ( 5.838193839761705917, -78.97708333333333997, -7.596835002782701629 ) ) ;
#7499 = CARTESIAN_POINT ( 'NONE',  ( -10.89465136399999956, -79.97499423886398517, 2.517158085631999942 ) ) ;
#7500 = FACE_OUTER_BOUND ( 'NONE', #28764, .T. ) ;
#7501 = CARTESIAN_POINT ( 'NONE',  ( -10.62993649278000063, -77.79662084572800040, 3.720001978191000092 ) ) ;
#7502 = CARTESIAN_POINT ( 'NONE',  ( 2.421239052663348268, -79.74628264568268321, -9.008702010510926783 ) ) ;
#7503 = CARTESIAN_POINT ( 'NONE',  ( 9.700000000000001066, -90.29999999999999716, 0.000000000000000000 ) ) ;
#7504 = EDGE_LOOP ( 'NONE', ( #10162, #13412, #18112, #21835, #32229 ) ) ;
#7505 = DIRECTION ( 'NONE',  ( 0.000000000000000000, 1.000000000000000000, 4.744707668127999788E-14 ) ) ;
#7506 = ADVANCED_FACE ( 'NONE', ( #45190 ), #31575, .F. ) ;
#7507 = CARTESIAN_POINT ( 'NONE',  ( -12.50686498859634455, -61.10484291343429675, 1.423095205018104936 ) ) ;
#7508 = CARTESIAN_POINT ( 'NONE',  ( 1.240145984052934303, -78.36013412040074400, 0.1580125328906592519 ) ) ;
#7509 = CARTESIAN_POINT ( 'NONE',  ( -0.06818180916829999494, -3.594953325257000287, 3.804809017442000396 ) ) ;
#7510 = CARTESIAN_POINT ( 'NONE',  ( -6.657338106343000383, -79.45823032903800254, 6.671287216456999403 ) ) ;
#7511 = AXIS2_PLACEMENT_3D ( 'NONE', #51242, #32610, #55362 ) ;
#7512 = CARTESIAN_POINT ( 'NONE',  ( -12.59682398755999877, -55.41262488626999527, 1.801644812721000077 ) ) ;
#7513 = CARTESIAN_POINT ( 'NONE',  ( 9.250000000000000000, -79.34999999999999432, 0.000000000000000000 ) ) ;
#7514 = DIRECTION ( 'NONE',  ( 0.000000000000000000, -1.000000000000000000, 0.000000000000000000 ) ) ;
#7515 = VECTOR ( 'NONE', #10175, 1000.000000000000000 ) ;
#7516 = CARTESIAN_POINT ( 'NONE',  ( 12.50000000000000000, -55.55000000209000177, 1.750000000000000000 ) ) ;
#7517 = ADVANCED_FACE ( 'NONE', ( #7996 ), #5013, .F. ) ;
#7518 = CARTESIAN_POINT ( 'NONE',  ( 2.322889965704216575, -78.67389998729011324, 4.022071092609738052 ) ) ;
#7519 = CARTESIAN_POINT ( 'NONE',  ( 0.9847086833720000154, -77.93903450768898722, -11.01265208048999966 ) ) ;
#7520 = B_SPLINE_CURVE_WITH_KNOTS ( 'NONE', 3,
 ( #10438, #5998, #18715, #19582, #55600, #14561, #28129, #36710, #23426, #32555, #23716, #41727, #15147, #33142, #1592, #51186, #29017, #16029, #7744, #52623, #33441, #34595, #29298, #42900, #38458, #25744, #11894, #20747, #51477, #12175, #3034, #52053, #38745, #21314, #21032, #38163, #39037, #57048, #16326, #3320, #11611, #29585, #16608, #7165, #30162, #48211, #43770, #39326, #24884, #7459, #56187, #15735, #56765, #57333, #33731, #11035, #47056, #56473, #34307, #6586, #2746, #52339, #24597, #29873, #47641, #51766, #25458, #43477, #42611, #6875, #2175, #11318 ),
 .UNSPECIFIED., .F., .F.,
 ( 4, 2, 2, 1, 1, 2, 2, 2, 2, 1, 1, 2, 2, 2, 2, 1, 1, 2, 2, 2, 2, 1, 1, 2, 2, 2, 2, 1, 1, 2, 2, 2, 2, 1, 2, 2, 2, 2, 1, 2, 2, 4 ),
 ( 0.000000000000000000, 0.06249999999999798772, 0.09374999999999730771, 0.1093749999999972800, 0.1171874999999975714, 0.1210937499999977102, 0.1249999999999978628, 0.1875000000000006661, 0.2187500000000024425, 0.2343750000000035805, 0.2421875000000041911, 0.2460937500000048017, 0.2500000000000053846, 0.3125000000000109357, 0.3437500000000133782, 0.3593750000000145994, 0.3671875000000155431, 0.3710937500000163203, 0.3750000000000170419, 0.4375000000000226485, 0.4687500000000254241, 0.4843750000000268119, 0.4921875000000275335, 0.4960937500000278666, 0.5000000000000281997, 0.5625000000000229816, 0.5937500000000199840, 0.6093750000000184297, 0.6171875000000176525, 0.6210937500000173195, 0.6250000000000169864, 0.6875000000000148770, 0.7187500000000138778, 0.7343750000000133227, 0.7421875000000127676, 0.7500000000000121014, 0.8125000000000074385, 0.8437500000000047740, 0.8593750000000034417, 0.8671875000000031086, 0.8750000000000026645, 1.000000000000000000 ),
 .UNSPECIFIED. ) ;
#7521 = CARTESIAN_POINT ( 'NONE',  ( 9.763034649155766687, -76.40254628798982139, -6.537437777648473336 ) ) ;
#7522 = CARTESIAN_POINT ( 'NONE',  ( -3.491544874602000359, -78.30851086359500357, -10.58601217070000189 ) ) ;
#7523 = CARTESIAN_POINT ( 'NONE',  ( 0.1585695142483192488, -81.96550636862359340, 1.239693765617767340 ) ) ;
#7524 = CARTESIAN_POINT ( 'NONE',  ( 9.100722152916000951, -76.99236172063068295, -3.274758550341999808 ) ) ;
#7525 = CARTESIAN_POINT ( 'NONE',  ( -4.658475568430831437, -78.41666666666665719, 8.082524092276877070 ) ) ;
#7526 = CARTESIAN_POINT ( 'NONE',  ( 0.4254240051736215000, -2.635416666666666963, -3.250000000000000000 ) ) ;
#7527 = CARTESIAN_POINT ( 'NONE',  ( 7.528911431583733105, -80.28673327718702524, -7.673874507591956551 ) ) ;
#7528 = LINE ( 'NONE', #29368, #47622 ) ;
#7529 = CARTESIAN_POINT ( 'NONE',  ( -11.20698691283975457, -79.85327479178147314, -0.4743978281313153689 ) ) ;
#7530 = CARTESIAN_POINT ( 'NONE',  ( -9.625846388754000671, -79.04949995641999294, -7.214584339064000318 ) ) ;
#7531 = CARTESIAN_POINT ( 'NONE',  ( -2.486604901413195456, -78.69583333333335418, 9.252740428348991131 ) ) ;
#7532 = CARTESIAN_POINT ( 'NONE',  ( -10.43948758838000046, -79.85401229401848866, -4.225051887250999449 ) ) ;
#7533 = CARTESIAN_POINT ( 'NONE',  ( 8.596672926062478126, -77.40213772681489957, 6.606658478622017938 ) ) ;
#7534 = ORIENTED_EDGE ( 'NONE', *, *, #4383, .T. ) ;
#7535 = CARTESIAN_POINT ( 'NONE',  ( 0.000000000000000000, -60.04999999966999980, -12.50000000000000000 ) ) ;
#7536 = EDGE_CURVE ( 'NONE', #49070, #30255, #43568, .T. ) ;
#7537 = ORIENTED_EDGE ( 'NONE', *, *, #851, .F. ) ;
#7538 = EDGE_LOOP ( 'NONE', ( #22415, #14478, #37446, #32918 ) ) ;
#7539 = DIRECTION ( 'NONE',  ( 0.000000000000000000, -1.000000000000000000, 0.000000000000000000 ) ) ;
#7540 = ORIENTED_EDGE ( 'NONE', *, *, #14271, .T. ) ;
#7541 = CARTESIAN_POINT ( 'NONE',  ( -2.501200655902999781, -81.56849421602200323, 2.511765616718999894 ) ) ;
#7542 = CARTESIAN_POINT ( 'NONE',  ( 2.946058150294987410, -79.24962501036633000, 9.031517904169495736 ) ) ;
#7543 = EDGE_LOOP ( 'NONE', ( #21464, #37603, #20753, #46193 ) ) ;
#7544 = CARTESIAN_POINT ( 'NONE',  ( -1.217816995976848338, -82.62131526224676747, -0.3277238727207466007 ) ) ;
#7545 = CARTESIAN_POINT ( 'NONE',  ( 5.684557159767975598, -79.67708333333332860, -7.396918292183157106 ) ) ;
#7546 = ORIENTED_EDGE ( 'NONE', *, *, #55086, .T. ) ;
#7547 = CARTESIAN_POINT ( 'NONE',  ( -0.9418125538657827756, -79.54291035859898784, 0.8257868174826785701 ) ) ;
#7548 = CARTESIAN_POINT ( 'NONE',  ( 4.044903269867999640, -79.46000000000000796, -8.595856998426999240 ) ) ;
#7549 = B_SPLINE_CURVE_WITH_KNOTS ( 'NONE', 3,
 ( #14485, #18642, #45216, #23351, #13903, #5627, #9487, #5057 ),
 .UNSPECIFIED., .F., .F.,
 ( 4, 2, 2, 4 ),
 ( 0.000000000000000000, 0.4999999999999946709, 0.7499999999999973355, 1.000000000000000000 ),
 .UNSPECIFIED. ) ;
#7550 = CARTESIAN_POINT ( 'NONE',  ( 0.9278077006636087365, -79.79999999999996874, 11.94918470935973254 ) ) ;
#7551 = CARTESIAN_POINT ( 'NONE',  ( -10.22334447120701739, -80.07501482205131538, 3.323462178327394323 ) ) ;
#7552 = AXIS2_PLACEMENT_3D ( 'NONE', #19897, #24321, #28142 ) ;
#7553 = DIRECTION ( 'NONE',  ( 0.000000000000000000, -1.000000000000000000, 0.000000000000000000 ) ) ;
#7554 = CARTESIAN_POINT ( 'NONE',  ( 2.439046057298411174, -86.39318692614398287, -3.425479544976959279 ) ) ;
#7555 = CARTESIAN_POINT ( 'NONE',  ( 8.332845033087998843, -76.02681988274399316, -7.273191856730000460 ) ) ;
#7556 = CARTESIAN_POINT ( 'NONE',  ( 4.812343589168453839, -79.02604166667481422, 10.81843774669307656 ) ) ;
#7557 = LINE ( 'NONE', #7268, #24058 ) ;
#7558 = CARTESIAN_POINT ( 'NONE',  ( -11.01492454107000007, -76.40176667242799624, -1.480222743997000157 ) ) ;
#7559 = CARTESIAN_POINT ( 'NONE',  ( -9.221951647947621566, -78.60624782743785488, -0.7198726630268430515 ) ) ;
#7560 = CARTESIAN_POINT ( 'NONE',  ( 1.137658753740000028, -79.51557416179699089, 0.6959227610743999870 ) ) ;
#7561 = CARTESIAN_POINT ( 'NONE',  ( -10.99980394231345926, -80.10023817985064909, 1.711188753626703361E-06 ) ) ;
#7562 = CARTESIAN_POINT ( 'NONE',  ( 2.295137415993966368, -2.913156379416062869, 2.300548530246512513 ) ) ;
#7563 = CARTESIAN_POINT ( 'NONE',  ( 3.496909181595999616, -80.85425264934799827, -0.5801637387983998861 ) ) ;
#7564 = CARTESIAN_POINT ( 'NONE',  ( -2.338276403494333966, -77.99259153130903144, 10.49268290638878831 ) ) ;
#7565 = LINE ( 'NONE', #12568, #36409 ) ;
#7566 = CARTESIAN_POINT ( 'NONE',  ( -1.490065003087000184, -84.95894503318798741, -3.218892454984999763 ) ) ;
#7567 = CARTESIAN_POINT ( 'NONE',  ( -2.422546195149999804, -2.212571010530000049, 2.935532677474999907 ) ) ;
#7568 = CARTESIAN_POINT ( 'NONE',  ( 10.07719973196000041, -20.25111654322000021, 7.718346056127999510 ) ) ;
#7569 = CARTESIAN_POINT ( 'NONE',  ( -9.310177428715999071, -61.93531023604000296, -8.596745825462999591 ) ) ;
#7570 = EDGE_CURVE ( 'NONE', #27444, #47291, #43657, .T. ) ;
#7571 = CARTESIAN_POINT ( 'NONE',  ( 0.000000000000000000, -74.70999999999999375, 0.000000000000000000 ) ) ;
#7572 = CARTESIAN_POINT ( 'NONE',  ( 1.246077061130999919, -80.89911715533600045, -0.4752592857455000264 ) ) ;
#7573 = VECTOR ( 'NONE', #33897, 1000.000000000000000 ) ;
#7574 = EDGE_CURVE ( 'NONE', #16529, #20818, #12606, .T. ) ;
#7575 = CARTESIAN_POINT ( 'NONE',  ( -1.199500263597270244, -80.45208333333333428, -0.9218200799623728070 ) ) ;
#7576 = CARTESIAN_POINT ( 'NONE',  ( -8.048032176077001054, -78.48332536818000449, 9.328081102756000220 ) ) ;
#7577 = CARTESIAN_POINT ( 'NONE',  ( -8.631379868284000167, -78.25656186178198936, 6.779623747090999686 ) ) ;
#7578 = CARTESIAN_POINT ( 'NONE',  ( 12.09999999999999964, -92.79999999999999716, 0.000000000000000000 ) ) ;
#7579 = CARTESIAN_POINT ( 'NONE',  ( -1.112866131775000156, -76.11229163771001538, -12.46277982123999983 ) ) ;
#7580 = ORIENTED_EDGE ( 'NONE', *, *, #53504, .T. ) ;
#7581 = CARTESIAN_POINT ( 'NONE',  ( 3.228614917279000185, -80.89813014380396794, -10.79283437469000084 ) ) ;
#7582 = CARTESIAN_POINT ( 'NONE',  ( 3.654181830570000233, -86.07389998728999103, -1.626946572303000105 ) ) ;
#7583 = EDGE_CURVE ( 'NONE', #56496, #21107, #56225, .T. ) ;
#7584 = CARTESIAN_POINT ( 'NONE',  ( -10.99606201159948426, -18.31532548059006515, -0.3145367810785520413 ) ) ;
#7585 = CARTESIAN_POINT ( 'NONE',  ( -10.99674072140000014, -79.21640068957000835, 5.906003873140000415 ) ) ;
#7586 = CARTESIAN_POINT ( 'NONE',  ( 0.000000000000000000, -76.10312499993298729, 0.000000000000000000 ) ) ;
#7587 = CARTESIAN_POINT ( 'NONE',  ( 7.515172033767000492, -78.75955723388199203, 5.847440938983000436 ) ) ;
#7588 = CARTESIAN_POINT ( 'NONE',  ( 0.3144568442405999975, -82.75050405486598493, 4.163020961247000606 ) ) ;
#7589 = CARTESIAN_POINT ( 'NONE',  ( 0.000000000000000000, -80.99999999999998579, 0.000000000000000000 ) ) ;
#7590 = CARTESIAN_POINT ( 'NONE',  ( -1.024999350969000078, -80.55902028819700433, -1.157050009743000096 ) ) ;
#7591 = ORIENTED_EDGE ( 'NONE', *, *, #5130, .T. ) ;
#7592 = FACE_OUTER_BOUND ( 'NONE', #49775, .T. ) ;
#7593 = CARTESIAN_POINT ( 'NONE',  ( -9.611650271896840181, -78.74166666666666003, -5.539808784079887083 ) ) ;
#7594 = AXIS2_PLACEMENT_3D ( 'NONE', #35454, #26317, #57909 ) ;
#7595 = CARTESIAN_POINT ( 'NONE',  ( 3.399999999999725908, -78.70000000000000284, 6.799999999999479350 ) ) ;
#7596 = ORIENTED_EDGE ( 'NONE', *, *, #8442, .F. ) ;
#7597 = CARTESIAN_POINT ( 'NONE',  ( -10.42531124903999995, -55.53514851492000304, 7.624341765436000173 ) ) ;
#7598 = CARTESIAN_POINT ( 'NONE',  ( 3.968454646034999644, -79.96041464100198937, -10.61226005143999984 ) ) ;
#7599 = EDGE_LOOP ( 'NONE', ( #53940, #25822, #46612, #21624, #36862 ) ) ;
#7600 = CARTESIAN_POINT ( 'NONE',  ( 6.958153983328000614, -78.86512485273199502, -9.837675768602998971 ) ) ;
#7601 = VERTEX_POINT ( 'NONE', #35129 ) ;
#7602 = ORIENTED_EDGE ( 'NONE', *, *, #35746, .T. ) ;
#7603 = CARTESIAN_POINT ( 'NONE',  ( 0.6623344797569685749, -80.43065007664468169, 1.060132421565134431 ) ) ;
#7604 = CARTESIAN_POINT ( 'NONE',  ( 9.393673072993333761, -77.99939921257045228, 7.217662729535765820 ) ) ;
#7605 = CARTESIAN_POINT ( 'NONE',  ( 9.226480760116999136, -79.36101818546501363, -2.263195259622999611 ) ) ;
#7606 = ORIENTED_EDGE ( 'NONE', *, *, #24294, .F. ) ;
#7607 = CARTESIAN_POINT ( 'NONE',  ( 12.77656766269999977, -53.48801851230000182, 0.1555695072194999973 ) ) ;
#7608 = VECTOR ( 'NONE', #54577, 1000.000000000000000 ) ;
#7609 = ORIENTED_EDGE ( 'NONE', *, *, #55721, .T. ) ;
#7610 = CARTESIAN_POINT ( 'NONE',  ( -3.911342194028000208, -78.64916925129686831, -11.62327352135999980 ) ) ;
#7611 = CARTESIAN_POINT ( 'NONE',  ( -0.03413113949348758891, -78.99318692614357929, -3.621286655835656898 ) ) ;
#7612 = EDGE_CURVE ( 'NONE', #35427, #18065, #53161, .T. ) ;
#7613 = CARTESIAN_POINT ( 'NONE',  ( 10.30768118222999874, -55.05239703883000146, 7.634415485482000108 ) ) ;
#7614 = CARTESIAN_POINT ( 'NONE',  ( 9.164374456839587069, -16.78432317405038532, -8.803712804485032350 ) ) ;
#7615 = CARTESIAN_POINT ( 'NONE',  ( 1.500000000000000000, -78.14999999999999147, 0.000000000000000000 ) ) ;
#7616 = DIRECTION ( 'NONE',  ( 0.7026410690473252618, -0.1122098755728027641, 0.7026410690473252618 ) ) ;
#7617 = CARTESIAN_POINT ( 'NONE',  ( -10.34301771562546435, -80.31833399541898189, 4.325112870545561705 ) ) ;
#7618 = CARTESIAN_POINT ( 'NONE',  ( -0.5337295926248202260, -77.94592315191539456, -1.412633301426811760 ) ) ;
#7619 = LINE ( 'NONE', #30035, #47309 ) ;
#7620 = CARTESIAN_POINT ( 'NONE',  ( -7.645398488021999839, -23.21531609142999741, 10.18948971874999998 ) ) ;
#7621 = CARTESIAN_POINT ( 'NONE',  ( -4.013619453071000542, -78.68490379462421913, 0.5804379921871000159 ) ) ;
#7622 = AXIS2_PLACEMENT_3D ( 'NONE', #58071, #9071, #27356 ) ;
#7623 = CARTESIAN_POINT ( 'NONE',  ( 7.596835002782719393, -78.09791666666666288, -5.838193839761677495 ) ) ;
#7624 = CARTESIAN_POINT ( 'NONE',  ( -12.43652237962999862, -17.07935153061999856, 0.1283967009857999997 ) ) ;
#7625 = CARTESIAN_POINT ( 'NONE',  ( 2.624826629463999694, -78.84050177318998465, 11.97953966613999910 ) ) ;
#7626 = CARTESIAN_POINT ( 'NONE',  ( 12.07535958108000074, -76.73373452783998516, -2.237927141218000404 ) ) ;
#7627 = CARTESIAN_POINT ( 'NONE',  ( -5.838193839761721016, -78.82708333333333428, 7.596835002782687418 ) ) ;
#7628 = CARTESIAN_POINT ( 'NONE',  ( 4.518722420425526742, -78.39451041693787658, 11.19879261494060962 ) ) ;
#7629 = DIRECTION ( 'NONE',  ( 0.000000000000000000, 0.000000000000000000, 1.000000000000000000 ) ) ;
#7631 = EDGE_CURVE ( 'NONE', #42169, #34312, #26285, .T. ) ;
#7630 = CARTESIAN_POINT ( 'NONE',  ( 1.292068742513557078, -81.04347613877415313, 0.7843776082647708758 ) ) ;
#7632 = CARTESIAN_POINT ( 'NONE',  ( 5.388524986465999866, -77.28388852172999179, 7.812415235880998843 ) ) ;
#7633 = CARTESIAN_POINT ( 'NONE',  ( 0.000000000000000000, -75.20000000000000284, -7.200000000000000178 ) ) ;
#7634 = CARTESIAN_POINT ( 'NONE',  ( 1.749722766158907650, -23.47588992887090953, 12.54673760678561223 ) ) ;
#7635 = CARTESIAN_POINT ( 'NONE',  ( 2.469846707035999955, -3.365950421107999802, 2.338639843265999829 ) ) ;
#7636 = CARTESIAN_POINT ( 'NONE',  ( 7.897520336252998874, -77.19073956883799781, -9.100831677656000096 ) ) ;
#7637 = CARTESIAN_POINT ( 'NONE',  ( -9.549999999999998934, -76.39999999999999147, 0.000000000000000000 ) ) ;
#7639 = CARTESIAN_POINT ( 'NONE',  ( -1.197912192620000038, -78.20753785706131112, 0.5527856627588000338 ) ) ;
#7638 = LINE ( 'NONE', #43949, #34484 ) ;
#7640 = CARTESIAN_POINT ( 'NONE',  ( -0.7723712723579999606, -81.22427319649999333, -1.248632555533999877 ) ) ;
#7641 = CARTESIAN_POINT ( 'NONE',  ( 0.000000000000000000, -78.59999999921299718, 0.000000000000000000 ) ) ;
#7642 = ORIENTED_EDGE ( 'NONE', *, *, #20193, .T. ) ;
#7643 = CARTESIAN_POINT ( 'NONE',  ( -10.24998526315000014, -21.75083378359999742, -7.705142895586000407 ) ) ;
#7644 = CARTESIAN_POINT ( 'NONE',  ( 10.80460657740000130, -79.40475467006099564, -5.315329678968999438 ) ) ;
#7645 = CARTESIAN_POINT ( 'NONE',  ( -5.226977690307169411, -79.32879368366329231, -7.969415024645670087 ) ) ;
#7646 = ADVANCED_FACE ( 'NONE', ( #35417 ), #53447, .F. ) ;
#7647 = CARTESIAN_POINT ( 'NONE',  ( 10.26699006316253637, -77.00833333333331154, -5.917523019358050362 ) ) ;
#7648 = CARTESIAN_POINT ( 'NONE',  ( -7.647735717269999789, -60.52294882350999927, 10.13404777204000062 ) ) ;
#7649 = CARTESIAN_POINT ( 'NONE',  ( -3.017608268723000364, -1.664752247162999854, -1.341678642855000048 ) ) ;
#7650 = CARTESIAN_POINT ( 'NONE',  ( 7.832365237661001345, -79.90583509515599303, -5.858077979548999892 ) ) ;
#7651 = CARTESIAN_POINT ( 'NONE',  ( 2.426647618366999603E-14, -5.949999999936560258, 0.000000000000000000 ) ) ;
#7652 = DIRECTION ( 'NONE',  ( 0.000000000000000000, -1.000000000000000000, 0.000000000000000000 ) ) ;
#7653 = ORIENTED_EDGE ( 'NONE', *, *, #11118, .T. ) ;
#7654 = CARTESIAN_POINT ( 'NONE',  ( -1.500000000000000000, -79.00000000000000000, 0.000000000000000000 ) ) ;
#7655 = FACE_OUTER_BOUND ( 'NONE', #9544, .T. ) ;
#7656 = FACE_OUTER_BOUND ( 'NONE', #36559, .T. ) ;
#7657 = CARTESIAN_POINT ( 'NONE',  ( 1.750000000001000089, -60.04999998641999781, -12.56594318054000148 ) ) ;
#7658 = CARTESIAN_POINT ( 'NONE',  ( -10.07719973194999952, -57.05111654290000445, -7.718346056122999954 ) ) ;
#7659 = CARTESIAN_POINT ( 'NONE',  ( 1.587978134902999994, -80.60404510987000037, 0.5035716945827000135 ) ) ;
#7660 = ORIENTED_EDGE ( 'NONE', *, *, #52934, .T. ) ;
#7661 = CYLINDRICAL_SURFACE ( 'NONE', #25666, 12.00000000000000000 ) ;
#7662 = AXIS2_PLACEMENT_3D ( 'NONE', #13776, #31180, #41235 ) ;
#7663 = CARTESIAN_POINT ( 'NONE',  ( -1.218691819105022001, -82.12147840418360545, -0.3276751685990938467 ) ) ;
#7664 = CARTESIAN_POINT ( 'NONE',  ( 1.799475304559999822, -58.55171076491000548, -12.69616050744000013 ) ) ;
#7665 = AXIS2_PLACEMENT_3D ( 'NONE', #14126, #50163, #27698 ) ;
#7666 = PRODUCT_RELATED_PRODUCT_CATEGORY ( 'part', '', ( #30452 ) ) ;
#7667 = CARTESIAN_POINT ( 'NONE',  ( -10.47018971533259446, -78.57921329502835306, 2.813858375529144862 ) ) ;
#7668 = CARTESIAN_POINT ( 'NONE',  ( 12.76303204513999923, -55.53514852210999919, -1.980584515753000208 ) ) ;
#7669 = ORIENTED_EDGE ( 'NONE', *, *, #11311, .F. ) ;
#7670 = VERTEX_POINT ( 'NONE', #46075 ) ;
#7671 = CARTESIAN_POINT ( 'NONE',  ( -3.213275664864000181, -77.36312553470499154, -12.04962829498999888 ) ) ;
#7672 = CARTESIAN_POINT ( 'NONE',  ( 0.03357693874575778253, -78.72534147169611174, -10.74990560618915936 ) ) ;
#7673 = ORIENTED_EDGE ( 'NONE', *, *, #56889, .F. ) ;
#7674 = CARTESIAN_POINT ( 'NONE',  ( 12.50686284816651472, -17.69510763146307397, 1.423064270789805574 ) ) ;
#7675 = EDGE_CURVE ( 'NONE', #51092, #54228, #24532, .T. ) ;
#7676 = CARTESIAN_POINT ( 'NONE',  ( 1.439896632895284911, -77.56458333333331723, 11.00000000000000355 ) ) ;
#7677 = CARTESIAN_POINT ( 'NONE',  ( 1.583004792641895531, -54.34790758811762146, 12.70616254407479140 ) ) ;
#7678 = CARTESIAN_POINT ( 'NONE',  ( 7.379132703266000348, -77.25467974817999561, -10.64946278274999969 ) ) ;
#7679 = EDGE_CURVE ( 'NONE', #26583, #3255, #13471, .T. ) ;
#7680 = CARTESIAN_POINT ( 'NONE',  ( 6.605974356996339836, -79.77709823288482482, -8.595918735704922042 ) ) ;
#7681 = PLANE ( 'NONE',  #4163 ) ;
#7682 = CARTESIAN_POINT ( 'NONE',  ( -1.310679582531389498, -79.95833333333335702, 0.7554284705563444335 ) ) ;
#7683 = CARTESIAN_POINT ( 'NONE',  ( 2.315902194296999728, -78.54323222745999544, -10.97517055051999968 ) ) ;
#7684 = CARTESIAN_POINT ( 'NONE',  ( 5.046009951596436949, -79.92957980094915627, 7.753141342909813716 ) ) ;
#7685 = VERTEX_POINT ( 'NONE', #1781 ) ;
#7686 = DIRECTION ( 'NONE',  ( 0.000000000000000000, -1.000000000000000000, 0.000000000000000000 ) ) ;
#7687 = ORIENTED_EDGE ( 'NONE', *, *, #43777, .F. ) ;
#7688 = CARTESIAN_POINT ( 'NONE',  ( 3.260743090391000187, -79.97244757809599491, 10.78408470153000032 ) ) ;
#7689 = CARTESIAN_POINT ( 'NONE',  ( 7.496060297333964506, -77.30026476220074017, -5.419471789427347197 ) ) ;
#7690 = CARTESIAN_POINT ( 'NONE',  ( 1.040651332726000078, -79.98790229619299907, -0.9628624948066000222 ) ) ;
#7691 = CARTESIAN_POINT ( 'NONE',  ( 0.000000000000000000, -80.99999999999998579, 5.800000000000029132 ) ) ;
#7692 = CARTESIAN_POINT ( 'NONE',  ( -10.86673736094340192, -76.86984768142733060, -2.781288557130109584 ) ) ;
#7693 = CARTESIAN_POINT ( 'NONE',  ( 1.360845176917000021, -78.26097266169459488, -0.6686124113221000309 ) ) ;
#7694 = DIRECTION ( 'NONE',  ( 0.000000000000000000, -1.000000000000000000, 0.000000000000000000 ) ) ;
#7695 = CARTESIAN_POINT ( 'NONE',  ( 1.250000000000000888, -81.73388662792250159, -0.2531082567149807172 ) ) ;
#7696 = CARTESIAN_POINT ( 'NONE',  ( -9.611650271896857944, -78.55833333333332291, 5.539808784079855997 ) ) ;
#7697 = B_SPLINE_CURVE_WITH_KNOTS ( 'NONE', 3,
 ( #27028, #4617, #40627, #46827, #52113, #11096, #6059, #33789, #51539, #24659, #28781, #42964, #2521, #50952, #24370, #20523, #55661, #6941, #38521, #56536, #6354, #2809, #56250, #1952, #42382, #42086, #11386, #37646, #10800, #2237, #42669, #10502, #29076, #33503, #16097 ),
 .UNSPECIFIED., .F., .F.,
 ( 4, 1, 1, 1, 1, 1, 1, 1, 1, 1, 1, 1, 1, 1, 1, 1, 1, 1, 1, 1, 1, 1, 1, 1, 1, 1, 1, 1, 1, 1, 1, 1, 4 ),
 ( 0.000000000000000000, 0.01250353271130624083, 0.04500329721509613301, 0.07750306171888603213, 0.1100028262226759312, 0.1425025907264658165, 0.1750023552302557295, 0.2075021197340456147, 0.2400018842378355277, 0.2725016487416254685, 0.3050014132454152982, 0.3375011777492052389, 0.3700009422529951242, 0.4025007067567850649, 0.4350004712605748947, 0.4675002357643648354, 0.5000000002681546096, 0.5324997647719444949, 0.5649995292757343801, 0.5974992937795243764, 0.6299990582833142616, 0.6624988227871041468, 0.6949985872908940321, 0.7274983517946840283, 0.7599981162984738026, 0.7924978808022636878, 0.8249976453060535730, 0.8574974098098435693, 0.8899971743136334545, 0.9224969388174233398, 0.9549967033212132250, 0.9874964678250032213, 1.000000000000000000 ),
 .UNSPECIFIED. ) ;
#7698 = CARTESIAN_POINT ( 'NONE',  ( -12.56594317819999951, -55.54999998572999687, -1.750000000000000000 ) ) ;
#7699 = CARTESIAN_POINT ( 'NONE',  ( 0.000000000000000000, -75.10000000032299283, 0.000000000000000000 ) ) ;
#7700 = CARTESIAN_POINT ( 'NONE',  ( -9.663285910017000546, -79.51527887665599792, 5.577858467032999812 ) ) ;
#7701 = CARTESIAN_POINT ( 'NONE',  ( 7.674627477108999507, -56.04922971914000129, 10.14950121126000049 ) ) ;
#7702 = CARTESIAN_POINT ( 'NONE',  ( -0.9103933733443999587, -79.76897164566861420, -11.99492895764000089 ) ) ;
#7703 = CARTESIAN_POINT ( 'NONE',  ( -2.066979895997999694, -79.92992088582298038, 3.624106733465999763 ) ) ;
#7704 = DIRECTION ( 'NONE',  ( 0.000000000000000000, -1.000000000000000000, 0.000000000000000000 ) ) ;
#7705 = ORIENTED_EDGE ( 'NONE', *, *, #14252, .F. ) ;
#7707 = EDGE_CURVE ( 'NONE', #51047, #29449, #33036, .T. ) ;
#7706 = CARTESIAN_POINT ( 'NONE',  ( -1.542276019614999827, -82.29518551926999237, 0.7219429580085000575 ) ) ;
#7708 = CARTESIAN_POINT ( 'NONE',  ( 0.7503380909894999951, -80.28898078654999892, 1.262315685543000221 ) ) ;
#7709 = DIRECTION ( 'NONE',  ( 4.134220892123999815E-14, -1.534448722697999916E-11, -1.000000000000000000 ) ) ;
#7710 = CARTESIAN_POINT ( 'NONE',  ( 7.919842512018000491, -77.38362833711200039, 8.988445846368000147 ) ) ;
#7711 = CARTESIAN_POINT ( 'NONE',  ( 2.858407197969000002, -77.00000000000000000, 8.797272775729998884 ) ) ;
#7712 = AXIS2_PLACEMENT_3D ( 'NONE', #20314, #10588, #2606 ) ;
#7713 = CARTESIAN_POINT ( 'NONE',  ( 0.5517547646476002043, -78.91101018058850514, -1.149559085547208426 ) ) ;
#7714 = CARTESIAN_POINT ( 'NONE',  ( -4.902828564081697316, -76.30798797490987795, 11.02313175347633667 ) ) ;
#7715 = CARTESIAN_POINT ( 'NONE',  ( 7.048436826466999428, -77.93776861655099708, 6.223291978577000449 ) ) ;
#7716 = CARTESIAN_POINT ( 'NONE',  ( 8.857396897828001769, -77.30170024541499174, -3.187116989308000026 ) ) ;
#7717 = CARTESIAN_POINT ( 'NONE',  ( 0.2796250015563770397, -81.24281920464285633, -1.222472053442152484 ) ) ;
#7718 = CARTESIAN_POINT ( 'NONE',  ( 11.75000000000000000, -75.95000000000000284, 0.000000000000000000 ) ) ;
#7719 = CARTESIAN_POINT ( 'NONE',  ( -0.4347137722153567307, -81.05291711652307640, 1.197434020721431125 ) ) ;
#7720 = ORIENTED_EDGE ( 'NONE', *, *, #40419, .F. ) ;
#7721 = DIRECTION ( 'NONE',  ( 0.000000000000000000, 1.000000000000000000, 0.000000000000000000 ) ) ;
#7722 = FACE_OUTER_BOUND ( 'NONE', #39453, .T. ) ;
#7723 = DIRECTION ( 'NONE',  ( 2.678932014865000134E-11, 1.000000000000000000, -2.678911359553000079E-11 ) ) ;
#7724 = FACE_OUTER_BOUND ( 'NONE', #54888, .T. ) ;
#7725 = EDGE_CURVE ( 'NONE', #41082, #52202, #23178, .T. ) ;
#7726 = CARTESIAN_POINT ( 'NONE',  ( 1.611423453808999984, -81.60001734814998997, 0.4225784326546000447 ) ) ;
#7727 = CARTESIAN_POINT ( 'NONE',  ( 9.028681611143001717, -78.13370064223998668, -5.970393136294000591 ) ) ;
#7728 = EDGE_CURVE ( 'NONE', #21905, #17178, #22925, .T. ) ;
#7729 = CARTESIAN_POINT ( 'NONE',  ( 2.836859645505057426, -80.35885416666536685, 10.55930595257627047 ) ) ;
#7730 = CARTESIAN_POINT ( 'NONE',  ( -6.587271542083999343, -76.92896184318099984, 10.35158977641000000 ) ) ;
#7731 = FACE_OUTER_BOUND ( 'NONE', #57988, .T. ) ;
#7732 = CARTESIAN_POINT ( 'NONE',  ( -1.500000000000000000, -77.89999999999999147, 0.000000000000000000 ) ) ;
#7733 = ORIENTED_EDGE ( 'NONE', *, *, #27870, .T. ) ;
#7734 = CARTESIAN_POINT ( 'NONE',  ( 8.500810681529999968, -79.90288448085529183, -7.210465973013999275 ) ) ;
#7735 = CARTESIAN_POINT ( 'NONE',  ( 3.549246799458173118, -77.34368329502935069, 8.572692145709080336 ) ) ;
#7736 = CARTESIAN_POINT ( 'NONE',  ( 5.684557159767946288, -78.17708333333332860, -7.396918292183178423 ) ) ;
#7737 = B_SPLINE_SURFACE_WITH_KNOTS ( 'NONE', 3, 3, ( 
 ( #1692, #14655, #1404, #19986 ),
 ( #24109, #832, #41241, #46280 ),
 ( #28226, #6100, #23236, #37095 ),
 ( #18813, #5805, #51286, #10245 ),
 ( #42424, #50705, #19395, #32365 ),
 ( #1993, #37387, #55406, #54823 ),
 ( #14951, #55111, #1116, #32653 ),
 ( #32948, #46574, #50991, #10541 ) ),
 .UNSPECIFIED., .F., .F., .F.,
 ( 4, 1, 1, 1, 1, 4 ),
 ( 4, 4 ),
 ( -0.01200407347462000007, 0.000000000000000000, 0.3333333333333000081, 0.6666666666667000474, 1.000000000000000000, 1.011997855551999947 ),
 ( -0.3559705542741999906, 1.355970554273999928 ),
 .UNSPECIFIED. ) ;
#7738 = B_SPLINE_CURVE_WITH_KNOTS ( 'NONE', 3,
 ( #40555, #36407, #22242, #4541, #31967, #22833, #8373, #40845, #439, #22545 ),
 .UNSPECIFIED., .F., .F.,
 ( 4, 2, 2, 2, 4 ),
 ( 0.000000000000000000, 0.2500000000000000555, 0.5000000000000001110, 0.7500000000000000000, 1.000000000000000000 ),
 .UNSPECIFIED. ) ;
#7739 = CARTESIAN_POINT ( 'NONE',  ( -10.85153605587000136, -79.66191800929898648, 2.386335476490000218 ) ) ;
#7740 = CARTESIAN_POINT ( 'NONE',  ( 7.374560639698993114, -76.97708333333332575, -9.596002108778149520 ) ) ;
#7741 = CARTESIAN_POINT ( 'NONE',  ( 5.894914467206975317, -77.90333333333336441, 7.125729969419699827 ) ) ;
#7742 = CARTESIAN_POINT ( 'NONE',  ( -7.651147547619999933, -59.56256650291999222, -10.45204383579000051 ) ) ;
#7743 = CARTESIAN_POINT ( 'NONE',  ( 1.348211372310171408, -82.64085315442503088, 0.7644857786683515455 ) ) ;
#7744 = CARTESIAN_POINT ( 'NONE',  ( 0.9013968416950485230, -79.78949536163368350, -0.8657002453825515254 ) ) ;
#7745 = EDGE_CURVE ( 'NONE', #26499, #41659, #45575, .T. ) ;
#7746 = DIRECTION ( 'NONE',  ( 0.000000000000000000, -1.000000000000000000, 0.000000000000000000 ) ) ;
#7747 = DIRECTION ( 'NONE',  ( 0.9957542233908819318, -0.04890176544946910064, -0.07798810124080861328 ) ) ;
#7748 = CARTESIAN_POINT ( 'NONE',  ( -12.78015149457000099, -24.30330660695999967, 1.806228889758999978 ) ) ;
#7749 = ORIENTED_EDGE ( 'NONE', *, *, #38374, .T. ) ;
#7750 = ORIENTED_EDGE ( 'NONE', *, *, #30956, .T. ) ;
#7751 = CARTESIAN_POINT ( 'NONE',  ( -12.43646312217999927, -53.87951485525000095, -0.1257251053154000153 ) ) ;
#7752 = TOROIDAL_SURFACE ( 'NONE', #37925, 13.50000000000000000, 0.5000000000000000000 ) ;
#7753 = ORIENTED_EDGE ( 'NONE', *, *, #45812, .T. ) ;
#7754 = CARTESIAN_POINT ( 'NONE',  ( 4.750030159171999777, -78.70865007999000795, -11.30647155123999958 ) ) ;
#7755 = EDGE_LOOP ( 'NONE', ( #1326, #57184, #32739, #54055 ) ) ;
#7756 = DIRECTION ( 'NONE',  ( 0.000000000000000000, -1.000000000000000000, 0.000000000000000000 ) ) ;
#7757 = CARTESIAN_POINT ( 'NONE',  ( 7.977342298186999692, -77.38320278771699634, 7.452340293345999456 ) ) ;
#7758 = CONTEXT_DEPENDENT_SHAPE_REPRESENTATION ( #1765, #29130 ) ;
#7759 = EDGE_CURVE ( 'NONE', #52628, #15626, #50587, .T. ) ;
#7760 = CARTESIAN_POINT ( 'NONE',  ( -0.6596342590195000133, -78.13718667140099683, 9.888746480308999054 ) ) ;
#7761 = CARTESIAN_POINT ( 'NONE',  ( 1.464740467520374123, -78.23771836109808930, -9.139813437711902466 ) ) ;
#7762 = CIRCLE ( 'NONE', #19102, 0.6000000000000008660 ) ;
#7763 = CARTESIAN_POINT ( 'NONE',  ( 10.93160348586000019, -78.96630245667299164, 2.513594203403000105 ) ) ;
#7764 = ORIENTED_EDGE ( 'NONE', *, *, #20729, .F. ) ;
#7765 = ORIENTED_EDGE ( 'NONE', *, *, #15022, .F. ) ;
#7766 = CARTESIAN_POINT ( 'NONE',  ( -6.071607140531662061, -77.53210482738238341, 6.979269262791448547 ) ) ;
#7767 = CARTESIAN_POINT ( 'NONE',  ( -0.5413127449341000874, -77.93064224879100266, -11.02683867434999954 ) ) ;
#7768 = SURFACE_SIDE_STYLE ('',( #52929 ) ) ;
#7769 = CARTESIAN_POINT ( 'NONE',  ( -12.43422056534000042, -61.23655741401000085, -1.197404442626999854 ) ) ;
#7770 = CARTESIAN_POINT ( 'NONE',  ( -5.159044788988000008, -77.35024324810899543, -8.219183903844999861 ) ) ;
#7771 = AXIS2_PLACEMENT_3D ( 'NONE', #37943, #51257, #11392 ) ;
#7772 = CARTESIAN_POINT ( 'NONE',  ( 7.864802647436849092, -61.25123893485678650, 10.10444599044500968 ) ) ;
#7773 = CARTESIAN_POINT ( 'NONE',  ( 7.730439324398687972, -54.67809618926516890, -10.25198230927261456 ) ) ;
#7774 = CARTESIAN_POINT ( 'NONE',  ( -10.49924843836999955, -80.45947872149298519, -4.054558598941000014 ) ) ;
#7775 = VECTOR ( 'NONE', #34773, 1000.000000000000000 ) ;
#7776 = B_SPLINE_CURVE_WITH_KNOTS ( 'NONE', 3,
 ( #29404, #32955, #10548, #1411, #46871, #38562, #24986, #5810, #23817, #28531 ),
 .UNSPECIFIED., .F., .F.,
 ( 4, 2, 2, 2, 4 ),
 ( 0.000000000000000000, 0.2500000000000000000, 0.5000000000000000000, 0.7500000000000000000, 1.000000000000000000 ),
 .UNSPECIFIED. ) ;
#7777 = CARTESIAN_POINT ( 'NONE',  ( 12.49996905250000090, -18.80797343466000271, -1.666511841114999948 ) ) ;
#7778 = CARTESIAN_POINT ( 'NONE',  ( 1.980464483675000054, -57.04439829357999514, 12.85140862645999782 ) ) ;
#7779 =( REPRESENTATION_RELATIONSHIP ('NONE','NONE', #58051, #7879 ) REPRESENTATION_RELATIONSHIP_WITH_TRANSFORMATION ( #57346 )SHAPE_REPRESENTATION_RELATIONSHIP( ) );
#7780 = EDGE_LOOP ( 'NONE', ( #11686, #22782, #55447, #10302, #41579, #6952, #36267 ) ) ;
#7781 = CARTESIAN_POINT ( 'NONE',  ( -9.205836503685999261, -53.79200673903999785, 8.541144771039000716 ) ) ;
#7782 = CARTESIAN_POINT ( 'NONE',  ( 11.53501176087999980, -78.92992984570099679, -3.234124663588000104 ) ) ;
#7783 = CARTESIAN_POINT ( 'NONE',  ( -9.996785040898998886, -17.84937852891999910, -7.758588586541999454 ) ) ;
#7785 = CARTESIAN_POINT ( 'NONE',  ( 7.919595949288999570, -57.79999999967000690, 8.909545442949999838 ) ) ;
#7784 = CARTESIAN_POINT ( 'NONE',  ( 7.626500902197000720, -55.48415522678000400, 10.35747158360999975 ) ) ;
#7786 = CARTESIAN_POINT ( 'NONE',  ( 2.600548699141073783, -1.299417036785829094, -1.998661137613467975 ) ) ;
#7787 =( NAMED_UNIT ( * ) PLANE_ANGLE_UNIT ( ) SI_UNIT ( $, .RADIAN. ) );
#7788 = CARTESIAN_POINT ( 'NONE',  ( -6.841895596235000099, -78.46354745617999527, -8.800175226803998996 ) ) ;
#7789 = CARTESIAN_POINT ( 'NONE',  ( -10.12290050124000018, -18.75000000007999645, 7.648026767085999822 ) ) ;
#7790 = CARTESIAN_POINT ( 'NONE',  ( -3.500000000146000101, -0.7499999998540000101, 2.054632350152999929E-08 ) ) ;
#7791 = ORIENTED_EDGE ( 'NONE', *, *, #45287, .T. ) ;
#7792 = DIRECTION ( 'NONE',  ( 0.000000000000000000, -1.000000000000000000, -8.830898975038999242E-14 ) ) ;
#7793 = CARTESIAN_POINT ( 'NONE',  ( -12.00000000000000000, -76.89999999999999147, 0.000000000000000000 ) ) ;
#7794 = CARTESIAN_POINT ( 'NONE',  ( -12.80896991329000123, -20.24546192895000019, 1.930989179114000143 ) ) ;
#7795 = CARTESIAN_POINT ( 'NONE',  ( 2.257397718401000120, -3.043015194441000215, 3.064303898428999862 ) ) ;
#7796 = CARTESIAN_POINT ( 'NONE',  ( -7.548024343608999764, -80.07190615245599474, -5.643896870619999895 ) ) ;
#7797 = VECTOR ( 'NONE', #23245, 1000.000000000000000 ) ;
#7798 = CARTESIAN_POINT ( 'NONE',  ( -12.43652237957999951, -53.87935153028999480, 0.1283967009859000308 ) ) ;
#7799 = CARTESIAN_POINT ( 'NONE',  ( 10.49438680834578719, -77.32500000000000284, -3.407966307000451334 ) ) ;
#7800 = CARTESIAN_POINT ( 'NONE',  ( 0.4356486348705999601, -61.68064955776999625, 12.43591427125000060 ) ) ;
#7801 = CARTESIAN_POINT ( 'NONE',  ( 9.500000000000001776, -79.14249999999998408, -0.8953539062730788700 ) ) ;
#7802 = CARTESIAN_POINT ( 'NONE',  ( 0.1949762683977999955, -86.11796544543098264, 3.958270212781000108 ) ) ;
#7803 = DIRECTION ( 'NONE',  ( 1.000000000000000000, 0.000000000000000000, 0.000000000000000000 ) ) ;
#7804 = CIRCLE ( 'NONE', #40796, 5.500000000000000000 ) ;
#7805 = CARTESIAN_POINT ( 'NONE',  ( -1.989802025464000090, -77.26035782317299550, 10.76548307208999944 ) ) ;
#7806 = CARTESIAN_POINT ( 'NONE',  ( 10.84423179882955779, -76.41830951051049681, -4.523413806819045924 ) ) ;
#7807 = CARTESIAN_POINT ( 'NONE',  ( 2.927762776937000044, -77.28751179411899841, -10.63625589685999984 ) ) ;
#7808 = B_SPLINE_CURVE_WITH_KNOTS ( 'NONE', 3,
 ( #23739, #23448, #50625, #41753 ),
 .UNSPECIFIED., .F., .F.,
 ( 4, 4 ),
 ( 0.000000000000000000, 1.000000000000000000 ),
 .UNSPECIFIED. ) ;
#7809 = CARTESIAN_POINT ( 'NONE',  ( 1.199399675185978564, -81.87278530070058480, 0.3527059046770779083 ) ) ;
#7810 = CARTESIAN_POINT ( 'NONE',  ( 7.601397897754999633, -18.75000000310999937, -10.07627163191000008 ) ) ;
#7811 = CARTESIAN_POINT ( 'NONE',  ( 4.067416459488999436, -79.23084805011500009, -8.418325902196000854 ) ) ;
#7812 = CARTESIAN_POINT ( 'NONE',  ( -5.539808784079933268, -77.51666666666667993, 9.611650271896811759 ) ) ;
#7813 = CARTESIAN_POINT ( 'NONE',  ( 4.114391408450323695, -80.25633541559250261, -9.931419796240385622 ) ) ;
#7814 = CARTESIAN_POINT ( 'NONE',  ( -1.624989163556999772E-14, -74.69999999881999031, 0.000000000000000000 ) ) ;
#7815 = CARTESIAN_POINT ( 'NONE',  ( -2.710460912692370439, -79.74432941977380551, 10.88462266706781811 ) ) ;
#7816 = AXIS2_PLACEMENT_3D ( 'NONE', #20649, #33636, #41928 ) ;
#7817 = EDGE_CURVE ( 'NONE', #12936, #8817, #35053, .T. ) ;
#7818 = CIRCLE ( 'NONE', #4047, 14.00000000000000000 ) ;
#7819 = CARTESIAN_POINT ( 'NONE',  ( -0.7406579117306999471, -79.37821989574298698, 12.00660533699000077 ) ) ;
#7820 = CARTESIAN_POINT ( 'NONE',  ( -1.250000000000000000, -81.99999999999998579, 0.000000000000000000 ) ) ;
#7821 = CARTESIAN_POINT ( 'NONE',  ( -9.774834661796999669, -79.28204909097999575, 5.593440076811999617 ) ) ;
#7822 = LINE ( 'NONE', #57413, #22367 ) ;
#7823 = CARTESIAN_POINT ( 'NONE',  ( 0.8804656547800843169, -25.02803394706689843, 12.70299681151785265 ) ) ;
#7824 = VERTEX_POINT ( 'NONE', #47815 ) ;
#7825 = ORIENTED_EDGE ( 'NONE', *, *, #50998, .F. ) ;
#7826 = CARTESIAN_POINT ( 'NONE',  ( -2.598917237794094337, -1.447916666666666297, 1.997276839918461722 ) ) ;
#7827 = DIRECTION ( 'NONE',  ( -0.9999999999999994449, -3.428898372811998503E-08, 7.236136581007996102E-12 ) ) ;
#7828 = ADVANCED_FACE ( 'NONE', ( #20921 ), #16213, .F. ) ;
#7829 = CARTESIAN_POINT ( 'NONE',  ( -2.026146017328999793, -80.48624039569099864, -2.908556962501000154 ) ) ;
#7830 = CARTESIAN_POINT ( 'NONE',  ( -5.496009875325862382, -79.32396257907269899, 7.748915864499907435 ) ) ;
#7831 = ORIENTED_EDGE ( 'NONE', *, *, #48162, .F. ) ;
#7832 = CARTESIAN_POINT ( 'NONE',  ( 2.645103879840000172, -78.86345638110998379, 12.07208373076000107 ) ) ;
#7833 = CARTESIAN_POINT ( 'NONE',  ( 7.664266801488738068, -55.05053022673565266, -7.892048199452570856 ) ) ;
#7834 = ORIENTED_EDGE ( 'NONE', *, *, #45921, .T. ) ;
#7835 = CARTESIAN_POINT ( 'NONE',  ( 10.07627163191000008, -18.75000000240999753, -7.601397897754999633 ) ) ;
#7836 = CONICAL_SURFACE ( 'NONE', #6873, 0.6999999997695000031, 0.7853981633972997312 ) ;
#7837 = CARTESIAN_POINT ( 'NONE',  ( -4.946691137268142135, -80.01318923639908576, 9.544298021765493800 ) ) ;
#7838 = CARTESIAN_POINT ( 'NONE',  ( -5.159044788988000008, -77.33039518626078745, -8.219183903844999861 ) ) ;
#7840 = EDGE_CURVE ( 'NONE', #604, #4986, #39890, .T. ) ;
#7839 = CARTESIAN_POINT ( 'NONE',  ( -11.08400893143999966, -76.34452448127198920, -1.489506537590000068 ) ) ;
#7841 = CARTESIAN_POINT ( 'NONE',  ( 8.786918763555123135, -79.00520833333479231, 7.904998819390135267 ) ) ;
#7842 = CARTESIAN_POINT ( 'NONE',  ( -1.439896632895359962, -78.58541666666666003, 10.99999999999999645 ) ) ;
#7843 = AXIS2_PLACEMENT_3D ( 'NONE', #42634, #20200, #11635 ) ;
#7844 = EDGE_CURVE ( 'NONE', #21107, #27560, #3216, .T. ) ;
#7845 = CARTESIAN_POINT ( 'NONE',  ( 5.347250836987999634, -76.22619307850399650, 9.743024754427001000 ) ) ;
#7846 = B_SPLINE_CURVE_WITH_KNOTS ( 'NONE', 3,
 ( #35925, #45397, #53955, #54246, #4048, #31781 ),
 .UNSPECIFIED., .F., .F.,
 ( 4, 2, 4 ),
 ( 0.000000000000000000, 0.5000000000000000000, 1.000000000000000000 ),
 .UNSPECIFIED. ) ;
#7847 = CARTESIAN_POINT ( 'NONE',  ( -5.694495468273999883, -77.08086167140099576, -7.629186780306000060 ) ) ;
#7848 = CARTESIAN_POINT ( 'NONE',  ( -0.4318353353321000010, -80.73831797169299307, -4.107557903773000341 ) ) ;
#7849 = CARTESIAN_POINT ( 'NONE',  ( -10.98916705908266778, -80.10458660312347945, -0.5762717334662600388 ) ) ;
#7850 = CARTESIAN_POINT ( 'NONE',  ( 0.8973824584412640748, -2.954159113890376887, 3.123983622971040486 ) ) ;
#7851 = CARTESIAN_POINT ( 'NONE',  ( -3.024299354891000213, -80.01250264934799361, 1.848939479835000066 ) ) ;
#7852 = CARTESIAN_POINT ( 'NONE',  ( 1.214377479881415978, -82.87154625297898747, 0.3342415832218785243 ) ) ;
#7853 = CARTESIAN_POINT ( 'NONE',  ( 1.358370974174965440, -80.96534657823993086, 10.66387759044030403 ) ) ;
#7854 = CARTESIAN_POINT ( 'NONE',  ( 0.2671888637738000227, -82.79444503318798354, 3.536973918679999773 ) ) ;
#7855 = CARTESIAN_POINT ( 'NONE',  ( 2.234646451474000095, -2.607731223386999808, 3.080979982494000069 ) ) ;
#7856 = CARTESIAN_POINT ( 'NONE',  ( -1.264053276207970367, -80.73968330173562435, 0.1648152915473942437 ) ) ;
#7857 = AXIS2_PLACEMENT_3D ( 'NONE', #56679, #16235, #2666 ) ;
#7858 = CARTESIAN_POINT ( 'NONE',  ( -9.643350356198000739, -61.74034317005999384, -8.260133465614998727 ) ) ;
#7859 = CARTESIAN_POINT ( 'NONE',  ( 0.000000000000000000, -83.49999999999998579, 0.000000000000000000 ) ) ;
#7860 = B_SPLINE_CURVE_WITH_KNOTS ( 'NONE', 3,
 ( #24355, #34347, #25502, #2788, #24641, #29916, #15195, #56809, #6339, #46813, #51812, #55943, #16366, #34058, #43520, #33186, #42367, #20787, #33483, #3081, #37627, #51523, #47684, #6634, #55645, #38211, #51232, #1936, #19928, #11081, #29061, #52096, #47390, #11654, #47103, #6921, #56232, #43231, #42653, #29631, #7210, #15782, #33773, #11368, #42946, #2502, #49106, #16941, #16654, #17814, #7790 ),
 .UNSPECIFIED., .F., .F.,
 ( 4, 2, 2, 2, 2, 2, 2, 2, 2, 1, 2, 2, 2, 2, 2, 2, 2, 2, 2, 2, 2, 2, 1, 2, 1, 2, 4 ),
 ( 0.000000000000000000, 0.03125000000000002776, 0.06250000000000005551, 0.1250000000000000555, 0.1875000000000000833, 0.2500000000000000555, 0.2812500000000000555, 0.3125000000000000555, 0.3437500000000000000, 0.3750000000000000555, 0.4062500000000000555, 0.4375000000000000555, 0.4687500000000000000, 0.5000000000000000000, 0.5312500000000000000, 0.5625000000000000000, 0.6250000000000000000, 0.6874999999999998890, 0.7499999999999998890, 0.7812499999999998890, 0.8124999999999998890, 0.8437500000000000000, 0.8750000000000000000, 0.9062500000000000000, 0.9375000000000000000, 0.9687500000000001110, 1.000000000000000000 ),
 .UNSPECIFIED. ) ;
#7861 = CARTESIAN_POINT ( 'NONE',  ( -1.200131629027000102, -80.70066666181199366, -0.3495483843597000373 ) ) ;
#7862 = CARTESIAN_POINT ( 'NONE',  ( -12.54977952618000003, -16.95167110035999869, 0.03756586072994999581 ) ) ;
#7863 = CARTESIAN_POINT ( 'NONE',  ( 11.82764905900999963, -77.33622945496999534, 5.426413045081000419 ) ) ;
#7864 = CARTESIAN_POINT ( 'NONE',  ( -11.00000000000000000, -79.71041666666664582, -1.439896632895322881 ) ) ;
#7865 = CARTESIAN_POINT ( 'NONE',  ( 0.000000000000000000, -75.00000000000000000, -8.399999999999769429 ) ) ;
#7866 = CARTESIAN_POINT ( 'NONE',  ( -4.147314951225999913, -75.89626379192999650, 11.80504683188000037 ) ) ;
#7867 = ORIENTED_EDGE ( 'NONE', *, *, #35084, .F. ) ;
#7868 = CARTESIAN_POINT ( 'NONE',  ( -9.497876546326999403, -77.35168256874098347, -0.2008509664869000122 ) ) ;
#7869 = CARTESIAN_POINT ( 'NONE',  ( -8.535194087266999574, -80.21887704144299391, 7.565591427388000056 ) ) ;
#7870 = CARTESIAN_POINT ( 'NONE',  ( -0.1119250601223000102, -80.86013818095800332, -1.305888816287000154 ) ) ;
#7871 = DIRECTION ( 'NONE',  ( 1.000000000000000000, 0.000000000000000000, 0.000000000000000000 ) ) ;
#7872 = CARTESIAN_POINT ( 'NONE',  ( 9.480930971721999612, -79.21433849994599541, 0.8843128721991000418 ) ) ;
#7873 = CARTESIAN_POINT ( 'NONE',  ( -3.349809558510000063, -83.06005720286400162, 2.487739645664000410 ) ) ;
#7874 = CARTESIAN_POINT ( 'NONE',  ( 1.796156089042924897, -79.96199394507185332, 10.59866495730046410 ) ) ;
#7875 = CARTESIAN_POINT ( 'NONE',  ( 1.086271320152000008, -79.29714775010999972, -0.9110860045855999623 ) ) ;
#7876 = ORIENTED_EDGE ( 'NONE', *, *, #35176, .F. ) ;
#7877 = CARTESIAN_POINT ( 'NONE',  ( -4.687312336529864787, -79.01734543862330895, 8.066552816164486828 ) ) ;
#7878 = CARTESIAN_POINT ( 'NONE',  ( 0.8524051983356712991, -78.91372865514620116, -3.816371284592112278 ) ) ;
#7879 = SHAPE_REPRESENTATION ( 'Push Button Case', ( #43526 ), #23620 ) ;
#7880 = ORIENTED_EDGE ( 'NONE', *, *, #40054, .T. ) ;
#7881 = CARTESIAN_POINT ( 'NONE',  ( 8.838457456548999502, -78.57066105045699089, -6.447440276951000193 ) ) ;
#7882 = AXIS2_PLACEMENT_3D ( 'NONE', #20372, #25650, #43676 ) ;
#7883 = CARTESIAN_POINT ( 'NONE',  ( 12.80900240956999880, -57.04634220890999785, 1.930989144707000005 ) ) ;
#7884 = CARTESIAN_POINT ( 'NONE',  ( -3.482343428915000150, -80.46974281206399837, -10.30556169736999905 ) ) ;
#7885 = VERTEX_POINT ( 'NONE', #25346 ) ;
#7886 = CARTESIAN_POINT ( 'NONE',  ( -11.93030759001999996, -78.70234896019000814, -1.692197530282999907 ) ) ;
#7887 = ORIENTED_EDGE ( 'NONE', *, *, #35949, .F. ) ;
#7888 = VERTEX_POINT ( 'NONE', #43361 ) ;
#7889 = AXIS2_PLACEMENT_3D ( 'NONE', #30989, #45485, #49028 ) ;
#7890 = DIRECTION ( 'NONE',  ( -0.9957542233430538570, 0.04890176636660768794, -0.07798810127639639600 ) ) ;
#7891 = ADVANCED_FACE ( 'NONE', ( #20352 ), #6912, .T. ) ;
#7892 = CARTESIAN_POINT ( 'NONE',  ( -3.518657424328000438, -86.36264283715298973, 1.566607219238000059 ) ) ;
#7893 = CARTESIAN_POINT ( 'NONE',  ( -1.779454691337655659, -0.7645432949399240119, 3.096242983992194553 ) ) ;
#7894 = ORIENTED_EDGE ( 'NONE', *, *, #8905, .T. ) ;
#7895 = CARTESIAN_POINT ( 'NONE',  ( 11.00000000000000000, -18.25000000000000000, 1.016729233725000008E-14 ) ) ;
#7896 = VERTEX_POINT ( 'NONE', #11215 ) ;
#7897 = CARTESIAN_POINT ( 'NONE',  ( 8.939244305430717574, -79.24132811518457231, -8.111072825249147300 ) ) ;
#7898 = CARTESIAN_POINT ( 'NONE',  ( -0.03344221497652981323, -78.96264282632948550, -3.548192314505119960 ) ) ;
#7899 = CARTESIAN_POINT ( 'NONE',  ( 12.65372179309999900, -57.04935286341999756, -1.750000000000000000 ) ) ;
#7900 = CARTESIAN_POINT ( 'NONE',  ( 7.000000000000000000, -80.99999999999998579, 0.000000000000000000 ) ) ;
#7901 = CARTESIAN_POINT ( 'NONE',  ( 11.74935832213735587, -77.44163738188349555, -0.7696680151942836279 ) ) ;
#7902 = B_SPLINE_CURVE_WITH_KNOTS ( 'NONE', 3,
 ( #46500, #33466, #19908, #51503, #42047, #55624 ),
 .UNSPECIFIED., .F., .F.,
 ( 4, 2, 4 ),
 ( 0.000000000000000000, 0.5000000000000000000, 1.000000000000000000 ),
 .UNSPECIFIED. ) ;
#7903 = CARTESIAN_POINT ( 'NONE',  ( 12.70722176278216686, -61.21036110583639100, -1.610175936231609484 ) ) ;
#7904 = ADVANCED_FACE ( 'NONE', ( #38922 ), #51223, .T. ) ;
#7905 = CARTESIAN_POINT ( 'NONE',  ( 7.483561698776001414, -78.47130766112512390, 9.354804580292000793 ) ) ;
#7906 = DIRECTION ( 'NONE',  ( 0.000000000000000000, 1.000000000000000000, 0.000000000000000000 ) ) ;
#7907 = CARTESIAN_POINT ( 'NONE',  ( 11.88049207238000093, -76.17691755325998315, -3.223263369271999856 ) ) ;
#7908 = CARTESIAN_POINT ( 'NONE',  ( -4.096741325518999943, -78.68975264934786651, -0.8036461072880000112 ) ) ;
#7909 = CARTESIAN_POINT ( 'NONE',  ( 9.230360848053999590, -77.48048667140099610, -3.179709793684999841 ) ) ;
#7910 = CARTESIAN_POINT ( 'NONE',  ( -12.43359548536000148, -17.29290601378000147, 0.8500179128024000219 ) ) ;
#7911 = CARTESIAN_POINT ( 'NONE',  ( 0.000000000000000000, -81.10000000285099020, 7.000000000000000000 ) ) ;
#7912 = DIRECTION ( 'NONE',  ( 0.000000000000000000, 1.000000000000000000, 0.000000000000000000 ) ) ;
#7913 = CARTESIAN_POINT ( 'NONE',  ( 5.155010784763280007, -79.93646688885499429, 9.790528303537310961 ) ) ;
#7914 = CARTESIAN_POINT ( 'NONE',  ( 11.75000000000000000, -76.45000000000000284, 0.000000000000000000 ) ) ;
#7915 = CARTESIAN_POINT ( 'NONE',  ( -1.980584515752000119, -23.26485146623999967, 12.76303204602000108 ) ) ;
#7916 = B_SPLINE_SURFACE_WITH_KNOTS ( 'NONE', 3, 3, ( 
 ( #9809, #15098, #1259, #6240, #32506, #27794, #15399, #5373, #33392, #42561, #42272, #23666, #51430, #54679, #37828, #10103, #41972, #45838, #55254, #19833, #33095, #10985, #23381, #14803, #32796, #36661, #41391, #10390, #28376, #974, #55848, #46421, #5950, #1840, #51139 ),
 ( #23953, #18958, #36952, #19536, #37530, #29538, #2703, #20128, #47594, #16559, #7121, #20698, #47876, #48439, #48161, #6826, #7693, #30112, #43424, #30404, #38697, #16848, #24837, #11272, #38116, #25694, #2412, #39274, #7981, #52859, #7405, #25121, #43144, #43722, #2984 ),
 ( #20983, #38986, #52575, #56997, #11846, #34542, #56139, #52287, #56718, #3275, #57284, #12125, #21268, #34829, #12413, #42852, #15686, #25979, #29825, #2127, #33683, #51720, #25409, #11561, #33969, #29251, #47300, #20412, #38407, #56427, #34254, #15979, #16275, #52007, #35401 ),
 ( #35113, #30972, #53432, #26847, #48726, #13865, #17129, #31860, #22131, #57859, #4132, #44284, #9448, #54325, #44878, #22430, #8269, #12695, #35706, #49010, #12975, #44577, #3555, #8557, #35, #40141, #40444, #53146, #18012, #49901, #3841, #45178, #36004, #21557, #54029 ) ),
 .UNSPECIFIED., .F., .F., .F.,
 ( 4, 4 ),
 ( 4, 1, 1, 1, 1, 1, 1, 1, 1, 1, 1, 1, 1, 1, 1, 1, 1, 1, 1, 1, 1, 1, 1, 1, 1, 1, 1, 1, 1, 1, 1, 1, 4 ),
 ( -0.05371687727927999811, 1.053716877278999986 ),
 ( -0.02000000000000000042, 0.01250000000000000069, 0.04499999999999999833, 0.07749999999999999944, 0.1100000000000000006, 0.1424999999999999878, 0.1749999999999999889, 0.2074999999999999900, 0.2399999999999999911, 0.2725000000000000200, 0.3049999999999999933, 0.3375000000000000222, 0.3699999999999999956, 0.4025000000000000244, 0.4349999999999999978, 0.4675000000000000266, 0.5000000000000000000, 0.5324999999999999734, 0.5649999999999999467, 0.5975000000000000311, 0.6300000000000000044, 0.6624999999999999778, 0.6949999999999999512, 0.7275000000000000355, 0.7600000000000000089, 0.7924999999999999822, 0.8249999999999999556, 0.8575000000000000400, 0.8900000000000000133, 0.9224999999999999867, 0.9549999999999999600, 0.9875000000000000444, 1.020000000000000018 ),
 .UNSPECIFIED. ) ;
#7917 = CARTESIAN_POINT ( 'NONE',  ( 1.151817246788077176, -80.55763602254313582, 1.030585181417483565 ) ) ;
#7918 = CARTESIAN_POINT ( 'NONE',  ( -3.524583092881000024, -77.36221662263500320, 8.811773852426000531 ) ) ;
#7919 = DIRECTION ( 'NONE',  ( 0.000000000000000000, 0.000000000000000000, 1.000000000000000000 ) ) ;
#7920 = DIRECTION ( 'NONE',  ( 1.000000000000000000, 0.000000000000000000, 0.000000000000000000 ) ) ;
#7921 = ADVANCED_FACE ( 'NONE', ( #43656 ), #7836, .F. ) ;
#7922 = CARTESIAN_POINT ( 'NONE',  ( 0.5109974968053999644, -3.332071030359000208, 3.520844556087999955 ) ) ;
#7923 = CARTESIAN_POINT ( 'NONE',  ( 12.25187917533000004, -78.62878573459099130, 0.8290103756198000662 ) ) ;
#7924 = DIRECTION ( 'NONE',  ( -1.000000000000000000, 0.000000000000000000, 0.000000000000000000 ) ) ;
#7926 = CARTESIAN_POINT ( 'NONE',  ( -1.295285823243000012, -78.25715048044240518, -0.2505997727336000125 ) ) ;
#7925 = CARTESIAN_POINT ( 'NONE',  ( -6.183644282731068920, -75.80000000000002558, 10.16304460950663113 ) ) ;
#7927 = CARTESIAN_POINT ( 'NONE',  ( 0.5770204343780001022, -82.36129654213999629, -1.476971271490000071 ) ) ;
#7928 = CARTESIAN_POINT ( 'NONE',  ( -4.762553456520412176, -79.51167294223473903, 9.637703495840463930 ) ) ;
#7929 = ORIENTED_EDGE ( 'NONE', *, *, #19590, .F. ) ;
#7930 = CARTESIAN_POINT ( 'NONE',  ( -10.59551070212000035, -21.75648180056000314, -7.678690995204998870 ) ) ;
#7931 = CARTESIAN_POINT ( 'NONE',  ( 4.684330217986999223, -79.78092145310699834, -10.80673261319000034 ) ) ;
#7932 = CARTESIAN_POINT ( 'NONE',  ( 6.206556651784778111, -79.06848936835629615, 7.218217299451517022 ) ) ;
#7933 = CARTESIAN_POINT ( 'NONE',  ( 7.815903581356871577, -79.71875000000000000, 9.154229383352316063 ) ) ;
#7934 = CARTESIAN_POINT ( 'NONE',  ( 2.879226727952049814, -78.95416666666666572, 10.71369944335148183 ) ) ;
#7935 = CARTESIAN_POINT ( 'NONE',  ( -3.850958688833999943, -1.225056440563999871, -0.3160333990881999955 ) ) ;
#7936 = CARTESIAN_POINT ( 'NONE',  ( 5.771514257604000164, -79.59623425335998093, 8.032758792294998784 ) ) ;
#7937 = CARTESIAN_POINT ( 'NONE',  ( 12.77568181202000019, -25.26511628633999962, -0.5294980821347999855 ) ) ;
#7938 = FACE_OUTER_BOUND ( 'NONE', #37656, .T. ) ;
#7939 = ORIENTED_EDGE ( 'NONE', *, *, #15168, .T. ) ;
#7940 = ADVANCED_FACE ( 'NONE', ( #12068 ), #38349, .T. ) ;
#7941 = DIRECTION ( 'NONE',  ( 0.000000000000000000, 1.000000000000000000, 0.000000000000000000 ) ) ;
#7942 = CARTESIAN_POINT ( 'NONE',  ( -6.862551019151999832, -79.75786001420199511, 6.914489430668000480 ) ) ;
#7943 = DIRECTION ( 'NONE',  ( -1.000000000000000000, 0.000000000000000000, 0.000000000000000000 ) ) ;
#7944 = CARTESIAN_POINT ( 'NONE',  ( -10.59548767699999949, -57.04263462147999775, -7.678667886061999681 ) ) ;
#7945 = CARTESIAN_POINT ( 'NONE',  ( -0.7048934085577001074, -80.91984118541999749, -1.509431780672999990 ) ) ;
#7946 = AXIS2_PLACEMENT_3D ( 'NONE', #48584, #26130, #8411 ) ;
#7947 = EDGE_LOOP ( 'NONE', ( #6301, #19384, #42979, #47826 ) ) ;
#7948 = CARTESIAN_POINT ( 'NONE',  ( 0.5713819827555001174, -77.30008885281499431, 11.08689227811000144 ) ) ;
#7949 = CARTESIAN_POINT ( 'NONE',  ( 5.208980231641255010, -77.85915179526145380, -10.56064782346102682 ) ) ;
#7950 = CARTESIAN_POINT ( 'NONE',  ( -1.997276839918471714, -1.072916666666666963, -2.598917237794086788 ) ) ;
#7951 = CARTESIAN_POINT ( 'NONE',  ( -12.49168451100999988, -60.09848884406000025, 1.667916687331000070 ) ) ;
#7952 = CARTESIAN_POINT ( 'NONE',  ( -9.422860735104000796, -53.54048607621999878, -8.643926020445999114 ) ) ;
#7953 = EDGE_CURVE ( 'NONE', #49594, #49808, #28561, .T. ) ;
#7954 = AXIS2_PLACEMENT_3D ( 'NONE', #9859, #37289, #735 ) ;
#7955 = SURFACE_SIDE_STYLE ('',( #53123 ) ) ;
#7956 = FACE_OUTER_BOUND ( 'NONE', #4926, .T. ) ;
#7957 = ORIENTED_EDGE ( 'NONE', *, *, #47949, .F. ) ;
#7958 = ORIENTED_EDGE ( 'NONE', *, *, #44295, .T. ) ;
#7959 = CARTESIAN_POINT ( 'NONE',  ( 10.42437852075000038, -76.52923235641000588, -7.057286423715000367 ) ) ;
#7960 = DIRECTION ( 'NONE',  ( 1.000000000000000000, 0.000000000000000000, 0.000000000000000000 ) ) ;
#7961 = EDGE_CURVE ( 'NONE', #28651, #49809, #33906, .T. ) ;
#7962 = CARTESIAN_POINT ( 'NONE',  ( -0.8698315184489000540, -77.71593921376999958, -1.124239518549000172 ) ) ;
#7963 = ORIENTED_EDGE ( 'NONE', *, *, #34007, .T. ) ;
#7964 = CARTESIAN_POINT ( 'NONE',  ( 8.979348251287998295, -77.96650584965399844, 3.086914251890999772 ) ) ;
#7965 = CYLINDRICAL_SURFACE ( 'NONE', #31966, 12.50000000000000000 ) ;
#7966 = CARTESIAN_POINT ( 'NONE',  ( -0.5999999999999999778, -23.15000000000999947, 11.79999999999999893 ) ) ;
#7967 = CARTESIAN_POINT ( 'NONE',  ( -3.078285613438000112, -78.56286269907000985, 12.42192206172999924 ) ) ;
#7968 = PRODUCT_DEFINITION_CONTEXT ( 'detailed design', #28888, 'design' ) ;
#7969 = CARTESIAN_POINT ( 'NONE',  ( -5.751434148371999733, -77.83215719852289283, -9.630115047516998317 ) ) ;
#7970 = CARTESIAN_POINT ( 'NONE',  ( -12.51072239526000196, -26.30294702885999669, -0.7871079366006996647 ) ) ;
#7971 = CARTESIAN_POINT ( 'NONE',  ( -0.5413909687619357092, -86.39318692756700102, 4.353993567106698492 ) ) ;
#7972 = CARTESIAN_POINT ( 'NONE',  ( 10.54265532893000135, -78.67941394246899733, 3.830212845596999927 ) ) ;
#7973 = CARTESIAN_POINT ( 'NONE',  ( 1.425295968735332597, -79.96318692083401913, 9.139224115734268850 ) ) ;
#7974 = ADVANCED_FACE ( 'NONE', ( #51370 ), #28907, .T. ) ;
#7975 = CARTESIAN_POINT ( 'NONE',  ( -0.6747260877994001316, -82.25000000000000000, -1.052256958371999840 ) ) ;
#7976 = ORIENTED_EDGE ( 'NONE', *, *, #13476, .F. ) ;
#7977 = CARTESIAN_POINT ( 'NONE',  ( 5.445998289199994957, -77.27523227367147740, -7.476759099558663912 ) ) ;
#7978 = CARTESIAN_POINT ( 'NONE',  ( -1.191059436918999959, -79.34293819223900357, -0.7689280169367000983 ) ) ;
#7979 = DIRECTION ( 'NONE',  ( 0.000000000000000000, -1.000000000000000000, 0.000000000000000000 ) ) ;
#7980 = CARTESIAN_POINT ( 'NONE',  ( 7.189039685305540495, -77.07583944371667428, -9.673072753243905808 ) ) ;
#7981 = CARTESIAN_POINT ( 'NONE',  ( 1.118108678836999825, -78.85632414226799369, 1.024097206608999944 ) ) ;
#7982 = DIRECTION ( 'NONE',  ( 0.9999476293090542312, 0.000000000000000000, 0.01023418971888952027 ) ) ;
#7983 = CARTESIAN_POINT ( 'NONE',  ( 12.83044027760000105, -23.30639784948999704, 2.062670899361999766 ) ) ;
#7984 = DIRECTION ( 'NONE',  ( 2.719057617950000092E-13, 0.000000000000000000, -1.000000000000000000 ) ) ;
#7985 = CARTESIAN_POINT ( 'NONE',  ( -9.875985572548097835, -80.44999999999996021, -4.392572548244121577 ) ) ;
#7986 = CARTESIAN_POINT ( 'NONE',  ( -11.08844420678000020, -79.06580120733299566, -1.240163186867999867 ) ) ;
#7987 = DIRECTION ( 'NONE',  ( -0.9999873237594404385, 0.000000000000000000, -0.005035108780571202237 ) ) ;
#7988 = CARTESIAN_POINT ( 'NONE',  ( -0.8854615841765430817, -83.03831763565791846, 0.8817396644130072181 ) ) ;
#7989 = CARTESIAN_POINT ( 'NONE',  ( 3.979198690588999998, -82.45517979992798985, 0.4013901926927000430 ) ) ;
#7990 = CIRCLE ( 'NONE', #42906, 0.8000000000000011546 ) ;
#7991 = CARTESIAN_POINT ( 'NONE',  ( -5.413904038987206846, -77.91666666666665719, 9.393203674808249914 ) ) ;
#7992 = ORIENTED_EDGE ( 'NONE', *, *, #44758, .F. ) ;
#7993 = CARTESIAN_POINT ( 'NONE',  ( -7.154810283782063962, -77.19999999999998863, 8.208487408017942855 ) ) ;
#7994 = VECTOR ( 'NONE', #31577, 1000.000000000000114 ) ;
#7995 = CARTESIAN_POINT ( 'NONE',  ( -1.274573384913999963, -80.41529921676999493, 0.7293221697183999153 ) ) ;
#7996 = FACE_OUTER_BOUND ( 'NONE', #8393, .T. ) ;
#7997 = CARTESIAN_POINT ( 'NONE',  ( 0.3864029911681999829, -77.19372312914599377, -11.74364478040999948 ) ) ;
#7998 = CARTESIAN_POINT ( 'NONE',  ( -12.70259395227543209, -17.26112126506535915, 1.314575638808931579 ) ) ;
#7999 = B_SPLINE_CURVE_WITH_KNOTS ( 'NONE', 3,
 ( #8268, #44005, #49827, #30687, #48725, #27363 ),
 .UNSPECIFIED., .F., .F.,
 ( 4, 1, 1, 4 ),
 ( 0.000000000000000000, 0.3333333333333000081, 0.6666666666667000474, 1.000000000000000000 ),
 .UNSPECIFIED. ) ;
#8000 = CARTESIAN_POINT ( 'NONE',  ( 1.579899301681999990, -81.98685842128999468, 0.5283722218587000308 ) ) ;
#8001 = CARTESIAN_POINT ( 'NONE',  ( 3.290942002251577403, -1.971106319304349208, -1.249796515420581455 ) ) ;
#8002 = CARTESIAN_POINT ( 'NONE',  ( -9.601739433208001273, -79.08254805011499400, -1.533141744029000053 ) ) ;
#8003 = CARTESIAN_POINT ( 'NONE',  ( -1.798954018885000172, -55.58469026579999905, -12.61117007300000026 ) ) ;
#8004 = CARTESIAN_POINT ( 'NONE',  ( 9.770175552643170391, -75.99682500216157166, 6.527251886581928453 ) ) ;
#8005 = CARTESIAN_POINT ( 'NONE',  ( -0.5518643889788126256, -85.83735716284300565, 4.438223277016693835 ) ) ;
#8006 = ORIENTED_EDGE ( 'NONE', *, *, #27932, .T. ) ;
#8007 = DIRECTION ( 'NONE',  ( 0.000000000000000000, 1.000000000000000000, 0.000000000000000000 ) ) ;
#8008 = CARTESIAN_POINT ( 'NONE',  ( -11.74590880730695908, -77.18882810128452832, 1.536480942173005682 ) ) ;
#8009 = CIRCLE ( 'NONE', #7087, 13.86363636363999952 ) ;
#8010 = CARTESIAN_POINT ( 'NONE',  ( -8.335659130299518438, -78.76230910829006859, -8.330744675050686610 ) ) ;
#8011 = DIRECTION ( 'NONE',  ( 0.000000000000000000, 0.000000000000000000, -1.000000000000000000 ) ) ;
#8012 = CARTESIAN_POINT ( 'NONE',  ( 0.1291013223160000223, -79.30421540610097964, 10.97485077029999978 ) ) ;
#8013 = CARTESIAN_POINT ( 'NONE',  ( 0.1380878922962947286, -16.77265597675712172, 12.70555840932531488 ) ) ;
#8014 = CARTESIAN_POINT ( 'NONE',  ( -9.811892674444001372, -75.99338179775399738, -7.560764302057000563 ) ) ;
#8015 = DIRECTION ( 'NONE',  ( -1.000000000000000000, 0.000000000000000000, 0.000000000000000000 ) ) ;
#8016 = CARTESIAN_POINT ( 'NONE',  ( -7.764217752296561414, -61.05600304933474121, 10.21028588418797867 ) ) ;
#8017 = VERTEX_POINT ( 'NONE', #25062 ) ;
#8018 = EDGE_CURVE ( 'NONE', #54902, #11044, #44575, .T. ) ;
#8019 = CARTESIAN_POINT ( 'NONE',  ( -0.2253802134100999777, -78.26452830333799682, -10.88640714497000062 ) ) ;
#8020 = CARTESIAN_POINT ( 'NONE',  ( 0.2548808781567560300, -79.95924185380276583, 1.223919185308683266 ) ) ;
#8021 = DIRECTION ( 'NONE',  ( -1.000000000000000000, 0.000000000000000000, 0.000000000000000000 ) ) ;
#8022 = B_SPLINE_CURVE_WITH_KNOTS ( 'NONE', 3,
 ( #8465, #9648, #18509, #9065, #36215, #36792, #36503, #53639, #54528, #14066, #31770, #18800, #27050, #5218, #13180, #58064, #26461, #32063 ),
 .UNSPECIFIED., .F., .F.,
 ( 4, 2, 2, 2, 2, 2, 2, 2, 4 ),
 ( 0.000000000000000000, 0.1249999999999999722, 0.2499999999999999445, 0.3749999999999998890, 0.4999999999999998890, 0.6249999999999998890, 0.7499999999999997780, 0.8749999999999998890, 1.000000000000000000 ),
 .UNSPECIFIED. ) ;
#8023 = CARTESIAN_POINT ( 'NONE',  ( 10.34967326289000056, -78.08539999468298731, 3.868085496227999798 ) ) ;
#8024 = CARTESIAN_POINT ( 'NONE',  ( -10.69999999999999929, -80.49999999999998579, 0.000000000000000000 ) ) ;
#8025 = PLANE ( 'NONE',  #47314 ) ;
#8026 = CARTESIAN_POINT ( 'NONE',  ( 0.4639995417680284895, -81.69951572676090734, 1.438848120810740872 ) ) ;
#8027 = CARTESIAN_POINT ( 'NONE',  ( -11.33781659400000130, -78.29521678053998812, 4.716958136547999558 ) ) ;
#8028 = DIRECTION ( 'NONE',  ( 1.000000000000000000, 0.000000000000000000, 0.000000000000000000 ) ) ;
#8029 = CARTESIAN_POINT ( 'NONE',  ( -12.70556836333273409, -62.02772277294080538, -0.2642470009393159125 ) ) ;
#8030 = AXIS2_PLACEMENT_3D ( 'NONE', #11092, #47118, #14907 ) ;
#8031 = CARTESIAN_POINT ( 'NONE',  ( -5.917523019358107206, -76.21666666666666856, 10.26699006316250795 ) ) ;
#8032 = ORIENTED_EDGE ( 'NONE', *, *, #47268, .T. ) ;
#8033 = ORIENTED_EDGE ( 'NONE', *, *, #31603, .T. ) ;
#8034 = CARTESIAN_POINT ( 'NONE',  ( -12.77297374709000088, -54.07184670079000455, -1.476174539902000094 ) ) ;
#8035 = ADVANCED_FACE ( 'NONE', ( #51668 ), #9635, .F. ) ;
#8036 = CONICAL_SURFACE ( 'NONE', #15596, 12.14999999923000118, 0.7853981633972997312 ) ;
#8037 = ORIENTED_EDGE ( 'NONE', *, *, #13088, .T. ) ;
#8038 = CARTESIAN_POINT ( 'NONE',  ( -3.911342194028000208, -78.65116864382999040, -11.62327352135999980 ) ) ;
#8039 = ORIENTED_EDGE ( 'NONE', *, *, #6580, .T. ) ;
#8040 = CARTESIAN_POINT ( 'NONE',  ( -7.134970007453478757, -81.00000000000001421, -8.203445754864530315 ) ) ;
#8041 = CARTESIAN_POINT ( 'NONE',  ( 5.122310662682999727, -77.73727524673999767, -9.640399341584998893 ) ) ;
#8042 = CONTEXT_DEPENDENT_SHAPE_REPRESENTATION ( #10818, #50333 ) ;
#8043 = CARTESIAN_POINT ( 'NONE',  ( 2.202483111904999902, -79.27258998579800675, -9.433251486511000650 ) ) ;
#8044 = CARTESIAN_POINT ( 'NONE',  ( -6.534469237059214564, -78.16274746009533203, -6.546848636492562434 ) ) ;
#8045 =( REPRESENTATION_RELATIONSHIP ('NONE','NONE', #58051, #13452 ) REPRESENTATION_RELATIONSHIP_WITH_TRANSFORMATION ( #43489 )SHAPE_REPRESENTATION_RELATIONSHIP( ) );
#8046 = CARTESIAN_POINT ( 'NONE',  ( -9.735611069857000643, -79.15695685768498890, 5.570995215215999607 ) ) ;
#8047 = EDGE_CURVE ( 'NONE', #28865, #32105, #31493, .T. ) ;
#8048 = ORIENTED_EDGE ( 'NONE', *, *, #17294, .T. ) ;
#8049 = VERTEX_POINT ( 'NONE', #31196 ) ;
#8050 = CARTESIAN_POINT ( 'NONE',  ( -7.383570525523341921, -77.54854952769156284, 5.573145937136878558 ) ) ;
#8051 = CARTESIAN_POINT ( 'NONE',  ( 2.386167682861000117, -77.22751216649398032, 10.77916482977000001 ) ) ;
#8052 = ADVANCED_FACE ( 'NONE', ( #4359 ), #17945, .F. ) ;
#8053 = CARTESIAN_POINT ( 'NONE',  ( -8.300970689365447797, -77.44166666666666288, -4.784380313523547201 ) ) ;
#8054 = CARTESIAN_POINT ( 'NONE',  ( -1.959694873104000257, -77.37866707723799209, -9.504225410855001499 ) ) ;
#8055 = CARTESIAN_POINT ( 'NONE',  ( 7.640030139755999983, -23.30716934606000024, 10.18491068059999805 ) ) ;
#8056 = CARTESIAN_POINT ( 'NONE',  ( -4.947170628245625146, -79.48109446742806483, -8.109985010457963384 ) ) ;
#8057 = CARTESIAN_POINT ( 'NONE',  ( -1.578837173282999995, -79.19167545639999162, 0.3948290484592000271 ) ) ;
#8058 = CARTESIAN_POINT ( 'NONE',  ( 1.791008777272000030, -80.17182820879699534, 11.11143388882000060 ) ) ;
#8059 = DIRECTION ( 'NONE',  ( -0.7071067811865475727, 0.000000000000000000, 0.7071067811865475727 ) ) ;
#8060 = CARTESIAN_POINT ( 'NONE',  ( -1.217465845835394411, -78.02083333333332860, -0.3271848554491003647 ) ) ;
#8061 = CARTESIAN_POINT ( 'NONE',  ( 7.396918292183175758, -78.69791666666665719, -5.684557159767951617 ) ) ;
#8062 = ORIENTED_EDGE ( 'NONE', *, *, #14950, .T. ) ;
#8063 = CARTESIAN_POINT ( 'NONE',  ( 11.54819794350999906, -79.30280790634400034, -3.557883190958000430 ) ) ;
#8064 = CARTESIAN_POINT ( 'NONE',  ( -12.50000000000000000, -60.24678171298000251, -1.250000000000000000 ) ) ;
#8065 = CARTESIAN_POINT ( 'NONE',  ( 3.249499231398999655, -78.84854189942899438, -11.53069031867000049 ) ) ;
#8066 = CARTESIAN_POINT ( 'NONE',  ( -9.966229686710001090, -18.33098097385000003, -7.657726530248999630 ) ) ;
#8068 = CARTESIAN_POINT ( 'NONE',  ( -1.814305421036000121, -17.71058030669000161, -12.78003582253000125 ) ) ;
#8067 = CARTESIAN_POINT ( 'NONE',  ( -8.082088197687879116, -78.55834743794827091, 4.658190788286820982 ) ) ;
#8069 = EDGE_CURVE ( 'NONE', #11901, #48636, #19407, .T. ) ;
#8070 = DIRECTION ( 'NONE',  ( -1.893719483827980309E-11, 1.538483568841980365E-07, 0.9999999999999882316 ) ) ;
#8071 = CARTESIAN_POINT ( 'NONE',  ( 10.18589226633000067, -60.08917723397000543, -7.641012305240000302 ) ) ;
#8072 = CARTESIAN_POINT ( 'NONE',  ( 3.113304451009999863, -78.49783470746899638, -10.55022916317000181 ) ) ;
#8073 = CARTESIAN_POINT ( 'NONE',  ( 7.228832758458999308, -77.14294861368399836, 8.635852100895000660 ) ) ;
#8074 = CARTESIAN_POINT ( 'NONE',  ( 0.000000000000000000, -28.92928575306000383, 0.000000000000000000 ) ) ;
#8075 = CARTESIAN_POINT ( 'NONE',  ( 6.760013919724038978, -80.02291666667453285, 8.796335266380001627 ) ) ;
#8076 = VERTEX_POINT ( 'NONE', #50419 ) ;
#8077 = CARTESIAN_POINT ( 'NONE',  ( 11.90000000000000036, -21.00000000000000000, 0.6999999999999999556 ) ) ;
#8078 = CARTESIAN_POINT ( 'NONE',  ( 1.798368564629000188, -55.60363242921000193, 12.61278090839000043 ) ) ;
#8079 = AXIS2_PLACEMENT_3D ( 'NONE', #55797, #33913, #28912 ) ;
#8080 = CARTESIAN_POINT ( 'NONE',  ( -12.58338334669999981, -21.74800977511999989, 1.667961445601999992 ) ) ;
#8081 = CARTESIAN_POINT ( 'NONE',  ( -2.870258726797999760, -3.078587262672000335, 2.247988175434000091 ) ) ;
#8082 = CARTESIAN_POINT ( 'NONE',  ( 2.977199900158871149, -78.09769602762067109, -10.42248997560320056 ) ) ;
#8083 = CARTESIAN_POINT ( 'NONE',  ( -5.018480251613000043, -80.10112881071398760, -7.977531891197001457 ) ) ;
#8084 = CARTESIAN_POINT ( 'NONE',  ( -12.48408657656000109, -55.43026141536999774, 1.669508654504999967 ) ) ;
#8085 = CARTESIAN_POINT ( 'NONE',  ( -1.249999992656000147, -76.50000000027618796, 0.4999999997238000482 ) ) ;
#8086 = CARTESIAN_POINT ( 'NONE',  ( -3.248580004278440292, -2.091064288162170381, 0.4260749490998382294 ) ) ;
#8087 = CARTESIAN_POINT ( 'NONE',  ( 0.8506806241676642122, -3.145833333333332593, -3.165411199172024848 ) ) ;
#8088 = AXIS2_PLACEMENT_3D ( 'NONE', #55352, #14312, #45342 ) ;
#8089 = EDGE_CURVE ( 'NONE', #35853, #313, #16069, .T. ) ;
#8090 = CARTESIAN_POINT ( 'NONE',  ( -1.753806336804000221, -85.02799735065198661, -3.788636048325999983 ) ) ;
#8091 = CARTESIAN_POINT ( 'NONE',  ( 1.750000000001000089, -55.55000001292999912, 12.56594318049000059 ) ) ;
#8092 = EDGE_CURVE ( 'NONE', #21405, #38037, #48382, .T. ) ;
#8093 = CARTESIAN_POINT ( 'NONE',  ( 9.499178638196321245, -79.00092112126561972, 0.1004274591880019996 ) ) ;
#8094 = CARTESIAN_POINT ( 'NONE',  ( 10.74237452437923501, -76.41648142056769188, -4.760415518113283007 ) ) ;
#8095 = CARTESIAN_POINT ( 'NONE',  ( 3.988644160859999399, -78.36298354959900792, -10.40888963995999994 ) ) ;
#8096 = CARTESIAN_POINT ( 'NONE',  ( 1.129777590424469569, -81.88536348647744489, 0.5350541287706942484 ) ) ;
#8097 = DIRECTION ( 'NONE',  ( 0.000000000000000000, -1.000000000000000000, 0.000000000000000000 ) ) ;
#8098 = CARTESIAN_POINT ( 'NONE',  ( -3.591972190522999764, -77.17512728940789657, 8.980252640667000463 ) ) ;
#8099 = CARTESIAN_POINT ( 'NONE',  ( -0.7554284705563544255, -78.91666666666668561, 1.310679582531384169 ) ) ;
#8100 = CARTESIAN_POINT ( 'NONE',  ( 0.2548462785871886682, -3.469750342128967269, 3.250954444181449965 ) ) ;
#8101 = CARTESIAN_POINT ( 'NONE',  ( 0.02474134673687657798, -80.22542497378589132, -10.74983343428174187 ) ) ;
#8102 = CARTESIAN_POINT ( 'NONE',  ( -12.50000000000000000, -39.49523982883999906, 0.000000000000000000 ) ) ;
#8103 = CARTESIAN_POINT ( 'NONE',  ( -8.274781782264163610, -17.02110650125764479, -9.689260013727274412 ) ) ;
#8104 = ORIENTED_EDGE ( 'NONE', *, *, #14095, .T. ) ;
#8105 = CARTESIAN_POINT ( 'NONE',  ( 6.536979956083999177, -79.23682303308700625, -10.09826910480999906 ) ) ;
#8106 = CARTESIAN_POINT ( 'NONE',  ( -7.596835002782738933, -78.74791666666668277, 5.838193839761661508 ) ) ;
#8107 = DIRECTION ( 'NONE',  ( -1.000000000000000000, 0.000000000000000000, 0.000000000000000000 ) ) ;
#8108 = CARTESIAN_POINT ( 'NONE',  ( -1.407186781496920336, -77.48544845159872807, 10.68067397006091745 ) ) ;
#8109 = ORIENTED_EDGE ( 'NONE', *, *, #49807, .T. ) ;
#8110 = DIRECTION ( 'NONE',  ( 0.000000000000000000, 0.000000000000000000, 1.000000000000000000 ) ) ;
#8111 = ORIENTED_EDGE ( 'NONE', *, *, #27080, .F. ) ;
#8112 = CARTESIAN_POINT ( 'NONE',  ( 0.000000000000000000, -39.30476017083000073, 0.000000000000000000 ) ) ;
#8113 = ORIENTED_EDGE ( 'NONE', *, *, #890, .T. ) ;
#8114 = DIRECTION ( 'NONE',  ( -0.7071067811865475727, 0.000000000000000000, 0.7071067811865475727 ) ) ;
#8115 = CARTESIAN_POINT ( 'NONE',  ( 1.500000000000000000, -78.26041666666669983, 0.1963495408493652339 ) ) ;
#8116 = CARTESIAN_POINT ( 'NONE',  ( -4.041492642110999789, -79.16823080598898343, -10.14108984350000142 ) ) ;
#8117 = CARTESIAN_POINT ( 'NONE',  ( 1.394325645166000216, -80.85856839617498792, -3.307506794681999818 ) ) ;
#8118 = CARTESIAN_POINT ( 'NONE',  ( -3.689560173563782630, -79.30639694791827310, 8.754108420648137212 ) ) ;
#8119 = ORIENTED_EDGE ( 'NONE', *, *, #49214, .T. ) ;
#8120 = CARTESIAN_POINT ( 'NONE',  ( -6.065106684382000068, -77.27128372030617243, 9.224892016835999797 ) ) ;
#8121 = CARTESIAN_POINT ( 'NONE',  ( -5.924797529000001006, -78.83385696754000094, 10.67634899623000067 ) ) ;
#8122 = ORIENTED_EDGE ( 'NONE', *, *, #28150, .F. ) ;
#8123 = EDGE_LOOP ( 'NONE', ( #39523, #1832, #37365, #46970, #42879 ) ) ;
#8124 = CARTESIAN_POINT ( 'NONE',  ( 12.76303204513999923, -55.53514852210999919, -1.980584515753000208 ) ) ;
#8125 = LINE ( 'NONE', #40294, #28207 ) ;
#8126 = DIRECTION ( 'NONE',  ( 0.7071067811865975328, -0.7071067811864976127, -1.396793747092993108E-09 ) ) ;
#8127 = AXIS2_PLACEMENT_3D ( 'NONE', #3785, #21786, #57803 ) ;
#8128 = CARTESIAN_POINT ( 'NONE',  ( -8.588659815671681130, -80.04882308261660739, 6.465083054473538482 ) ) ;
#8129 = CARTESIAN_POINT ( 'NONE',  ( -1.004305231718999991, -1.000000000000000000, 3.090933677959000203 ) ) ;
#8130 = CARTESIAN_POINT ( 'NONE',  ( 0.4312503660543859918, -86.36264282632897960, -4.097589455045484108 ) ) ;
#8131 = CARTESIAN_POINT ( 'NONE',  ( 2.968901491624184263, -85.84407030804550232, 1.939968274069872045 ) ) ;
#8132 = AXIS2_PLACEMENT_3D ( 'NONE', #18351, #13906, #8900 ) ;
#8133 = CARTESIAN_POINT ( 'NONE',  ( -1.235365865572026101, -79.05208333334985582, 11.80208333293604461 ) ) ;
#8134 = CARTESIAN_POINT ( 'NONE',  ( -9.073214995490001655, -77.80567315384000437, -8.802385182600000135 ) ) ;
#8135 = CARTESIAN_POINT ( 'NONE',  ( -4.873207417809000574, -76.93853187307900043, 9.732535352345999868 ) ) ;
#8136 = VECTOR ( 'NONE', #26641, 1000.000000000000114 ) ;
#8137 = CARTESIAN_POINT ( 'NONE',  ( -9.109849427410853906, -78.61403873330360170, -1.603955441074990995 ) ) ;
#8138 = CARTESIAN_POINT ( 'NONE',  ( 2.747588261965000278, -81.33957009409999728, 3.083710821981000105 ) ) ;
#8139 = CARTESIAN_POINT ( 'NONE',  ( -10.42274798266000069, -57.04634220890999785, 7.691916945423999508 ) ) ;
#8140 = CARTESIAN_POINT ( 'NONE',  ( -1.250993231609307310, -3.007667436560337304, 2.998783452090319823 ) ) ;
#8141 = CARTESIAN_POINT ( 'NONE',  ( 1.666332141969999903, -79.72080496681199691, 3.131277625125000075 ) ) ;
#8142 = EDGE_CURVE ( 'NONE', #14039, #54879, #2687, .T. ) ;
#8143 = FACE_OUTER_BOUND ( 'NONE', #48287, .T. ) ;
#8144 = CARTESIAN_POINT ( 'NONE',  ( -1.059394002417758163, -80.98296073876636569, 10.69789347654190337 ) ) ;
#8145 = CARTESIAN_POINT ( 'NONE',  ( -3.318400460481999659, -86.11509620537599119, 0.9372051681108999333 ) ) ;
#8146 = CARTESIAN_POINT ( 'NONE',  ( -2.809159726167000048, -3.376266856787000226, -2.568020482856000264 ) ) ;
#8147 = CARTESIAN_POINT ( 'NONE',  ( 0.4802634405885786162, -80.40574918970366980, -1.180242626984035370 ) ) ;
#8148 = EDGE_LOOP ( 'NONE', ( #9860, #36928, #2033, #31364 ) ) ;
#8149 = CARTESIAN_POINT ( 'NONE',  ( -7.657745562929999750, -60.46920625093000012, -9.966193613345000202 ) ) ;
#8150 = EDGE_CURVE ( 'NONE', #46551, #52925, #52142, .T. ) ;
#8151 = CARTESIAN_POINT ( 'NONE',  ( 11.00000000000000000, -79.44999999999998863, 0.000000000000000000 ) ) ;
#8152 = CARTESIAN_POINT ( 'NONE',  ( -1.310615285706999922, -81.69291912943299394, -0.2467057407436999972 ) ) ;
#8153 = CARTESIAN_POINT ( 'NONE',  ( -12.79895942954000176, -18.19538174383999873, -2.015930660725000045 ) ) ;
#8154 = CARTESIAN_POINT ( 'NONE',  ( -1.189541931187000134, -77.16971553208000500, -12.95855809378999979 ) ) ;
#8155 = CARTESIAN_POINT ( 'NONE',  ( -5.755176823513999729, -78.22846950744899175, 9.345691860246999383 ) ) ;
#8156 = CARTESIAN_POINT ( 'NONE',  ( 12.79999999996999982, -0.1000000000339999751, -4.310453117238000074E-10 ) ) ;
#8157 = CARTESIAN_POINT ( 'NONE',  ( -4.630778388809000390, -76.57449046486000555, 11.29997541932999994 ) ) ;
#8158 = ORIENTED_EDGE ( 'NONE', *, *, #15752, .F. ) ;
#8159 = EDGE_CURVE ( 'NONE', #33091, #39794, #54028, .T. ) ;
#8160 = CARTESIAN_POINT ( 'NONE',  ( -9.497662397991334160, -77.31834923540763782, -0.2008463566140032963 ) ) ;
#8161 = CARTESIAN_POINT ( 'NONE',  ( 8.266198729575041426, -76.95520833333529254, -4.776057930356138570 ) ) ;
#8162 = CARTESIAN_POINT ( 'NONE',  ( -1.180080746428999960, -80.76608867448199192, -0.3694817012252999966 ) ) ;
#8163 = DIRECTION ( 'NONE',  ( 0.000000000000000000, 1.000000000000000000, 0.000000000000000000 ) ) ;
#8164 = CARTESIAN_POINT ( 'NONE',  ( 9.630178197611998669, -77.64399981532699258, 0.1134805908624000048 ) ) ;
#8165 = CARTESIAN_POINT ( 'NONE',  ( -3.884382724393999897, -84.62331260133198896, 1.523693970455000102 ) ) ;
#8166 = CARTESIAN_POINT ( 'NONE',  ( 6.092940285862026073, -79.92743084948268972, 8.866677603556114562 ) ) ;
#8167 = CARTESIAN_POINT ( 'NONE',  ( 1.407029943534999994, -79.84288660730200604, -0.1741439582578000189 ) ) ;
#8168 = ORIENTED_EDGE ( 'NONE', *, *, #53762, .T. ) ;
#8169 = AXIS2_PLACEMENT_3D ( 'NONE', #46966, #7078, #38364 ) ;
#8170 = CARTESIAN_POINT ( 'NONE',  ( -9.191600602562143507, -79.08998696896227898, 1.206688570074718969 ) ) ;
#8171 = CARTESIAN_POINT ( 'NONE',  ( -3.399999999999753886, -78.70000000000000284, 6.799999999999466027 ) ) ;
#8172 = ORIENTED_EDGE ( 'NONE', *, *, #5380, .T. ) ;
#8173 = VECTOR ( 'NONE', #625, 1000.000000000000227 ) ;
#8174 = VERTEX_POINT ( 'NONE', #3078 ) ;
#8175 = CARTESIAN_POINT ( 'NONE',  ( -4.263934386054000214, -78.96395401111398371, -10.07505235160000012 ) ) ;
#8176 = ADVANCED_FACE ( 'NONE', ( #7500 ), #39078, .T. ) ;
#8177 = DIRECTION ( 'NONE',  ( 1.000000000000000000, 0.000000000000000000, 0.000000000000000000 ) ) ;
#8178 = CARTESIAN_POINT ( 'NONE',  ( -8.802519067788999507, -80.25274279837199742, 7.133338619267999725 ) ) ;
#8179 = AXIS2_PLACEMENT_3D ( 'NONE', #30707, #13585, #49625 ) ;
#8180 = VERTEX_POINT ( 'NONE', #47388 ) ;
#8181 = VECTOR ( 'NONE', #27637, 1000.000000000000000 ) ;
#8182 = ORIENTED_EDGE ( 'NONE', *, *, #46535, .T. ) ;
#8183 = EDGE_LOOP ( 'NONE', ( #48961, #58303, #34680, #34060 ) ) ;
#8184 = CARTESIAN_POINT ( 'NONE',  ( -0.7706254096772040540, -78.07838742812036514, 11.74774115849858980 ) ) ;
#8185 = DIRECTION ( 'NONE',  ( -1.000000000000000000, 0.000000000000000000, 0.000000000000000000 ) ) ;
#8186 = EDGE_LOOP ( 'NONE', ( #17095, #26057, #46268, #26463 ) ) ;
#8187 = VERTEX_POINT ( 'NONE', #47101 ) ;
#8188 = CARTESIAN_POINT ( 'NONE',  ( -5.869402599192000025, -78.46567021303999923, 10.46661899222999992 ) ) ;
#8189 = CARTESIAN_POINT ( 'NONE',  ( -3.406490272659980612, -78.77851879815550262, 0.06421901112149767943 ) ) ;
#8190 = CARTESIAN_POINT ( 'NONE',  ( 7.631896578914999729, -55.57877526445999905, 10.36221705163000095 ) ) ;
#8191 = CARTESIAN_POINT ( 'NONE',  ( -0.4764073897351723819, -18.48308356130623054, 10.98970030907993589 ) ) ;
#8192 = CARTESIAN_POINT ( 'NONE',  ( -9.083128614440136417, -79.67447916666266394, 2.440148008508001620 ) ) ;
#8193 = CARTESIAN_POINT ( 'NONE',  ( -6.577349813594124406, -80.77474465748072419, 9.078716047411401036 ) ) ;
#8194 = CARTESIAN_POINT ( 'NONE',  ( 2.697636866285999968, -77.79307477553111028, -11.67213861177999945 ) ) ;
#8195 = LINE ( 'NONE', #31188, #26519 ) ;
#8196 = CARTESIAN_POINT ( 'NONE',  ( -9.422842877294000274, -25.25952027282999879, 8.643944052295999825 ) ) ;
#8197 = VECTOR ( 'NONE', #44952, 1000.000000000000000 ) ;
#8198 = CARTESIAN_POINT ( 'NONE',  ( 0.6656714966510000053, -82.12580496681198383, -4.119086676869000208 ) ) ;
#8199 = CARTESIAN_POINT ( 'NONE',  ( -0.1226781409794000105, -77.88088667140100085, -9.761919256278002166 ) ) ;
#8200 = CARTESIAN_POINT ( 'NONE',  ( -0.1636246173744726473, -83.38541666666664298, 1.249999999999999112 ) ) ;
#8201 = CYLINDRICAL_SURFACE ( 'NONE', #1910, 0.5000000000000004441 ) ;
#8202 = CARTESIAN_POINT ( 'NONE',  ( -12.27595451887999900, -75.99604523835098746, 0.3505736730271999391 ) ) ;
#8203 = CARTESIAN_POINT ( 'NONE',  ( -8.107762507645800198, -60.31691643837310579, -7.434020715870987672 ) ) ;
#8204 = AXIS2_PLACEMENT_3D ( 'NONE', #45857, #18977, #36969 ) ;
#8205 = CARTESIAN_POINT ( 'NONE',  ( -1.078908860263670499, -78.21713606389884887, -10.72771984716255567 ) ) ;
#8206 = CIRCLE ( 'NONE', #44046, 14.00000000000000000 ) ;
#8207 = CARTESIAN_POINT ( 'NONE',  ( -0.8298952231115165334, -79.92822769484411083, -1.265560781775035171 ) ) ;
#8208 = CARTESIAN_POINT ( 'NONE',  ( 5.056474866540000335, -77.19110806070449371, -7.902943353631999734 ) ) ;
#8209 = CARTESIAN_POINT ( 'NONE',  ( 1.980464483675000054, -58.55560170709000545, -12.85140862643000048 ) ) ;
#8210 = CARTESIAN_POINT ( 'NONE',  ( 8.096452064242996016, -22.78578169018999944, -13.15643568217000769 ) ) ;
#8211 = CARTESIAN_POINT ( 'NONE',  ( 7.091067894987999942, -78.54739778831900310, -10.02559399679999963 ) ) ;
#8212 = CARTESIAN_POINT ( 'NONE',  ( -8.485281374238999419, -55.54999999966999980, -8.485281374238999419 ) ) ;
#8213 = CARTESIAN_POINT ( 'NONE',  ( 0.000000000000000000, -77.19999999999998863, 0.000000000000000000 ) ) ;
#8215 = LINE ( 'NONE', #16219, #49524 ) ;
#8214 = CARTESIAN_POINT ( 'NONE',  ( -11.51299102148243136, -76.18361529713614289, 2.346991155758191283 ) ) ;
#8216 = CARTESIAN_POINT ( 'NONE',  ( -0.4887637738901999818, -82.04534299292998867, 1.384759226041999858 ) ) ;
#8217 = CARTESIAN_POINT ( 'NONE',  ( -4.048145914920218580, -79.50588259898441379, 9.958952688048560375 ) ) ;
#8218 = VERTEX_POINT ( 'NONE', #56806 ) ;
#8219 = EDGE_CURVE ( 'NONE', #54533, #57635, #15383, .T. ) ;
#8220 = CARTESIAN_POINT ( 'NONE',  ( 0.3271848554491016414, -82.14583333333331439, -1.217465845835393967 ) ) ;
#8221 = CARTESIAN_POINT ( 'NONE',  ( -2.688164603868000047, -79.29822014667099950, -11.73737721775999887 ) ) ;
#8222 = CARTESIAN_POINT ( 'NONE',  ( -4.285131888247867060, -79.16215997888556899, 8.500474416186351689 ) ) ;
#8223 = CARTESIAN_POINT ( 'NONE',  ( 7.220923959705269013, -76.97708333333335418, -9.396085398178609438 ) ) ;
#8224 = CARTESIAN_POINT ( 'NONE',  ( -11.00000000000000000, -79.09999999999999432, 0.000000000000000000 ) ) ;
#8225 = CARTESIAN_POINT ( 'NONE',  ( 2.260467989216000007, -0.8087401806307999985, -2.930715944272999973 ) ) ;
#8226 = CARTESIAN_POINT ( 'NONE',  ( 7.724294138338000160, -79.00949129696499540, 5.999925182671999480 ) ) ;
#8227 = CARTESIAN_POINT ( 'NONE',  ( 12.54983138327999903, -25.05098386350000084, -0.1356331847737999863 ) ) ;
#8228 = CARTESIAN_POINT ( 'NONE',  ( -1.667917367010000040, -60.08056692637000396, 12.49306752636999995 ) ) ;
#8229 = VERTEX_POINT ( 'NONE', #29629 ) ;
#8230 = CARTESIAN_POINT ( 'NONE',  ( 0.000000000000000000, -77.50000000000000000, 0.000000000000000000 ) ) ;
#8231 = CARTESIAN_POINT ( 'NONE',  ( 8.872958366908434868, -25.01010144684876835, -8.813896668998575379 ) ) ;
#8232 = DIRECTION ( 'NONE',  ( -2.011981753536000215E-11, -1.000000000000000000, 1.337054718097999961E-10 ) ) ;
#8233 = CARTESIAN_POINT ( 'NONE',  ( 4.000000000000000000, -78.67389998729011324, 0.000000000000000000 ) ) ;
#8234 = CARTESIAN_POINT ( 'NONE',  ( 0.2486943578317000192, -85.07292953870899055, -3.538743245300000062 ) ) ;
#8235 = ADVANCED_FACE ( 'NONE', ( #20220 ), #30205, .F. ) ;
#8236 = B_SPLINE_CURVE_WITH_KNOTS ( 'NONE', 3,
 ( #47195, #37138, #32696, #10001, #56036, #10286, #6727, #5845, #23851, #46905 ),
 .UNSPECIFIED., .F., .F.,
 ( 4, 2, 2, 2, 4 ),
 ( 0.000000000000000000, 0.2500000000000000555, 0.5000000000000000000, 0.7500000000000000000, 1.000000000000000000 ),
 .UNSPECIFIED. ) ;
#8237 = ORIENTED_EDGE ( 'NONE', *, *, #35484, .T. ) ;
#8238 = CARTESIAN_POINT ( 'NONE',  ( 0.000000000000000000, 4.040000000000000036, 0.000000000000000000 ) ) ;
#8239 = CARTESIAN_POINT ( 'NONE',  ( 3.074415043147969318, -77.84369498227056283, -11.43808899272451463 ) ) ;
#8240 = CARTESIAN_POINT ( 'NONE',  ( -1.931086388578000079, -23.29778754190000001, 12.71798269385000069 ) ) ;
#8241 = ORIENTED_EDGE ( 'NONE', *, *, #6996, .T. ) ;
#8242 = VECTOR ( 'NONE', #2829, 1000.000000000000000 ) ;
#8243 = CARTESIAN_POINT ( 'NONE',  ( -10.08162962779999994, -54.08146287347000225, -7.981572332307999673 ) ) ;
#8244 = CARTESIAN_POINT ( 'NONE',  ( 9.534323188421000239, -79.01153086664199066, -1.008198710029000189 ) ) ;
#8245 = ORIENTED_EDGE ( 'NONE', *, *, #37396, .T. ) ;
#8246 = VECTOR ( 'NONE', #10158, 1000.000000000000000 ) ;
#8247 = ORIENTED_EDGE ( 'NONE', *, *, #38413, .F. ) ;
#8248 = CARTESIAN_POINT ( 'NONE',  ( -8.566065236488999091, -77.18668866757499814, -8.735497583133000177 ) ) ;
#8249 = CYLINDRICAL_SURFACE ( 'NONE', #15481, 1.750000000000000000 ) ;
#8250 = CARTESIAN_POINT ( 'NONE',  ( 0.06134695251390999415, -79.33472580599999446, -1.460504705271000070 ) ) ;
#8251 = AXIS2_PLACEMENT_3D ( 'NONE', #54486, #23181, #8722 ) ;
#8252 = EDGE_LOOP ( 'NONE', ( #14003, #22409, #40423, #58053 ) ) ;
#8253 = EDGE_CURVE ( 'NONE', #29038, #56208, #56230, .T. ) ;
#8254 = CARTESIAN_POINT ( 'NONE',  ( 6.214091009702999102, -77.87193084965399237, -7.179311535719000048 ) ) ;
#8255 = DIRECTION ( 'NONE',  ( -1.000000000000000000, 0.000000000000000000, 0.000000000000000000 ) ) ;
#8256 = AXIS2_PLACEMENT_3D ( 'NONE', #20300, #37715, #55737 ) ;
#8257 = CARTESIAN_POINT ( 'NONE',  ( 0.8515566320460936645, -80.28524471423844489, -0.9156626745943138301 ) ) ;
#8258 = CARTESIAN_POINT ( 'NONE',  ( 7.406580528771000260, -77.66714066711000442, -10.82165712228000132 ) ) ;
#8259 = CARTESIAN_POINT ( 'NONE',  ( -10.93308570624999732, -78.26793868655188646, -2.507139558745000052 ) ) ;
#8260 = CARTESIAN_POINT ( 'NONE',  ( 12.51072239526000196, -26.30294702885999669, -0.7871079366006996647 ) ) ;
#8261 = CARTESIAN_POINT ( 'NONE',  ( -3.547560735670414633, -86.36264283715698298, 1.500007025275827521 ) ) ;
#8262 = DIRECTION ( 'NONE',  ( -0.07798810297684731496, 0.04890180918263831167, -0.9957542211071653826 ) ) ;
#8263 = CARTESIAN_POINT ( 'NONE',  ( -2.226953637271548825, -79.99461437525772567, 9.002238948001519248 ) ) ;
#8264 = CARTESIAN_POINT ( 'NONE',  ( 7.635939924825046354, -18.22474192286703598, 10.36595855977228453 ) ) ;
#8265 = EDGE_LOOP ( 'NONE', ( #22869, #31244, #57323, #16233 ) ) ;
#8266 = CARTESIAN_POINT ( 'NONE',  ( 6.153863461931999623, -76.21865827134000426, -10.66140155521000032 ) ) ;
#8267 = CARTESIAN_POINT ( 'NONE',  ( -1.304983203281999904, -80.23020634875099688, 0.1938670925079999940 ) ) ;
#8268 = CARTESIAN_POINT ( 'NONE',  ( -12.56594317989000054, -23.24999999414999863, -1.750000000001000089 ) ) ;
#8269 = CARTESIAN_POINT ( 'NONE',  ( 1.184104130434999957, -78.37171603715040646, -0.5817757459379000462 ) ) ;
#8270 = CARTESIAN_POINT ( 'NONE',  ( 1.978728478177648853, -3.021815653195938367, -2.910175349659095634 ) ) ;
#8271 = CARTESIAN_POINT ( 'NONE',  ( 12.69616050742999924, -21.75171076523999858, 1.799475304559999822 ) ) ;
#8272 = DIRECTION ( 'NONE',  ( 1.000000000000000000, 0.000000000000000000, 0.000000000000000000 ) ) ;
#8273 = CARTESIAN_POINT ( 'NONE',  ( -8.813891479790338934, -61.81010130340408892, -8.872963529899354995 ) ) ;
#8274 = CARTESIAN_POINT ( 'NONE',  ( -6.511242784100999437, -78.98152414433498336, 9.060646613982999753 ) ) ;
#8275 = CARTESIAN_POINT ( 'NONE',  ( 10.35747145892000098, -23.31584731985000047, -7.626500777234999973 ) ) ;
#8276 = CARTESIAN_POINT ( 'NONE',  ( -1.155509423026611415, -83.06897101105678871, 0.4765901429544092682 ) ) ;
#8277 = CARTESIAN_POINT ( 'NONE',  ( 1.620688577297000110, -80.65142343270998992, -3.844466678252000058 ) ) ;
#8278 = B_SPLINE_SURFACE_WITH_KNOTS ( 'NONE', 3, 3, ( 
 ( #3463, #41156, #749, #40870 ),
 ( #461, #45898, #18441, #36431 ),
 ( #54458, #18728, #36722, #5430 ),
 ( #54736, #57194, #4566, #21469 ),
 ( #35843, #53872, #13405, #24320 ),
 ( #55318, #24020, #6306, #15160 ),
 ( #29030, #20187, #1902, #19896 ),
 ( #37888, #5720, #37010, #47360 ),
 ( #11332, #42335, #33744, #28731 ),
 ( #51780, #19019, #56200, #10166 ),
 ( #33156, #55613, #51200, #23730 ),
 ( #24609, #55910, #38179, #55027 ),
 ( #10754, #23439, #46782, #10452 ),
 ( #32567, #42624, #1318, #46486 ),
 ( #15463, #50615, #2188, #33454 ),
 ( #51491, #11049, #47070, #19596 ),
 ( #37596, #28141, #28439, #6599 ) ),
 .UNSPECIFIED., .F., .F., .F.,
 ( 4, 1, 1, 1, 1, 1, 1, 1, 1, 1, 1, 1, 1, 1, 4 ),
 ( 4, 4 ),
 ( -0.01011408452870000106, 0.000000000000000000, 0.08333333333333001192, 0.1666666666667000196, 0.2500000000000000000, 0.3333333333333000081, 0.4166666666666999919, 0.5000000000000000000, 0.5833333333333000637, 0.6666666666667000474, 0.7500000000000000000, 0.8333333333333000637, 0.9166666666667000474, 1.000000000000000000, 1.010362559107000013 ),
 ( -0.3559705546267999954, 1.357612419600999987 ),
 .UNSPECIFIED. ) ;
#8279 = CARTESIAN_POINT ( 'NONE',  ( -10.47020627418440242, -77.97916666666668561, 2.813789756862221214 ) ) ;
#8280 = VERTEX_POINT ( 'NONE', #42944 ) ;
#8281 = CARTESIAN_POINT ( 'NONE',  ( -1.400413196275999805, -83.43236633857299012, 0.4410028580390000230 ) ) ;
#8282 = CARTESIAN_POINT ( 'NONE',  ( 0.5769282351073999893, -81.29952822830999537, 1.350407801515999928 ) ) ;
#8283 = CARTESIAN_POINT ( 'NONE',  ( -10.68110250243102399, -79.11058856173531240, -1.407228983746247941 ) ) ;
#8284 = CARTESIAN_POINT ( 'NONE',  ( 1.720939166139000109, -77.13497768101099439, -11.69973432676000158 ) ) ;
#8285 = CARTESIAN_POINT ( 'NONE',  ( 4.518822441307924542, -77.00000000000000000, 8.100777538286340729 ) ) ;
#8286 = CARTESIAN_POINT ( 'NONE',  ( -12.50000000000000000, -55.54999999966999980, 1.250000000000000000 ) ) ;
#8287 = CARTESIAN_POINT ( 'NONE',  ( -8.118170145944999305, -78.64206171986300831, -8.748189294319999476 ) ) ;
#8288 = CARTESIAN_POINT ( 'NONE',  ( 2.013632425233999879, -78.33175584965400162, -9.512575055159999238 ) ) ;
#8289 = CARTESIAN_POINT ( 'NONE',  ( -10.36597333712761326, -23.77522429014145544, -7.635925938716360051 ) ) ;
#8290 = CARTESIAN_POINT ( 'NONE',  ( 11.67550463150810991, -75.95899070002479903, 1.336096097494961832 ) ) ;
#8291 = CARTESIAN_POINT ( 'NONE',  ( -3.684198380124617866, -86.09999999999999432, 1.557781209248835008 ) ) ;
#8292 = EDGE_LOOP ( 'NONE', ( #20254, #42892, #11249, #48989 ) ) ;
#8293 = CARTESIAN_POINT ( 'NONE',  ( -0.7528178228308939346, -79.57551938009331138, -1.041016560679725478 ) ) ;
#8294 = ADVANCED_FACE ( 'NONE', ( #2499 ), #3380, .F. ) ;
#8295 = CARTESIAN_POINT ( 'NONE',  ( -5.913247735470008593, -77.11512497811247613, 10.26344855921360733 ) ) ;
#8296 = CARTESIAN_POINT ( 'NONE',  ( -12.27099179350999947, -79.32713975210698720, -0.08468213707432999116 ) ) ;
#8297 = CARTESIAN_POINT ( 'NONE',  ( 3.999999999999605649, -78.67389998729009903, -2.360693579763057492 ) ) ;
#8298 = EDGE_CURVE ( 'NONE', #31756, #15737, #9795, .T. ) ;
#8299 = CARTESIAN_POINT ( 'NONE',  ( 0.5269479332349999989, -83.17899772590298824, 1.580352090963000000 ) ) ;
#8300 = CARTESIAN_POINT ( 'NONE',  ( 5.151324428776999476, -77.67092400397599761, 9.964033682248000900 ) ) ;
#8301 = CARTESIAN_POINT ( 'NONE',  ( 10.94409238582999855, -78.68618361078299017, 0.8311789410725000105 ) ) ;
#8302 = CARTESIAN_POINT ( 'NONE',  ( 1.217390015642536349, -17.18106975072029741, 12.70229597940824107 ) ) ;
#8303 = CARTESIAN_POINT ( 'NONE',  ( 12.02938582184000005, -76.71030382554799587, 2.954811323672000167 ) ) ;
#8304 = CARTESIAN_POINT ( 'NONE',  ( -0.2078146149822125144, -79.51265551170533286, -1.400962704543201154 ) ) ;
#8305 = CARTESIAN_POINT ( 'NONE',  ( 9.678374330664796688, -76.78695867686717236, 4.842468990515385485 ) ) ;
#8306 = ORIENTED_EDGE ( 'NONE', *, *, #36214, .T. ) ;
#8307 = CARTESIAN_POINT ( 'NONE',  ( -1.769784341028000085, -79.82117545184989638, -11.00556513567000039 ) ) ;
#8308 = CARTESIAN_POINT ( 'NONE',  ( 1.249963906870020347, -79.86378459473635871, 0.2155801268755469513 ) ) ;
#8309 = COLOUR_RGB ( '', 0.09019608, 0.27058824, 0.51372549) ;
#8310 = CARTESIAN_POINT ( 'NONE',  ( 10.86862532138017912, -77.93584017775066286, -1.957230818804968520 ) ) ;
#8311 = EDGE_CURVE ( 'NONE', #19156, #46351, #47484, .T. ) ;
#8312 = CARTESIAN_POINT ( 'NONE',  ( -10.99582742793000101, -79.22949549020498239, 1.892981466416000069 ) ) ;
#8313 = CARTESIAN_POINT ( 'NONE',  ( 7.000000000000000000, -81.19999999999998863, -1.000000000000000000 ) ) ;
#8314 = CARTESIAN_POINT ( 'NONE',  ( 10.99071003982047579, -23.54576790506894923, -0.4528411669651079552 ) ) ;
#8315 = PRODUCT ( 'Spring', 'Spring', '', ( #42338 ) ) ;
#8316 = CARTESIAN_POINT ( 'NONE',  ( 6.187157694146999454, -78.15957020342199257, 10.60730214752000045 ) ) ;
#8317 = CARTESIAN_POINT ( 'NONE',  ( 8.813906588475214576, -16.98989792586488434, -8.872948313418005384 ) ) ;
#8318 = CARTESIAN_POINT ( 'NONE',  ( -9.469606800734000629, -79.65752053325199711, 5.597012331546999953 ) ) ;
#8319 = CARTESIAN_POINT ( 'NONE',  ( -10.07627163191000008, -23.24999999758999536, -7.601397897754999633 ) ) ;
#8320 = VERTEX_POINT ( 'NONE', #49699 ) ;
#8321 = ORIENTED_EDGE ( 'NONE', *, *, #48454, .T. ) ;
#8322 = CARTESIAN_POINT ( 'NONE',  ( 10.65991607774613747, -78.83964975953574594, -1.400468160174369148 ) ) ;
#8323 = CARTESIAN_POINT ( 'NONE',  ( 3.670568130644999982, -77.97173998579799559, 8.453023018411998990 ) ) ;
#8324 = EDGE_LOOP ( 'NONE', ( #39747, #43908, #40648, #2977 ) ) ;
#8325 = FACE_OUTER_BOUND ( 'NONE', #28064, .T. ) ;
#8326 = ORIENTED_EDGE ( 'NONE', *, *, #2481, .T. ) ;
#8327 = CARTESIAN_POINT ( 'NONE',  ( 9.029867227896000159, -25.33262194290999858, 9.038867509618000895 ) ) ;
#8328 = CARTESIAN_POINT ( 'NONE',  ( -5.762797186001000327, -77.55987522413700219, 9.407013499219999630 ) ) ;
#8329 = CIRCLE ( 'NONE', #4554, 1.750000000000000222 ) ;
#8330 = CARTESIAN_POINT ( 'NONE',  ( 9.342221983604002133, -78.35803998579800123, -2.562053005734000077 ) ) ;
#8331 = CARTESIAN_POINT ( 'NONE',  ( -9.235030002071850319, -78.10620107062753448, -0.6966500853201260668 ) ) ;
#8332 = CARTESIAN_POINT ( 'NONE',  ( 3.371435477143000181, -79.34761125869799514, -10.69820234502000034 ) ) ;
#8333 = ORIENTED_EDGE ( 'NONE', *, *, #53277, .F. ) ;
#8334 = VERTEX_POINT ( 'NONE', #53234 ) ;
#8335 = CARTESIAN_POINT ( 'NONE',  ( -4.200795967633649042, -77.51264282153384499, 8.241008886275963619 ) ) ;
#8336 = DIRECTION ( 'NONE',  ( 0.000000000000000000, -1.000000000000000000, 0.000000000000000000 ) ) ;
#8337 = CARTESIAN_POINT ( 'NONE',  ( 0.1963495408493571015, -77.86458333333330017, 1.500000000000000444 ) ) ;
#8338 = ADVANCED_FACE ( 'NONE', ( #40236 ), #29520, .F. ) ;
#8339 = CARTESIAN_POINT ( 'NONE',  ( 9.512131559252001267, -78.12459716941698673, -1.920953556448999899 ) ) ;
#8340 = CARTESIAN_POINT ( 'NONE',  ( 6.585972550682999582, -76.08593941427999141, -11.16860520736000062 ) ) ;
#8341 = AXIS2_PLACEMENT_3D ( 'NONE', #12135, #30123, #57005 ) ;
#8342 = CARTESIAN_POINT ( 'NONE',  ( -8.991148217401329745, -79.42591775919153463, -3.068505234713029051 ) ) ;
#8343 = CARTESIAN_POINT ( 'NONE',  ( 7.792421629638690561, -54.50899070338012820, -10.18245656324170412 ) ) ;
#8344 = CARTESIAN_POINT ( 'NONE',  ( 7.117135278674999732, -80.25067289479999033, 8.718833803912000135 ) ) ;
#8345 = DIRECTION ( 'NONE',  ( 0.000000000000000000, 1.000000000000000000, 0.000000000000000000 ) ) ;
#8346 = CARTESIAN_POINT ( 'NONE',  ( 1.250000000000000000, -78.25000000000000000, 0.000000000000000000 ) ) ;
#8347 = CARTESIAN_POINT ( 'NONE',  ( 2.421167930323352646, -78.64583333333331439, -9.009247259181915268 ) ) ;
#8348 = ORIENTED_EDGE ( 'NONE', *, *, #5405, .F. ) ;
#8349 = CARTESIAN_POINT ( 'NONE',  ( 1.476561009027000049, -79.44184242973399535, 11.99329713346000048 ) ) ;
#8350 = CARTESIAN_POINT ( 'NONE',  ( -7.620012214408999895, -55.59439747889000216, 10.53562508622999871 ) ) ;
#8351 = CARTESIAN_POINT ( 'NONE',  ( 1.001315001700999963, -54.11477588220000001, 12.50000000000000000 ) ) ;
#8352 = CARTESIAN_POINT ( 'NONE',  ( -12.70722176278296267, -61.21036110582522127, 1.610175936235292760 ) ) ;
#8354 = CARTESIAN_POINT ( 'NONE',  ( -1.698401934077000019, -17.77985954096000043, -12.66748707612999958 ) ) ;
#8353 = CARTESIAN_POINT ( 'NONE',  ( -9.250000000000000000, -78.59999999999999432, 0.000000000000000000 ) ) ;
#8355 = DIRECTION ( 'NONE',  ( 0.0001178721535688749143, 0.000000000000000000, -0.9999999930530777403 ) ) ;
#8356 = CARTESIAN_POINT ( 'NONE',  ( 10.89190632572000084, -80.28569813701800229, -2.978178067245000005 ) ) ;
#8357 = CARTESIAN_POINT ( 'NONE',  ( -9.252740428348994683, -78.32083333333335418, -2.486604901413163926 ) ) ;
#8358 = CARTESIAN_POINT ( 'NONE',  ( -11.21475409559999825, -76.81611249766200444, 1.031226285144000165 ) ) ;
#8359 = CARTESIAN_POINT ( 'NONE',  ( 0.000000000000000000, 4.040000000000000036, 0.000000000000000000 ) ) ;
#8360 = CARTESIAN_POINT ( 'NONE',  ( 2.879226727952050258, -80.05416666667792924, 10.71369944335148361 ) ) ;
#8361 = VERTEX_POINT ( 'NONE', #27231 ) ;
#8362 = CARTESIAN_POINT ( 'NONE',  ( 12.00000000000000000, -18.84999999999999787, 0.000000000000000000 ) ) ;
#8363 = CARTESIAN_POINT ( 'NONE',  ( 0.000000000000000000, -80.74999999950000529, 0.000000000000000000 ) ) ;
#8364 = CARTESIAN_POINT ( 'NONE',  ( 3.500567196895000510, -2.403996213896999912, 1.018756774997999992 ) ) ;
#8365 = EDGE_CURVE ( 'NONE', #34885, #23335, #17214, .T. ) ;
#8366 = CARTESIAN_POINT ( 'NONE',  ( -3.513443458492000016, -78.29796450147399867, -10.65240647004999985 ) ) ;
#8367 = CARTESIAN_POINT ( 'NONE',  ( 3.250000000000000444, -1.739583333333333037, -0.4254240051736113415 ) ) ;
#8368 = FACE_OUTER_BOUND ( 'NONE', #40784, .T. ) ;
#8369 = CARTESIAN_POINT ( 'NONE',  ( -1.632307027704000157, -60.46927189524000568, 12.46200249215000078 ) ) ;
#8370 = CARTESIAN_POINT ( 'NONE',  ( 12.77656766273999978, -16.68801851262999847, 0.1555695072196000006 ) ) ;
#8371 = CARTESIAN_POINT ( 'NONE',  ( 2.169073408916999846, -85.88132450217399594, 3.514774583532000118 ) ) ;
#8372 = CIRCLE ( 'NONE', #55499, 1.000000000000000000 ) ;
#8373 = CARTESIAN_POINT ( 'NONE',  ( -7.901937438446521966, -76.05000000000001137, 8.782705132841526208 ) ) ;
#8374 = CARTESIAN_POINT ( 'NONE',  ( -8.714384359252477452, -76.89210801961958452, 8.361740495897693748 ) ) ;
#8375 = EDGE_CURVE ( 'NONE', #27205, #37084, #44625, .T. ) ;
#8376 = CARTESIAN_POINT ( 'NONE',  ( 9.107239040596999402, -78.07663815498800375, 6.625115969983998987 ) ) ;
#8377 = CARTESIAN_POINT ( 'NONE',  ( 0.4690275182270805532, -81.94447212118758728, 1.158641618440934051 ) ) ;
#8378 = CARTESIAN_POINT ( 'NONE',  ( 1.195585824879000114, -78.14121194367999124, 1.156768630296999945 ) ) ;
#8379 = CARTESIAN_POINT ( 'NONE',  ( 9.199999999999999289, -79.79999999999999716, 0.000000000000000000 ) ) ;
#8380 = CYLINDRICAL_SURFACE ( 'NONE', #57640, 0.5000000000000004441 ) ;
#8381 = CARTESIAN_POINT ( 'NONE',  ( -2.839805762151337731, -2.541666666666666519, -1.636761686205423949 ) ) ;
#8382 = CARTESIAN_POINT ( 'NONE',  ( 1.795800964791006482, -80.23879961656356841, -10.60311702371338960 ) ) ;
#8383 = CARTESIAN_POINT ( 'NONE',  ( -12.50409240825461765, -24.52129362382453337, -1.233800929768802401 ) ) ;
#8384 = CARTESIAN_POINT ( 'NONE',  ( -8.894932048719153883, -16.77190732483956737, -9.073469156704689453 ) ) ;
#8385 = CIRCLE ( 'NONE', #6501, 4.999999999999996447 ) ;
#8386 = EDGE_LOOP ( 'NONE', ( #57549, #46961, #36867, #2539 ) ) ;
#8387 = B_SPLINE_CURVE_WITH_KNOTS ( 'NONE', 3,
 ( #24498, #38931, #29768, #10935, #7355, #34199 ),
 .UNSPECIFIED., .F., .F.,
 ( 4, 1, 1, 4 ),
 ( 0.000000000000000000, 0.3333333333333000081, 0.6666666666667000474, 1.000000000000000000 ),
 .UNSPECIFIED. ) ;
#8388 = CARTESIAN_POINT ( 'NONE',  ( 8.583665413911145237, -53.82814424961789257, 9.102144265363879327 ) ) ;
#8389 = DIRECTION ( 'NONE',  ( 0.000000000000000000, -1.000000000000000000, 0.000000000000000000 ) ) ;
#8390 = CARTESIAN_POINT ( 'NONE',  ( 2.047466772651000078, -79.96295766602578681, -11.07437783411999987 ) ) ;
#8391 = CARTESIAN_POINT ( 'NONE',  ( 0.1636246173744697330, -80.13541666666665719, -1.249999999999999778 ) ) ;
#8392 = ORIENTED_EDGE ( 'NONE', *, *, #46302, .F. ) ;
#8393 = EDGE_LOOP ( 'NONE', ( #55972, #52073, #32992, #33298 ) ) ;
#8394 = CARTESIAN_POINT ( 'NONE',  ( -0.5897045597925999472, -82.08556254607600522, -1.428858609762999832 ) ) ;
#8395 = ORIENTED_EDGE ( 'NONE', *, *, #57426, .F. ) ;
#8396 = CARTESIAN_POINT ( 'NONE',  ( -12.50745077490000057, -24.99994448286999926, -2.662114616045000020E-09 ) ) ;
#8397 = ORIENTED_EDGE ( 'NONE', *, *, #20120, .T. ) ;
#8398 = DIRECTION ( 'NONE',  ( 0.000000000000000000, -1.000000000000000000, 0.000000000000000000 ) ) ;
#8399 = CARTESIAN_POINT ( 'NONE',  ( 0.9618768815558239593, -79.14322916213880887, -3.272074968132094863 ) ) ;
#8400 = CARTESIAN_POINT ( 'NONE',  ( 4.528616239255999432, -78.73244931796000401, -9.933126443765001312 ) ) ;
#8401 = CARTESIAN_POINT ( 'NONE',  ( 1.484804496640999893, -24.71869153383000040, -12.77261165608999960 ) ) ;
#8402 = CARTESIAN_POINT ( 'NONE',  ( 3.952142091860000317, -79.77245509461999973, 0.2942162200264000216 ) ) ;
#8403 = CARTESIAN_POINT ( 'NONE',  ( 1.470118532801963473, -79.26259840585061056, 9.385540567805065848 ) ) ;
#8404 = ORIENTED_EDGE ( 'NONE', *, *, #21135, .T. ) ;
#8405 = CARTESIAN_POINT ( 'NONE',  ( 10.69999999997999929, -81.80000000002199556, -2.760617010408999913E-10 ) ) ;
#8406 = CARTESIAN_POINT ( 'NONE',  ( 0.4517264908803999557, -78.63353063649999797, -12.35021147003999964 ) ) ;
#8407 = ORIENTED_EDGE ( 'NONE', *, *, #28500, .T. ) ;
#8408 = CARTESIAN_POINT ( 'NONE',  ( 0.000000000000000000, -45.91785611817000046, 0.000000000000000000 ) ) ;
#8409 = ADVANCED_FACE ( 'NONE', ( #4819 ), #34919, .F. ) ;
#8410 = CARTESIAN_POINT ( 'NONE',  ( 1.313995274498999999, -80.50198802361599348, -0.2280190045613000038 ) ) ;
#8411 = DIRECTION ( 'NONE',  ( 1.000000000000000000, 0.000000000000000000, 0.000000000000000000 ) ) ;
#8412 = VECTOR ( 'NONE', #16989, 1000.000000000000227 ) ;
#8413 = CARTESIAN_POINT ( 'NONE',  ( 12.00000000000000000, -23.25000000000000000, 0.000000000000000000 ) ) ;
#8414 = CARTESIAN_POINT ( 'NONE',  ( -2.746347158439794267, -86.07377126432851355, 2.036105618457984434 ) ) ;
#8415 = CARTESIAN_POINT ( 'NONE',  ( 7.344138154013000630, -78.17792498495001041, -10.86413439232000044 ) ) ;
#8416 = EDGE_CURVE ( 'NONE', #31547, #27322, #11644, .T. ) ;
#8417 = CARTESIAN_POINT ( 'NONE',  ( -1.001315001699999874, -54.11477588220000001, -12.50000000000000000 ) ) ;
#8418 = CARTESIAN_POINT ( 'NONE',  ( 10.68461344661000112, -76.26131943937400592, -2.075949589353000224 ) ) ;
#8419 = CARTESIAN_POINT ( 'NONE',  ( -9.210376165418230343, -78.60745015110788358, -0.8564966472666962760 ) ) ;
#8420 = CARTESIAN_POINT ( 'NONE',  ( -3.867642873348000165, -82.05721315976299479, -0.8644818823220999926 ) ) ;
#8421 = CIRCLE ( 'NONE', #31974, 0.5000000000000004441 ) ;
#8422 = CARTESIAN_POINT ( 'NONE',  ( -10.35845608626999947, -60.09778754156999980, 7.627487525433000570 ) ) ;
#8423 = CARTESIAN_POINT ( 'NONE',  ( 0.4879870162820874047, -2.964277948476393920, 3.219086890419578406 ) ) ;
#8424 = CARTESIAN_POINT ( 'NONE',  ( 1.377960558539999880, -80.68280496681198599, -3.268453312188999593 ) ) ;
#8425 = AXIS2_PLACEMENT_3D ( 'NONE', #38537, #7247, #48571 ) ;
#8426 = CARTESIAN_POINT ( 'NONE',  ( 11.84266115483542237, -77.53516788874328824, -2.236516232491893241 ) ) ;
#8427 = CARTESIAN_POINT ( 'NONE',  ( -0.9320940738602599973, -80.98202026695135203, 10.70948474841207876 ) ) ;
#8428 = CARTESIAN_POINT ( 'NONE',  ( -2.895922040489999905, -80.29737158873430758, 10.88681414971999928 ) ) ;
#8429 = B_SPLINE_CURVE_WITH_KNOTS ( 'NONE', 3,
 ( #35743, #40480, #18052, #44912, #58193, #36044, #53774, #16889, #49347, #4469, #12167, #30153, #26308, #48204, #34870, #21307, #7735, #52901, #12450, #48476, #3879, #39886, #5622, #10354, #54068, #49938, #50225, #19500, #54928, #36917 ),
 .UNSPECIFIED., .F., .F.,
 ( 4, 2, 2, 2, 2, 2, 2, 2, 2, 2, 2, 2, 2, 2, 4 ),
 ( 0.000000000000000000, 0.06250000000000001388, 0.1250000000000000278, 0.1875000000000000555, 0.2500000000000000555, 0.3125000000000000555, 0.3750000000000001110, 0.4375000000000001110, 0.5000000000000001110, 0.6250000000000001110, 0.6875000000000001110, 0.7500000000000002220, 0.8750000000000001110, 0.9375000000000001110, 1.000000000000000000 ),
 .UNSPECIFIED. ) ;
#8430 = CARTESIAN_POINT ( 'NONE',  ( -3.593558748265999636, -1.745109825020999983, 0.1459214154804999997 ) ) ;
#8431 = CARTESIAN_POINT ( 'NONE',  ( -0.2777255150705856823, -79.64247121934312190, 1.244507665173133715 ) ) ;
#8432 = ORIENTED_EDGE ( 'NONE', *, *, #13062, .F. ) ;
#8433 = CARTESIAN_POINT ( 'NONE',  ( 1.406250000003000045, -82.09374999999700151, -9.314605757769000352E-11 ) ) ;
#8434 = CARTESIAN_POINT ( 'NONE',  ( 0.000000000000000000, -81.79999999999998295, 0.000000000000000000 ) ) ;
#8435 = CARTESIAN_POINT ( 'NONE',  ( 0.8962411872155999770, -81.53824265348700351, 0.9875868993909000526 ) ) ;
#8436 = CARTESIAN_POINT ( 'NONE',  ( 0.9983493978779336420, -79.03333333333330302, -9.480860074790918191 ) ) ;
#8437 = CARTESIAN_POINT ( 'NONE',  ( 12.55073801092999908, -77.21139148068000679, -3.437763296274999991 ) ) ;
#8438 = CARTESIAN_POINT ( 'NONE',  ( -6.030860253222999567, -79.64106001420199732, -7.365124455302999529 ) ) ;
#8439 = CARTESIAN_POINT ( 'NONE',  ( 0.000000000000000000, -75.20000000000000284, 0.000000000000000000 ) ) ;
#8440 = VERTEX_POINT ( 'NONE', #8072 ) ;
#8441 = CARTESIAN_POINT ( 'NONE',  ( 9.468749999988999022, -76.98125000001098783, 2.084568677130999610E-09 ) ) ;
#8442 = EDGE_CURVE ( 'NONE', #27322, #15167, #30780, .T. ) ;
#8443 = CARTESIAN_POINT ( 'NONE',  ( 1.200322591745000000, -82.09112869963200865, 0.7368979351527999988 ) ) ;
#8444 = CARTESIAN_POINT ( 'NONE',  ( -1.930989144707000005, -21.75365779208000205, -12.80900240953000058 ) ) ;
#8445 = CARTESIAN_POINT ( 'NONE',  ( 9.400066902809999903, -78.76658531640698868, -0.4999367261865000356 ) ) ;
#8446 = ADVANCED_FACE ( 'NONE', ( #44374, #3926 ), #35497, .T. ) ;
#8447 = CARTESIAN_POINT ( 'NONE',  ( 2.283490840499000196, -82.69930595706300380, 3.492230424653999687 ) ) ;
#8448 = CARTESIAN_POINT ( 'NONE',  ( -2.062597265787999845, -59.58461666436000570, -12.87024489159000140 ) ) ;
#8449 = CARTESIAN_POINT ( 'NONE',  ( 0.2147767365671000017, -80.23978759434999120, -1.401402989476999927 ) ) ;
#8450 = ORIENTED_EDGE ( 'NONE', *, *, #45774, .T. ) ;
#8451 = CARTESIAN_POINT ( 'NONE',  ( 0.02140828840467117605, -77.22524110190225599, -10.74993023099652412 ) ) ;
#8452 = CARTESIAN_POINT ( 'NONE',  ( -1.250000000000000000, -82.25000000000000000, 8.279869130157999738E-11 ) ) ;
#8453 = CARTESIAN_POINT ( 'NONE',  ( -3.490339670599558630, -78.76207911824394614, -1.975393177341282946 ) ) ;
#8454 = ORIENTED_EDGE ( 'NONE', *, *, #48239, .T. ) ;
#8455 = ORIENTED_EDGE ( 'NONE', *, *, #38169, .T. ) ;
#8456 = CARTESIAN_POINT ( 'NONE',  ( -7.666647577134583003, -55.04957415510975949, -7.889735440108408326 ) ) ;
#8457 = CARTESIAN_POINT ( 'NONE',  ( -1.662118031109000027, -80.35591171894299123, -10.80109114220999977 ) ) ;
#8458 = ORIENTED_EDGE ( 'NONE', *, *, #26849, .T. ) ;
#8459 = CARTESIAN_POINT ( 'NONE',  ( 7.972949129781999211, -77.44073956883799781, -9.187753233325999247 ) ) ;
#8460 = AXIS2_PLACEMENT_3D ( 'NONE', #52403, #52974, #25811 ) ;
#8461 = EDGE_LOOP ( 'NONE', ( #35980, #240, #9526, #11616 ) ) ;
#8462 = ORIENTED_EDGE ( 'NONE', *, *, #11446, .T. ) ;
#8463 = CIRCLE ( 'NONE', #9414, 12.50000000000000000 ) ;
#8464 = EDGE_CURVE ( 'NONE', #50392, #50856, #46444, .T. ) ;
#8465 = CARTESIAN_POINT ( 'NONE',  ( 12.00000000000000000, -78.54999999999999716, 0.000000000000000000 ) ) ;
#8466 = CARTESIAN_POINT ( 'NONE',  ( 12.04999999926000243, -79.29999999926000953, 5.384918141074000180E-09 ) ) ;
#8467 = VERTEX_POINT ( 'NONE', #18399 ) ;
#8468 = CARTESIAN_POINT ( 'NONE',  ( 10.99069764842708175, -18.45457471225845580, 0.4531388007100142223 ) ) ;
#8469 = ORIENTED_EDGE ( 'NONE', *, *, #17541, .T. ) ;
#8470 = CARTESIAN_POINT ( 'NONE',  ( -1.136454603970731725, -80.68718303390609492, -0.5770417699229399844 ) ) ;
#8471 = CARTESIAN_POINT ( 'NONE',  ( -2.089807409446279074, -78.91452042059378869, -3.465957297018673611 ) ) ;
#8472 = CARTESIAN_POINT ( 'NONE',  ( 0.000000000000000000, 0.000000000000000000, 12.00000000000000000 ) ) ;
#8473 = B_SPLINE_CURVE_WITH_KNOTS ( 'NONE', 3,
 ( #46128, #31923, #23376, #9509, #5083, #685 ),
 .UNSPECIFIED., .F., .F.,
 ( 4, 2, 4 ),
 ( 0.000000000000000000, 0.5000000000000000000, 1.000000000000000000 ),
 .UNSPECIFIED. ) ;
#8474 = CARTESIAN_POINT ( 'NONE',  ( -10.85772169724999969, -76.68550427251300050, 1.763485056683000041 ) ) ;
#8475 = CARTESIAN_POINT ( 'NONE',  ( -2.455355391147715061, -79.62239583332932114, 9.133204103880812497 ) ) ;
#8476 = ADVANCED_FACE ( 'NONE', ( #51158 ), #42206, .F. ) ;
#8477 = CARTESIAN_POINT ( 'NONE',  ( -1.247385798842000071, -54.32277743483000165, 12.50301438874000048 ) ) ;
#8478 = CARTESIAN_POINT ( 'NONE',  ( 7.705142895592000052, -58.55083378327000077, -10.24998526315000014 ) ) ;
#8479 = CARTESIAN_POINT ( 'NONE',  ( 9.072454766260275250, -78.83445074300934152, -1.803379576545697471 ) ) ;
#8480 = VECTOR ( 'NONE', #25913, 1000.000000000000000 ) ;
#8481 = DIRECTION ( 'NONE',  ( 0.000000000000000000, 0.000000000000000000, 1.000000000000000000 ) ) ;
#8482 = CARTESIAN_POINT ( 'NONE',  ( -1.500000000000000222, -79.91041666666666288, -0.1963495408493622363 ) ) ;
#8483 = B_SPLINE_CURVE_WITH_KNOTS ( 'NONE', 3,
 ( #41813, #817, #14067, #13770, #1388, #55389 ),
 .UNSPECIFIED., .F., .F.,
 ( 4, 1, 1, 4 ),
 ( 0.000000000000000000, 0.3333333333333000081, 0.6666666666667000474, 1.000000000000000000 ),
 .UNSPECIFIED. ) ;
#8484 = CARTESIAN_POINT ( 'NONE',  ( -0.06117039151549000242, -79.84105496681198133, 4.172088263230999239 ) ) ;
#8485 = CARTESIAN_POINT ( 'NONE',  ( 9.762601837900000135, -77.00728667140100470, 0.04909978866182999196 ) ) ;
#8486 = CARTESIAN_POINT ( 'NONE',  ( 5.800000004703999679, -81.00000000470399186, -2.775962740116999943E-08 ) ) ;
#8487 = FACE_OUTER_BOUND ( 'NONE', #37661, .T. ) ;
#8488 = CARTESIAN_POINT ( 'NONE',  ( -1.798954018882000128, -23.21530973387000074, 12.61117007302000026 ) ) ;
#8489 = LINE ( 'NONE', #53079, #1623 ) ;
#8490 = CARTESIAN_POINT ( 'NONE',  ( -1.067023211856000131, -1.656831454374000145, -3.462241726570000289 ) ) ;
#8491 = CARTESIAN_POINT ( 'NONE',  ( 0.3271848554490964789, -80.85416666666665719, 1.217465845835395521 ) ) ;
#8492 = CARTESIAN_POINT ( 'NONE',  ( 0.9540091777473798107, -80.17115348262751695, 1.221456096381576151 ) ) ;
#8493 = CARTESIAN_POINT ( 'NONE',  ( 12.54983138332999815, -61.85098386317000063, -0.1356331847737999863 ) ) ;
#8494 = DIRECTION ( 'NONE',  ( -1.000000000000000000, 0.000000000000000000, 0.000000000000000000 ) ) ;
#8495 = FACE_OUTER_BOUND ( 'NONE', #24395, .T. ) ;
#8496 = CARTESIAN_POINT ( 'NONE',  ( -3.157677208335999630, -77.12823906290799414, -10.45009290908999944 ) ) ;
#8497 = CIRCLE ( 'NONE', #7594, 12.57042253521000141 ) ;
#8498 = CARTESIAN_POINT ( 'NONE',  ( -12.26242965668000018, -77.86916490272500369, 0.6546740380507000134 ) ) ;
#8499 = CARTESIAN_POINT ( 'NONE',  ( -1.310679582531389498, -80.95833333333332860, 0.7554284705563444335 ) ) ;
#8500 = AXIS2_PLACEMENT_3D ( 'NONE', #37722, #1443, #14404 ) ;
#8502 = CARTESIAN_POINT ( 'NONE',  ( 1.184104130434999957, -78.45560097396669619, -0.5817757459379000462 ) ) ;
#8501 = CARTESIAN_POINT ( 'NONE',  ( 0.000000000000000000, -80.49999999999998579, 0.000000000000000000 ) ) ;
#8503 = CARTESIAN_POINT ( 'NONE',  ( -0.6962927961685000389, -82.36145401580000680, -1.554024870232999955 ) ) ;
#8504 = ORIENTED_EDGE ( 'NONE', *, *, #26955, .T. ) ;
#8505 = CARTESIAN_POINT ( 'NONE',  ( -1.812920252538464894, -78.78700244415333032, 11.90997463893260466 ) ) ;
#8506 = CARTESIAN_POINT ( 'NONE',  ( -6.455508761419999963, -79.33931358023599500, -10.30055883293000107 ) ) ;
#8507 = CARTESIAN_POINT ( 'NONE',  ( -8.273492252229999622, -80.01569584820420289, 7.333619062208000194 ) ) ;
#8508 = CARTESIAN_POINT ( 'NONE',  ( -14.00000000000000000, -72.39999999999999147, 0.000000000000000000 ) ) ;
#8509 = CARTESIAN_POINT ( 'NONE',  ( 11.01642476345000077, -77.09896080093798787, 2.111041454437999842 ) ) ;
#8510 = DIRECTION ( 'NONE',  ( -1.000000000000000000, 0.000000000000000000, 0.000000000000000000 ) ) ;
#8511 = CARTESIAN_POINT ( 'NONE',  ( -3.238788824226999985, -1.555722370088000073, -0.4869776969663000554 ) ) ;
#8512 = CARTESIAN_POINT ( 'NONE',  ( -3.035968726241000226, -79.60705382909299033, 9.297629541271000164 ) ) ;
#8513 = CARTESIAN_POINT ( 'NONE',  ( 12.65989858207000118, -24.94344101132999825, -0.9743214026256000748 ) ) ;
#8514 = DIRECTION ( 'NONE',  ( 0.000000000000000000, -1.000000000000000000, 0.000000000000000000 ) ) ;
#8515 = ORIENTED_EDGE ( 'NONE', *, *, #57030, .F. ) ;
#8516 = FACE_OUTER_BOUND ( 'NONE', #34455, .T. ) ;
#8517 = DIRECTION ( 'NONE',  ( 0.000000000000000000, 1.000000000000000000, 0.000000000000000000 ) ) ;
#8518 = CARTESIAN_POINT ( 'NONE',  ( 0.000000000000000000, -0.1000000063292999924, 0.000000000000000000 ) ) ;
#8519 = MECHANICAL_DESIGN_GEOMETRIC_PRESENTATION_REPRESENTATION (  '', ( #17122 ), #21834 ) ;
#8520 = CARTESIAN_POINT ( 'NONE',  ( 3.778552491321000240, -78.40681307243319509, 0.000000000000000000 ) ) ;
#8521 = CARTESIAN_POINT ( 'NONE',  ( -0.6683785725393999178, -84.35142953870898452, 3.483937815952000250 ) ) ;
#8522 = B_SPLINE_CURVE_WITH_KNOTS ( 'NONE', 3,
 ( #40925, #36197, #54215, #31156, #53621, #513, #17906, #49194, #50087, #8746, #798, #58343, #14332, #31750, #40030, #9341, #36772, #27330 ),
 .UNSPECIFIED., .F., .F.,
 ( 4, 2, 2, 2, 2, 2, 2, 2, 4 ),
 ( 0.000000000000000000, 0.1249999999999999722, 0.2500000000000000000, 0.3750000000000000000, 0.5000000000000001110, 0.6250000000000001110, 0.7500000000000000000, 0.8750000000000000000, 1.000000000000000000 ),
 .UNSPECIFIED. ) ;
#8523 = VERTEX_POINT ( 'NONE', #29845 ) ;
#8524 = AXIS2_PLACEMENT_3D ( 'NONE', #33256, #51298, #20569 ) ;
#8525 = DIRECTION ( 'NONE',  ( 0.000000000000000000, -1.000000000000000000, 0.000000000000000000 ) ) ;
#8526 = CARTESIAN_POINT ( 'NONE',  ( 8.179414027362144068, -61.54093020446555329, -9.502908391260222132 ) ) ;
#8527 = FACE_OUTER_BOUND ( 'NONE', #34502, .T. ) ;
#8528 = VERTEX_POINT ( 'NONE', #52597 ) ;
#8529 = ORIENTED_EDGE ( 'NONE', *, *, #41895, .F. ) ;
#8530 = ADVANCED_FACE ( 'NONE', ( #19855 ), #19763, .F. ) ;
#8531 = CARTESIAN_POINT ( 'NONE',  ( -12.49306752631999906, -55.51943307300000185, 1.667917367010000040 ) ) ;
#8532 = CARTESIAN_POINT ( 'NONE',  ( -7.758899961864000439, -54.49918178063000340, -10.31442855571999928 ) ) ;
#8533 = CARTESIAN_POINT ( 'NONE',  ( 1.841371367509999857, -79.97024400411599743, -9.592189096167999196 ) ) ;
#8534 = ORIENTED_EDGE ( 'NONE', *, *, #51594, .T. ) ;
#8535 = EDGE_LOOP ( 'NONE', ( #48493, #5793, #106, #38544 ) ) ;
#8536 = CARTESIAN_POINT ( 'NONE',  ( -8.953452373791000340, -77.06374045265999939, 8.338029955349002265 ) ) ;
#8537 = DIRECTION ( 'NONE',  ( 1.000000000000000000, 0.000000000000000000, 0.000000000000000000 ) ) ;
#8538 = AXIS2_PLACEMENT_3D ( 'NONE', #45799, #5334, #18917 ) ;
#8539 = CARTESIAN_POINT ( 'NONE',  ( 0.8664330213526999502, -79.10093026602000066, 1.402205237644999825 ) ) ;
#8540 = ORIENTED_EDGE ( 'NONE', *, *, #48777, .T. ) ;
#8541 = CARTESIAN_POINT ( 'NONE',  ( 10.53495272788999948, -18.77289072628000355, 7.618387390369000478 ) ) ;
#8542 = AXIS2_PLACEMENT_3D ( 'NONE', #57312, #52888, #20725 ) ;
#8543 = CARTESIAN_POINT ( 'NONE',  ( -1.407266007596761570, -79.27925411857121674, -0.5431331937064914905 ) ) ;
#8544 = CARTESIAN_POINT ( 'NONE',  ( -0.04676854649727409108, -80.22264845957727175, -1.249623885083431807 ) ) ;
#8545 = CARTESIAN_POINT ( 'NONE',  ( -3.259705057564000530, -77.47669831202999546, 12.53941704951999903 ) ) ;
#8546 = CARTESIAN_POINT ( 'NONE',  ( -10.05535668103000191, -78.21346600054846476, 4.970705447719998560 ) ) ;
#8548 = EDGE_CURVE ( 'NONE', #30955, #32917, #4131, .T. ) ;
#8547 = CARTESIAN_POINT ( 'NONE',  ( -13.13047446164998711, -19.21421830981000767, -0.8260994316375004365 ) ) ;
#8549 = CARTESIAN_POINT ( 'NONE',  ( -2.705739474708485748, -86.31452044230000809, 3.652324231546889788 ) ) ;
#8550 = CARTESIAN_POINT ( 'NONE',  ( 11.15679540746000065, -79.65992229053399853, 1.159321710118000004 ) ) ;
#8551 = LINE ( 'NONE', #11835, #41220 ) ;
#8552 = DIRECTION ( 'NONE',  ( 0.7071067811865474617, 0.000000000000000000, 0.7071067811865474617 ) ) ;
#8553 = ORIENTED_EDGE ( 'NONE', *, *, #15749, .T. ) ;
#8554 = CARTESIAN_POINT ( 'NONE',  ( 0.1325202778310999863, -79.49487755444098980, 11.26549478459000042 ) ) ;
#8555 = CARTESIAN_POINT ( 'NONE',  ( -1.771468677314999907, -75.90382483601000274, 12.18184739844999953 ) ) ;
#8556 = CARTESIAN_POINT ( 'NONE',  ( 0.7212099693301999848, -80.68823808787499274, 1.333715969168000059 ) ) ;
#8557 = CARTESIAN_POINT ( 'NONE',  ( -0.9509180703096998810, -78.71900440081799388, -0.9145055679095001056 ) ) ;
#8558 = CARTESIAN_POINT ( 'NONE',  ( -1.263607411038969008, -2.945081867600211734, -3.286951345324313767 ) ) ;
#8559 = CARTESIAN_POINT ( 'NONE',  ( -8.792808668242045655, -16.77303577624769559, 9.175550543643495871 ) ) ;
#8560 = EDGE_CURVE ( 'NONE', #52300, #20296, #49210, .T. ) ;
#8561 = CYLINDRICAL_SURFACE ( 'NONE', #35708, 1.250000000000000000 ) ;
#8562 = DIRECTION ( 'NONE',  ( -4.860927510790000040E-11, -1.000000000000000000, -3.762819604792999951E-10 ) ) ;
#8563 = CARTESIAN_POINT ( 'NONE',  ( -9.975891578018998729, -79.09389356166599327, -4.997317968730000004 ) ) ;
#8564 = CARTESIAN_POINT ( 'NONE',  ( 3.967828918824999995, -77.10191332859899660, -8.773065546720999919 ) ) ;
#8565 = FACE_OUTER_BOUND ( 'NONE', #48626, .T. ) ;
#8566 = CARTESIAN_POINT ( 'NONE',  ( -3.970056213021999625, -79.05176450532758281, 11.35542513096999961 ) ) ;
#8567 = CARTESIAN_POINT ( 'NONE',  ( 10.75000000000000000, -77.75000000000000000, 0.000000000000000000 ) ) ;
#8568 = ADVANCED_FACE ( 'NONE', ( #33413 ), #43430, .F. ) ;
#8569 = CARTESIAN_POINT ( 'NONE',  ( 10.75000000000000000, -77.75000000000000000, 0.000000000000000000 ) ) ;
#8570 = TOROIDAL_SURFACE ( 'NONE', #13283, 12.50000000000000000, 1.500000000000000000 ) ;
#8571 = ORIENTED_EDGE ( 'NONE', *, *, #14100, .F. ) ;
#8572 = B_SPLINE_CURVE_WITH_KNOTS ( 'NONE', 3,
 ( #3924, #45267, #31063, #39934, #17505, #44671, #35495, #53525, #8651, #27811 ),
 .UNSPECIFIED., .F., .F.,
 ( 4, 2, 2, 2, 4 ),
 ( 0.000000000000000000, 0.2500000000000000000, 0.5000000000000000000, 0.7500000000000000000, 1.000000000000000000 ),
 .UNSPECIFIED. ) ;
#8573 = CARTESIAN_POINT ( 'NONE',  ( -0.6675286376147999690, -83.36920712346199025, 1.308112063971999861 ) ) ;
#8574 = DIRECTION ( 'NONE',  ( -0.7026410690473250398, -0.1122098755728047209, 0.7026410690473250398 ) ) ;
#8575 = CARTESIAN_POINT ( 'NONE',  ( -10.74991650949179345, -79.10538127169735390, -0.7036244177452357640 ) ) ;
#8576 = LINE ( 'NONE', #22149, #33339 ) ;
#8577 = CARTESIAN_POINT ( 'NONE',  ( 7.990874060778157428, -76.99999999999998579, 4.858782514301908328 ) ) ;
#8578 = CARTESIAN_POINT ( 'NONE',  ( -0.7572724432162000197, -83.12372429327399459, 1.483977110291999857 ) ) ;
#8579 = CARTESIAN_POINT ( 'NONE',  ( -1.355082891136000001, -77.69253568003099986, -11.85745557885999979 ) ) ;
#8580 = CARTESIAN_POINT ( 'NONE',  ( -0.6471704932797999188, -77.89014415034598926, 9.701898969124000516 ) ) ;
#8581 = CARTESIAN_POINT ( 'NONE',  ( -2.062323307449999810, -55.57286846775000555, -12.83634826441000065 ) ) ;
#8582 = CARTESIAN_POINT ( 'NONE',  ( 11.64020011326665660, -75.96092683841732196, 1.623265142550421203 ) ) ;
#8583 = CARTESIAN_POINT ( 'NONE',  ( 3.654181830570427003, -86.09999999999999432, -1.626946572303645366 ) ) ;
#8584 = VERTEX_POINT ( 'NONE', #22451 ) ;
#8585 = DIRECTION ( 'NONE',  ( -1.000000000000000000, 0.000000000000000000, 0.000000000000000000 ) ) ;
#8586 = FACE_OUTER_BOUND ( 'NONE', #16509, .T. ) ;
#8587 = CARTESIAN_POINT ( 'NONE',  ( -0.03284986460708162054, -78.48547957940618858, -3.485344413137181352 ) ) ;
#8588 = CARTESIAN_POINT ( 'NONE',  ( -1.508789225394999933, -82.29476871435998930, 0.7062677124845000431 ) ) ;
#8589 = AXIS2_PLACEMENT_3D ( 'NONE', #10091, #5935, #9206 ) ;
#8590 = CARTESIAN_POINT ( 'NONE',  ( 7.788493169598000421, -78.74236831944799064, 7.733265204867000087 ) ) ;
#8591 = CARTESIAN_POINT ( 'NONE',  ( 1.931736162947209179, -18.23329604289370209, 12.72978979890546292 ) ) ;
#8592 = EDGE_CURVE ( 'NONE', #26124, #23569, #39296, .T. ) ;
#8593 = CARTESIAN_POINT ( 'NONE',  ( 3.305503757990000402, -77.08763120859698859, -11.93766403289999900 ) ) ;
#8594 = CARTESIAN_POINT ( 'NONE',  ( 2.069888253764102792, -78.55744420716430909, 11.57512296172573052 ) ) ;
#8595 = CARTESIAN_POINT ( 'NONE',  ( 1.277523036634464537, -77.92187500009777068, 0.4181665473888493412 ) ) ;
#8596 = ORIENTED_EDGE ( 'NONE', *, *, #30941, .F. ) ;
#8597 = AXIS2_PLACEMENT_3D ( 'NONE', #14048, #17604, #32042 ) ;
#8598 = CARTESIAN_POINT ( 'NONE',  ( 0.9420327262254000189, -78.77294003937198852, -10.99155624668999920 ) ) ;
#8599 = CARTESIAN_POINT ( 'NONE',  ( 0.7287571107289755323, -79.92570316464997404, 1.016895782456411323 ) ) ;
#8600 = CYLINDRICAL_SURFACE ( 'NONE', #22591, 1.250000000000000000 ) ;
#8601 = DIRECTION ( 'NONE',  ( 0.000000000000000000, 0.000000000000000000, -1.000000000000000000 ) ) ;
#8602 = CARTESIAN_POINT ( 'NONE',  ( 3.980415848809999879, -79.08903371854199804, 10.42342982551999953 ) ) ;
#8603 = CARTESIAN_POINT ( 'NONE',  ( 12.50386483995752052, -61.58505343581200719, -0.8574420495986169177 ) ) ;
#8604 = CARTESIAN_POINT ( 'NONE',  ( -10.99607952893977370, -23.68503250286043027, 0.3139933498860824068 ) ) ;
#8605 = B_SPLINE_CURVE_WITH_KNOTS ( 'NONE', 3,
 ( #12534, #33591, #30240, #17249, #20036, #21679, #48564, #43550, #28868, #25821, #38024, #8108, #51629, #29946, #35237, #3395, #43850, #7533, #3115, #57119, #34668, #53269 ),
 .UNSPECIFIED., .F., .F.,
 ( 4, 2, 2, 2, 2, 2, 2, 2, 2, 2, 4 ),
 ( 0.000000000000000000, 0.1250000000000001665, 0.2500000000000003331, 0.3125000000000002776, 0.3750000000000002776, 0.4375000000000002220, 0.5000000000000002220, 0.6250000000000001110, 0.7500000000000001110, 0.8750000000000000000, 1.000000000000000000 ),
 .UNSPECIFIED. ) ;
#8606 = CARTESIAN_POINT ( 'NONE',  ( 6.606416481926000728, -77.99679431087899673, -10.35137867379999932 ) ) ;
#8607 = ORIENTED_EDGE ( 'NONE', *, *, #3416, .T. ) ;
#8608 = CARTESIAN_POINT ( 'NONE',  ( 1.500000000000000888, -81.23958333333332860, -0.1963495408493590444 ) ) ;
#8609 = CARTESIAN_POINT ( 'NONE',  ( -10.47020627418440242, -79.47916666666667140, 2.813789756862221214 ) ) ;
#8610 = CARTESIAN_POINT ( 'NONE',  ( -12.71536556660682926, -60.92544729011922300, -1.781281569003885679 ) ) ;
#8611 = CARTESIAN_POINT ( 'NONE',  ( -12.77651065749000026, -25.30896598096000005, -0.04308629978602999955 ) ) ;
#8612 = ORIENTED_EDGE ( 'NONE', *, *, #41158, .T. ) ;
#8613 = VERTEX_POINT ( 'NONE', #44306 ) ;
#8614 = CIRCLE ( 'NONE', #47293, 1.250000000000000444 ) ;
#8615 = CARTESIAN_POINT ( 'NONE',  ( 4.100000000000000533, -78.69999999999998863, 0.000000000000000000 ) ) ;
#8616 = VERTEX_POINT ( 'NONE', #44601 ) ;
#8617 = CARTESIAN_POINT ( 'NONE',  ( -10.61911868076999887, -78.59368720767999150, -6.134606423928000041 ) ) ;
#8618 = ORIENTED_EDGE ( 'NONE', *, *, #8716, .F. ) ;
#8619 = CARTESIAN_POINT ( 'NONE',  ( 7.646092217281999837, -23.70851177913000285, 10.13691708057999996 ) ) ;
#8620 = CARTESIAN_POINT ( 'NONE',  ( -10.75275020201999965, -78.15907477017699989, -2.465785609032999925 ) ) ;
#8622 = EDGE_CURVE ( 'NONE', #53336, #43546, #35813, .T. ) ;
#8621 = CARTESIAN_POINT ( 'NONE',  ( 7.981661899572999985, -77.98631332859899601, 4.815606314103999530 ) ) ;
#8623 = CARTESIAN_POINT ( 'NONE',  ( -12.50657368821661208, -24.97245458995920586, -0.3553454087125454408 ) ) ;
#8624 = CARTESIAN_POINT ( 'NONE',  ( 2.039250879084999912, -79.90565398600709557, -11.02993955029000084 ) ) ;
#8625 = CARTESIAN_POINT ( 'NONE',  ( 1.139330238168773324, -79.38420227355845782, 0.5135602714818040537 ) ) ;
#8626 = ORIENTED_EDGE ( 'NONE', *, *, #50416, .T. ) ;
#8628 = ORIENTED_EDGE ( 'NONE', *, *, #41760, .T. ) ;
#8627 = EDGE_CURVE ( 'NONE', #8467, #14636, #2294, .T. ) ;
#8629 = CARTESIAN_POINT ( 'NONE',  ( -0.003491213567336264294, -77.47518361382161345, 9.249907303942231707 ) ) ;
#8630 = CARTESIAN_POINT ( 'NONE',  ( -9.177034484502000211, -77.32294129249000036, 6.137278520473000043 ) ) ;
#8631 = CARTESIAN_POINT ( 'NONE',  ( 9.252740428349001789, -77.62916666666666288, -2.486604901413144830 ) ) ;
#8632 = AXIS2_PLACEMENT_3D ( 'NONE', #49205, #53936, #17916 ) ;
#8633 = CARTESIAN_POINT ( 'NONE',  ( -6.473047519705999342, -78.32356397331999176, 7.229824698717000508 ) ) ;
#8634 = CARTESIAN_POINT ( 'NONE',  ( -13.11938987471999951, -76.50757595554999568, -0.3223533933333999624 ) ) ;
#8635 = CARTESIAN_POINT ( 'NONE',  ( -9.023370604008427165, -79.42502604630486474, -2.970777336590622930 ) ) ;
#8636 = CARTESIAN_POINT ( 'NONE',  ( 12.85140862673999784, -58.55560170131000319, 1.980464483675000054 ) ) ;
#8637 = CARTESIAN_POINT ( 'NONE',  ( 10.52776997023000050, -80.26921465513198939, 3.979665013433000720 ) ) ;
#8638 = LINE ( 'NONE', #25777, #25028 ) ;
#8639 = FACE_OUTER_BOUND ( 'NONE', #56775, .T. ) ;
#8640 = B_SPLINE_CURVE_WITH_KNOTS ( 'NONE', 3,
 ( #2292, #47750, #43304, #2860, #56014, #51595, #29127, #16438, #2574, #11436, #42142, #56882, #34421, #20287, #29417, #12008, #52450, #46880 ),
 .UNSPECIFIED., .F., .F.,
 ( 4, 2, 2, 2, 2, 2, 2, 2, 4 ),
 ( 0.000000000000000000, 0.1250000000000000000, 0.2500000000000000000, 0.3750000000000000000, 0.5000000000000000000, 0.6250000000000000000, 0.7500000000000000000, 0.8750000000000000000, 1.000000000000000000 ),
 .UNSPECIFIED. ) ;
#8641 = EDGE_CURVE ( 'NONE', #38246, #19156, #10564, .T. ) ;
#8642 = CARTESIAN_POINT ( 'NONE',  ( -9.250000000000001776, -78.51041666666667140, -1.210822168571065616 ) ) ;
#8643 = ORIENTED_EDGE ( 'NONE', *, *, #54821, .F. ) ;
#8644 = CARTESIAN_POINT ( 'NONE',  ( -12.41539209960999912, -79.37769575988599513, -0.6693894873470999096 ) ) ;
#8645 = CARTESIAN_POINT ( 'NONE',  ( -8.643969996042999426, -53.54046576124999746, 9.422817222679000793 ) ) ;
#8646 = CARTESIAN_POINT ( 'NONE',  ( -7.560044382379633277, -78.03705853110491830, 7.642724606814406130 ) ) ;
#8647 = CARTESIAN_POINT ( 'NONE',  ( 0.4844284812283000119, -77.57346407451200321, 11.97002061314999999 ) ) ;
#8648 = CARTESIAN_POINT ( 'NONE',  ( -8.260145278149000347, -17.05964900975000020, -9.643338479001000607 ) ) ;
#8650 = CARTESIAN_POINT ( 'NONE',  ( -1.632307027708999936, -18.33072810443000122, -12.46200249212000166 ) ) ;
#8649 = CARTESIAN_POINT ( 'NONE',  ( -4.658533681657620384, -78.51668711297222103, 8.082509443235778690 ) ) ;
#8651 = CARTESIAN_POINT ( 'NONE',  ( 0.8338927956426691601, -53.99946422210107499, 12.50366901599831060 ) ) ;
#8652 = CARTESIAN_POINT ( 'NONE',  ( -9.013126759186999237, -80.17326805110798205, -6.983032781201999661 ) ) ;
#8653 = CARTESIAN_POINT ( 'NONE',  ( 0.000000000000000000, 0.000000000000000000, 0.000000000000000000 ) ) ;
#8654 = CARTESIAN_POINT ( 'NONE',  ( 5.284336329618000150, -77.98727524673999767, -9.945338310677000138 ) ) ;
#8655 = CARTESIAN_POINT ( 'NONE',  ( -11.44999999995999929, -74.99999999996167332, -1.667681223830999978E-09 ) ) ;
#8656 = CARTESIAN_POINT ( 'NONE',  ( -10.71369944335148361, -80.17916666669142955, 2.879226727952040044 ) ) ;
#8657 = EDGE_LOOP ( 'NONE', ( #48517, #17412, #3410, #29533 ) ) ;
#8658 = CARTESIAN_POINT ( 'NONE',  ( -0.4268555006395731710, -1.487093160906469036, 3.249579827604153870 ) ) ;
#8659 = CARTESIAN_POINT ( 'NONE',  ( 0.005119011380280999966, -53.86186137778000216, 12.43705489340000092 ) ) ;
#8660 = CARTESIAN_POINT ( 'NONE',  ( -12.71798280855999863, -23.29778595484999926, 1.931086388455000025 ) ) ;
#8661 = CARTESIAN_POINT ( 'NONE',  ( -1.440490910816999870, -2.210199159476000208, 3.695416286417999796 ) ) ;
#8662 = CARTESIAN_POINT ( 'NONE',  ( 3.299939911277999460, -79.86734754465000208, 8.828171983641000864 ) ) ;
#8663 = CARTESIAN_POINT ( 'NONE',  ( -1.374053708643000007E-14, -74.80000000000001137, 0.000000000000000000 ) ) ;
#8664 = DIRECTION ( 'NONE',  ( 0.000000000000000000, -1.000000000000000000, 0.000000000000000000 ) ) ;
#8665 = ADVANCED_FACE ( 'NONE', ( #51597, #55727 ), #51306, .T. ) ;
#8666 = CARTESIAN_POINT ( 'NONE',  ( -1.056237665594999875, -61.84866013665000395, 12.77256098201999990 ) ) ;
#8667 = CARTESIAN_POINT ( 'NONE',  ( 12.66314509270999977, -16.82135249322999826, -0.04032083120557000688 ) ) ;
#8668 = CARTESIAN_POINT ( 'NONE',  ( -3.886511739433000212, -84.66724735065199070, 1.524672515453000088 ) ) ;
#8669 = CYLINDRICAL_SURFACE ( 'NONE', #16948, 0.5000000000000006661 ) ;
#8670 = CARTESIAN_POINT ( 'NONE',  ( 10.81498442169830909, -77.23901691334977215, 5.255458039015602267 ) ) ;
#8671 = CARTESIAN_POINT ( 'NONE',  ( -10.56602462368999973, -78.44534377886000698, 7.483748555556999804 ) ) ;
#8672 = CARTESIAN_POINT ( 'NONE',  ( -10.58739904582000158, -77.80427472496999997, -3.839393962977000196 ) ) ;
#8673 = CARTESIAN_POINT ( 'NONE',  ( 0.4455676568320503517, -81.94613279277081119, 1.167930216820072920 ) ) ;
#8674 = CARTESIAN_POINT ( 'NONE',  ( -0.1648886907344999930, -77.77763659747000702, 1.456783013396000248 ) ) ;
#8675 = CARTESIAN_POINT ( 'NONE',  ( 9.670530767802999250, -77.07877401326959443, -0.1674091926992999912 ) ) ;
#8676 = CARTESIAN_POINT ( 'NONE',  ( 12.50745077490000057, -24.99994448286999926, 2.662071812989000278E-09 ) ) ;
#8677 = AXIS2_PLACEMENT_3D ( 'NONE', #25196, #57073, #57362 ) ;
#8678 = CARTESIAN_POINT ( 'NONE',  ( -12.77656765298000074, -62.11198129881000085, 0.1555235816857000186 ) ) ;
#8679 = CARTESIAN_POINT ( 'NONE',  ( 4.117763575831188128, -80.25636342326222916, -9.930021758596684123 ) ) ;
#8680 = ADVANCED_FACE ( 'NONE', ( #28547 ), #53341, .F. ) ;
#8681 = CARTESIAN_POINT ( 'NONE',  ( -12.55433072264035843, -23.38725213725906471, -1.749897784985361637 ) ) ;
#8682 = CARTESIAN_POINT ( 'NONE',  ( 0.7503693421468168312, -77.82491630038197172, -1.029957698447139913 ) ) ;
#8683 = CARTESIAN_POINT ( 'NONE',  ( 9.546815223802999739, -54.11472046612000497, 8.130854305859999798 ) ) ;
#8684 = CARTESIAN_POINT ( 'NONE',  ( 11.00000000000000711, -79.36041666666665151, 1.439896632895290240 ) ) ;
#8685 = CARTESIAN_POINT ( 'NONE',  ( 3.485296502184999756, -79.24083078338598796, 10.58807389768000107 ) ) ;
#8686 = CYLINDRICAL_SURFACE ( 'NONE', #33710, 2.500000000000000000 ) ;
#8687 = ORIENTED_EDGE ( 'NONE', *, *, #7202, .F. ) ;
#8688 = VERTEX_POINT ( 'NONE', #3157 ) ;
#8689 = LINE ( 'NONE', #49739, #2339 ) ;
#8690 = ORIENTED_EDGE ( 'NONE', *, *, #21945, .F. ) ;
#8691 = DIRECTION ( 'NONE',  ( -1.000000000000000000, 0.000000000000000000, 0.000000000000000000 ) ) ;
#8692 = ORIENTED_EDGE ( 'NONE', *, *, #33961, .F. ) ;
#8693 = VECTOR ( 'NONE', #29369, 1000.000000000000000 ) ;
#8694 = CARTESIAN_POINT ( 'NONE',  ( -7.179058446791997561, -79.91995496524606324, -8.667882172381000672 ) ) ;
#8695 = LINE ( 'NONE', #49746, #54176 ) ;
#8696 = CARTESIAN_POINT ( 'NONE',  ( -2.665716224216999830, -79.53555764342200973, 10.70493771085999946 ) ) ;
#8698 = ADVANCED_FACE ( 'NONE', ( #52740 ), #57453, .T. ) ;
#8697 = CARTESIAN_POINT ( 'NONE',  ( 3.140974612311377090, -76.44583333331208053, -11.68767212001978528 ) ) ;
#8699 = CARTESIAN_POINT ( 'NONE',  ( -3.429316649911000159, -78.93070212325169166, 1.098603813411000107 ) ) ;
#8700 = CARTESIAN_POINT ( 'NONE',  ( -1.506252837058942529, -79.28748717942596613, 9.379723702719340750 ) ) ;
#8701 = ORIENTED_EDGE ( 'NONE', *, *, #51494, .F. ) ;
#8702 = CARTESIAN_POINT ( 'NONE',  ( 10.65102452230999930, -77.62119051562517313, 2.905137941167998950 ) ) ;
#8703 = CARTESIAN_POINT ( 'NONE',  ( -11.33685376752999829, -78.94881983984001295, -4.534688555742999228 ) ) ;
#8704 = VERTEX_POINT ( 'NONE', #17013 ) ;
#8706 = ORIENTED_EDGE ( 'NONE', *, *, #25996, .T. ) ;
#8705 = EDGE_CURVE ( 'NONE', #50911, #28385, #16812, .T. ) ;
#8707 = CYLINDRICAL_SURFACE ( 'NONE', #20700, 0.5000000000000004441 ) ;
#8708 = LINE ( 'NONE', #53582, #8412 ) ;
#8709 = CARTESIAN_POINT ( 'NONE',  ( -1.308081345731999967, -80.75005114052200383, 0.2599445073669000017 ) ) ;
#8710 = CARTESIAN_POINT ( 'NONE',  ( -5.351292223237999579, -77.63102627198600203, 8.095330809056001442 ) ) ;
#8711 = CARTESIAN_POINT ( 'NONE',  ( 0.000000000000000000, 0.000000000000000000, 0.000000000000000000 ) ) ;
#8712 = CARTESIAN_POINT ( 'NONE',  ( 2.137738514688780178, -85.88386088149393061, 2.761283067625453835 ) ) ;
#8713 = CARTESIAN_POINT ( 'NONE',  ( -11.86979166781643968, -79.11979166670496966, 1.243547081883744188 ) ) ;
#8714 = CARTESIAN_POINT ( 'NONE',  ( 7.079708506942000490, -77.91668243576999942, -10.47296538612000028 ) ) ;
#8715 = CARTESIAN_POINT ( 'NONE',  ( -10.90118402791000030, -76.46949373684098816, -1.464937909874000077 ) ) ;
#8716 = EDGE_CURVE ( 'NONE', #28402, #4126, #52453, .T. ) ;
#8717 = DIRECTION ( 'NONE',  ( 0.000000000000000000, -1.000000000000000000, 0.000000000000000000 ) ) ;
#8718 = CARTESIAN_POINT ( 'NONE',  ( -4.126002678693000192, -80.37756669824999278, 0.1860526405827999941 ) ) ;
#8719 = FACE_OUTER_BOUND ( 'NONE', #47836, .T. ) ;
#8720 = CARTESIAN_POINT ( 'NONE',  ( -4.310712596281979891, -76.79473241825421326, -11.00476471888044827 ) ) ;
#8721 = CARTESIAN_POINT ( 'NONE',  ( -3.541116149846999850, -80.13275264934799225, 0.1595625314431999842 ) ) ;
#8722 = DIRECTION ( 'NONE',  ( -0.9135454576429105078, 0.000000000000000000, 0.4067366430751048201 ) ) ;
#8723 = CARTESIAN_POINT ( 'NONE',  ( -2.055177818477693652, -80.99049588671762478, 10.56044713659669654 ) ) ;
#8724 = CARTESIAN_POINT ( 'NONE',  ( -11.09105850093000001, -80.31987609346899148, 1.974238845993000258 ) ) ;
#8725 = CARTESIAN_POINT ( 'NONE',  ( 3.171758640500000226, -3.567406026038999922, 1.479846994257000059 ) ) ;
#8726 = CARTESIAN_POINT ( 'NONE',  ( 1.046486999526615502, -79.45165172675351073, -0.7277384538878118869 ) ) ;
#8727 = EDGE_LOOP ( 'NONE', ( #26003, #36730, #31571, #43402 ) ) ;
#8728 = CARTESIAN_POINT ( 'NONE',  ( -0.3135214471687461368, -23.68581381185224544, 10.99610567419509977 ) ) ;
#8729 = AXIS2_PLACEMENT_3D ( 'NONE', #29528, #20688, #21256 ) ;
#8730 = CARTESIAN_POINT ( 'NONE',  ( 0.000000000000000000, -75.15999999999999659, 0.000000000000000000 ) ) ;
#8731 = CARTESIAN_POINT ( 'NONE',  ( 1.316231252753000014, -81.94098224633900429, 0.2147359707272000207 ) ) ;
#8732 = CARTESIAN_POINT ( 'NONE',  ( -12.43640296266999989, -17.08252466130999991, 0.05222744260230000046 ) ) ;
#8733 = CARTESIAN_POINT ( 'NONE',  ( -9.339950055924999717, -78.04396109509998780, -9.061158367717998985 ) ) ;
#8734 = VECTOR ( 'NONE', #27908, 1000.000000000000000 ) ;
#8735 = CARTESIAN_POINT ( 'NONE',  ( 5.689140600256999747, -79.33158667140099851, 7.768672748409000128 ) ) ;
#8736 = CARTESIAN_POINT ( 'NONE',  ( 12.58335110166999904, -20.25111654322000021, -1.667961430005999945 ) ) ;
#8737 = EDGE_LOOP ( 'NONE', ( #1444, #8168 ) ) ;
#8738 = AXIS2_PLACEMENT_3D ( 'NONE', #3495, #3217, #20353 ) ;
#8739 = CARTESIAN_POINT ( 'NONE',  ( -8.251802458333543200, -24.80055625133827846, -9.431055090843393884 ) ) ;
#8740 = CARTESIAN_POINT ( 'NONE',  ( -2.858407197967999913, -77.19999999999998863, -8.797272775729998884 ) ) ;
#8741 = CARTESIAN_POINT ( 'NONE',  ( -1.372219269624000093, -82.27922771258300827, 0.3172897272240999822 ) ) ;
#8742 = CARTESIAN_POINT ( 'NONE',  ( 7.612971414716000140, -18.67547470641000018, -10.53003223724000037 ) ) ;
#8743 = CARTESIAN_POINT ( 'NONE',  ( 9.403616370364000332, -78.21950448043199344, 1.497456306884999977 ) ) ;
#8745 = CARTESIAN_POINT ( 'NONE',  ( -3.754890333716000228, -1.311529764407000087, -1.424957469106999941 ) ) ;
#8744 = CARTESIAN_POINT ( 'NONE',  ( 4.040457884044000636, -83.83275779226799784, -1.050861572499000030 ) ) ;
#8746 = CARTESIAN_POINT ( 'NONE',  ( 0.1636246173744642929, -82.36458333333334281, 1.250000000000000888 ) ) ;
#8747 = CARTESIAN_POINT ( 'NONE',  ( 0.3023484132065000218, -79.68828967281199027, -1.485775080250999913 ) ) ;
#8748 = ORIENTED_EDGE ( 'NONE', *, *, #22352, .F. ) ;
#8749 = ADVANCED_FACE ( 'NONE', ( #12578 ), #4336, .F. ) ;
#8750 = CARTESIAN_POINT ( 'NONE',  ( -4.886687280655466203, -77.18749172000538294, -9.575324941435306769 ) ) ;
#8751 = CARTESIAN_POINT ( 'NONE',  ( -1.460959015002473826, -78.92083333333336270, -0.3926218265389207485 ) ) ;
#8752 = CARTESIAN_POINT ( 'NONE',  ( 0.8695890703638051722, -78.91427086690823955, -3.811935123611656984 ) ) ;
#8753 = ORIENTED_EDGE ( 'NONE', *, *, #5454, .F. ) ;
#8754 = VERTEX_POINT ( 'NONE', #37344 ) ;
#8755 = FACE_OUTER_BOUND ( 'NONE', #52488, .T. ) ;
#8756 = DIRECTION ( 'NONE',  ( 0.000000000000000000, -1.000000000000000000, 0.000000000000000000 ) ) ;
#8757 = DIRECTION ( 'NONE',  ( 7.074021373685000131E-10, -1.000000000000000000, 4.749368372333999376E-10 ) ) ;
#8758 = EDGE_LOOP ( 'NONE', ( #17300, #15234, #55091 ) ) ;
#8759 = CARTESIAN_POINT ( 'NONE',  ( -10.02269271100999859, -77.64430565866300071, 6.688901441487999477 ) ) ;
#8760 = ORIENTED_EDGE ( 'NONE', *, *, #54521, .F. ) ;
#8761 = ORIENTED_EDGE ( 'NONE', *, *, #35602, .F. ) ;
#8762 = CARTESIAN_POINT ( 'NONE',  ( 7.429974109838866525, -60.31614597266855782, 8.111636311564803137 ) ) ;
#8763 = AXIS2_PLACEMENT_3D ( 'NONE', #15891, #5071, #41081 ) ;
#8764 = CARTESIAN_POINT ( 'NONE',  ( 7.374239324226436132, -76.57642972729847486, -9.595271688162245738 ) ) ;
#8765 = CARTESIAN_POINT ( 'NONE',  ( -0.4621935165842904203, -1.232020812799707432, 3.993632164156191600 ) ) ;
#8766 = EDGE_LOOP ( 'NONE', ( #30651, #28507, #30661, #54947 ) ) ;
#8767 = CARTESIAN_POINT ( 'NONE',  ( 0.8928155417757041024, -82.04817708000638277, -1.160372106499861333 ) ) ;
#8769 = EDGE_CURVE ( 'NONE', #11225, #6077, #47940, .T. ) ;
#8768 = ORIENTED_EDGE ( 'NONE', *, *, #2161, .F. ) ;
#8770 = CARTESIAN_POINT ( 'NONE',  ( -1.236716109016945175, -79.66948819531968695, -0.3055935817348646166 ) ) ;
#8771 = CARTESIAN_POINT ( 'NONE',  ( -11.76955644394622880, -79.80000000000001137, -2.210969502171932888 ) ) ;
#8772 = CARTESIAN_POINT ( 'NONE',  ( 10.01752115540999988, -55.60828330164999755, 7.660412752583999563 ) ) ;
#8773 = CARTESIAN_POINT ( 'NONE',  ( -7.653559626094000201, -18.70151115557999688, -10.01235002622999914 ) ) ;
#8774 = CARTESIAN_POINT ( 'NONE',  ( 9.462239583424770117, -79.53776041666264973, 1.239456475944461955 ) ) ;
#8775 = AXIS2_PLACEMENT_3D ( 'NONE', #7586, #2873, #42159 ) ;
#8776 = CARTESIAN_POINT ( 'NONE',  ( 13.86363636363000218, -46.43897132165000130, 1.277887489249999988E-05 ) ) ;
#8777 = CARTESIAN_POINT ( 'NONE',  ( 2.228685126279000173, -78.01010929892113666, 11.77068507109000350 ) ) ;
#8778 = EDGE_CURVE ( 'NONE', #8841, #56133, #33610, .T. ) ;
#8779 = FACE_OUTER_BOUND ( 'NONE', #32211, .T. ) ;
#8780 = CARTESIAN_POINT ( 'NONE',  ( -9.395758989562999375, -24.70491532583000449, 8.188252216825999241 ) ) ;
#8781 = EDGE_CURVE ( 'NONE', #39540, #3332, #1943, .T. ) ;
#8782 = CARTESIAN_POINT ( 'NONE',  ( 5.684625949311768345, -77.77723352849264415, -7.397146152607679603 ) ) ;
#8783 = CARTESIAN_POINT ( 'NONE',  ( 2.485654608723999903, -79.17075264934788947, -3.354268632559000096 ) ) ;
#8784 = CARTESIAN_POINT ( 'NONE',  ( 5.016617212972000139, -78.02337999526599788, 7.984403404948999139 ) ) ;
#8785 = CARTESIAN_POINT ( 'NONE',  ( -1.217465845835396188, -83.47916666666668561, 0.3271848554490955907 ) ) ;
#8786 = CARTESIAN_POINT ( 'NONE',  ( -9.611650271896857944, -78.05833333333333712, 5.539808784079855997 ) ) ;
#8787 = CARTESIAN_POINT ( 'NONE',  ( 1.758095523367999791, -23.72291663880000101, 12.57362173515999970 ) ) ;
#8788 = CARTESIAN_POINT ( 'NONE',  ( 4.054145691792255590, -79.94511357774049998, 10.29526509435834214 ) ) ;
#8789 = DIRECTION ( 'NONE',  ( 0.7071067811865475727, 0.000000000000000000, 0.7071067811865475727 ) ) ;
#8790 = CARTESIAN_POINT ( 'NONE',  ( -3.114032450773999816, -1.916752247163000078, -1.479365640781999947 ) ) ;
#8791 = CARTESIAN_POINT ( 'NONE',  ( -0.9027627336519593593, -82.16588911174736154, -1.005952998842721158 ) ) ;
#8792 = CARTESIAN_POINT ( 'NONE',  ( -0.1058354079650530299, -79.96871532614137834, -1.507746398707539681 ) ) ;
#8793 = CARTESIAN_POINT ( 'NONE',  ( -1.466115278491000096, -78.37365292024510666, 0.6765500100044000709 ) ) ;
#8794 = CARTESIAN_POINT ( 'NONE',  ( -1.980584515752000119, -18.73514853375999678, -12.76303204602000108 ) ) ;
#8795 = CARTESIAN_POINT ( 'NONE',  ( 0.1355484243949000023, -77.40060249292598371, 10.91590548763000079 ) ) ;
#8796 = PRODUCT ( 'Security screw', 'Security screw', '', ( #32861 ) ) ;
#8797 = CARTESIAN_POINT ( 'NONE',  ( -12.15819904699000098, -78.38462189577700201, -1.724521706148000044 ) ) ;
#8798 = CARTESIAN_POINT ( 'NONE',  ( 1.460959015002472494, -80.77083333333334281, 0.3926218265389233020 ) ) ;
#8799 = EDGE_CURVE ( 'NONE', #46040, #42021, #30769, .T. ) ;
#8801 = CARTESIAN_POINT ( 'NONE',  ( -0.2736340887363999941, -78.96324533647100452, -1.491330460909999989 ) ) ;
#8800 = CARTESIAN_POINT ( 'NONE',  ( -11.75000000000000000, -76.70000000000000284, 1.487410190129999909E-14 ) ) ;
#8802 = CARTESIAN_POINT ( 'NONE',  ( -1.631971144587999856, -81.79302107981000347, -0.4862994432698999892 ) ) ;
#8803 = ORIENTED_EDGE ( 'NONE', *, *, #34070, .T. ) ;
#8804 = CARTESIAN_POINT ( 'NONE',  ( 2.741068799628999741, -84.43446544543100174, 2.568638535162999670 ) ) ;
#8805 = VECTOR ( 'NONE', #39272, 1000.000000000000000 ) ;
#8806 = CARTESIAN_POINT ( 'NONE',  ( 8.107625576107000853, -78.93752314293499239, 8.443305427288999354 ) ) ;
#8807 = CARTESIAN_POINT ( 'NONE',  ( 10.49124522239000079, -80.36320440064619675, -3.841552970220999619 ) ) ;
#8808 = CARTESIAN_POINT ( 'NONE',  ( -8.942878731355392574, -80.00000000000000000, -2.529715217048958742 ) ) ;
#8809 = CARTESIAN_POINT ( 'NONE',  ( 2.329613959545419277, -85.25208334169079194, -2.535327851541462785 ) ) ;
#8810 = CARTESIAN_POINT ( 'NONE',  ( 2.976864594307000011, -77.48026960296300558, -10.81463766284999828 ) ) ;
#8811 = CARTESIAN_POINT ( 'NONE',  ( 10.71369944335146762, -78.87083333333333712, 2.879226727952103548 ) ) ;
#8812 = CARTESIAN_POINT ( 'NONE',  ( -7.484045594489000308, -78.77392489796099539, 6.232877124219999843 ) ) ;
#8813 = CARTESIAN_POINT ( 'NONE',  ( 3.901255009783000105, -1.575525618456000032, 0.9967003545521999630 ) ) ;
#8814 = CARTESIAN_POINT ( 'NONE',  ( 13.86301033151605289, -9.638971321655001034, 0.1317488955328472711 ) ) ;
#8815 = CARTESIAN_POINT ( 'NONE',  ( 12.77306367228999839, -25.05881314456000197, -1.040970605966999862 ) ) ;
#8816 = CARTESIAN_POINT ( 'NONE',  ( -1.667961445601999992, -57.05199022587000002, 12.58338334673999981 ) ) ;
#8817 = VERTEX_POINT ( 'NONE', #28181 ) ;
#8818 = ADVANCED_FACE ( 'NONE', ( #1355 ), #40650, .F. ) ;
#8819 = VECTOR ( 'NONE', #11164, 1000.000000000000000 ) ;
#8820 = CARTESIAN_POINT ( 'NONE',  ( -12.72966282067487143, -55.03110224943692685, 1.931329623869216583 ) ) ;
#8821 = CARTESIAN_POINT ( 'NONE',  ( 2.751744599267999636, -79.48073998579799593, 9.005047869058000032 ) ) ;
#8822 = DIRECTION ( 'NONE',  ( 1.000000000000000000, 0.000000000000000000, 0.000000000000000000 ) ) ;
#8823 = EDGE_CURVE ( 'NONE', #36505, #604, #34066, .T. ) ;
#8824 = AXIS2_PLACEMENT_3D ( 'NONE', #1011, #24588, #38155 ) ;
#8825 = CARTESIAN_POINT ( 'NONE',  ( -1.500000000000000222, -81.41041666666664867, -0.1963495408493622363 ) ) ;
#8826 = CARTESIAN_POINT ( 'NONE',  ( -0.3164372427141999844, -79.77903242220000379, 1.635583079321000000 ) ) ;
#8827 = VERTEX_POINT ( 'NONE', #56818 ) ;
#8828 = CARTESIAN_POINT ( 'NONE',  ( 0.000000000000000000, -75.15999999999999659, 0.000000000000000000 ) ) ;
#8829 = CARTESIAN_POINT ( 'NONE',  ( -7.223926682746276917, -77.77156318831207216, -9.395512816074530704 ) ) ;
#8830 = CARTESIAN_POINT ( 'NONE',  ( -1.423904377294301637, -54.49487194733364959, -12.50677628652253759 ) ) ;
#8831 = ORIENTED_EDGE ( 'NONE', *, *, #7675, .F. ) ;
#8832 = ORIENTED_EDGE ( 'NONE', *, *, #5160, .F. ) ;
#8833 = CARTESIAN_POINT ( 'NONE',  ( -9.650965486062000664, -53.86598967493999623, -8.252456811976999873 ) ) ;
#8834 = SURFACE_STYLE_USAGE ( .BOTH. , #39821 ) ;
#8835 = CARTESIAN_POINT ( 'NONE',  ( -2.116314338179000387, -79.93777134585798194, -9.535298106756000536 ) ) ;
#8836 = ORIENTED_EDGE ( 'NONE', *, *, #22873, .F. ) ;
#8837 = ORIENTED_EDGE ( 'NONE', *, *, #36891, .T. ) ;
#8838 = CARTESIAN_POINT ( 'NONE',  ( -4.866794825236000044, -76.53096485469599486, 11.22503275805000023 ) ) ;
#8839 = DIRECTION ( 'NONE',  ( 0.7071067811865474617, 0.000000000000000000, -0.7071067811865474617 ) ) ;
#8840 = CARTESIAN_POINT ( 'NONE',  ( -0.9392528719664000603, -77.77925590253998678, -1.213965203811000038 ) ) ;
#8841 = VERTEX_POINT ( 'NONE', #34929 ) ;
#8842 = CARTESIAN_POINT ( 'NONE',  ( -9.391369684923001060, -77.17838084965399048, 1.399863080762999923 ) ) ;
#8843 = CARTESIAN_POINT ( 'NONE',  ( -12.00000000000000000, 0.000000000000000000, 0.000000000000000000 ) ) ;
#8844 = CARTESIAN_POINT ( 'NONE',  ( 1.165063941761719013, -80.32067678519440790, -0.4527090129185701306 ) ) ;
#8845 = CARTESIAN_POINT ( 'NONE',  ( 7.468771752218000159, -77.16759889844999520, -10.77882862479000003 ) ) ;
#8846 = CARTESIAN_POINT ( 'NONE',  ( 7.508079800428999917, -76.93335787946290338, -8.333477563431999968 ) ) ;
#8847 = CARTESIAN_POINT ( 'NONE',  ( 8.096452064242996016, -19.21421830981000056, 13.15643568217000769 ) ) ;
#8848 = CARTESIAN_POINT ( 'NONE',  ( 3.308356911591838312, -86.39318692614399708, -1.472975398279363191 ) ) ;
#8849 = VECTOR ( 'NONE', #24893, 1000.000000000000227 ) ;
#8850 = CARTESIAN_POINT ( 'NONE',  ( 9.376438147752001129, -79.60544960453100316, -6.156339679782000474 ) ) ;
#8851 = CARTESIAN_POINT ( 'NONE',  ( 8.961394318992308428, -79.87002398672908043, 2.292941110240554359 ) ) ;
#8852 = CARTESIAN_POINT ( 'NONE',  ( -10.33718531723983425, -80.42232376127893190, 3.786698599999175130 ) ) ;
#8853 = ORIENTED_EDGE ( 'NONE', *, *, #2118, .F. ) ;
#8854 = CARTESIAN_POINT ( 'NONE',  ( 9.252740428348991131, -77.57083333333333997, 2.486604901413179913 ) ) ;
#8855 = CARTESIAN_POINT ( 'NONE',  ( 3.295079792876999925, -76.40543611710999983, 11.86077433336000020 ) ) ;
#8856 = CARTESIAN_POINT ( 'NONE',  ( -1.087531843820000121, -80.29133710082599862, 1.056511543117000018 ) ) ;
#8857 = CARTESIAN_POINT ( 'NONE',  ( 3.574643530366263366, -2.595516844331640538, -0.1804099968710304036 ) ) ;
#8858 = CARTESIAN_POINT ( 'NONE',  ( 0.000000000000000000, -33.10361340872000113, 0.000000000000000000 ) ) ;
#8859 = CARTESIAN_POINT ( 'NONE',  ( -1.750000000000000000, -20.25022860793999868, 12.65375411744000012 ) ) ;
#8860 = CARTESIAN_POINT ( 'NONE',  ( -8.035240867088845107, -80.44999999999998863, -7.229432123523354292 ) ) ;
#8861 = CARTESIAN_POINT ( 'NONE',  ( -7.655192530954000318, -79.92897315952798465, 7.967190206674000130 ) ) ;
#8862 = CARTESIAN_POINT ( 'NONE',  ( -1.661399596109000010, -77.55431332859899385, -9.484202486144001298 ) ) ;
#8863 = CARTESIAN_POINT ( 'NONE',  ( -11.72115528760076941, -77.06915921447735229, -2.879779154500307747 ) ) ;
#8864 = CARTESIAN_POINT ( 'NONE',  ( 6.606377239730347739, -79.67708333333331439, -8.596418555780422466 ) ) ;
#8865 = CARTESIAN_POINT ( 'NONE',  ( 0.000000000000000000, -76.00000000000000000, 0.000000000000000000 ) ) ;
#8866 = B_SPLINE_CURVE_WITH_KNOTS ( 'NONE', 3,
 ( #31390, #14267, #42320, #28423 ),
 .UNSPECIFIED., .F., .F.,
 ( 4, 4 ),
 ( 0.000000000000000000, 1.000000000000000000 ),
 .UNSPECIFIED. ) ;
#8867 = VERTEX_POINT ( 'NONE', #52672 ) ;
#8868 = CARTESIAN_POINT ( 'NONE',  ( -0.5103843434498001042, -83.05341104791099838, -1.376937268564000005 ) ) ;
#8869 = CARTESIAN_POINT ( 'NONE',  ( 1.330733645151999989, -79.78386453932999700, 0.2346736355698000043 ) ) ;
#8870 = DIRECTION ( 'NONE',  ( -1.000000000000000000, 0.000000000000000000, 0.000000000000000000 ) ) ;
#8871 = CARTESIAN_POINT ( 'NONE',  ( 6.035966914210000311, -77.83129677688799575, 10.34809972146999968 ) ) ;
#8872 = CARTESIAN_POINT ( 'NONE',  ( 6.540748709914804948, -77.00000000000001421, 6.638316095770077752 ) ) ;
#8873 = CARTESIAN_POINT ( 'NONE',  ( 8.737371597357999065, -78.88622555867699759, 8.129823451939000023 ) ) ;
#8874 = CARTESIAN_POINT ( 'NONE',  ( 4.495978696100999983, -77.84659415034599306, 8.621246072682998474 ) ) ;
#8876 = EDGE_CURVE ( 'NONE', #25256, #10113, #7407, .T. ) ;
#8875 = CARTESIAN_POINT ( 'NONE',  ( -1.669724228661999987, -55.43102323432999867, -12.48434610065999983 ) ) ;
#8877 = CARTESIAN_POINT ( 'NONE',  ( 9.132460868846187907, -76.00377128848815289, 7.392938176916904247 ) ) ;
#8878 = CARTESIAN_POINT ( 'NONE',  ( 4.654517711782999889, -79.86653908624468556, 9.874757255799998745 ) ) ;
#8879 = PLANE ( 'NONE',  #15322 ) ;
#8880 = ORIENTED_EDGE ( 'NONE', *, *, #25689, .F. ) ;
#8881 = CARTESIAN_POINT ( 'NONE',  ( 5.684557159767942736, -78.82291666666664298, 7.396918292183182864 ) ) ;
#8882 = DIRECTION ( 'NONE',  ( 0.000000000000000000, 0.000000000000000000, 1.000000000000000000 ) ) ;
#8883 = EDGE_CURVE ( 'NONE', #7888, #28871, #11772, .T. ) ;
#8884 = AXIS2_PLACEMENT_3D ( 'NONE', #26539, #13264, #25967 ) ;
#8885 = CARTESIAN_POINT ( 'NONE',  ( -2.060841138106245474, -78.54828564506388489, -3.417916573713450479 ) ) ;
#8886 = CARTESIAN_POINT ( 'NONE',  ( 10.97550047727999889, -78.24082415846498861, 0.05101033830554000531 ) ) ;
#8887 = CARTESIAN_POINT ( 'NONE',  ( 12.50000000000000000, -23.25000000000000000, 0.000000000000000000 ) ) ;
#8888 = CARTESIAN_POINT ( 'NONE',  ( -7.770178157204999714, -76.43843624521699098, 9.495887966417999593 ) ) ;
#8889 = DIRECTION ( 'NONE',  ( 1.000000000000000000, 0.000000000000000000, 0.000000000000000000 ) ) ;
#8890 = CARTESIAN_POINT ( 'NONE',  ( -0.5976101762332876044, -76.87935536903508194, 10.80570671848152031 ) ) ;
#8891 = EDGE_LOOP ( 'NONE', ( #41025, #58290 ) ) ;
#8892 = AXIS2_PLACEMENT_3D ( 'NONE', #51816, #20790, #39378 ) ;
#8893 = CARTESIAN_POINT ( 'NONE',  ( -1.629741404508999958, -78.59554001676799828, 11.02717296151999982 ) ) ;
#8894 = CARTESIAN_POINT ( 'NONE',  ( 0.5875992245590921925, -79.93626096961999394, 1.106550443725125232 ) ) ;
#8895 = CARTESIAN_POINT ( 'NONE',  ( -7.000000000000000000, -80.99999999999998579, 0.000000000000000000 ) ) ;
#8896 = FACE_OUTER_BOUND ( 'NONE', #19477, .T. ) ;
#8897 = EDGE_CURVE ( 'NONE', #15380, #10154, #54744, .T. ) ;
#8898 = APPLICATION_CONTEXT ( 'automotive_design' ) ;
#8899 = CARTESIAN_POINT ( 'NONE',  ( -4.472180980751999435, -79.65088080519498703, 10.22208999787000039 ) ) ;
#8900 = DIRECTION ( 'NONE',  ( -1.000000000000000000, 0.000000000000000000, 0.000000000000000000 ) ) ;
#8901 = CARTESIAN_POINT ( 'NONE',  ( 11.00000000000000000, -23.75000000000000000, -1.203259120426999909E-14 ) ) ;
#8902 = AXIS2_PLACEMENT_3D ( 'NONE', #1799, #19212, #10654 ) ;
#8903 = CARTESIAN_POINT ( 'NONE',  ( 12.18149635271999820, -78.56650993477799716, -1.551427017228999894 ) ) ;
#8904 = DIRECTION ( 'NONE',  ( -0.7592504785508700227, 0.04890181650103809369, -0.6489586451871750539 ) ) ;
#8905 = EDGE_CURVE ( 'NONE', #47045, #37071, #54429, .T. ) ;
#8906 = CARTESIAN_POINT ( 'NONE',  ( -1.733997378035443404, -60.32383216727247088, 12.54437956615585215 ) ) ;
#8907 = DIRECTION ( 'NONE',  ( -1.000000000000000000, 0.000000000000000000, 0.000000000000000000 ) ) ;
#8908 = ADVANCED_FACE ( 'NONE', ( #17519, #21939 ), #49114, .T. ) ;
#8909 = LINE ( 'NONE', #88, #12954 ) ;
#8910 = ORIENTED_EDGE ( 'NONE', *, *, #41494, .F. ) ;
#8911 = ORIENTED_EDGE ( 'NONE', *, *, #49590, .T. ) ;
#8912 = CYLINDRICAL_SURFACE ( 'NONE', #18348, 9.549999999999998934 ) ;
#8913 = CARTESIAN_POINT ( 'NONE',  ( -7.118194945375000415, -77.57133998579800505, 6.355464284701999311 ) ) ;
#8914 = ORIENTED_EDGE ( 'NONE', *, *, #54145, .T. ) ;
#8915 = CARTESIAN_POINT ( 'NONE',  ( -7.847895170810467391, -79.70206533371160162, 5.399415251817809569 ) ) ;
#8916 = ORIENTED_EDGE ( 'NONE', *, *, #17963, .T. ) ;
#8917 = CARTESIAN_POINT ( 'NONE',  ( 8.188293269161999177, -24.70494400568999893, 9.395718629078000816 ) ) ;
#8918 = CARTESIAN_POINT ( 'NONE',  ( 8.190817883596546167, -55.56980390652893220, -7.342377162853135353 ) ) ;
#8919 = CARTESIAN_POINT ( 'NONE',  ( 0.3278620359192580547, -82.45482759320131549, 1.218429155783411044 ) ) ;
#8920 = CARTESIAN_POINT ( 'NONE',  ( -12.50385649908071706, -24.78436723039500222, -0.8579675316857384715 ) ) ;
#8921 = CARTESIAN_POINT ( 'NONE',  ( -7.301194973305000779, -79.12972051468399570, 8.515319286630999684 ) ) ;
#8922 = CARTESIAN_POINT ( 'NONE',  ( 7.988132153045272688, -81.00000000000000000, 7.420399617384452640 ) ) ;
#8923 = AXIS2_PLACEMENT_3D ( 'NONE', #39660, #35805, #48258 ) ;
#8924 = EDGE_LOOP ( 'NONE', ( #19516, #2942, #26613, #33056, #25546, #41373, #3441, #36490, #37557, #9500, #53282 ) ) ;
#8925 = ORIENTED_EDGE ( 'NONE', *, *, #39957, .T. ) ;
#8926 = CARTESIAN_POINT ( 'NONE',  ( 1.441789035861242851, -77.46255880455122167, 9.136936837248049059 ) ) ;
#8927 = CARTESIAN_POINT ( 'NONE',  ( -9.808193611224998776, -77.83189663113499535, 5.067887917229000116 ) ) ;
#8928 = AXIS2_PLACEMENT_3D ( 'NONE', #43277, #36358, #27198 ) ;
#8929 = LINE ( 'NONE', #3342, #42248 ) ;
#8930 = CARTESIAN_POINT ( 'NONE',  ( 2.867548251969000095, -78.03932568202999676, -9.270807752789000489 ) ) ;
#8931 = CARTESIAN_POINT ( 'NONE',  ( 6.425964501063000434, -75.91177771482000480, -10.89726081251999901 ) ) ;
#8932 = CARTESIAN_POINT ( 'NONE',  ( -7.632609106719096204, -79.45061835715877407, -5.673732696205357584 ) ) ;
#8933 = CARTESIAN_POINT ( 'NONE',  ( 12.85144117167999944, -57.04527983067000463, 1.980464439859999981 ) ) ;
#8934 = FACE_OUTER_BOUND ( 'NONE', #40439, .T. ) ;
#8935 = CARTESIAN_POINT ( 'NONE',  ( 12.66316398248999953, -16.82133896655000171, 0.04044089952542000155 ) ) ;
#8936 = VECTOR ( 'NONE', #52119, 1000.000000000000000 ) ;
#8937 = CARTESIAN_POINT ( 'NONE',  ( -9.643350356168998161, -24.94034317039000115, -8.260133465584999612 ) ) ;
#8938 = FACE_OUTER_BOUND ( 'NONE', #16399, .T. ) ;
#8939 = CARTESIAN_POINT ( 'NONE',  ( 0.2669918255893000136, -82.75050405486598493, 3.534642628288999777 ) ) ;
#8940 = VERTEX_POINT ( 'NONE', #9550 ) ;
#8941 = B_SPLINE_CURVE_WITH_KNOTS ( 'NONE', 3,
 ( #44449, #58028, #58326, #17589 ),
 .UNSPECIFIED., .F., .F.,
 ( 4, 4 ),
 ( 0.000000000000000000, 1.000000000000000000 ),
 .UNSPECIFIED. ) ;
#8942 = CARTESIAN_POINT ( 'NONE',  ( 8.788067143180999352, -78.75025020734798886, 8.070261318923000360 ) ) ;
#8943 = CARTESIAN_POINT ( 'NONE',  ( 10.96037575245999918, -76.49979439517699120, -3.836821987761000141 ) ) ;
#8944 = CARTESIAN_POINT ( 'NONE',  ( -7.815187951055542648, -78.03981183751436390, 7.382325091166371145 ) ) ;
#8945 = CARTESIAN_POINT ( 'NONE',  ( 10.46934363224000109, -77.49207612824099556, 5.823135730235999397 ) ) ;
#8946 = CARTESIAN_POINT ( 'NONE',  ( 5.000000000000000000, -75.19999999999998863, 0.000000000000000000 ) ) ;
#8947 = B_SPLINE_CURVE_WITH_KNOTS ( 'NONE', 3,
 ( #49055, #8603, #23639, #32189, #14192, #10666 ),
 .UNSPECIFIED., .F., .F.,
 ( 4, 2, 4 ),
 ( 0.000000000000000000, 0.5000000000000000000, 1.000000000000000000 ),
 .UNSPECIFIED. ) ;
#8949 = DIRECTION ( 'NONE',  ( 0.000000000000000000, 0.000000000000000000, 1.000000000000000000 ) ) ;
#8948 = FACE_OUTER_BOUND ( 'NONE', #54517, .T. ) ;
#8950 = CARTESIAN_POINT ( 'NONE',  ( -9.369164850722000892, -23.25000000000000000, 7.601397897754999633 ) ) ;
#8951 = CARTESIAN_POINT ( 'NONE',  ( 3.456234606873382020, -80.94905652473062219, 10.18103548260220315 ) ) ;
#8952 = CARTESIAN_POINT ( 'NONE',  ( 10.53003236230999917, -55.47547726255000100, -7.612971540256999958 ) ) ;
#8953 = CARTESIAN_POINT ( 'NONE',  ( -0.3713770062794000126, -82.25256573098799606, -1.193557338046999927 ) ) ;
#8954 = CARTESIAN_POINT ( 'NONE',  ( -4.618124570880000057, -78.30012939816998596, 10.14532039989999923 ) ) ;
#8955 = CARTESIAN_POINT ( 'NONE',  ( -7.374560639699022424, -78.22708333333335418, 9.596002108778135309 ) ) ;
#8956 = CARTESIAN_POINT ( 'NONE',  ( 11.10501747946000073, -80.56036808024779816, -1.836383218517000149 ) ) ;
#8957 = ORIENTED_EDGE ( 'NONE', *, *, #17131, .T. ) ;
#8958 = DIRECTION ( 'NONE',  ( 0.000000000000000000, 1.000000000000000000, -1.561587422443000175E-14 ) ) ;
#8959 = CARTESIAN_POINT ( 'NONE',  ( 1.667269374601999976, -55.59060116482999803, 12.49858097728999873 ) ) ;
#8960 = CARTESIAN_POINT ( 'NONE',  ( -1.930628539543000066, -60.02124444054000207, -12.72375828107000117 ) ) ;
#8961 = CARTESIAN_POINT ( 'NONE',  ( -3.553300626444999555, -1.714275249885000019, 0.2100116894659999900 ) ) ;
#8962 = CARTESIAN_POINT ( 'NONE',  ( -4.531904799951000484, -77.29021981040699529, -10.26060180864999971 ) ) ;
#8963 = CARTESIAN_POINT ( 'NONE',  ( 1.636761686205427058, -1.666666666666666519, -2.839805762151336399 ) ) ;
#8964 = CARTESIAN_POINT ( 'NONE',  ( 3.317493147027334555, -82.59270831520866807, 2.257618346177341806 ) ) ;
#8965 = CYLINDRICAL_SURFACE ( 'NONE', #55330, 1.750000000000000000 ) ;
#8966 = CARTESIAN_POINT ( 'NONE',  ( 12.54902617719999824, -16.99030198144999915, 0.4617931494614999632 ) ) ;
#8967 = B_SPLINE_SURFACE_WITH_KNOTS ( 'NONE', 3, 3, ( 
 ( #2298, #14976, #50732, #32974, #42735, #29134, #56021, #38287, #6418, #51602, #19421, #32678, #42447, #20013, #23837, #55135, #14392, #51019, #37996, #46599, #15570, #33564, #2015, #47181, #5830, #46889, #19129, #14680, #19712, #6713, #10272, #32390, #50434, #37412, #15276 ),
 ( #1432, #9984, #33269, #27964, #5537, #23546, #51310, #10869, #41560, #28840, #28253, #24431, #1142, #10569, #46307, #41853, #55433, #55732, #28551, #6126, #24132, #42150, #1720, #53031, #8157, #25291, #48611, #47476, #43310, #2582, #52456, #30287, #7002, #2867, #47755 ),
 ( #20584, #26157, #34713, #43599, #21150, #57164, #52744, #25578, #3161, #25004, #57456, #48326, #43894, #16157, #3440, #29424, #39158, #20865, #25867, #43025, #38581, #21441, #44177, #3725, #12581, #34999, #16732, #39452, #7290, #56597, #34133, #33850, #30579, #52175, #12014 ),
 ( #21726, #11730, #56310, #15864, #51888, #17017, #11444, #29709, #12296, #38867, #7866, #56887, #16443, #34426, #29994, #48046, #7579, #27321, #9331, #35584, #35286, #36473, #26435, #54499, #50077, #4903, #17897, #12860, #44756, #48899, #9622, #57740, #14038, #22610, #40914 ) ),
 .UNSPECIFIED., .F., .F., .F.,
 ( 4, 4 ),
 ( 4, 1, 1, 1, 1, 1, 1, 1, 1, 1, 1, 1, 1, 1, 1, 1, 1, 1, 1, 1, 1, 1, 1, 1, 1, 1, 1, 1, 1, 1, 1, 1, 4 ),
 ( -0.3708084972814000291, 1.370808497280999960 ),
 ( 0.3383484129489999770, 0.3594304488109000273, 0.3805124846727999666, 0.4015945205347000169, 0.4226765563966999872, 0.4437585922585999820, 0.4648406281204999768, 0.4859226639823999716, 0.5070046998442999664, 0.5280867357063000478, 0.5491687715681999871, 0.5702508074300999263, 0.5913328432919999766, 0.6124148791539000269, 0.6334969150158999973, 0.6545789508778000476, 0.6756609867396999869, 0.6967430226016000372, 0.7178250584634999765, 0.7389070943254999468, 0.7599891301873999971, 0.7810711660493000474, 0.8021532019111999867, 0.8232352377731000370, 0.8443172736351000074, 0.8653993094969999467, 0.8864813453588999970, 0.9075633812208000473, 0.9286454170826999865, 0.9497274529446999569, 0.9708094888066000072, 0.9918915246685000575, 1.012973560530000094 ),
 .UNSPECIFIED. ) ;
#8968 = CARTESIAN_POINT ( 'NONE',  ( 3.596156905650000013, -85.76107450217398309, 2.031294216177999878 ) ) ;
#8969 = DIRECTION ( 'NONE',  ( 0.000000000000000000, -1.000000000000000000, 0.000000000000000000 ) ) ;
#8970 = EDGE_CURVE ( 'NONE', #45023, #16336, #1230, .T. ) ;
#8971 = DIRECTION ( 'NONE',  ( 1.000000000000000000, 0.000000000000000000, 0.000000000000000000 ) ) ;
#8972 = CARTESIAN_POINT ( 'NONE',  ( 2.552428662871000231, -79.02735696754000116, 12.37732342135999986 ) ) ;
#8973 = CARTESIAN_POINT ( 'NONE',  ( -7.800315838420999626, -76.64709394048399815, 7.658422569234000221 ) ) ;
#8974 = CARTESIAN_POINT ( 'NONE',  ( 0.6544915521845998674, -81.11326172198998563, 1.531959166345999934 ) ) ;
#8975 = CARTESIAN_POINT ( 'NONE',  ( -1.497311080048000065, -78.87270746980999547, 0.3971898337434000004 ) ) ;
#8976 = VECTOR ( 'NONE', #54820, 1000.000000000000114 ) ;
#8977 = CARTESIAN_POINT ( 'NONE',  ( 9.100722152916000951, -77.05266464630139467, -3.274758550341999808 ) ) ;
#8978 = CARTESIAN_POINT ( 'NONE',  ( 1.501514506084554723, -82.48075314929823776, -0.3793901851540854020 ) ) ;
#8979 = DIRECTION ( 'NONE',  ( -0.4045837981831721941, 0.8201365133289436615, -0.4045837981831721941 ) ) ;
#8980 = CARTESIAN_POINT ( 'NONE',  ( -10.45237130512470181, -80.11958314839849038, -2.607326810107436277 ) ) ;
#8981 = DIRECTION ( 'NONE',  ( 1.000000000000000000, 0.000000000000000000, 0.000000000000000000 ) ) ;
#8982 = CARTESIAN_POINT ( 'NONE',  ( -0.6868264915819426442, -77.72950740926451374, -1.073137721056557803 ) ) ;
#8983 = CARTESIAN_POINT ( 'NONE',  ( 1.079681942422447305, -81.80797850944155414, -0.6305161809801804740 ) ) ;
#8984 = AXIS2_PLACEMENT_3D ( 'NONE', #58244, #32523, #31651 ) ;
#8985 = DIRECTION ( 'NONE',  ( 0.000000000000000000, -1.000000000000000000, 0.000000000000000000 ) ) ;
#8986 = ADVANCED_FACE ( 'NONE', ( #30793 ), #12092, .F. ) ;
#8987 = CARTESIAN_POINT ( 'NONE',  ( 8.769046271958000460, -78.51943148693000296, -7.066663249742999753 ) ) ;
#8988 = DIRECTION ( 'NONE',  ( -9.217554797286021519E-07, 2.297153352953660798E-20, 0.9999999999995752287 ) ) ;
#8989 = ORIENTED_EDGE ( 'NONE', *, *, #14095, .F. ) ;
#8990 = ORIENTED_EDGE ( 'NONE', *, *, #25417, .T. ) ;
#8991 = CARTESIAN_POINT ( 'NONE',  ( -1.281859202539999965, -80.58640536786400332, -0.6809617183367999704 ) ) ;
#8992 = CARTESIAN_POINT ( 'NONE',  ( -1.391457981517000064, -78.65970746980998740, -0.2902696593763000044 ) ) ;
#8993 = ORIENTED_EDGE ( 'NONE', *, *, #29375, .F. ) ;
#8994 = DIRECTION ( 'NONE',  ( -1.000000000000000000, 0.000000000000000000, 0.000000000000000000 ) ) ;
#8995 = EDGE_LOOP ( 'NONE', ( #40634, #35600, #49217 ) ) ;
#8996 = LINE ( 'NONE', #27563, #50008 ) ;
#8997 = CARTESIAN_POINT ( 'NONE',  ( -0.7554284705563544255, -78.41666666666667140, 1.310679582531384169 ) ) ;
#8998 = CARTESIAN_POINT ( 'NONE',  ( 10.32003611956000100, -79.86239375944418839, -3.898536120860000231 ) ) ;
#8999 = CARTESIAN_POINT ( 'NONE',  ( 0.5294349409057999001, -79.41170382117660154, -3.927556981920999668 ) ) ;
#9000 = CARTESIAN_POINT ( 'NONE',  ( -5.740620664195313694, -79.32657994115034228, 7.569668994968869136 ) ) ;
#9001 = CARTESIAN_POINT ( 'NONE',  ( 6.574300740938999077, -77.52576138962918151, -8.869200617850999890 ) ) ;
#9002 = CARTESIAN_POINT ( 'NONE',  ( 12.02473175675000050, -79.23708571609999751, -2.852631171805999788 ) ) ;
#9003 = ORIENTED_EDGE ( 'NONE', *, *, #50958, .F. ) ;
#9004 = ORIENTED_EDGE ( 'NONE', *, *, #33623, .F. ) ;
#9005 = DIRECTION ( 'NONE',  ( 0.000000000000000000, 1.000000000000000000, 0.000000000000000000 ) ) ;
#9006 = CARTESIAN_POINT ( 'NONE',  ( -12.56594317823000040, -18.74999998606000062, -1.750000000000000000 ) ) ;
#9007 = EDGE_CURVE ( 'NONE', #21517, #17310, #47759, .T. ) ;
#9008 = CARTESIAN_POINT ( 'NONE',  ( 1.323534079420999987, -79.96208777222700803, -0.1638099207045999872 ) ) ;
#9009 = CARTESIAN_POINT ( 'NONE',  ( 8.898653440358000211, -78.42689348759698476, -3.871004561473999850 ) ) ;
#9010 = B_SPLINE_CURVE_WITH_KNOTS ( 'NONE', 3,
 ( #35283, #22009, #58032, #8436, #26431, #30282, #22305, #26725, #44753, #57452, #4305, #52739, #4004, #57735, #40320, #12291, #34994, #57160 ),
 .UNSPECIFIED., .F., .F.,
 ( 4, 2, 2, 2, 2, 2, 2, 2, 4 ),
 ( 0.000000000000000000, 0.1249999999999999167, 0.2499999999999998890, 0.3749999999999998335, 0.4999999999999998890, 0.6249999999999998890, 0.7499999999999998890, 0.8750000000000000000, 1.000000000000000000 ),
 .UNSPECIFIED. ) ;
#9011 = CARTESIAN_POINT ( 'NONE',  ( -4.367558755064909093, -86.39318692756695839, -0.4180839177783179372 ) ) ;
#9012 = PLANE ( 'NONE',  #28001 ) ;
#9013 = CARTESIAN_POINT ( 'NONE',  ( -3.291354266399999950, -76.72715654337000046, 12.36836470155000001 ) ) ;
#9014 = CARTESIAN_POINT ( 'NONE',  ( -1.273831304311999979, -80.60709877522999989, -0.4509157470602000450 ) ) ;
#9015 = CIRCLE ( 'NONE', #8079, 11.59999999999999964 ) ;
#9016 = CARTESIAN_POINT ( 'NONE',  ( -9.669536374352000863, -76.41932985286300095, 5.242320344620000405 ) ) ;
#9017 = CARTESIAN_POINT ( 'NONE',  ( -0.9948376905992144525, -76.94999999999998863, -9.499999997335510926 ) ) ;
#9018 = CARTESIAN_POINT ( 'NONE',  ( 2.458896070359999797, -79.41556330239998829, -3.318484741470999921 ) ) ;
#9019 = CARTESIAN_POINT ( 'NONE',  ( -11.09105850093000001, -80.25208754019278956, 1.974238845993000258 ) ) ;
#9020 = B_SPLINE_CURVE_WITH_KNOTS ( 'NONE', 3,
 ( #52222, #51942, #2065, #42786, #2916, #7627, #25628, #52505, #28898, #38340, #15622, #21200, #51661, #11209, #33326, #30043, #11779, #34474 ),
 .UNSPECIFIED., .F., .F.,
 ( 4, 2, 2, 2, 2, 2, 2, 2, 4 ),
 ( 0.000000000000000000, 0.1249999999999998335, 0.2499999999999997224, 0.3749999999999997224, 0.4999999999999997780, 0.6249999999999997780, 0.7499999999999998890, 0.8749999999999998890, 1.000000000000000000 ),
 .UNSPECIFIED. ) ;
#9021 = CARTESIAN_POINT ( 'NONE',  ( -10.53101990622000095, -60.10639784916000394, 7.613962745625999062 ) ) ;
#9022 = CARTESIAN_POINT ( 'NONE',  ( 8.665496919457343239, -76.89000174921478958, -8.038609273865034766 ) ) ;
#9023 = CARTESIAN_POINT ( 'NONE',  ( 0.5659508144816000064, -82.13207046129099353, -3.502028359967999549 ) ) ;
#9024 = CARTESIAN_POINT ( 'NONE',  ( -2.799999998984000094, -78.69999999898398357, 6.819591523630000610E-10 ) ) ;
#9025 = CYLINDRICAL_SURFACE ( 'NONE', #44928, 12.05000000000000071 ) ;
#9026 = CARTESIAN_POINT ( 'NONE',  ( -12.09999999999999964, -92.79999999999999716, 0.000000000000000000 ) ) ;
#9027 = CARTESIAN_POINT ( 'NONE',  ( -0.8385792221450999451, -2.959321851618000210, -3.712528424878000166 ) ) ;
#9028 = CARTESIAN_POINT ( 'NONE',  ( -0.2693486100347141088, -80.35804431655570568, -1.245426196537031682 ) ) ;
#9029 = ORIENTED_EDGE ( 'NONE', *, *, #26192, .F. ) ;
#9030 = LINE ( 'NONE', #31440, #14021 ) ;
#9031 = CARTESIAN_POINT ( 'NONE',  ( 12.05000000000000071, -80.60000000000000853, 0.000000000000000000 ) ) ;
#9032 = CARTESIAN_POINT ( 'NONE',  ( 0.6224761083686999319, -81.88553101715500304, -1.179448874982999884 ) ) ;
#9033 = CARTESIAN_POINT ( 'NONE',  ( -12.78015286811999829, -17.69674784880999852, -1.806262579046000072 ) ) ;
#9034 = CARTESIAN_POINT ( 'NONE',  ( 6.891227191158999510, -76.62167840439001054, -9.824000600561999974 ) ) ;
#9035 = CARTESIAN_POINT ( 'NONE',  ( -7.864802647442891370, -61.25123893484760629, -10.10444599044162572 ) ) ;
#9036 = CARTESIAN_POINT ( 'NONE',  ( 12.82904091339000097, -18.67547470641000018, -2.062673488738000049 ) ) ;
#9037 = ORIENTED_EDGE ( 'NONE', *, *, #37431, .T. ) ;
#9038 = EDGE_CURVE ( 'NONE', #46323, #21810, #41340, .T. ) ;
#9039 = CARTESIAN_POINT ( 'NONE',  ( 1.750000000000000000, -60.04999999657000131, -12.50000000000000000 ) ) ;
#9040 = EDGE_CURVE ( 'NONE', #6883, #23569, #25316, .T. ) ;
#9041 = CARTESIAN_POINT ( 'NONE',  ( -0.9627379117275000064, -82.23220295934500257, 1.028099582737000084 ) ) ;
#9042 = DIRECTION ( 'NONE',  ( 1.000000000000000000, 0.000000000000000000, 0.000000000000000000 ) ) ;
#9043 = CARTESIAN_POINT ( 'NONE',  ( -8.751877897654001259, -79.05082360769699790, -3.466385404677000182 ) ) ;
#9045 = CARTESIAN_POINT ( 'NONE',  ( -3.616527695712999702, -1.793843644679999905, -0.5438149879621999583 ) ) ;
#9044 = CARTESIAN_POINT ( 'NONE',  ( 3.677350641359999450, -85.27576277546900485, -1.976537971046000042 ) ) ;
#9046 = CARTESIAN_POINT ( 'NONE',  ( -1.667917367065999912, -60.08056535122999975, -12.49306764019000049 ) ) ;
#9047 = CARTESIAN_POINT ( 'NONE',  ( 0.6743760579952999823, -80.43823808787499274, 1.247107161604999792 ) ) ;
#9048 = ORIENTED_EDGE ( 'NONE', *, *, #3001, .F. ) ;
#9049 = CARTESIAN_POINT ( 'NONE',  ( 7.893016554558063724, -77.29077850116276238, -7.298496125915765020 ) ) ;
#9050 = CARTESIAN_POINT ( 'NONE',  ( 0.7554284705563509839, -79.06666666666667709, -1.310679582531386167 ) ) ;
#9051 = CARTESIAN_POINT ( 'NONE',  ( 0.000000000000000000, -76.75499999999999545, 0.000000000000000000 ) ) ;
#9052 = ORIENTED_EDGE ( 'NONE', *, *, #53943, .T. ) ;
#9053 = EDGE_LOOP ( 'NONE', ( #30138, #58350, #20958, #54673 ) ) ;
#9054 = DIRECTION ( 'NONE',  ( 0.000000000000000000, -1.000000000000000000, 0.000000000000000000 ) ) ;
#9055 = DIRECTION ( 'NONE',  ( 0.000000000000000000, 1.000000000000000000, 0.000000000000000000 ) ) ;
#9056 = CONICAL_SURFACE ( 'NONE', #29755, 0.6999999997694995590, 0.7853981633972997312 ) ;
#9057 = ADVANCED_FACE ( 'NONE', ( #15130 ), #5123, .F. ) ;
#9058 = LINE ( 'NONE', #27339, #44455 ) ;
#9059 = ORIENTED_EDGE ( 'NONE', *, *, #3326, .T. ) ;
#9060 = CARTESIAN_POINT ( 'NONE',  ( -11.68231536908000123, -77.67143497408700625, 2.952842578158000109 ) ) ;
#9061 = ORIENTED_EDGE ( 'NONE', *, *, #55984, .F. ) ;
#9062 = AXIS2_PLACEMENT_3D ( 'NONE', #24927, #29344, #20506 ) ;
#9063 = ORIENTED_EDGE ( 'NONE', *, *, #29153, .T. ) ;
#9064 = CARTESIAN_POINT ( 'NONE',  ( -2.569810659366867256, -2.654058635901579866, -1.999144479470090330 ) ) ;
#9065 = CARTESIAN_POINT ( 'NONE',  ( 10.48543666025108401, -78.59166666666666856, 6.043427764450814976 ) ) ;
#9066 = CARTESIAN_POINT ( 'NONE',  ( 9.534323188421000239, -79.49169524832855416, -1.008198710029000189 ) ) ;
#9067 = ORIENTED_EDGE ( 'NONE', *, *, #34007, .F. ) ;
#9068 = VERTEX_POINT ( 'NONE', #19866 ) ;
#9069 = CARTESIAN_POINT ( 'NONE',  ( -1.229479409833385883, -80.67128155205320184, -0.3337909954253061029 ) ) ;
#9070 = CARTESIAN_POINT ( 'NONE',  ( -11.99583751076623450, -79.79999999999998295, -0.3766131536002892410 ) ) ;
#9071 = DIRECTION ( 'NONE',  ( -0.7071067811865475727, 0.000000000000000000, 0.7071067811865475727 ) ) ;
#9072 = CARTESIAN_POINT ( 'NONE',  ( 0.5962167095188423138, -18.77158755789457345, 10.98383273456533615 ) ) ;
#9073 = FACE_OUTER_BOUND ( 'NONE', #12657, .T. ) ;
#9074 = CARTESIAN_POINT ( 'NONE',  ( 5.917523019358037040, -78.63333333333332575, 10.26699006316254525 ) ) ;
#9075 = CARTESIAN_POINT ( 'NONE',  ( 4.458743082292000004, -77.49465230586955045, 11.11915799896999957 ) ) ;
#9076 = CARTESIAN_POINT ( 'NONE',  ( 0.01626845465039130842, -78.72528669419055802, -9.249899724983746907 ) ) ;
#9077 = CARTESIAN_POINT ( 'NONE',  ( -9.317978910659999059, -25.13238463018999980, 8.588869595444998950 ) ) ;
#9078 = CARTESIAN_POINT ( 'NONE',  ( -1.310679582531386389, -79.94166666666667709, -0.7554284705563492075 ) ) ;
#9079 = CARTESIAN_POINT ( 'NONE',  ( 2.879226727952049814, -78.45416666666666572, 10.71369944335148183 ) ) ;
#9080 = CARTESIAN_POINT ( 'NONE',  ( -7.220923959705292994, -76.72708333333335418, 9.396085398178589898 ) ) ;
#9081 = CARTESIAN_POINT ( 'NONE',  ( -3.126974709266999941, -81.88530496681200077, -2.762623496493000097 ) ) ;
#9082 = EDGE_CURVE ( 'NONE', #33152, #15494, #10419, .T. ) ;
#9083 = CARTESIAN_POINT ( 'NONE',  ( 9.545926504039998761, -77.99008667140098794, -2.045769860731999845 ) ) ;
#9084 = CARTESIAN_POINT ( 'NONE',  ( -12.68702648026999924, -18.24922088193000036, 1.889939500033999797 ) ) ;
#9085 = CARTESIAN_POINT ( 'NONE',  ( -8.343860018000999190, -55.64999999967000122, -8.343860018000999190 ) ) ;
#9086 = CARTESIAN_POINT ( 'NONE',  ( 1.460729357738999923, -24.09091243202000143, 12.44211643240000065 ) ) ;
#9087 = CARTESIAN_POINT ( 'NONE',  ( 10.99999999999999822, -79.85864668888551421, 1.195232468347080079 ) ) ;
#9088 = CARTESIAN_POINT ( 'NONE',  ( 3.124713657347000240, -85.35108058741198533, -1.679501302629999859 ) ) ;
#9089 = CARTESIAN_POINT ( 'NONE',  ( -0.4548042850443000384, -1.265628508794999885, 3.929784724312000321 ) ) ;
#9090 = CARTESIAN_POINT ( 'NONE',  ( -1.466822177622293388, -82.03317782236065625, -0.2501548871699424414 ) ) ;
#9091 = CARTESIAN_POINT ( 'NONE',  ( 0.5010153433495700970, -81.00114992422807347, -1.428186821674153117 ) ) ;
#9092 = CARTESIAN_POINT ( 'NONE',  ( -1.249848728141158993, -78.59781426991139597, 0.03830777415639201322 ) ) ;
#9093 = CARTESIAN_POINT ( 'NONE',  ( 0.1747633057891999908, -78.27442767348290431, 1.605201443249000048 ) ) ;
#9094 = CARTESIAN_POINT ( 'NONE',  ( 0.000000000000000000, -19.21421830981000767, -13.15643568216998638 ) ) ;
#9095 = CARTESIAN_POINT ( 'NONE',  ( 8.827997450462000018, -78.32663815498800375, 6.421979991006000255 ) ) ;
#9096 = AXIS2_PLACEMENT_3D ( 'NONE', #42485, #56065, #29742 ) ;
#9097 = CARTESIAN_POINT ( 'NONE',  ( 2.739292792226000195, -77.58421086662899313, -11.85237552491999935 ) ) ;
#9098 = CARTESIAN_POINT ( 'NONE',  ( 0.000000000000000000, -78.59999999921299718, 0.000000000000000000 ) ) ;
#9100 = CARTESIAN_POINT ( 'NONE',  ( 1.505666248717000055, -79.11208320661400251, 0.1786365444185999962 ) ) ;
#9099 = DIRECTION ( 'NONE',  ( -0.07798810159604820103, 0.04890177472414890258, 0.9957542229075772022 ) ) ;
#9101 = CARTESIAN_POINT ( 'NONE',  ( -0.5277720668919000380, -82.10865968170000428, 1.495277019118000039 ) ) ;
#9102 = ORIENTED_EDGE ( 'NONE', *, *, #31239, .F. ) ;
#9103 = AXIS2_PLACEMENT_3D ( 'NONE', #38701, #16280, #47304 ) ;
#9104 = CARTESIAN_POINT ( 'NONE',  ( -2.415641975597000002, -83.71296544543099571, -2.876810031038000037 ) ) ;
#9105 = DIRECTION ( 'NONE',  ( 0.000000000000000000, -1.000000000000000000, 0.000000000000000000 ) ) ;
#9106 = CARTESIAN_POINT ( 'NONE',  ( 10.38178191893000069, -80.29547733623329009, -3.801471066729000370 ) ) ;
#9107 = VECTOR ( 'NONE', #42067, 1000.000000000000000 ) ;
#9108 = EDGE_CURVE ( 'NONE', #29606, #30887, #2684, .T. ) ;
#9109 = CARTESIAN_POINT ( 'NONE',  ( 12.57042253521000141, -52.69905023022000279, 0.000000000000000000 ) ) ;
#9110 = CARTESIAN_POINT ( 'NONE',  ( -0.3497048678475328520, -85.84947917316429766, 3.392553434455469752 ) ) ;
#9111 = CARTESIAN_POINT ( 'NONE',  ( -0.8253947190445000137, -77.45303325996100341, -11.18645762290999990 ) ) ;
#9112 = CARTESIAN_POINT ( 'NONE',  ( 5.539808784079867543, -78.93333333333333712, 9.611650271896852615 ) ) ;
#9113 = CARTESIAN_POINT ( 'NONE',  ( 7.009066229391000213, -78.51811043579999705, -6.762594642477000484 ) ) ;
#9114 = AXIS2_PLACEMENT_3D ( 'NONE', #13093, #58275, #39965 ) ;
#9115 = CARTESIAN_POINT ( 'NONE',  ( -0.6832218802960999815, -0.9170547980460999060, -3.968530914128000298 ) ) ;
#9116 = CARTESIAN_POINT ( 'NONE',  ( -7.612366974783192575, -76.36927836883999987, -9.041534318350693766 ) ) ;
#9117 = CARTESIAN_POINT ( 'NONE',  ( 12.00000000000000000, -18.75000000000000000, 1.250000000000000000 ) ) ;
#9118 = CARTESIAN_POINT ( 'NONE',  ( -1.799475304559999822, -58.55171076491000548, 12.69616050744000013 ) ) ;
#9119 = ORIENTED_EDGE ( 'NONE', *, *, #39959, .F. ) ;
#9120 = CARTESIAN_POINT ( 'NONE',  ( -1.003693376013180982, -53.83776007857952095, -12.70247752660270812 ) ) ;
#9121 = CARTESIAN_POINT ( 'NONE',  ( -2.944350850530000230, -79.72860665246399492, -8.802063698512000656 ) ) ;
#9122 = DIRECTION ( 'NONE',  ( 1.000000000000000000, 0.000000000000000000, 0.000000000000000000 ) ) ;
#9123 = CARTESIAN_POINT ( 'NONE',  ( 1.310679582531388387, -81.60833333333333428, -0.7554284705563470981 ) ) ;
#9124 = CARTESIAN_POINT ( 'NONE',  ( 0.8512149552595998925, -80.22114692796999691, 1.432023780608000063 ) ) ;
#9125 = CARTESIAN_POINT ( 'NONE',  ( -12.49306764013999960, -55.51943464808999806, -1.667917367065999912 ) ) ;
#9126 = EDGE_CURVE ( 'NONE', #18438, #42771, #53596, .T. ) ;
#9127 = LINE ( 'NONE', #19149, #51059 ) ;
#9128 = ORIENTED_EDGE ( 'NONE', *, *, #2704, .F. ) ;
#9129 = CARTESIAN_POINT ( 'NONE',  ( 9.157990535730000659, -77.69412697158699643, -6.468229441713999606 ) ) ;
#9130 = LINE ( 'NONE', #31537, #46894 ) ;
#9131 = ADVANCED_FACE ( 'NONE', ( #23411 ), #23222, .F. ) ;
#9132 = ORIENTED_EDGE ( 'NONE', *, *, #2786, .F. ) ;
#9133 = CARTESIAN_POINT ( 'NONE',  ( -10.31988039472999930, -54.51085245502000021, -7.753829094159000235 ) ) ;
#9134 = CARTESIAN_POINT ( 'NONE',  ( 9.767191983224998708, -79.58057210502099110, 0.05162932631433000269 ) ) ;
#9135 = ORIENTED_EDGE ( 'NONE', *, *, #18932, .F. ) ;
#9136 = CARTESIAN_POINT ( 'NONE',  ( -11.87094579582000087, -77.21343299368299995, -3.415941325536000051 ) ) ;
#9137 = CARTESIAN_POINT ( 'NONE',  ( -9.691523086186688118, -78.63578696449211236, -4.654780356785987117 ) ) ;
#9138 = CARTESIAN_POINT ( 'NONE',  ( -1.062134069330999964, -79.14247671680999474, 1.107996173502999948 ) ) ;
#9139 = ORIENTED_EDGE ( 'NONE', *, *, #17110, .T. ) ;
#9140 = CARTESIAN_POINT ( 'NONE',  ( 5.807838419657000095, -77.24732305011499989, -7.511754867730999763 ) ) ;
#9141 = AXIS2_PLACEMENT_3D ( 'NONE', #15079, #19520, #37513 ) ;
#9142 = ADVANCED_FACE ( 'NONE', ( #52038 ), #29001, .F. ) ;
#9143 = CARTESIAN_POINT ( 'NONE',  ( 1.174637156278667494, -80.32243980880512879, -0.4274726629302632586 ) ) ;
#9144 = CARTESIAN_POINT ( 'NONE',  ( 7.317687889309999250, -77.75422151684000482, -10.69177725920999933 ) ) ;
#9145 = AXIS2_PLACEMENT_3D ( 'NONE', #22696, #40708, #18280 ) ;
#9146 = CARTESIAN_POINT ( 'NONE',  ( -7.803863155890000236, -78.18622965754646259, 8.057160196619001624 ) ) ;
#9147 = CARTESIAN_POINT ( 'NONE',  ( 3.229228496053007103, -86.25171435493598437, 2.345485728341277554 ) ) ;
#9148 = CARTESIAN_POINT ( 'NONE',  ( -7.843978203195000276, -77.69990496493777243, 5.713380375430999969 ) ) ;
#9149 = CARTESIAN_POINT ( 'NONE',  ( 8.100245516517501798, -79.89060762577963715, 4.466210091324835929 ) ) ;
#9150 = CARTESIAN_POINT ( 'NONE',  ( 3.700621377604330853, -79.35520831959095744, -1.552723024119195827 ) ) ;
#9151 = VERTEX_POINT ( 'NONE', #29283 ) ;
#9152 = CARTESIAN_POINT ( 'NONE',  ( -10.13316084080999957, -80.08481699542699062, 4.924182635666999985 ) ) ;
#9153 = CARTESIAN_POINT ( 'NONE',  ( 11.88049207238000093, -76.28091755325999657, -3.223263369271999856 ) ) ;
#9154 = CARTESIAN_POINT ( 'NONE',  ( -1.508831841893000236, -79.84482349039599569, 0.1495614418054999895 ) ) ;
#9155 = VECTOR ( 'NONE', #48554, 1000.000000000000114 ) ;
#9156 = ADVANCED_FACE ( 'NONE', ( #34002 ), #11595, .F. ) ;
#9157 = CARTESIAN_POINT ( 'NONE',  ( -3.404284203830477917, -3.328750795578371502, 0.8991780458718586777 ) ) ;
#9158 = CARTESIAN_POINT ( 'NONE',  ( 8.270412359550473269, -77.00833333333331154, -4.779119312162220190 ) ) ;
#9159 = CARTESIAN_POINT ( 'NONE',  ( -9.050966798898000931, -55.65000000893999754, 7.919595949288999570 ) ) ;
#9160 = LINE ( 'NONE', #44290, #52474 ) ;
#9161 = EDGE_CURVE ( 'NONE', #40041, #25888, #32867, .T. ) ;
#9162 = CARTESIAN_POINT ( 'NONE',  ( -1.680129511012999899, -77.49053998579799440, -9.591123365327000272 ) ) ;
#9163 = CARTESIAN_POINT ( 'NONE',  ( 0.1322711626442740762, -77.17589890863403923, -12.01631470786458422 ) ) ;
#9164 = DIRECTION ( 'NONE',  ( -1.000000000000000000, 0.000000000000000000, 0.000000000000000000 ) ) ;
#9165 = CARTESIAN_POINT ( 'NONE',  ( 0.000000000000000000, 4.040000000000000036, 0.000000000000000000 ) ) ;
#9166 = ORIENTED_EDGE ( 'NONE', *, *, #57691, .T. ) ;
#9167 = CARTESIAN_POINT ( 'NONE',  ( 1.467208996055999748, -82.67429828359199462, 0.6014104092625999209 ) ) ;
#9168 = CARTESIAN_POINT ( 'NONE',  ( 0.3004848064042999756, -80.16281982998998501, -1.317452118262000038 ) ) ;
#9169 = DIRECTION ( 'NONE',  ( 0.000000000000000000, 0.000000000000000000, -1.000000000000000000 ) ) ;
#9170 = CARTESIAN_POINT ( 'NONE',  ( -11.96278216175999987, -77.99407266942999684, 0.6386762756999999624 ) ) ;
#9171 = CARTESIAN_POINT ( 'NONE',  ( 8.492816448344902014, -77.00000000000001421, -4.278825844373149501 ) ) ;
#9172 = FACE_OUTER_BOUND ( 'NONE', #4217, .T. ) ;
#9173 = CARTESIAN_POINT ( 'NONE',  ( -5.764562846862999912, -78.93534415034599760, 7.830301022820999712 ) ) ;
#9174 = CARTESIAN_POINT ( 'NONE',  ( -9.504204889957000191, -77.13818535316588054, 0.5832244475350000235 ) ) ;
#9175 = CARTESIAN_POINT ( 'NONE',  ( 9.085506314616404566, -76.00424330776989734, 7.450508573089704711 ) ) ;
#9176 = CARTESIAN_POINT ( 'NONE',  ( -8.741790450690999137, -79.97548445825189845, 6.538842841549999285 ) ) ;
#9177 = DIRECTION ( 'NONE',  ( 1.000000000000000000, 0.000000000000000000, 0.000000000000000000 ) ) ;
#9178 = ORIENTED_EDGE ( 'NONE', *, *, #45523, .F. ) ;
#9179 = CARTESIAN_POINT ( 'NONE',  ( -11.91862232003999544, -76.02988133117466418, 3.079279237876998199 ) ) ;
#9180 = CARTESIAN_POINT ( 'NONE',  ( 1.974456364586158141, -78.67390000031812747, -3.418760544059161077 ) ) ;
#9181 = CARTESIAN_POINT ( 'NONE',  ( -6.606377239730371720, -77.42708333333332860, 8.596418555780411808 ) ) ;
#9182 = CARTESIAN_POINT ( 'NONE',  ( 10.85730540529999999, -79.19184598877099290, 1.607151491820999922 ) ) ;
#9183 = CARTESIAN_POINT ( 'NONE',  ( 3.336775769941000114, -77.01990414418399666, -12.05060136398000026 ) ) ;
#9184 = DIRECTION ( 'NONE',  ( -1.893382764135975334E-11, -1.538485725003980272E-07, -0.9999999999999882316 ) ) ;
#9185 = CARTESIAN_POINT ( 'NONE',  ( -3.057614831332267524, -76.89783470746864680, 10.38130180429175375 ) ) ;
#9186 = ORIENTED_EDGE ( 'NONE', *, *, #58236, .F. ) ;
#9187 = VECTOR ( 'NONE', #43072, 1000.000000000000000 ) ;
#9188 = CARTESIAN_POINT ( 'NONE',  ( -10.43948758838000046, -79.80719348725739337, -4.225051887250999449 ) ) ;
#9189 = CARTESIAN_POINT ( 'NONE',  ( 12.70305331329204535, -53.76853698820474392, 0.8727610012071782553 ) ) ;
#9190 = CARTESIAN_POINT ( 'NONE',  ( -9.611650271896833075, -77.64166666666667993, -5.539808784079895077 ) ) ;
#9191 = CARTESIAN_POINT ( 'NONE',  ( -3.661088694550203471, -78.40681307385641219, 2.068643353826707720 ) ) ;
#9193 = DIRECTION ( 'NONE',  ( -1.000000000000000000, 0.000000000000000000, 0.000000000000000000 ) ) ;
#9192 = CARTESIAN_POINT ( 'NONE',  ( 1.275275057825000058, -80.92867431909800757, 0.3379927550398999503 ) ) ;
#9194 = VECTOR ( 'NONE', #29876, 1000.000000000000000 ) ;
#9195 = CARTESIAN_POINT ( 'NONE',  ( -5.018808260229000062, -78.39441589234299101, -9.843244246394000641 ) ) ;
#9196 = CARTESIAN_POINT ( 'NONE',  ( 0.000000000000000000, -45.91785611817000046, 0.000000000000000000 ) ) ;
#9197 = VECTOR ( 'NONE', #8664, 1000.000000000000000 ) ;
#9198 = CARTESIAN_POINT ( 'NONE',  ( 0.000000000000000000, -75.15999999999999659, 0.000000000000000000 ) ) ;
#9199 = CARTESIAN_POINT ( 'NONE',  ( -4.658475568430852753, -79.91666666666665719, 8.082524092276868188 ) ) ;
#9200 = CARTESIAN_POINT ( 'NONE',  ( -2.098469896607999926E-14, 0.000000000000000000, 0.000000000000000000 ) ) ;
#9201 = CARTESIAN_POINT ( 'NONE',  ( 12.69999999999999929, 0.000000000000000000, 0.000000000000000000 ) ) ;
#9202 = ORIENTED_EDGE ( 'NONE', *, *, #6956, .F. ) ;
#9203 = EDGE_LOOP ( 'NONE', ( #8612, #14726, #6071, #574 ) ) ;
#9204 = CARTESIAN_POINT ( 'NONE',  ( -4.784380313523539208, -78.48333333333332007, -8.300970689365453126 ) ) ;
#9205 = ORIENTED_EDGE ( 'NONE', *, *, #17715, .F. ) ;
#9206 = DIRECTION ( 'NONE',  ( -1.000000000000000000, 0.000000000000000000, 0.000000000000000000 ) ) ;
#9207 = ORIENTED_EDGE ( 'NONE', *, *, #25617, .F. ) ;
#9208 = CARTESIAN_POINT ( 'NONE',  ( 7.658894224177999810, -23.20939395863999977, 10.01676912201999947 ) ) ;
#9209 = CARTESIAN_POINT ( 'NONE',  ( -2.271373002040000255, -77.53263888113500002, 10.79548975578000025 ) ) ;
#9210 = EDGE_CURVE ( 'NONE', #48909, #20818, #41364, .T. ) ;
#9211 = CARTESIAN_POINT ( 'NONE',  ( 7.429974109822146566, -55.28385402668686055, -8.111636311580273428 ) ) ;
#9212 = CARTESIAN_POINT ( 'NONE',  ( 6.644622036202999737, -78.31448998579800502, -7.049129409659999901 ) ) ;
#9213 = EDGE_CURVE ( 'NONE', #25746, #56911, #52782, .T. ) ;
#9214 = CARTESIAN_POINT ( 'NONE',  ( -3.517582505936258208, -78.19409754089322462, -8.554969473927931389 ) ) ;
#9215 = CARTESIAN_POINT ( 'NONE',  ( -11.06493808903000087, -79.27921809696499622, -1.839906431680000010 ) ) ;
#9216 = CARTESIAN_POINT ( 'NONE',  ( 5.643768039804604619, -81.00000000000002842, 9.293348226988427996 ) ) ;
#9217 = B_SPLINE_CURVE_WITH_KNOTS ( 'NONE', 3,
 ( #5535, #25224, #16087, #38800, #41558, #56528, #6932, #47974, #3090, #43243, #2801, #21084, #20796, #46305, #19127, #30218, #34068, #23544 ),
 .UNSPECIFIED., .F., .F.,
 ( 4, 2, 2, 2, 2, 2, 2, 2, 4 ),
 ( 0.000000000000000000, 0.1250000000000000000, 0.2500000000000000000, 0.3750000000000000000, 0.5000000000000000000, 0.6250000000000000000, 0.7500000000000000000, 0.8750000000000000000, 1.000000000000000000 ),
 .UNSPECIFIED. ) ;
#9218 = ORIENTED_EDGE ( 'NONE', *, *, #57744, .F. ) ;
#9219 = CARTESIAN_POINT ( 'NONE',  ( -11.00000000000000000, -18.25000000000000000, 0.000000000000000000 ) ) ;
#9220 = ORIENTED_EDGE ( 'NONE', *, *, #45118, .T. ) ;
#9221 = CARTESIAN_POINT ( 'NONE',  ( -0.9113069885316975594, -77.48300007202549011, 9.208075695052512444 ) ) ;
#9222 = CARTESIAN_POINT ( 'NONE',  ( -3.203604947276999848, -77.82858013947499387, 10.56508708803000118 ) ) ;
#9223 = CARTESIAN_POINT ( 'NONE',  ( 0.3926218265389159190, -77.85416666666667140, 1.460959015002474715 ) ) ;
#9224 = CARTESIAN_POINT ( 'NONE',  ( -9.282419925074000489, -77.35369851552198384, -2.829762163499999872 ) ) ;
#9225 = CARTESIAN_POINT ( 'NONE',  ( -9.803620017999000069, -75.77582143684999494, 8.243458997453000592 ) ) ;
#9226 = CARTESIAN_POINT ( 'NONE',  ( -8.469455166620191378, -79.43739211172909620, -4.303251210716531716 ) ) ;
#9227 = CARTESIAN_POINT ( 'NONE',  ( -0.8961266428360998848, -77.69180782643999805, 1.358359200922999888 ) ) ;
#9228 = DIRECTION ( 'NONE',  ( 0.000000000000000000, 0.000000000000000000, 1.000000000000000000 ) ) ;
#9229 = EDGE_CURVE ( 'NONE', #32213, #1567, #6756, .T. ) ;
#9230 = CARTESIAN_POINT ( 'NONE',  ( 9.274475910318999539, -79.13469620609498634, -5.802750462065000114 ) ) ;
#9231 = CARTESIAN_POINT ( 'NONE',  ( -10.00831380745999866, -23.37230364585000331, -7.646786653130999589 ) ) ;
#9232 = CIRCLE ( 'NONE', #54503, 12.57042253521000141 ) ;
#9233 = CARTESIAN_POINT ( 'NONE',  ( -3.512421248448999833, -83.11125530066698275, 0.4773554171805000079 ) ) ;
#9234 = ORIENTED_EDGE ( 'NONE', *, *, #44386, .T. ) ;
#9235 = CARTESIAN_POINT ( 'NONE',  ( 12.31534470299000006, -79.13438534395299939, 1.709481828355000177 ) ) ;
#9236 = CARTESIAN_POINT ( 'NONE',  ( 8.726902940210999660, -75.87452899014900254, 6.502829119990000351 ) ) ;
#9237 = CARTESIAN_POINT ( 'NONE',  ( -5.166105824225122767, -78.01496696634453087, 9.427318864941536702 ) ) ;
#9238 = B_SPLINE_CURVE_WITH_KNOTS ( 'NONE', 3,
 ( #10970, #39256, #25964, #33955, #52273, #24822, #21542, #7389, #39548, #56982, #20396, #56702, #38394, #57271, #6813, #11827, #43988, #30388 ),
 .UNSPECIFIED., .F., .F.,
 ( 4, 2, 2, 2, 2, 2, 2, 2, 4 ),
 ( 0.000000000000000000, 0.1249999999999999722, 0.2499999999999999445, 0.3749999999999998890, 0.4999999999999998890, 0.6249999999999998890, 0.7499999999999997780, 0.8749999999999998890, 1.000000000000000000 ),
 .UNSPECIFIED. ) ;
#9239 = CARTESIAN_POINT ( 'NONE',  ( -9.964549960864999889, -77.65485202078399141, 6.650098383618000319 ) ) ;
#9240 = CARTESIAN_POINT ( 'NONE',  ( -12.70457892003044620, -61.97873330296432215, 0.5105076821750260674 ) ) ;
#9242 = CARTESIAN_POINT ( 'NONE',  ( -10.74987180213209292, -79.09496495074813538, 0.7036268749256830990 ) ) ;
#9241 = CARTESIAN_POINT ( 'NONE',  ( -12.00000000000000000, -79.39999999999999147, 0.000000000000000000 ) ) ;
#9243 = MECHANICAL_DESIGN_GEOMETRIC_PRESENTATION_REPRESENTATION (  '', ( #41308 ), #19612 ) ;
#9244 = CARTESIAN_POINT ( 'NONE',  ( 26.49999981590656262, -39.30476017083000073, 0.003123612069575185893 ) ) ;
#9245 = CARTESIAN_POINT ( 'NONE',  ( -10.76455872347999865, -80.53252629438799204, 3.409670607742999682 ) ) ;
#9246 = DIRECTION ( 'NONE',  ( 0.000000000000000000, 1.000000000000000000, 0.000000000000000000 ) ) ;
#9247 = CARTESIAN_POINT ( 'NONE',  ( 10.72689817447000138, -77.61922082312399596, -3.031213639016000272 ) ) ;
#9248 = CYLINDRICAL_SURFACE ( 'NONE', #23354, 12.05000000000000071 ) ;
#9249 = CARTESIAN_POINT ( 'NONE',  ( 4.142522846324000696, -80.80321295308820595, 10.21795800799999832 ) ) ;
#9250 = ORIENTED_EDGE ( 'NONE', *, *, #8823, .F. ) ;
#9251 = ADVANCED_FACE ( 'NONE', ( #42778 ), #52213, .F. ) ;
#9252 = CARTESIAN_POINT ( 'NONE',  ( 1.814305421036000121, -54.51058030636000495, 12.78003582248999948 ) ) ;
#9253 = CARTESIAN_POINT ( 'NONE',  ( -2.062312494845999655, -60.02715659860000130, -12.83634740211000036 ) ) ;
#9254 = CARTESIAN_POINT ( 'NONE',  ( -3.585353612862000272, -2.245771227706999884, -1.277122609306000189 ) ) ;
#9255 = CARTESIAN_POINT ( 'NONE',  ( -9.998780405325002008, -77.23574712440399992, -5.083552005986999411 ) ) ;
#9256 = CARTESIAN_POINT ( 'NONE',  ( 9.028681611143001717, -78.01309479089799481, -5.970393136294000591 ) ) ;
#9257 = CARTESIAN_POINT ( 'NONE',  ( -0.4254240051736147277, -1.614583333333333259, -3.250000000000000888 ) ) ;
#9258 = DIRECTION ( 'NONE',  ( 0.7071067811865473507, -1.433669009702094715E-08, 0.7071067811865473507 ) ) ;
#9259 = CARTESIAN_POINT ( 'NONE',  ( -7.711243899566701643, -78.56159779477874849, -7.536022382359825578 ) ) ;
#9260 = CARTESIAN_POINT ( 'NONE',  ( 7.648026766753000416, -60.05000000550000294, -10.12290050090999927 ) ) ;
#9261 = CARTESIAN_POINT ( 'NONE',  ( 4.174305119369000394, -82.50274735065200105, -0.06567590414889999673 ) ) ;
#9262 = CARTESIAN_POINT ( 'NONE',  ( 0.000000000000000000, -74.64999999999999147, 0.000000000000000000 ) ) ;
#9263 = CARTESIAN_POINT ( 'NONE',  ( 9.643342484248000446, -53.85965044121000034, -8.260141428653000162 ) ) ;
#9264 = B_SPLINE_SURFACE_WITH_KNOTS ( 'NONE', 3, 3, ( 
 ( #57936, #30484, #31049, #48510, #8057, #35781, #12767, #44077, #49084, #53810, #3626, #30763, #39922, #40810, #693, #31639, #28379, #14224, #46425, #5376, #27213, #5092, #45251, #46137, #13644, #18675, #50847, #37245, #54966, #13937, #32222, #5660, #27506, #5954, #36666 ),
 ( #54682, #50264, #23088, #9812, #23384, #23956, #23670, #22801, #41683, #1263, #978, #41976, #27797, #32799, #402, #4800, #36083, #19250, #18380, #55257, #18090, #10393, #41395, #41101, #45841, #14806, #18961, #36955, #54102, #49682, #14517, #31932, #9227, #32509, #36373 ),
 ( #54399, #49976, #10106, #9519, #50554, #28086, #45547, #56143, #56431, #15690, #6243, #47011, #7124, #11849, #29828, #56721, #33098, #42564, #24260, #25414, #42276, #37831, #37534, #34258, #38411, #38700, #47879, #11276, #16278, #7410, #33972, #52290, #47597, #51434, #47303 ),
 ( #55551, #2130, #1547, #20702, #15982, #55851, #33686, #25124, #10988, #19539, #20131, #15403, #28673, #43148, #38119, #33396, #15101, #52010, #51142, #6541, #19836, #29542, #2707, #28969, #1844, #10696, #51724, #46727, #29254, #24550, #6829, #24841, #42855, #11564, #2415 ) ),
 .UNSPECIFIED., .F., .F., .F.,
 ( 4, 4 ),
 ( 4, 1, 1, 1, 1, 1, 1, 1, 1, 1, 1, 1, 1, 1, 1, 1, 1, 1, 1, 1, 1, 1, 1, 1, 1, 1, 1, 1, 1, 1, 1, 1, 4 ),
 ( -0.3882448580381000491, 1.388244858038000018 ),
 ( -0.01763212848115999765, 0.01102008030072000079, 0.03967228908261000164, 0.06832449786448999141, 0.09697670664638000093, 0.1256289154283000142, 0.1542811242101000124, 0.1829333329919999862, 0.2115855417738999877, 0.2402377505557999893, 0.2688899593376999908, 0.2975421681195999923, 0.3261943769014999939, 0.3548465856833000198, 0.3834987944651999658, 0.4121510032471000229, 0.4408032120290000244, 0.4694554208109000260, 0.4981076295927999720, 0.5267598383746000534, 0.5554120471565000550, 0.5840642559384000565, 0.6127164647203000580, 0.6413686735021999485, 0.6700208822840999501, 0.6986730910659999516, 0.7273252998478000331, 0.7559775086296999236, 0.7846297174115999251, 0.8132819261935000377, 0.8419341349753999282, 0.8705863437573000407, 0.8992385525391000112 ),
 .UNSPECIFIED. ) ;
#9265 = CARTESIAN_POINT ( 'NONE',  ( 10.22699339414000086, -77.49142057354099222, 4.434321446068000050 ) ) ;
#9266 = CARTESIAN_POINT ( 'NONE',  ( -0.5298108134926000634, -80.67114721621999252, 1.579417458585999912 ) ) ;
#9267 = CARTESIAN_POINT ( 'NONE',  ( -1.391730330000000126, -79.43715828658999101, 0.3480381455443000149 ) ) ;
#9268 = CARTESIAN_POINT ( 'NONE',  ( 2.309272084855999996, -77.03463947106759235, -9.392260232199999948 ) ) ;
#9269 = CARTESIAN_POINT ( 'NONE',  ( 0.8225791642732954712, -82.42002313476852748, -1.311939220806510153 ) ) ;
#9270 = CARTESIAN_POINT ( 'NONE',  ( -12.66736977985000046, -61.03307288738999858, 1.690635117038999935 ) ) ;
#9271 = CARTESIAN_POINT ( 'NONE',  ( -10.96673197750000206, -78.35320051065244229, -0.4413686857046000278 ) ) ;
#9272 = CARTESIAN_POINT ( 'NONE',  ( 12.56594317823000040, -23.25000001387000026, -1.750000000000000000 ) ) ;
#9273 = CARTESIAN_POINT ( 'NONE',  ( -10.75744095928762789, -78.87276644371578982, -3.177903864377569665 ) ) ;
#9274 = AXIS2_PLACEMENT_3D ( 'NONE', #1626, #19331, #50053 ) ;
#9275 = CARTESIAN_POINT ( 'NONE',  ( 1.001278227489189598, -81.79905685887599986, -0.7511161502827685688 ) ) ;
#9276 = CARTESIAN_POINT ( 'NONE',  ( -9.611650271896852615, -79.55833333333332291, 5.539808784079869319 ) ) ;
#9277 = CARTESIAN_POINT ( 'NONE',  ( 6.836697942985000331, -79.21359444038398578, 8.804212730688998789 ) ) ;
#9278 = CARTESIAN_POINT ( 'NONE',  ( 8.188331488387602164, -55.57158755757197355, 7.345153731672233732 ) ) ;
#9279 = VERTEX_POINT ( 'NONE', #20906 ) ;
#9280 = ORIENTED_EDGE ( 'NONE', *, *, #12812, .T. ) ;
#9281 = CARTESIAN_POINT ( 'NONE',  ( -3.046994021028059052, -0.7499999999999998890, 1.760728177967239461 ) ) ;
#9282 = ORIENTED_EDGE ( 'NONE', *, *, #24871, .F. ) ;
#9283 = CARTESIAN_POINT ( 'NONE',  ( 1.733997378016492341, -55.27616783188641136, 12.54437956609226035 ) ) ;
#9284 = ORIENTED_EDGE ( 'NONE', *, *, #356, .F. ) ;
#9285 = CARTESIAN_POINT ( 'NONE',  ( 1.249765501161204995, -80.36036749726001460, 0.1566955736949024458 ) ) ;
#9286 = CARTESIAN_POINT ( 'NONE',  ( -11.03649469273005046, -79.84071565590951991, 1.313607443778667783 ) ) ;
#9287 =( GEOMETRIC_REPRESENTATION_CONTEXT ( 3 ) GLOBAL_UNCERTAINTY_ASSIGNED_CONTEXT ( ( #11271 ) ) GLOBAL_UNIT_ASSIGNED_CONTEXT ( ( #20137, #52585, #47603 ) ) REPRESENTATION_CONTEXT ( 'NONE', 'WORKASPACE' ) );
#9288 = EDGE_CURVE ( 'NONE', #6742, #24385, #31500, .T. ) ;
#9289 = CARTESIAN_POINT ( 'NONE',  ( -1.818468715484000065E-14, -79.21250000010999770, -11.96250000010999948 ) ) ;
#9290 = B_SPLINE_CURVE_WITH_KNOTS ( 'NONE', 3,
 ( #37561, #28698, #4162, #12441, #39876, #8010, #35430, #53460, #57888, #3868, #30715, #30142, #44311, #49040, #34285, #48191, #30434, #58182, #35143, #17156, #26298, #13003, #52890 ),
 .UNSPECIFIED., .F., .F.,
 ( 4, 2, 2, 1, 2, 2, 2, 2, 2, 2, 2, 4 ),
 ( 0.000000000000000000, 0.1250000000000001388, 0.1875000000000001388, 0.2500000000000001665, 0.3125000000000001665, 0.3750000000000001665, 0.5000000000000001110, 0.6250000000000001110, 0.6875000000000001110, 0.7500000000000000000, 0.8750000000000001110, 1.000000000000000000 ),
 .UNSPECIFIED. ) ;
#9291 = CARTESIAN_POINT ( 'NONE',  ( -1.432040783484000102, -79.29145339669528880, -3.695292598717999866 ) ) ;
#9292 = CARTESIAN_POINT ( 'NONE',  ( -7.748038516948378529, -79.35049307451645006, 5.497056738179014523 ) ) ;
#9293 = CARTESIAN_POINT ( 'NONE',  ( 1.277168492611395978, -77.21571277153906010, 10.79911615156215099 ) ) ;
#9294 = CARTESIAN_POINT ( 'NONE',  ( -1.726904517088999835, -78.63095455000001266, 11.78767162433000060 ) ) ;
#9295 = ORIENTED_EDGE ( 'NONE', *, *, #27197, .F. ) ;
#9296 = ORIENTED_EDGE ( 'NONE', *, *, #27766, .T. ) ;
#9297 = CARTESIAN_POINT ( 'NONE',  ( -3.248553649406136667, -1.606043880758631248, -0.1773244309825293408 ) ) ;
#9298 = CARTESIAN_POINT ( 'NONE',  ( 1.313995274498999999, -80.45821400603800555, -0.2280190045613000038 ) ) ;
#9299 = CARTESIAN_POINT ( 'NONE',  ( -8.771427373352999268, -77.74472158850198866, -4.151237309591000013 ) ) ;
#9300 = CARTESIAN_POINT ( 'NONE',  ( 0.4592281444767835619, -86.39318692756698681, -4.363424475405689229 ) ) ;
#9301 = CARTESIAN_POINT ( 'NONE',  ( -10.59548767697000038, -21.75736537952000305, 7.678667886032999768 ) ) ;
#9302 = CARTESIAN_POINT ( 'NONE',  ( 9.135190432272999317, -76.61072037624001041, -8.185884657762999339 ) ) ;
#9303 = ADVANCED_FACE ( 'NONE', ( #4941 ), #31795, .F. ) ;
#9304 = CARTESIAN_POINT ( 'NONE',  ( 1.367321113498000118, -80.92305232442998886, 0.5356168500207999505 ) ) ;
#9305 = CARTESIAN_POINT ( 'NONE',  ( 10.77194460988999936, -76.78804022114499617, 1.560654010453999874 ) ) ;
#9306 = CARTESIAN_POINT ( 'NONE',  ( -0.8944171124340070111, -79.16181922138737548, -0.8730969871168202667 ) ) ;
#9307 = FACE_OUTER_BOUND ( 'NONE', #22114, .T. ) ;
#9308 = CARTESIAN_POINT ( 'NONE',  ( -3.559879492179999882, -80.05643680478300439, 2.176540992451000189 ) ) ;
#9309 = CARTESIAN_POINT ( 'NONE',  ( -0.3187246912203000049, -80.64335745824000412, 11.26088853021000169 ) ) ;
#9310 = CARTESIAN_POINT ( 'NONE',  ( -10.18491080491000034, -55.49283319101999723, 7.640030264136999705 ) ) ;
#9311 = CARTESIAN_POINT ( 'NONE',  ( 3.099784061626695841, -2.875628255113011456, 1.008047939721263608 ) ) ;
#9312 = CARTESIAN_POINT ( 'NONE',  ( -3.026655884748000069, -80.08782046129100252, 1.850380170909999844 ) ) ;
#9313 = CARTESIAN_POINT ( 'NONE',  ( -1.210921577777000158, -78.23125641502100791, 0.5587889421650999999 ) ) ;
#9314 = AXIS2_PLACEMENT_3D ( 'NONE', #50422, #42724, #24714 ) ;
#9315 = DIRECTION ( 'NONE',  ( -1.000000000000000000, 3.791735831002999804E-11, 3.791715846987999626E-11 ) ) ;
#9316 = CARTESIAN_POINT ( 'NONE',  ( 7.496935112050000072, -80.71873919278517917, 8.408636027568000770 ) ) ;
#9317 = ADVANCED_FACE ( 'NONE', ( #19685 ), #7737, .F. ) ;
#9318 = CARTESIAN_POINT ( 'NONE',  ( 6.677308892935373663, -77.19999999999997442, -8.580962954970415169 ) ) ;
#9319 = EDGE_LOOP ( 'NONE', ( #17864, #38888, #11473, #34810 ) ) ;
#9320 = CARTESIAN_POINT ( 'NONE',  ( 0.000000000000000000, -15.06282895647999887, 0.000000000000000000 ) ) ;
#9321 = CARTESIAN_POINT ( 'NONE',  ( 1.500000000000000000, -80.25000000000000000, 0.000000000000000000 ) ) ;
#9322 = ADVANCED_FACE ( 'NONE', ( #37686 ), #14378, .F. ) ;
#9323 = CARTESIAN_POINT ( 'NONE',  ( -1.439896632895311113, -79.31458333333334565, -11.00000000000000355 ) ) ;
#9324 = B_SPLINE_CURVE_WITH_KNOTS ( 'NONE', 3,
 ( #16340, #56203, #42917, #42339, #46785, #19899, #33456, #2474, #56490, #1905, #34318, #52068, #47073, #11905, #20477, #29884, #38473, #37891 ),
 .UNSPECIFIED., .F., .F.,
 ( 4, 2, 2, 2, 2, 2, 2, 2, 4 ),
 ( 0.000000000000000000, 0.1250000000000000000, 0.2500000000000000000, 0.3750000000000000000, 0.5000000000000000000, 0.6250000000000000000, 0.7500000000000000000, 0.8750000000000000000, 1.000000000000000000 ),
 .UNSPECIFIED. ) ;
#9325 = CARTESIAN_POINT ( 'NONE',  ( -7.247844507162001015, -18.75000000000000000, -9.722718241315000398 ) ) ;
#9326 = CARTESIAN_POINT ( 'NONE',  ( 1.667917367010000040, -55.51943307300000185, 12.49306752631999906 ) ) ;
#9327 = CARTESIAN_POINT ( 'NONE',  ( 9.175280770439000477, -76.67484661803999302, -8.221808909867000636 ) ) ;
#9328 = CARTESIAN_POINT ( 'NONE',  ( -3.584700322809565520, -79.50216406493034071, 10.13469974220001113 ) ) ;
#9329 = AXIS2_PLACEMENT_3D ( 'NONE', #29321, #56210, #29608 ) ;
#9330 = CARTESIAN_POINT ( 'NONE',  ( 8.213537570112000807, -79.71768667140099751, -4.408490834274999770 ) ) ;
#9331 = CARTESIAN_POINT ( 'NONE',  ( 9.112744727833000269, -76.18430091963000450, -8.574219231229999849 ) ) ;
#9332 = ORIENTED_EDGE ( 'NONE', *, *, #5039, .T. ) ;
#9333 = CARTESIAN_POINT ( 'NONE',  ( -13.89248034750000116, -69.19159251015000223, -2.632538496651000052E-05 ) ) ;
#9334 = CARTESIAN_POINT ( 'NONE',  ( -9.254388464354001087, -79.80752053325198858, 5.469807505829999528 ) ) ;
#9335 = B_SPLINE_CURVE_WITH_KNOTS ( 'NONE', 3,
 ( #53520, #48807, #13061, #52376, #11929, #8352, #44368, #3921, #31060, #49097, #29907, #41113, #27225, #9240, #54114, #990 ),
 .UNSPECIFIED., .F., .F.,
 ( 4, 2, 2, 2, 2, 2, 2, 4 ),
 ( 0.000000000000000000, 0.2499999999999955591, 0.3749999999999933387, 0.4374999999999921729, 0.4999999999999910072, 0.6249999999999932276, 0.7499999999999954481, 1.000000000000000000 ),
 .UNSPECIFIED. ) ;
#9336 = CARTESIAN_POINT ( 'NONE',  ( -0.3379921552883999869, -81.90302968668000005, -1.367316507193000019 ) ) ;
#9337 = CARTESIAN_POINT ( 'NONE',  ( -7.648026768024999811, -18.75000001589999954, 10.12290050218000026 ) ) ;
#9338 = CARTESIAN_POINT ( 'NONE',  ( -6.987523971486999663, -79.07924743682598034, -6.307590925213999888 ) ) ;
#9340 = CARTESIAN_POINT ( 'NONE',  ( 3.981113306789000106, -1.022141436244000001, -0.5296481109823999445 ) ) ;
#9339 = CARTESIAN_POINT ( 'NONE',  ( 2.242347041487000148, -85.02368520868098756, -3.468485713094000111 ) ) ;
#9341 = CARTESIAN_POINT ( 'NONE',  ( 1.217465845835393967, -82.27083333333331439, 0.3271848554491025851 ) ) ;
#9342 = CARTESIAN_POINT ( 'NONE',  ( -1.247892825656000015, -79.17060648544099877, -0.1947040076506000028 ) ) ;
#9343 = ADVANCED_FACE ( 'NONE', ( #30842 ), #828, .F. ) ;
#9344 = VERTEX_POINT ( 'NONE', #26415 ) ;
#9345 = CARTESIAN_POINT ( 'NONE',  ( -2.166067413260452490, -77.20901008302325863, -10.53065413872945300 ) ) ;
#9346 = CARTESIAN_POINT ( 'NONE',  ( 11.75000000000000000, -77.45000000000000284, 1.043320980279999928E-14 ) ) ;
#9347 = ORIENTED_EDGE ( 'NONE', *, *, #57788, .T. ) ;
#9348 = ORIENTED_EDGE ( 'NONE', *, *, #32148, .T. ) ;
#9349 = CARTESIAN_POINT ( 'NONE',  ( -0.9103933733443999587, -79.82065460235210708, -11.99492895764000089 ) ) ;
#9350 = DIRECTION ( 'NONE',  ( -0.9135454576426007556, 0.000000000000000000, 0.4067366430758003193 ) ) ;
#9351 = DIRECTION ( 'NONE',  ( 0.000000000000000000, -1.000000000000000000, 0.000000000000000000 ) ) ;
#9352 = EDGE_LOOP ( 'NONE', ( #36280, #42103, #12251, #20693 ) ) ;
#9353 = PRODUCT_DEFINITION_FORMATION_WITH_SPECIFIED_SOURCE ( 'ANY', '', #8315, .NOT_KNOWN. ) ;
#9354 = CARTESIAN_POINT ( 'NONE',  ( -4.109499447189000065, -78.59383169849499495, 11.32730267836999971 ) ) ;
#9355 = EDGE_LOOP ( 'NONE', ( #44774, #40275, #17545, #42761 ) ) ;
#9356 = ORIENTED_EDGE ( 'NONE', *, *, #41685, .F. ) ;
#9357 = CARTESIAN_POINT ( 'NONE',  ( 1.048127130988076861, -2.751564908735101067, -3.083268915589403303 ) ) ;
#9358 = DIRECTION ( 'NONE',  ( 0.000000000000000000, 1.000000000000000000, 0.000000000000000000 ) ) ;
#9359 = CARTESIAN_POINT ( 'NONE',  ( 9.445921377069225855, -79.15851891711977828, 1.025770609074986961 ) ) ;
#9360 = ORIENTED_EDGE ( 'NONE', *, *, #20685, .F. ) ;
#9361 = CARTESIAN_POINT ( 'NONE',  ( 1.227045062450840884, -82.83502415505597583, -0.2377312851286680906 ) ) ;
#9362 = EDGE_LOOP ( 'NONE', ( #9573, #21755, #38834, #16750 ) ) ;
#9363 = CARTESIAN_POINT ( 'NONE',  ( -1.149554727142765964, -79.68538967717259425, -0.5515177578643482015 ) ) ;
#9364 = AXIS2_PLACEMENT_3D ( 'NONE', #146, #44690, #31081 ) ;
#9365 = CARTESIAN_POINT ( 'NONE',  ( -4.006190475301194098, -78.85171438276198330, -2.263637441416614493 ) ) ;
#9366 = LINE ( 'NONE', #18809, #48202 ) ;
#9367 = CARTESIAN_POINT ( 'NONE',  ( -7.718368845809999712, -20.25199022618999933, -10.07722254369999959 ) ) ;
#9368 = DIRECTION ( 'NONE',  ( 3.675129103447999014E-09, -0.9999999999999997780, -2.168720766502999921E-08 ) ) ;
#9369 = EDGE_CURVE ( 'NONE', #15380, #25723, #1968, .T. ) ;
#9370 = CARTESIAN_POINT ( 'NONE',  ( -1.538071403320043551, -78.68541666666666856, 11.74999999999999467 ) ) ;
#9371 = CARTESIAN_POINT ( 'NONE',  ( 10.42503750987000011, -77.35900572875097225, -5.902083371034001047 ) ) ;
#9372 = CARTESIAN_POINT ( 'NONE',  ( 7.747891071769697824, -78.80404215024988446, -5.053095730781000050 ) ) ;
#9373 = CARTESIAN_POINT ( 'NONE',  ( 8.852642474645792348, -77.09067155497332635, -8.178101815369201333 ) ) ;
#9374 = EDGE_CURVE ( 'NONE', #31775, #13118, #8329, .T. ) ;
#9375 = CARTESIAN_POINT ( 'NONE',  ( -9.650948395506999233, -24.93402498662999989, 8.252474012539000370 ) ) ;
#9376 = CARTESIAN_POINT ( 'NONE',  ( -14.00000000000000000, -9.295797029142999435, 0.000000000000000000 ) ) ;
#9377 = CARTESIAN_POINT ( 'NONE',  ( -4.658611238344869676, -77.68345333943109665, -8.082910578726778539 ) ) ;
#9378 = CARTESIAN_POINT ( 'NONE',  ( 0.000000000000000000, -86.20000000000000284, 0.000000000000000000 ) ) ;
#9379 = CARTESIAN_POINT ( 'NONE',  ( -2.360708107464999816, -80.24142549782600042, -3.389035370063000041 ) ) ;
#9380 = CARTESIAN_POINT ( 'NONE',  ( -1.281965430112000037, -77.30751332859900060, -9.567121928242999118 ) ) ;
#9381 = CARTESIAN_POINT ( 'NONE',  ( -1.750000000001000089, -56.04922971509999741, 12.60356226394999979 ) ) ;
#9382 = DIRECTION ( 'NONE',  ( -0.7071067811865475727, 0.000000000000000000, 0.7071067811865475727 ) ) ;
#9383 = CARTESIAN_POINT ( 'NONE',  ( -1.484804496640999893, -24.71869153383000040, 12.77261165608999960 ) ) ;
#9384 = CARTESIAN_POINT ( 'NONE',  ( 10.12290050256999940, -18.75000002239000096, 7.648026768411000376 ) ) ;
#9385 = CARTESIAN_POINT ( 'NONE',  ( 2.479132830488999684, -1.786791850769000156, 2.865938273056999996 ) ) ;
#9386 = CARTESIAN_POINT ( 'NONE',  ( -0.7681833999686477066, -80.92708333333332860, 0.9995835529977223910 ) ) ;
#9387 = ADVANCED_FACE ( 'NONE', ( #6326 ), #47009, .F. ) ;
#9388 = CYLINDRICAL_SURFACE ( 'NONE', #9534, 1.250000000000000000 ) ;
#9389 = CARTESIAN_POINT ( 'NONE',  ( -1.546786622596739047, -80.35334782346511417, -0.08660658759117148553 ) ) ;
#9390 = CARTESIAN_POINT ( 'NONE',  ( -0.1873428942460613755, -78.48719004869164451, 1.238278019793636942 ) ) ;
#9391 = CARTESIAN_POINT ( 'NONE',  ( 10.75000000000000000, -80.25000000000000000, -1.651583051307000043E-14 ) ) ;
#9392 = CARTESIAN_POINT ( 'NONE',  ( -10.18491080493000212, -23.30716680861999990, -7.640030264156999706 ) ) ;
#9393 = CARTESIAN_POINT ( 'NONE',  ( -6.189430218157277785, -77.37374590179841505, 8.895180375493302094 ) ) ;
#9394 = DIRECTION ( 'NONE',  ( -1.000000000000000000, 0.000000000000000000, 0.000000000000000000 ) ) ;
#9395 = VECTOR ( 'NONE', #1714, 1000.000000000000114 ) ;
#9397 = CARTESIAN_POINT ( 'NONE',  ( -1.021885754039999927, -78.85826102536199755, -0.9827557610011000699 ) ) ;
#9396 = CARTESIAN_POINT ( 'NONE',  ( -13.79999999999999893, 0.000000000000000000, 0.000000000000000000 ) ) ;
#9398 = CARTESIAN_POINT ( 'NONE',  ( 0.000000000000000000, -74.99999999999998579, 0.000000000000000000 ) ) ;
#9399 = ORIENTED_EDGE ( 'NONE', *, *, #32337, .F. ) ;
#9400 = CARTESIAN_POINT ( 'NONE',  ( -2.308176599197000023, -83.59657450217399344, -2.748828535461000033 ) ) ;
#9401 = CARTESIAN_POINT ( 'NONE',  ( 9.651204802600000576, -80.43314977265349341, 5.628321366006999504 ) ) ;
#9402 = CARTESIAN_POINT ( 'NONE',  ( -14.00000000000000000, -0.2000000000000005107, 0.000000000000000000 ) ) ;
#9403 = CARTESIAN_POINT ( 'NONE',  ( -3.366989981489502348, -84.75104167658417964, -0.7261064475801897178 ) ) ;
#9404 = CARTESIAN_POINT ( 'NONE',  ( 8.196653188619999142, -77.64368766097399543, 7.657217973713000170 ) ) ;
#9405 = FACE_OUTER_BOUND ( 'NONE', #25675, .T. ) ;
#9406 = CARTESIAN_POINT ( 'NONE',  ( 9.401690036064000111, -79.05816318924999564, -2.543243121375000193 ) ) ;
#9407 = AXIS2_PLACEMENT_3D ( 'NONE', #5695, #23704, #1580 ) ;
#9408 = CARTESIAN_POINT ( 'NONE',  ( 2.850509184763999837, -1.027515194441000146, 2.608524172722999968 ) ) ;
#9409 = CARTESIAN_POINT ( 'NONE',  ( 7.958776490642000212, -61.27699850017000216, -9.723157983989999309 ) ) ;
#9410 = CARTESIAN_POINT ( 'NONE',  ( -8.872958366221523008, -61.81010144656713123, 8.813896669733001232 ) ) ;
#9411 = DIRECTION ( 'NONE',  ( -0.9998748951565024079, 0.000000000000000000, -0.01581752306063006000 ) ) ;
#9412 = ORIENTED_EDGE ( 'NONE', *, *, #16899, .T. ) ;
#9413 = DIRECTION ( 'NONE',  ( 0.7071067811865475727, 0.000000000000000000, -0.7071067811865475727 ) ) ;
#9414 = AXIS2_PLACEMENT_3D ( 'NONE', #19290, #27833, #42015 ) ;
#9415 = LINE ( 'NONE', #41286, #42985 ) ;
#9416 = CYLINDRICAL_SURFACE ( 'NONE', #51696, 0.5000000000000000000 ) ;
#9417 = CARTESIAN_POINT ( 'NONE',  ( -0.9218200799623714747, -81.47291666666669130, -1.199500263597270466 ) ) ;
#9418 = CARTESIAN_POINT ( 'NONE',  ( -12.50485633186319490, -17.13407854666478514, -0.6924329881533773934 ) ) ;
#9419 = CARTESIAN_POINT ( 'NONE',  ( 11.00000000000000000, -23.75000000000000000, -1.203259120426999909E-14 ) ) ;
#9420 = VERTEX_POINT ( 'NONE', #479 ) ;
#9421 = CARTESIAN_POINT ( 'NONE',  ( 10.12378227972000033, -78.20771289290198069, -4.818073696357999758 ) ) ;
#9422 = CARTESIAN_POINT ( 'NONE',  ( 10.18248259422395385, -61.09095036164143266, -7.792398156856013891 ) ) ;
#9423 = ORIENTED_EDGE ( 'NONE', *, *, #31123, .T. ) ;
#9424 = ADVANCED_FACE ( 'NONE', ( #14884 ), #19617, .F. ) ;
#9425 = ORIENTED_EDGE ( 'NONE', *, *, #5504, .F. ) ;
#9426 = CARTESIAN_POINT ( 'NONE',  ( -13.86363636363000218, -9.638971321655001034, -1.277887488715999925E-05 ) ) ;
#9427 = FILL_AREA_STYLE_COLOUR ( '', #24685 ) ;
#9428 = CARTESIAN_POINT ( 'NONE',  ( 9.202039358297998461, -80.28029040626950064, 2.360608321670000453 ) ) ;
#9429 = ORIENTED_EDGE ( 'NONE', *, *, #40075, .T. ) ;
#9430 = CARTESIAN_POINT ( 'NONE',  ( -6.111832503000000472, -76.17462612386199794, 10.87001744695999861 ) ) ;
#9431 = CYLINDRICAL_SURFACE ( 'NONE', #40935, 1.750000000000001332 ) ;
#9432 = VECTOR ( 'NONE', #45998, 1000.000000000000000 ) ;
#9433 = CARTESIAN_POINT ( 'NONE',  ( 1.409966096066999963, -77.98898218165999197, 0.6064444106313999772 ) ) ;
#9434 = CARTESIAN_POINT ( 'NONE',  ( 8.256620083228000340, -77.27884805011498770, -4.688888258373000717 ) ) ;
#9435 = CARTESIAN_POINT ( 'NONE',  ( 0.8901331092129259881, -80.28864483123025764, -0.8771058481484877989 ) ) ;
#9436 = CARTESIAN_POINT ( 'NONE',  ( 11.98112765039999950, -78.27769171769000423, 5.330601325896000553 ) ) ;
#9437 = CARTESIAN_POINT ( 'NONE',  ( -6.043427764450786555, -78.88333333333333997, -10.48543666025110177 ) ) ;
#9438 = CARTESIAN_POINT ( 'NONE',  ( -6.766389538252999714, -77.81360028145363117, -6.956053621355001049 ) ) ;
#9439 = CARTESIAN_POINT ( 'NONE',  ( 8.220005723591295776, -79.88839068397346921, 4.241318902065857266 ) ) ;
#9440 = CARTESIAN_POINT ( 'NONE',  ( 11.75000000000000000, -78.04999999999999716, 0.000000000000000000 ) ) ;
#9441 = ORIENTED_EDGE ( 'NONE', *, *, #23257, .F. ) ;
#9442 = FACE_OUTER_BOUND ( 'NONE', #58115, .T. ) ;
#9443 = ADVANCED_FACE ( 'NONE', ( #23456 ), #49821, .F. ) ;
#9444 = CARTESIAN_POINT ( 'NONE',  ( 11.05577208806000122, -76.76861526166000260, -4.921212746988999243 ) ) ;
#9445 = CARTESIAN_POINT ( 'NONE',  ( 0.2296925013217000211, -80.48978759434999120, -1.498727297740999775 ) ) ;
#9446 = AXIS2_PLACEMENT_3D ( 'NONE', #34014, #33728, #34874 ) ;
#9447 = B_SPLINE_SURFACE_WITH_KNOTS ( 'NONE', 3, 3, ( 
 ( #22541, #144, #17523, #21942 ),
 ( #58263, #22239, #31375, #4832 ),
 ( #57968, #45579, #18122, #26369 ),
 ( #23122, #53541, #437, #17825 ),
 ( #13673, #54134, #724, #18413 ),
 ( #35812, #49418, #18701, #13081 ),
 ( #53247, #50007, #36404, #54432 ),
 ( #49716, #48828, #8966, #30796 ),
 ( #8370, #45284, #31964, #44388 ),
 ( #4240, #8667, #3940, #35513 ),
 ( #26653, #40252, #26951, #44984 ) ),
 .UNSPECIFIED., .F., .F., .F.,
 ( 4, 1, 1, 1, 1, 1, 1, 1, 4 ),
 ( 4, 4 ),
 ( -0.02001211456244999728, 0.000000000000000000, 0.1666666666667000196, 0.3333333333333000081, 0.5000000000000000000, 0.6666666666667000474, 0.8333333333333000637, 1.000000000000000000, 1.020273719995999917 ),
 ( -0.3582002740325999635, 1.358863140973999961 ),
 .UNSPECIFIED. ) ;
#9448 = CARTESIAN_POINT ( 'NONE',  ( -1.295285823243000012, -78.17326554362610125, -0.2505997727336000125 ) ) ;
#9449 = CARTESIAN_POINT ( 'NONE',  ( 2.836926435089343723, -3.149705295855155018, 2.084417755536846606 ) ) ;
#9450 = AXIS2_PLACEMENT_3D ( 'NONE', #12323, #22568, #50322 ) ;
#9451 = CARTESIAN_POINT ( 'NONE',  ( 8.292771711479000274, -61.85529938492000213, -9.770424367394999976 ) ) ;
#9452 = CARTESIAN_POINT ( 'NONE',  ( -4.802691730569000228, -78.42489718999000559, 11.09149278351999968 ) ) ;
#9453 = LINE ( 'NONE', #9159, #51768 ) ;
#9454 = CARTESIAN_POINT ( 'NONE',  ( 4.099999999699000419, -75.20000000030088927, -8.298664203784000017E-10 ) ) ;
#9455 = CARTESIAN_POINT ( 'NONE',  ( 7.170910619513000128, -77.68846498579799231, 6.587124128982000393 ) ) ;
#9456 = CARTESIAN_POINT ( 'NONE',  ( 2.148140615799914777, -77.18924137040484368, -11.93000460038572719 ) ) ;
#9457 = DIRECTION ( 'NONE',  ( 0.7071067811865475727, 0.000000000000000000, -0.7071067811865475727 ) ) ;
#9458 = ADVANCED_FACE ( 'NONE', ( #41468 ), #21402, .F. ) ;
#9459 = VERTEX_POINT ( 'NONE', #48729 ) ;
#9460 = CARTESIAN_POINT ( 'NONE',  ( -0.6256353049379000941, -82.80061671381200483, 1.457043991488000012 ) ) ;
#9461 = CARTESIAN_POINT ( 'NONE',  ( -11.75000000000000355, -77.81041666666666856, -1.538071403320004249 ) ) ;
#9462 = CARTESIAN_POINT ( 'NONE',  ( -0.9995835529977281642, -79.44791666666662877, 0.7681833999686391579 ) ) ;
#9463 = CARTESIAN_POINT ( 'NONE',  ( -11.61454496413000115, -77.47861567637899327, 2.935712811417999557 ) ) ;
#9464 = CARTESIAN_POINT ( 'NONE',  ( 9.089938076053588389, -77.00000000000001421, 2.444550776227857991 ) ) ;
#9465 = CARTESIAN_POINT ( 'NONE',  ( 8.321246128606000880, -78.19452423951800313, -8.715080868295999039 ) ) ;
#9466 = CARTESIAN_POINT ( 'NONE',  ( 8.384816012895999648, -78.77769805011500637, -4.923277454554000343 ) ) ;
#9467 = CARTESIAN_POINT ( 'NONE',  ( -7.784718833714999064, -77.65684236001300178, 5.670217160303000270 ) ) ;
#9468 = CARTESIAN_POINT ( 'NONE',  ( 4.515762143495796188, -76.04307832163055991, 10.84725862635628602 ) ) ;
#9469 = CARTESIAN_POINT ( 'NONE',  ( -11.01515889844999840, -78.95448538877499800, 0.6066373079611000474 ) ) ;
#9470 = CARTESIAN_POINT ( 'NONE',  ( -0.4881686207928203070, -86.02148120184399716, 3.925966920820129769 ) ) ;
#9471 = VERTEX_POINT ( 'NONE', #52864 ) ;
#9472 = CARTESIAN_POINT ( 'NONE',  ( 7.568503529865000523, -76.37230738176410227, 9.708412483427999007 ) ) ;
#9473 = CARTESIAN_POINT ( 'NONE',  ( -3.777881228421892335, -78.40681307243319509, 0.07122045777464609817 ) ) ;
#9474 = AXIS2_PLACEMENT_3D ( 'NONE', #10433, #19292, #37284 ) ;
#9475 = CARTESIAN_POINT ( 'NONE',  ( 4.038786804788999873, -79.64544187509899587, -10.20549938643999965 ) ) ;
#9476 = CARTESIAN_POINT ( 'NONE',  ( 10.61050599188999932, -77.92876026662598576, -2.901234667509999809 ) ) ;
#9477 = CARTESIAN_POINT ( 'NONE',  ( -10.99961599049050953, -80.09872922184305821, 0.2432713142634969350 ) ) ;
#9478 = CARTESIAN_POINT ( 'NONE',  ( 1.209853131585020947, -79.32753753103162353, -0.3581602740580526190 ) ) ;
#9479 = DIRECTION ( 'NONE',  ( 0.000000000000000000, -1.000000000000000000, 0.000000000000000000 ) ) ;
#9480 = B_SPLINE_CURVE_WITH_KNOTS ( 'NONE', 3,
 ( #18353, #8608, #36343, #5347, #13910, #49355, #5063, #23356, #31904, #27476, #50234, #662, #32192, #17765, #54075, #31022, #27770, #31609 ),
 .UNSPECIFIED., .F., .F.,
 ( 4, 2, 2, 2, 2, 2, 2, 2, 4 ),
 ( 0.000000000000000000, 0.1250000000000000000, 0.2500000000000000000, 0.3750000000000000000, 0.5000000000000000000, 0.6250000000000000000, 0.7500000000000000000, 0.8750000000000000000, 1.000000000000000000 ),
 .UNSPECIFIED. ) ;
#9481 = ORIENTED_EDGE ( 'NONE', *, *, #26362, .T. ) ;
#9482 = CARTESIAN_POINT ( 'NONE',  ( -11.13008859988999966, -78.70448538877499800, 0.6129668257943999832 ) ) ;
#9483 = FACE_BOUND ( 'NONE', #35414, .T. ) ;
#9484 = CARTESIAN_POINT ( 'NONE',  ( 4.254218938430716079, -79.70414273500806246, -11.04225118825767993 ) ) ;
#9485 = CARTESIAN_POINT ( 'NONE',  ( 2.024107789166968985, -78.48547957940617437, 3.504731411014806230 ) ) ;
#9487 = CARTESIAN_POINT ( 'NONE',  ( 12.55433072267388894, -60.18725213688288989, 1.749897784984624005 ) ) ;
#9486 = CARTESIAN_POINT ( 'NONE',  ( -0.8625730533285999035, -81.22635005938499830, -0.9982651640015999250 ) ) ;
#9488 = CARTESIAN_POINT ( 'NONE',  ( -8.035240866938249127, -76.44166666666666288, 7.229432123683928069 ) ) ;
#9489 = PLANE ( 'NONE',  #20495 ) ;
#9490 = EDGE_CURVE ( 'NONE', #48229, #45641, #48883, .T. ) ;
#9491 = CIRCLE ( 'NONE', #37759, 11.65000000000000036 ) ;
#9492 = DIRECTION ( 'NONE',  ( 0.000000000000000000, 1.000000000000000000, 0.000000000000000000 ) ) ;
#9493 = EDGE_CURVE ( 'NONE', #39575, #3891, #24364, .T. ) ;
#9494 = CARTESIAN_POINT ( 'NONE',  ( 8.838834764832000701, -23.25000000000000000, 8.838834764832000701 ) ) ;
#9495 = CARTESIAN_POINT ( 'NONE',  ( -12.43646324844999995, -24.92048514568000073, 0.1256879863178999857 ) ) ;
#9496 = ORIENTED_EDGE ( 'NONE', *, *, #14112, .T. ) ;
#9497 = ORIENTED_EDGE ( 'NONE', *, *, #7745, .F. ) ;
#9498 = CARTESIAN_POINT ( 'NONE',  ( 10.63720963964777688, -78.83845499315577854, -1.560381659779633168 ) ) ;
#9499 = CARTESIAN_POINT ( 'NONE',  ( -5.413884141668839689, -77.68335102312344986, -9.393024699257772170 ) ) ;
#9500 = ORIENTED_EDGE ( 'NONE', *, *, #46706, .F. ) ;
#9501 = CARTESIAN_POINT ( 'NONE',  ( 7.597989044191865382, -76.06501007995230168, 8.084992307224259989 ) ) ;
#9502 = CARTESIAN_POINT ( 'NONE',  ( 9.992017125381000398, -24.16084087012999859, 7.762968460669999793 ) ) ;
#9503 = CARTESIAN_POINT ( 'NONE',  ( 8.188293269190999979, -61.50494400535999517, 9.395718629102999486 ) ) ;
#9504 = CARTESIAN_POINT ( 'NONE',  ( -2.562437971592963937, -76.44121971063705701, 11.92753260506139057 ) ) ;
#9505 = CARTESIAN_POINT ( 'NONE',  ( 8.941640842993423988, -78.85745151639218875, 7.898998304516130275 ) ) ;
#9506 = CARTESIAN_POINT ( 'NONE',  ( 3.507155896972999898, -79.11580003895399216, 10.65448112794999957 ) ) ;
#9507 = LINE ( 'NONE', #50252, #42203 ) ;
#9508 = VERTEX_POINT ( 'NONE', #7698 ) ;
#9509 = CARTESIAN_POINT ( 'NONE',  ( 7.764010764072387438, -60.92280919713373777, -9.931043767944542466 ) ) ;
#9510 = AXIS2_PLACEMENT_3D ( 'NONE', #13168, #9055, #40345 ) ;
#9511 = EDGE_LOOP ( 'NONE', ( #57928, #47001, #26601, #18869 ) ) ;
#9512 = EDGE_CURVE ( 'NONE', #10113, #25387, #43245, .T. ) ;
#9513 = CARTESIAN_POINT ( 'NONE',  ( 2.816423976644823579, -77.45055722664174880, 8.810706099923065082 ) ) ;
#9514 = CARTESIAN_POINT ( 'NONE',  ( 10.42639159904000046, -77.16057625750279669, -2.617796444239999687 ) ) ;
#9515 = CARTESIAN_POINT ( 'NONE',  ( 0.000000000000000000, -32.88214388149999934, 0.000000000000000000 ) ) ;
#9516 = CARTESIAN_POINT ( 'NONE',  ( -5.159044788988000008, -77.41054617377999136, -8.219183903844999861 ) ) ;
#9517 = CARTESIAN_POINT ( 'NONE',  ( -10.11336291351999961, -76.36473582389999137, 8.113742140220999488 ) ) ;
#9518 = CARTESIAN_POINT ( 'NONE',  ( -12.00000000000000178, -78.41041666666667709, -1.570796326794897668 ) ) ;
#9519 = CARTESIAN_POINT ( 'NONE',  ( -1.462188802161999979, -79.36578967391999129, -0.7147474581103999691 ) ) ;
#9520 = LINE ( 'NONE', #31051, #54456 ) ;
#9521 = CARTESIAN_POINT ( 'NONE',  ( 10.70874647057999951, -79.16278856042799816, -2.238429218213000116 ) ) ;
#9522 = CARTESIAN_POINT ( 'NONE',  ( 12.70249480710770662, -61.76498603277217825, 0.9989402949278443078 ) ) ;
#9523 = CARTESIAN_POINT ( 'NONE',  ( -8.111636311560200596, -60.31614597267139999, 7.429974109843835883 ) ) ;
#9524 = ADVANCED_FACE ( 'NONE', ( #52579 ), #34547, .F. ) ;
#9525 = CARTESIAN_POINT ( 'NONE',  ( 0.2517727111220999792, -84.90343479341399302, -3.580552409225000066 ) ) ;
#9526 = ORIENTED_EDGE ( 'NONE', *, *, #1459, .F. ) ;
#9527 = CARTESIAN_POINT ( 'NONE',  ( 11.10214774708000007, -79.58624754497100184, -5.597531737657999606 ) ) ;
#9528 = AXIS2_PLACEMENT_3D ( 'NONE', #24732, #55445, #46902 ) ;
#9529 = CARTESIAN_POINT ( 'NONE',  ( -9.420416572830998092, -76.25741179485200405, -6.585164207577999917 ) ) ;
#9530 = CARTESIAN_POINT ( 'NONE',  ( -7.628363392376307672, -78.03778907345090943, 7.574339073857688120 ) ) ;
#9531 = ADVANCED_FACE ( 'NONE', ( #30693 ), #34834, .F. ) ;
#9532 = CARTESIAN_POINT ( 'NONE',  ( -0.7928179559538000021, -78.75362403072900008, -11.95355612866999984 ) ) ;
#9533 = FACE_OUTER_BOUND ( 'NONE', #7312, .T. ) ;
#9534 = AXIS2_PLACEMENT_3D ( 'NONE', #46295, #32668, #23536 ) ;
#9536 = DIRECTION ( 'NONE',  ( 1.000000000000000000, 0.000000000000000000, 0.000000000000000000 ) ) ;
#9535 = CARTESIAN_POINT ( 'NONE',  ( -9.396085398178614767, -78.35208333333332575, -7.220923959705254802 ) ) ;
#9537 = CARTESIAN_POINT ( 'NONE',  ( 3.106054555984999688, -86.09999999999999432, -1.382904586457999851 ) ) ;
#9538 = CARTESIAN_POINT ( 'NONE',  ( 7.849383194069857517, -80.91008263851306026, 7.345942549935802646 ) ) ;
#9539 = CARTESIAN_POINT ( 'NONE',  ( -8.334831687997999339, -78.04071980276798115, 4.375131454052000102 ) ) ;
#9540 = CARTESIAN_POINT ( 'NONE',  ( 0.3550910806849119639, -85.83735717367099483, -7.926401815244934923 ) ) ;
#9541 = CARTESIAN_POINT ( 'NONE',  ( 6.099615176083999835, -78.63114111160000164, -9.019941877331000057 ) ) ;
#9542 = CARTESIAN_POINT ( 'NONE',  ( 11.90625000002000000, -76.20625000001498961, 3.701036097655999965E-09 ) ) ;
#9543 = CARTESIAN_POINT ( 'NONE',  ( -10.27832156847999912, -80.35961828462440337, 4.298059050626999777 ) ) ;
#9544 = EDGE_LOOP ( 'NONE', ( #31909, #53058, #49252, #32266 ) ) ;
#9545 = FACE_OUTER_BOUND ( 'NONE', #7025, .T. ) ;
#9546 = CARTESIAN_POINT ( 'NONE',  ( 6.214091009702999102, -77.83177403538302030, -7.179311535718999160 ) ) ;
#9547 = CARTESIAN_POINT ( 'NONE',  ( -1.269242897982000073, -1.816486014851000030, -3.588396222942000335 ) ) ;
#9548 = CARTESIAN_POINT ( 'NONE',  ( 5.151324428776999476, -77.53534689742400587, 9.964033682248000900 ) ) ;
#9549 = CARTESIAN_POINT ( 'NONE',  ( 2.879226727952094222, -79.84583333333331723, -10.71369944335146940 ) ) ;
#9550 = CARTESIAN_POINT ( 'NONE',  ( 5.299999999999999822, -75.00000000000000000, 0.000000000000000000 ) ) ;
#9551 = CARTESIAN_POINT ( 'NONE',  ( 0.000000000000000000, -75.19999999999998863, 0.000000000000000000 ) ) ;
#9552 = CARTESIAN_POINT ( 'NONE',  ( 2.865789910122292561, -79.75000000000000000, -8.824825250167616986 ) ) ;
#9553 = CARTESIAN_POINT ( 'NONE',  ( 0.000000000000000000, -77.50000000000000000, 0.000000000000000000 ) ) ;
#9554 = CARTESIAN_POINT ( 'NONE',  ( 1.289254494606999923, -84.23117953870900010, 3.967917333274999958 ) ) ;
#9555 = EDGE_CURVE ( 'NONE', #35383, #5753, #30937, .T. ) ;
#9556 = CARTESIAN_POINT ( 'NONE',  ( 5.246383657897999875, -77.46100733245999947, -10.79237965019999912 ) ) ;
#9557 = CARTESIAN_POINT ( 'NONE',  ( 9.205836503685999261, -53.79200673903999785, -8.541144771039000716 ) ) ;
#9558 = CARTESIAN_POINT ( 'NONE',  ( 9.608679508909999001, -77.00116639950799424, 5.650475968096999146 ) ) ;
#9559 = CARTESIAN_POINT ( 'NONE',  ( 0.8512149552595998925, -80.04349795635999953, 1.432023780608000063 ) ) ;
#9560 = CARTESIAN_POINT ( 'NONE',  ( -0.8715281638271999975, -78.31589177200999075, 1.280679076496999969 ) ) ;
#9561 = CARTESIAN_POINT ( 'NONE',  ( 0.2584144823669621838, -62.02845396880400841, 12.70558781493838296 ) ) ;
#9562 = CARTESIAN_POINT ( 'NONE',  ( -1.499047393880830858, -83.23987833091183575, 0.1907839512157355755 ) ) ;
#9563 = DIRECTION ( 'NONE',  ( 0.000000000000000000, 1.000000000000000000, 0.000000000000000000 ) ) ;
#9564 = CARTESIAN_POINT ( 'NONE',  ( -10.74981572755469550, -80.10331782357827990, -0.4067125980479509018 ) ) ;
#9565 = FACE_OUTER_BOUND ( 'NONE', #43200, .T. ) ;
#9566 = EDGE_CURVE ( 'NONE', #16901, #45372, #14946, .T. ) ;
#9567 = VERTEX_POINT ( 'NONE', #26274 ) ;
#9568 = EDGE_CURVE ( 'NONE', #35685, #14936, #50795, .T. ) ;
#9569 = CARTESIAN_POINT ( 'NONE',  ( 11.00000000000000000, -79.44999999999998863, 0.000000000000000000 ) ) ;
#9570 = CARTESIAN_POINT ( 'NONE',  ( 6.277205522164990725, -79.03065722717676067, 10.03106614420215337 ) ) ;
#9571 = CARTESIAN_POINT ( 'NONE',  ( -8.320158381697998706, -78.76455857394600457, 7.590054615178000397 ) ) ;
#9572 = CARTESIAN_POINT ( 'NONE',  ( 8.190859204290999784, -55.64999999967000122, 7.342331066867000544 ) ) ;
#9573 = ORIENTED_EDGE ( 'NONE', *, *, #26432, .T. ) ;
#9574 = VERTEX_POINT ( 'NONE', #49014 ) ;
#9575 = CARTESIAN_POINT ( 'NONE',  ( -1.453051419519999943, -80.51449613900899749, -0.4232133907648999993 ) ) ;
#9576 = CIRCLE ( 'NONE', #21812, 14.00000000000000000 ) ;
#9577 = EDGE_LOOP ( 'NONE', ( #32034, #30884, #15305, #35897 ) ) ;
#9578 = ORIENTED_EDGE ( 'NONE', *, *, #32734, .T. ) ;
#9579 = CIRCLE ( 'NONE', #18976, 1.000000000000000000 ) ;
#9580 = CARTESIAN_POINT ( 'NONE',  ( 12.00000000000000000, -23.15000000000000213, 0.000000000000000000 ) ) ;
#9581 = DIRECTION ( 'NONE',  ( 0.000000000000000000, 0.7071067811866525998, -0.7071067811864425456 ) ) ;
#9582 = CARTESIAN_POINT ( 'NONE',  ( -2.725819353531988121, -80.35729165740173130, -2.104322176367662056 ) ) ;
#9583 = CARTESIAN_POINT ( 'NONE',  ( 1.814305421036000121, -24.28941969330999839, -12.78003582253000125 ) ) ;
#9584 = CARTESIAN_POINT ( 'NONE',  ( -1.208807979972000179, -82.18132306546799271, -3.379724958325999840 ) ) ;
#9585 = LINE ( 'NONE', #27569, #32883 ) ;
#9586 = CARTESIAN_POINT ( 'NONE',  ( -1.269878056453999982, -78.86088029460999849, -11.84562412616999971 ) ) ;
#9587 = ORIENTED_EDGE ( 'NONE', *, *, #24546, .T. ) ;
#9588 = ORIENTED_EDGE ( 'NONE', *, *, #17784, .T. ) ;
#9589 = CARTESIAN_POINT ( 'NONE',  ( -7.624341766647000362, -18.73514853758999976, 10.42531125024999916 ) ) ;
#9590 = CYLINDRICAL_SURFACE ( 'NONE', #36663, 1.500000000000000000 ) ;
#9591 = CARTESIAN_POINT ( 'NONE',  ( 1.092232985442820992, -81.29166666666665719, 0.6295237254636267821 ) ) ;
#9592 = CARTESIAN_POINT ( 'NONE',  ( -1.319155384867000125, -80.25392490671100632, 0.1959724986398999891 ) ) ;
#9593 = CARTESIAN_POINT ( 'NONE',  ( -0.1538805260928999830, -78.08580753804999119, 9.702939253146000809 ) ) ;
#9594 = CARTESIAN_POINT ( 'NONE',  ( -1.164828128805999992E-14, -72.75000000040999737, 0.000000000000000000 ) ) ;
#9595 = CARTESIAN_POINT ( 'NONE',  ( -3.474676814090385424, -86.08685047304777527, 2.030121440354399898 ) ) ;
#9596 = CARTESIAN_POINT ( 'NONE',  ( 5.555615362064000529, -77.25827452080000057, 11.70460571637999969 ) ) ;
#9597 = CARTESIAN_POINT ( 'NONE',  ( -1.322249586278000155, -79.59655133345999900, -0.2786171024073000324 ) ) ;
#9598 = CARTESIAN_POINT ( 'NONE',  ( -12.64500484462999985, -22.77152778045000048, -1.799490225533999732 ) ) ;
#9599 = DIRECTION ( 'NONE',  ( 1.000000000000000000, 0.000000000000000000, 0.000000000000000000 ) ) ;
#9600 =( GEOMETRIC_REPRESENTATION_CONTEXT ( 3 ) GLOBAL_UNCERTAINTY_ASSIGNED_CONTEXT ( ( #47299 ) ) GLOBAL_UNIT_ASSIGNED_CONTEXT ( ( #5710, #24311, #37293 ) ) REPRESENTATION_CONTEXT ( 'NONE', 'WORKASPACE' ) );
#9601 = CARTESIAN_POINT ( 'NONE',  ( -4.094489195923999958, -78.73368213548981487, -0.8029745938706001063 ) ) ;
#9602 = CARTESIAN_POINT ( 'NONE',  ( -0.9849936891751999157, -80.88413894626904721, -11.22225356808999841 ) ) ;
#9603 = CARTESIAN_POINT ( 'NONE',  ( 4.581254438705999910, -78.73486001420198477, -8.535416510302999527 ) ) ;
#9604 = LINE ( 'NONE', #27590, #5999 ) ;
#9605 = CARTESIAN_POINT ( 'NONE',  ( 3.262642866299000133, -82.36630496681199531, -1.391542130826000090 ) ) ;
#9607 = CARTESIAN_POINT ( 'NONE',  ( -0.1120320062231000002, -77.88396805135350576, -1.328911429676000067 ) ) ;
#9606 = CARTESIAN_POINT ( 'NONE',  ( 1.250000000000000000, -79.25000000000000000, 0.000000000000000000 ) ) ;
#9608 = DIRECTION ( 'NONE',  ( 0.000000000000000000, -1.000000000000000000, 0.000000000000000000 ) ) ;
#9609 = CARTESIAN_POINT ( 'NONE',  ( 5.365883907697000410, -80.23717621672710720, 9.905345355165000143 ) ) ;
#9610 = CARTESIAN_POINT ( 'NONE',  ( 1.217465845835394855, -79.22916666666665719, -0.3271848554490981997 ) ) ;
#9611 = ORIENTED_EDGE ( 'NONE', *, *, #15089, .T. ) ;
#9612 = DIRECTION ( 'NONE',  ( 0.000000000000000000, -1.000000000000000000, 0.000000000000000000 ) ) ;
#9613 = CARTESIAN_POINT ( 'NONE',  ( 11.03313550157999856, -78.37214908313399064, 0.1851758569619000039 ) ) ;
#9614 = DIRECTION ( 'NONE',  ( 0.000000000000000000, -1.000000000000000000, 0.000000000000000000 ) ) ;
#9615 = CARTESIAN_POINT ( 'NONE',  ( 0.9432352957733999288, -82.03436888729800103, 0.9428059748164999698 ) ) ;
#9616 = CARTESIAN_POINT ( 'NONE',  ( 1.799490225533999732, -56.02847221959000024, 12.64500484464000074 ) ) ;
#9617 = CARTESIAN_POINT ( 'NONE',  ( -3.346450045594000056, -76.87836363489999769, 12.57540552286999791 ) ) ;
#9618 = CARTESIAN_POINT ( 'NONE',  ( -3.790933506348975524, -79.50381487114017887, 10.05939893380695516 ) ) ;
#9619 = AXIS2_PLACEMENT_3D ( 'NONE', #33801, #23789, #41804 ) ;
#9620 = EDGE_CURVE ( 'NONE', #40940, #45319, #44008, .T. ) ;
#9621 = CARTESIAN_POINT ( 'NONE',  ( -2.355755099258999508, -79.46556001420199777, 9.223161221019999800 ) ) ;
#9622 = CARTESIAN_POINT ( 'NONE',  ( -0.4750644714246999856, -76.61635661117000495, -12.50333200011000123 ) ) ;
#9623 = ORIENTED_EDGE ( 'NONE', *, *, #42368, .F. ) ;
#9624 = CARTESIAN_POINT ( 'NONE',  ( -13.98934701301999972, -69.37813015403000350, -1.420884291397000047E-05 ) ) ;
#9625 = CARTESIAN_POINT ( 'NONE',  ( -2.975062338844999932, -77.84659905823998827, -10.76170074862000092 ) ) ;
#9626 = CARTESIAN_POINT ( 'NONE',  ( -0.6688296391966999099, -81.65955898600100227, 1.127159194743000192 ) ) ;
#9627 = CARTESIAN_POINT ( 'NONE',  ( 7.601397897754999633, -60.04999999657000131, 10.07627163191000008 ) ) ;
#9628 = CARTESIAN_POINT ( 'NONE',  ( 8.774584709929998283, -79.29716346014799910, 3.021992008916999595 ) ) ;
#9630 = CARTESIAN_POINT ( 'NONE',  ( 2.627446458840999810, -1.566251425905000216, 3.037392460054000320 ) ) ;
#9629 = CARTESIAN_POINT ( 'NONE',  ( 3.013671259490000143, -83.94143147127900306, 2.824234233979999953 ) ) ;
#9631 = CARTESIAN_POINT ( 'NONE',  ( -1.799501877793999949, -55.51082276539999327, -12.60552511008000032 ) ) ;
#9632 = CARTESIAN_POINT ( 'NONE',  ( -8.485281374238999419, -18.75000000000000000, -8.485281374238999419 ) ) ;
#9633 = ORIENTED_EDGE ( 'NONE', *, *, #33398, .T. ) ;
#9634 = CARTESIAN_POINT ( 'NONE',  ( 3.266381872689648080, -77.24970252057229914, -10.26631233854832281 ) ) ;
#9635 = B_SPLINE_SURFACE_WITH_KNOTS ( 'NONE', 3, 3, ( 
 ( #11504, #29193, #2356, #47240 ),
 ( #6771, #7062, #24780, #43086 ),
 ( #2644, #56657, #53964, #13501 ),
 ( #35337, #40967, #8787, #49836 ),
 ( #17644, #45704, #4952, #9086 ),
 ( #36528, #31793, #22361, #49236 ),
 ( #4057, #40675, #13201, #22956 ),
 ( #50130, #4664, #27072, #22664 ),
 ( #13792, #9672, #35935, #265 ),
 ( #558, #22061, #18536, #45410 ),
 ( #35634, #18246, #23247, #45112 ),
 ( #9383, #36236, #48943, #54551 ),
 ( #54259, #53362, #40375, #27372 ),
 ( #17348, #14091, #32090, #27662 ),
 ( #5242, #41255, #12910, #30909 ),
 ( #49540, #53662, #8488, #26483 ),
 ( #26778, #44808, #44507, #40068 ) ),
 .UNSPECIFIED., .F., .F., .F.,
 ( 4, 1, 1, 1, 1, 1, 1, 1, 1, 1, 1, 1, 1, 1, 4 ),
 ( 4, 4 ),
 ( -0.01011408452870000106, 0.000000000000000000, 0.08333333333333001192, 0.1666666666667000196, 0.2500000000000000000, 0.3333333333333000081, 0.4166666666666999919, 0.5000000000000000000, 0.5833333333333000637, 0.6666666666667000474, 0.7500000000000000000, 0.8333333333333000637, 0.9166666666667000474, 1.000000000000000000, 1.010362559107000013 ),
 ( -0.3559705546268999710, 1.357612419602000076 ),
 .UNSPECIFIED. ) ;
#9636 = CARTESIAN_POINT ( 'NONE',  ( -0.1963495408493606265, -79.01458333333334849, -1.500000000000000222 ) ) ;
#9637 = ORIENTED_EDGE ( 'NONE', *, *, #39362, .F. ) ;
#9639 = EDGE_CURVE ( 'NONE', #2137, #23895, #20987, .T. ) ;
#9638 = EDGE_LOOP ( 'NONE', ( #5946, #9712, #31842, #53865 ) ) ;
#9640 = CARTESIAN_POINT ( 'NONE',  ( -10.78159125964999987, -79.35724697177198550, 1.856099740267000087 ) ) ;
#9641 = CARTESIAN_POINT ( 'NONE',  ( -10.75000000000000178, -80.49266322307225607, 0.9911140733791250490 ) ) ;
#9642 = EDGE_LOOP ( 'NONE', ( #23737, #38757, #50605, #8701, #16690, #25886 ) ) ;
#9643 = CARTESIAN_POINT ( 'NONE',  ( 9.752895431365999457, -78.82452710374299443, -6.878701514737999290 ) ) ;
#9644 = ORIENTED_EDGE ( 'NONE', *, *, #36687, .T. ) ;
#9645 = ORIENTED_EDGE ( 'NONE', *, *, #38085, .F. ) ;
#9646 = CARTESIAN_POINT ( 'NONE',  ( 0.3737964730420059167, -2.734503530802450122, -3.231708774972011700 ) ) ;
#9647 = EDGE_CURVE ( 'NONE', #33154, #53225, #56722, .T. ) ;
#9648 = CARTESIAN_POINT ( 'NONE',  ( 11.99999999999999822, -78.56041666666666856, 1.570796326794923203 ) ) ;
#9649 = CARTESIAN_POINT ( 'NONE',  ( 9.368176195122705607, -79.16304405940145728, 1.578867174401747064 ) ) ;
#9650 = ADVANCED_FACE ( 'NONE', ( #39849 ), #37532, .F. ) ;
#9651 = ORIENTED_EDGE ( 'NONE', *, *, #787, .F. ) ;
#9652 = CARTESIAN_POINT ( 'NONE',  ( -9.431004454403218773, -53.99940410528813572, -8.251853356944486961 ) ) ;
#9653 = ORIENTED_EDGE ( 'NONE', *, *, #39686, .F. ) ;
#9654 = CARTESIAN_POINT ( 'NONE',  ( -1.018293611623504402, -80.09882820534807024, 0.7672941069546416193 ) ) ;
#9655 = AXIS2_PLACEMENT_3D ( 'NONE', #3546, #21549, #12686 ) ;
#9656 = CARTESIAN_POINT ( 'NONE',  ( 2.273238512818713808, -78.91452044229970397, -3.936100221940973309 ) ) ;
#9657 = DIRECTION ( 'NONE',  ( 0.000000000000000000, 0.000000000000000000, 1.000000000000000000 ) ) ;
#9658 = CARTESIAN_POINT ( 'NONE',  ( -1.963210506780999953, -76.37706369595299805, -11.00998129987999974 ) ) ;
#9659 = CARTESIAN_POINT ( 'NONE',  ( 10.75000000000000000, -78.75000000000000000, 0.000000000000000000 ) ) ;
#9660 = CARTESIAN_POINT ( 'NONE',  ( -3.075537641221584018, -78.69583333333332575, 11.44417895085269876 ) ) ;
#9661 = CARTESIAN_POINT ( 'NONE',  ( -11.12866505422999985, -76.33403960801499011, -1.495507578120999881 ) ) ;
#9662 = CARTESIAN_POINT ( 'NONE',  ( -1.723907883222934201, -78.71014354949818426, -9.087954477670448838 ) ) ;
#9663 = DIRECTION ( 'NONE',  ( 0.000000000000000000, 1.000000000000000000, 0.000000000000000000 ) ) ;
#9664 = CARTESIAN_POINT ( 'NONE',  ( 5.165981523686999921, -77.89863501420200009, 7.709125646902999840 ) ) ;
#9665 = FACE_OUTER_BOUND ( 'NONE', #5718, .T. ) ;
#9666 = CARTESIAN_POINT ( 'NONE',  ( 0.000000000000000000, -75.00000000000000000, 0.000000000000000000 ) ) ;
#9667 = CARTESIAN_POINT ( 'NONE',  ( 0.000000000000000000, -75.00000000000000000, -5.300000000000069988 ) ) ;
#9668 = CARTESIAN_POINT ( 'NONE',  ( 2.442096516908000225, -81.92878455456799713, -3.121272388588999913 ) ) ;
#9669 = AXIS2_PLACEMENT_3D ( 'NONE', #9928, #44772, #13754 ) ;
#9670 = CARTESIAN_POINT ( 'NONE',  ( -12.49996905250000090, -18.80797343466000271, 1.666511841114999948 ) ) ;
#9671 = CARTESIAN_POINT ( 'NONE',  ( -8.909545442950999927, -55.64999999967000122, 8.061017305527000687 ) ) ;
#9672 = CARTESIAN_POINT ( 'NONE',  ( -0.005928781627502999370, -25.20113050262999721, 12.66336824419000173 ) ) ;
#9673 = CARTESIAN_POINT ( 'NONE',  ( 10.44683666574804093, -79.24999999999998579, -6.036782287597141305 ) ) ;
#9674 = CARTESIAN_POINT ( 'NONE',  ( -0.3862712429687000237, -78.00000000000000000, 1.188820645369000006 ) ) ;
#9675 = VECTOR ( 'NONE', #12796, 1000.000000000000114 ) ;
#9676 = CARTESIAN_POINT ( 'NONE',  ( 3.756388134018000091, -1.208015194441000251, -0.4997506290278999619 ) ) ;
#9677 = CARTESIAN_POINT ( 'NONE',  ( -8.130811096542000627, -24.68523690389000080, -9.546858433121998999 ) ) ;
#9678 = CARTESIAN_POINT ( 'NONE',  ( 10.07719973194999952, -57.05111654290000445, 7.718346056121999865 ) ) ;
#9679 = CARTESIAN_POINT ( 'NONE',  ( -1.474633671607979091, -79.86749624789827351, -0.3407938052334066326 ) ) ;
#9680 = CARTESIAN_POINT ( 'NONE',  ( 0.000000000000000000, -0.1000000063292999924, 0.000000000000000000 ) ) ;
#9681 = CARTESIAN_POINT ( 'NONE',  ( -0.5999999999999999778, -5.000000000000000000, 4.000000000000000000 ) ) ;
#9682 = CARTESIAN_POINT ( 'NONE',  ( 7.714905556308770507, -79.55033101189913225, -5.543136766205470245 ) ) ;
#9683 = B_SPLINE_CURVE_WITH_KNOTS ( 'NONE', 3,
 ( #2859, #12007, #38574, #43591, #20855, #29986, #16723, #47469, #11723, #16147, #34125, #39151, #21435, #34706, #12288, #34992, #17009, #53023 ),
 .UNSPECIFIED., .F., .F.,
 ( 4, 2, 2, 2, 2, 2, 2, 2, 4 ),
 ( 0.000000000000000000, 0.1250000000000000555, 0.2500000000000001110, 0.3750000000000001665, 0.5000000000000002220, 0.6250000000000002220, 0.7500000000000002220, 0.8750000000000001110, 1.000000000000000000 ),
 .UNSPECIFIED. ) ;
#9684 = CARTESIAN_POINT ( 'NONE',  ( 8.637786863126128978, -77.25138813405403937, 6.437705951042563157 ) ) ;
#9685 = CARTESIAN_POINT ( 'NONE',  ( 7.651147547606000465, -22.76256650325000308, 10.45204383577999963 ) ) ;
#9687 = CARTESIAN_POINT ( 'NONE',  ( -1.377158602743000060, -77.81639593435950530, -0.3366111412210999743 ) ) ;
#9686 = CARTESIAN_POINT ( 'NONE',  ( 0.000000000000000000, -80.79999999999999716, 0.000000000000000000 ) ) ;
#9688 = CARTESIAN_POINT ( 'NONE',  ( 0.3767945000176999848, -81.35074910037999985, -1.540381938526000027 ) ) ;
#9689 = VERTEX_POINT ( 'NONE', #57001 ) ;
#9690 = CARTESIAN_POINT ( 'NONE',  ( 3.125281217184999960, -85.76107450217398309, 1.765319430424000080 ) ) ;
#9691 = CARTESIAN_POINT ( 'NONE',  ( -5.785951846261999876, -80.29104072104459533, -9.693547939119000034 ) ) ;
#9692 = CARTESIAN_POINT ( 'NONE',  ( 10.75000000000000000, -80.75000000000000000, 3.489821576044999869E-14 ) ) ;
#9693 = DIRECTION ( 'NONE',  ( 0.000000000000000000, -1.000000000000000000, 2.131628207279999907E-13 ) ) ;
#9694 = CARTESIAN_POINT ( 'NONE',  ( -9.524774638983998898, -77.28961520195100832, 5.924253427062000199 ) ) ;
#9695 = CARTESIAN_POINT ( 'NONE',  ( 10.13881649148000008, -76.50783510652000530, -5.938594122520999719 ) ) ;
#9696 = CARTESIAN_POINT ( 'NONE',  ( 8.931146968900000260, -78.54653426492899371, -3.885139576175999920 ) ) ;
#9697 = CIRCLE ( 'NONE', #33235, 13.94827586206999825 ) ;
#9698 = CARTESIAN_POINT ( 'NONE',  ( -12.60246356036999948, -77.76186929341000109, -0.9915196953554998860 ) ) ;
#9699 = CARTESIAN_POINT ( 'NONE',  ( -11.75000000000000000, -76.30000000000001137, 1.487410190129999909E-14 ) ) ;
#9700 = CARTESIAN_POINT ( 'NONE',  ( -1.147008567282696401, -76.10208333332839459, 10.94791666671693164 ) ) ;
#9701 = VERTEX_POINT ( 'NONE', #1921 ) ;
#9702 = CARTESIAN_POINT ( 'NONE',  ( -0.1380878923252624457, -53.57265597643803545, -12.70555840928063773 ) ) ;
#9703 = CARTESIAN_POINT ( 'NONE',  ( 2.979603836623999857, -79.28053998579800066, -8.720586535794000227 ) ) ;
#9704 = CARTESIAN_POINT ( 'NONE',  ( 11.75000000000000000, -75.95000000000000284, 0.000000000000000000 ) ) ;
#9705 = EDGE_CURVE ( 'NONE', #53225, #30862, #50579, .T. ) ;
#9706 = VECTOR ( 'NONE', #37760, 1000.000000000000000 ) ;
#9707 = CARTESIAN_POINT ( 'NONE',  ( 0.000000000000000000, -23.25000000000000000, 12.50000000000000000 ) ) ;
#9708 = VERTEX_POINT ( 'NONE', #40144 ) ;
#9709 = CARTESIAN_POINT ( 'NONE',  ( 6.855510751285000204, -78.10715244345298913, -8.732042287340998854 ) ) ;
#9710 = CARTESIAN_POINT ( 'NONE',  ( 8.121699804378911480, -61.63626205718931317, -9.841121124288225275 ) ) ;
#9711 = ORIENTED_EDGE ( 'NONE', *, *, #38780, .T. ) ;
#9712 = ORIENTED_EDGE ( 'NONE', *, *, #31298, .T. ) ;
#9713 = AXIS2_PLACEMENT_3D ( 'NONE', #49549, #31804, #26212 ) ;
#9714 = CARTESIAN_POINT ( 'NONE',  ( -10.18949731070000020, -55.58470987670000341, -7.645392562244000878 ) ) ;
#9715 = AXIS2_PLACEMENT_3D ( 'NONE', #20302, #30001, #38297 ) ;
#9716 =( NAMED_UNIT ( * ) PLANE_ANGLE_UNIT ( ) SI_UNIT ( $, .RADIAN. ) );
#9717 = CARTESIAN_POINT ( 'NONE',  ( -9.358268528169000788, -79.41356642288599232, -2.797054701638000296 ) ) ;
#9718 = EDGE_CURVE ( 'NONE', #7434, #46988, #19640, .T. ) ;
#9719 = ORIENTED_EDGE ( 'NONE', *, *, #44033, .T. ) ;
#9720 = DIRECTION ( 'NONE',  ( 0.7071067811865475727, 0.000000000000000000, -0.7071067811865475727 ) ) ;
#9721 = CARTESIAN_POINT ( 'NONE',  ( -1.250000000000000000, -78.50000000000000000, 0.000000000000000000 ) ) ;
#9722 = CARTESIAN_POINT ( 'NONE',  ( 1.162219475002999935, -78.51329787945999783, 1.002509651144999792 ) ) ;
#9723 = ORIENTED_EDGE ( 'NONE', *, *, #35872, .T. ) ;
#9724 = CARTESIAN_POINT ( 'NONE',  ( 4.574312611392000072, -77.46505194988499454, 8.320643751074999983 ) ) ;
#9725 = DIRECTION ( 'NONE',  ( -9.217554813251081680E-07, 2.920569602132825499E-20, 0.9999999999995752287 ) ) ;
#9726 = CARTESIAN_POINT ( 'NONE',  ( -1.154538933705213211, -80.13146567447462587, -0.4788082789554529706 ) ) ;
#9727 = CARTESIAN_POINT ( 'NONE',  ( 1.779623408250214922, -17.86369130974330233, -12.71471627657038361 ) ) ;
#9728 = CARTESIAN_POINT ( 'NONE',  ( 3.723051508230308393, -86.25171438276198899, 2.704164226566200924 ) ) ;
#9729 = CARTESIAN_POINT ( 'NONE',  ( 7.912189497417754680, -79.89383890195257720, 4.794239927622985675 ) ) ;
#9730 = DIRECTION ( 'NONE',  ( 0.7071067811865475727, 0.000000000000000000, -0.7071067811865475727 ) ) ;
#9731 = ORIENTED_EDGE ( 'NONE', *, *, #24108, .T. ) ;
#9732 = CARTESIAN_POINT ( 'NONE',  ( 1.243547092045928615, -77.66458333333332575, 9.500000000000003553 ) ) ;
#9733 = CARTESIAN_POINT ( 'NONE',  ( -1.476182556144000069, -76.36723242473999562, 12.22114576030999977 ) ) ;
#9734 = CARTESIAN_POINT ( 'NONE',  ( -0.6219878248318000402, -79.94404873715900806, -1.382777385570999940 ) ) ;
#9735 = VECTOR ( 'NONE', #17432, 1000.000000000000000 ) ;
#9736 = EDGE_CURVE ( 'NONE', #58179, #5420, #9453, .T. ) ;
#9737 = CARTESIAN_POINT ( 'NONE',  ( 2.772699504624841715, -2.152166083112415418, 2.171300326618198273 ) ) ;
#9738 = CARTESIAN_POINT ( 'NONE',  ( 8.596763593984000806, -61.93532396089999992, -9.310159863737000663 ) ) ;
#9739 = CARTESIAN_POINT ( 'NONE',  ( -5.531768889155999958, -79.10509418445998620, -10.94525552207000096 ) ) ;
#9740 = CARTESIAN_POINT ( 'NONE',  ( -11.94395460750000204, -77.18299661749800578, 2.857367593729999822 ) ) ;
#9741 = CARTESIAN_POINT ( 'NONE',  ( 11.70000000000000107, -80.79999999999999716, 0.000000000000000000 ) ) ;
#9742 = CARTESIAN_POINT ( 'NONE',  ( -10.87436498444000144, -80.04903360897698406, 1.083693866698000052 ) ) ;
#9743 = CARTESIAN_POINT ( 'NONE',  ( 5.316634094433000612, -77.27156332859900090, 8.027686297795002091 ) ) ;
#9744 = CARTESIAN_POINT ( 'NONE',  ( -9.722718241315000398, -18.75000000000000000, 7.247844507162001015 ) ) ;
#9745 = CARTESIAN_POINT ( 'NONE',  ( -1.880557995764754908, -76.56599386863840095, -12.89133805120253307 ) ) ;
#9746 = AXIS2_PLACEMENT_3D ( 'NONE', #57283, #34251, #47297 ) ;
#9747 = B_SPLINE_SURFACE_WITH_KNOTS ( 'NONE', 3, 3, ( 
 ( #50049, #32583, #23164, #6027 ),
 ( #32291, #1622, #5737, #10181 ),
 ( #28159, #23744, #41758, #1333 ),
 ( #9301, #27581, #22875, #40884 ),
 ( #476, #19328, #45624, #41172 ),
 ( #766, #36736, #51506, #29897 ),
 ( #43503, #38486, #56214, #38195 ),
 ( #34043, #24913, #47955, #24340 ) ),
 .UNSPECIFIED., .F., .F., .F.,
 ( 4, 1, 1, 1, 1, 4 ),
 ( 4, 4 ),
 ( -0.01200407347463999970, 0.000000000000000000, 0.3333333333333000081, 0.6666666666667000474, 1.000000000000000000, 1.011997855551999947 ),
 ( -0.3559705542741000150, 1.355970554273999928 ),
 .UNSPECIFIED. ) ;
#9748 = VERTEX_POINT ( 'NONE', #45475 ) ;
#9749 = DIRECTION ( 'NONE',  ( -0.9999999999999994449, -3.428898374088997947E-08, 7.236136583703995822E-12 ) ) ;
#9750 = CARTESIAN_POINT ( 'NONE',  ( 0.6120151737828000149, -80.85757119619998434, 1.204744225600999918 ) ) ;
#9751 = CARTESIAN_POINT ( 'NONE',  ( 0.3271848554490964789, -79.35416666666667140, 1.217465845835395521 ) ) ;
#9752 = CARTESIAN_POINT ( 'NONE',  ( -0.6295237254636286695, -82.91666666666667140, 1.092232985442819881 ) ) ;
#9753 = CARTESIAN_POINT ( 'NONE',  ( 4.977714881822485893, -76.94999999999998863, -8.125826846032065731 ) ) ;
#9754 = AXIS2_PLACEMENT_3D ( 'NONE', #52178, #57459, #25871 ) ;
#9755 = CARTESIAN_POINT ( 'NONE',  ( 11.43454631689000145, -77.73332587731398746, -3.800910706745999956 ) ) ;
#9756 = CARTESIAN_POINT ( 'NONE',  ( 1.475792658273999969, -77.34418023959399591, -9.517102871385000995 ) ) ;
#9757 = CARTESIAN_POINT ( 'NONE',  ( 6.329451544447319833, -76.02924920104398154, 9.917131221196935797 ) ) ;
#9758 = CARTESIAN_POINT ( 'NONE',  ( 9.892383529026000488, -79.17237613278999220, -4.882876457188000785 ) ) ;
#9759 = CARTESIAN_POINT ( 'NONE',  ( 3.194290819684705962, -86.07390000031791999, 2.320109443757823797 ) ) ;
#9760 = VERTEX_POINT ( 'NONE', #54896 ) ;
#9761 = AXIS2_PLACEMENT_3D ( 'NONE', #8230, #30071, #22089 ) ;
#9762 = DIRECTION ( 'NONE',  ( 1.894056205636980548E-11, -1.538484108169980264E-07, 0.9999999999999882316 ) ) ;
#9763 = CARTESIAN_POINT ( 'NONE',  ( 3.699999999669999262, -78.39678895079168797, -2.183641561086286487 ) ) ;
#9764 = CARTESIAN_POINT ( 'NONE',  ( -4.399243655502999673, -79.89827306409299013, 10.05537673064999815 ) ) ;
#9765 = CARTESIAN_POINT ( 'NONE',  ( -9.611650271896836628, -79.14166666666666572, -5.539808784079885307 ) ) ;
#9766 = CARTESIAN_POINT ( 'NONE',  ( -9.904718956742000202, -75.92565473334099124, -7.632293584405999809 ) ) ;
#9767 = LINE ( 'NONE', #27755, #48194 ) ;
#9768 = CARTESIAN_POINT ( 'NONE',  ( 10.01749678875999905, -18.80819056997000160, -7.660430392568000180 ) ) ;
#9769 = CARTESIAN_POINT ( 'NONE',  ( 10.07627163191000008, -23.24999999688999708, -7.601397897754999633 ) ) ;
#9770 = ORIENTED_EDGE ( 'NONE', *, *, #55900, .T. ) ;
#9771 = CARTESIAN_POINT ( 'NONE',  ( 3.350422000336999773, -79.35815762081898583, -10.63152260923000014 ) ) ;
#9772 = FACE_BOUND ( 'NONE', #4332, .T. ) ;
#9773 = CARTESIAN_POINT ( 'NONE',  ( -12.00000000000000000, -77.39999999999999147, 0.000000000000000000 ) ) ;
#9774 = CARTESIAN_POINT ( 'NONE',  ( -3.523652292752748938, -78.48547957940617437, 1.990986972659168019 ) ) ;
#9775 = EDGE_CURVE ( 'NONE', #32332, #13850, #333, .T. ) ;
#9776 = CARTESIAN_POINT ( 'NONE',  ( -0.9682055199207542096, -81.54584953990853080, 0.7910361119925342077 ) ) ;
#9777 = CARTESIAN_POINT ( 'NONE',  ( -0.5228656313312000092, -78.92817062466399136, -11.03650783440000005 ) ) ;
#9778 = EDGE_CURVE ( 'NONE', #13032, #29661, #32154, .T. ) ;
#9779 = CARTESIAN_POINT ( 'NONE',  ( -8.563626910508329360, -77.00000000000001421, -3.884937692711959656 ) ) ;
#9780 = CARTESIAN_POINT ( 'NONE',  ( 13.89999999999999858, -80.79999999999999716, 0.000000000000000000 ) ) ;
#9781 = PRODUCT_DEFINITION_SHAPE ( 'NONE', 'NONE',  #58408 ) ;
#9782 = CARTESIAN_POINT ( 'NONE',  ( 0.000000000000000000, -23.25000000000000000, -12.00000000000000000 ) ) ;
#9783 = CARTESIAN_POINT ( 'NONE',  ( 0.000000000000000000, -76.30000000005068728, -9.649999999948999374 ) ) ;
#9784 = CARTESIAN_POINT ( 'NONE',  ( 9.632278712654541053, -79.23988867217208565, 5.261846222106294491 ) ) ;
#9785 = AXIS2_PLACEMENT_3D ( 'NONE', #15647, #6790, #38656 ) ;
#9786 = CARTESIAN_POINT ( 'NONE',  ( 4.000000000000000000, -5.200000000000000178, -0.5999999999999999778 ) ) ;
#9787 = ORIENTED_EDGE ( 'NONE', *, *, #19680, .F. ) ;
#9788 = ADVANCED_FACE ( 'NONE', ( #4731 ), #8561, .F. ) ;
#9789 = ORIENTED_EDGE ( 'NONE', *, *, #38831, .T. ) ;
#9790 = CARTESIAN_POINT ( 'NONE',  ( 4.739769873023999658, -78.54353998579799168, -8.830749431300999319 ) ) ;
#9791 = CARTESIAN_POINT ( 'NONE',  ( 7.614890194919533783, -78.78764436229195667, -7.587871591982528585 ) ) ;
#9792 = B_SPLINE_CURVE_WITH_KNOTS ( 'NONE', 3,
 ( #52262, #7379, #43395, #56972, #43695, #16824, #39243, #12101, #42538, #7095, #34807, #38382, #20104, #52831, #12387, #33658, #11247, #51699 ),
 .UNSPECIFIED., .F., .F.,
 ( 4, 2, 2, 2, 2, 2, 2, 2, 4 ),
 ( 0.000000000000000000, 0.1249999999999999722, 0.2500000000000000000, 0.3750000000000000000, 0.5000000000000001110, 0.6250000000000001110, 0.7500000000000000000, 0.8750000000000000000, 1.000000000000000000 ),
 .UNSPECIFIED. ) ;
#9793 = ORIENTED_EDGE ( 'NONE', *, *, #43829, .T. ) ;
#9794 = DIRECTION ( 'NONE',  ( -1.000000000000000000, 0.000000000000000000, 0.000000000000000000 ) ) ;
#9795 = B_SPLINE_CURVE_WITH_KNOTS ( 'NONE', 3,
 ( #44970, #17811, #8357, #4526, #22818, #48527, #54119, #22225, #35202, #22526, #40536, #40829, #26639, #57658, #131, #31360, #18108, #35797 ),
 .UNSPECIFIED., .F., .F.,
 ( 4, 2, 2, 2, 2, 2, 2, 2, 4 ),
 ( 0.000000000000000000, 0.1250000000000000833, 0.2500000000000001665, 0.3750000000000002220, 0.5000000000000002220, 0.6250000000000002220, 0.7500000000000001110, 0.8750000000000001110, 1.000000000000000000 ),
 .UNSPECIFIED. ) ;
#9796 = CARTESIAN_POINT ( 'NONE',  ( -2.473589675488696571, -83.01666668198382126, 2.395243405415722560 ) ) ;
#9797 = VECTOR ( 'NONE', #46076, 1000.000000000000114 ) ;
#9798 = CARTESIAN_POINT ( 'NONE',  ( 7.619712170668999640, -60.20404510030000012, 10.35409959312000083 ) ) ;
#9799 = DIRECTION ( 'NONE',  ( 0.000000000000000000, 0.000000000000000000, 1.000000000000000000 ) ) ;
#9800 = CARTESIAN_POINT ( 'NONE',  ( -3.545693839590635221, -77.44881410897738760, 11.44325331982801863 ) ) ;
#9801 = CARTESIAN_POINT ( 'NONE',  ( 2.179295889402999897, -78.62554586492200315, 11.00312592022000047 ) ) ;
#9802 = CARTESIAN_POINT ( 'NONE',  ( 1.426370643901660129, -81.00000000000002842, 10.71686120634390171 ) ) ;
#9803 = VERTEX_POINT ( 'NONE', #23317 ) ;
#9804 = DIRECTION ( 'NONE',  ( 0.07798810297639352518, 0.04890180917562222257, 0.9957542211075455230 ) ) ;
#9805 = ORIENTED_EDGE ( 'NONE', *, *, #27746, .T. ) ;
#9806 = CARTESIAN_POINT ( 'NONE',  ( -0.02231494135697667525, -77.47534742525941454, 9.249882832515465836 ) ) ;
#9807 = CARTESIAN_POINT ( 'NONE',  ( 2.604371601988999974, -77.57410247015199900, -10.72853197743999942 ) ) ;
#9808 = CARTESIAN_POINT ( 'NONE',  ( 1.000000000000000000, -81.19999999999998863, 7.000000000000000000 ) ) ;
#9809 = CARTESIAN_POINT ( 'NONE',  ( -1.403403115923000044, -77.46141162325051255, 0.5665048067823000855 ) ) ;
#9810 = CARTESIAN_POINT ( 'NONE',  ( 12.00000000000000711, -77.63958333333333428, -1.570796326794872355 ) ) ;
#9811 = CARTESIAN_POINT ( 'NONE',  ( -10.47020627418440242, -80.97916666666665719, 2.813789756862221214 ) ) ;
#9812 = CARTESIAN_POINT ( 'NONE',  ( -1.462188802161999979, -79.30657335004998743, -0.7147474581103999691 ) ) ;
#9813 = DIRECTION ( 'NONE',  ( 1.000000000000000000, 0.000000000000000000, 0.000000000000000000 ) ) ;
#9814 = CARTESIAN_POINT ( 'NONE',  ( 10.82226978776999893, -79.19088091476099578, 1.601965348215999896 ) ) ;
#9815 = CARTESIAN_POINT ( 'NONE',  ( -8.643979526155998627, -25.25953772911000073, -9.422807787372999400 ) ) ;
#9816 = VECTOR ( 'NONE', #43412, 1000.000000000000000 ) ;
#9817 = CARTESIAN_POINT ( 'NONE',  ( 9.249780780301254168, -79.07089109199264954, 2.485615031187831558 ) ) ;
#9818 = CARTESIAN_POINT ( 'NONE',  ( -0.6860200224810000247, -83.47200654646700002, -3.477692862941000218 ) ) ;
#9819 = ORIENTED_EDGE ( 'NONE', *, *, #10383, .F. ) ;
#9820 = CARTESIAN_POINT ( 'NONE',  ( 7.691874984900000101, -79.55148891412299861, -9.768577294637001529 ) ) ;
#9821 = CARTESIAN_POINT ( 'NONE',  ( 0.1582166208049999856, -76.01502919452599372, 11.37418021090000053 ) ) ;
#9822 = CARTESIAN_POINT ( 'NONE',  ( 10.43518326032827126, -77.86936012529750428, 2.584052442912811109 ) ) ;
#9823 = CARTESIAN_POINT ( 'NONE',  ( 6.917788961650999546, -78.80788266157699695, -9.780606322222999083 ) ) ;
#9824 = CARTESIAN_POINT ( 'NONE',  ( -9.963464501286001251, -18.31723479381000175, 7.659241807038999816 ) ) ;
#9825 = AXIS2_PLACEMENT_3D ( 'NONE', #7215, #6638, #56523 ) ;
#9826 = ADVANCED_FACE ( 'NONE', ( #909 ), #54040, .F. ) ;
#9828 = CARTESIAN_POINT ( 'NONE',  ( -1.480597980168999888E-14, -80.60000000000000853, 0.000000000000000000 ) ) ;
#9827 = CARTESIAN_POINT ( 'NONE',  ( -1.538071403319991814, -78.41458333333333997, -11.75000000000000355 ) ) ;
#9829 = CARTESIAN_POINT ( 'NONE',  ( -2.278169229989186029, -3.319065836604013775, -2.686266703802629330 ) ) ;
#9830 = CARTESIAN_POINT ( 'NONE',  ( 4.104553908884746249, -80.94404747578096249, 9.935402628773564615 ) ) ;
#9831 = CARTESIAN_POINT ( 'NONE',  ( 8.191903123214999027, -77.87017682799398699, 4.637231687908999866 ) ) ;
#9832 = CARTESIAN_POINT ( 'NONE',  ( -3.112536659741993894, -86.02148120184399716, 1.385790604991013142 ) ) ;
#9833 = CARTESIAN_POINT ( 'NONE',  ( -0.9453041629244000044, -78.27289305516799800, 11.10679974661999836 ) ) ;
#9834 = CARTESIAN_POINT ( 'NONE',  ( 10.16964605767000052, -76.35263817687363996, -6.884832982024001069 ) ) ;
#9835 = CARTESIAN_POINT ( 'NONE',  ( -6.468715003314000178, -80.88375601109909496, 8.928767417134999107 ) ) ;
#9836 = ORIENTED_EDGE ( 'NONE', *, *, #47931, .T. ) ;
#9837 = CIRCLE ( 'NONE', #52263, 1.199999999999999956 ) ;
#9838 = DIRECTION ( 'NONE',  ( 0.7071067811865474617, 0.7071067811865474617, 2.341637280430153019E-09 ) ) ;
#9839 = CARTESIAN_POINT ( 'NONE',  ( -9.713032445540607185, -24.52293762691879309, 7.970418356296339546 ) ) ;
#9840 = B_SPLINE_CURVE_WITH_KNOTS ( 'NONE', 3,
 ( #54720, #19578, #29014, #55892, #32259, #28714, #50599, #19293, #19879, #33138, #37872, #36993, #6288, #24303, #42018, #46466, #55594, #50888 ),
 .UNSPECIFIED., .F., .F.,
 ( 4, 2, 2, 2, 2, 2, 2, 2, 4 ),
 ( 0.000000000000000000, 0.1249999999999999722, 0.2499999999999999445, 0.3749999999999998890, 0.4999999999999998890, 0.6249999999999998890, 0.7499999999999997780, 0.8749999999999998890, 1.000000000000000000 ),
 .UNSPECIFIED. ) ;
#9841 = CARTESIAN_POINT ( 'NONE',  ( -0.7803569495551999635, -81.85659709982999743, -1.471836271561000054 ) ) ;
#9842 = CARTESIAN_POINT ( 'NONE',  ( -10.05535668103000191, -78.22957133974199451, 4.970705447719999448 ) ) ;
#9843 = CARTESIAN_POINT ( 'NONE',  ( 0.9090372547675998893, -78.67794717677197980, 10.93790052299999971 ) ) ;
#9844 = DIRECTION ( 'NONE',  ( 0.8090169943751300830, 0.000000000000000000, -0.5877852522922218936 ) ) ;
#9845 = DIRECTION ( 'NONE',  ( 0.000000000000000000, -1.000000000000000000, 0.000000000000000000 ) ) ;
#9846 = CARTESIAN_POINT ( 'NONE',  ( -0.5999999999999999778, -18.84999999999999787, 10.98362417419999915 ) ) ;
#9847 = CARTESIAN_POINT ( 'NONE',  ( -1.249474801850635419, -81.11011701208103375, -0.1486004900664459893 ) ) ;
#9848 = CARTESIAN_POINT ( 'NONE',  ( -3.883940484920999747, -84.59192953870899601, 1.523663816304000163 ) ) ;
#9849 = CARTESIAN_POINT ( 'NONE',  ( -10.42531125074000009, -18.73514854687000053, -7.624341767140999870 ) ) ;
#9850 = CARTESIAN_POINT ( 'NONE',  ( 8.588893914397997875, -53.66760216274000328, -9.317954957978999531 ) ) ;
#9851 = CARTESIAN_POINT ( 'NONE',  ( -11.16978667388999824, -77.28678420793599457, -1.438690452479999937 ) ) ;
#9852 = EDGE_CURVE ( 'NONE', #20675, #46623, #53078, .T. ) ;
#9853 = CARTESIAN_POINT ( 'NONE',  ( -1.570423240223999928, -80.73824932256999887, -0.5559045111934000083 ) ) ;
#9854 = CARTESIAN_POINT ( 'NONE',  ( -1.209673032756999778, -78.05275416108999309, -0.5285249375785000536 ) ) ;
#9855 = DIRECTION ( 'NONE',  ( 0.000000000000000000, -3.446666965303000135E-11, 1.000000000000000000 ) ) ;
#9856 = CARTESIAN_POINT ( 'NONE',  ( -1.527490045409469532, -82.23783309118122986, 0.2444902829799560084 ) ) ;
#9857 = CARTESIAN_POINT ( 'NONE',  ( 1.476436775452767192, -83.11658282216879456, 0.3241340806173243494 ) ) ;
#9858 = CARTESIAN_POINT ( 'NONE',  ( -7.555765981425745181, -80.16344139804368751, -7.646384711791143651 ) ) ;
#9859 = CARTESIAN_POINT ( 'NONE',  ( 0.000000000000000000, -74.64999999999999147, 0.000000000000000000 ) ) ;
#9860 = ORIENTED_EDGE ( 'NONE', *, *, #2316, .T. ) ;
#9861 = CARTESIAN_POINT ( 'NONE',  ( -0.3392593397791182075, -81.70348311923245888, -1.202985507264590304 ) ) ;
#9862 = CARTESIAN_POINT ( 'NONE',  ( -2.693529710394999999, -79.78555764342200973, 10.81663063389000001 ) ) ;
#9863 = AXIS2_PLACEMENT_3D ( 'NONE', #42550, #15966, #56127 ) ;
#9864 = LINE ( 'NONE', #19306, #35587 ) ;
#9865 = VERTEX_POINT ( 'NONE', #52221 ) ;
#9866 = EDGE_CURVE ( 'NONE', #4192, #46183, #8372, .T. ) ;
#9867 = EDGE_LOOP ( 'NONE', ( #21392, #34868, #57918, #10046 ) ) ;
#9868 = CARTESIAN_POINT ( 'NONE',  ( 1.386500578471000056, -81.36942886518100693, 0.2961005337747000254 ) ) ;
#9869 = EDGE_CURVE ( 'NONE', #22759, #36944, #11497, .T. ) ;
#9870 = ORIENTED_EDGE ( 'NONE', *, *, #20391, .F. ) ;
#9871 = ORIENTED_EDGE ( 'NONE', *, *, #14552, .F. ) ;
#9872 = FACE_BOUND ( 'NONE', #57957, .T. ) ;
#9873 = PLANE ( 'NONE',  #50932 ) ;
#9874 = CARTESIAN_POINT ( 'NONE',  ( 0.1004720478954561208, -79.81770832617392841, 3.442836509308329074 ) ) ;
#9875 = B_SPLINE_CURVE_WITH_KNOTS ( 'NONE', 3,
 ( #10721, #24285, #28404, #2156, #20157, #46160, #23985, #24866, #14830, #6567, #16010, #5686, #46451, #41709, #50872, #10418, #5979, #42002, #1570, #28699, #6269, #1868, #19863 ),
 .UNSPECIFIED., .F., .F.,
 ( 4, 2, 2, 2, 2, 2, 1, 2, 2, 2, 2, 4 ),
 ( 0.000000000000000000, 0.1249999999999999722, 0.2500000000000000000, 0.3750000000000000000, 0.5000000000000001110, 0.5625000000000001110, 0.6250000000000001110, 0.6875000000000001110, 0.7500000000000000000, 0.8125000000000000000, 0.8750000000000000000, 1.000000000000000000 ),
 .UNSPECIFIED. ) ;
#9876 = VECTOR ( 'NONE', #41806, 1000.000000000000000 ) ;
#9877 = CARTESIAN_POINT ( 'NONE',  ( 3.589839488473549611, -78.25675447763170212, -8.524986016596304950 ) ) ;
#9878 = DIRECTION ( 'NONE',  ( -4.762495317921000031E-11, -1.000000000000000000, 4.762546956201999894E-11 ) ) ;
#9879 = ORIENTED_EDGE ( 'NONE', *, *, #14479, .F. ) ;
#9880 = VERTEX_POINT ( 'NONE', #12629 ) ;
#9881 = DIRECTION ( 'NONE',  ( 0.000000000000000000, -1.000000000000000000, 0.000000000000000000 ) ) ;
#9882 = CARTESIAN_POINT ( 'NONE',  ( -1.618935784642295816, -18.07248831326895910, -12.52134385800258087 ) ) ;
#9883 = CARTESIAN_POINT ( 'NONE',  ( -1.092232985442824100, -81.45833333333328596, 0.6295237254636200097 ) ) ;
#9884 = CARTESIAN_POINT ( 'NONE',  ( 0.000000000000000000, -49.87071424677999687, 0.000000000000000000 ) ) ;
#9885 = CARTESIAN_POINT ( 'NONE',  ( -9.022250383429000209, -78.79985853368698656, -3.573472734901999903 ) ) ;
#9886 = EDGE_CURVE ( 'NONE', #52710, #37882, #42321, .T. ) ;
#9887 = DIRECTION ( 'NONE',  ( -1.000000000000000000, 0.000000000000000000, 2.817678007057000277E-14 ) ) ;
#9888 = CARTESIAN_POINT ( 'NONE',  ( 2.485958775866533355, -85.88010983227711392, 3.011055413551058990 ) ) ;
#9889 = CARTESIAN_POINT ( 'NONE',  ( 11.77596950146999966, -77.20276987983000083, 5.402702954953999992 ) ) ;
#9890 = CARTESIAN_POINT ( 'NONE',  ( -1.359874270581000077, -81.11252996976000418, 0.5545210745837000355 ) ) ;
#9891 = CARTESIAN_POINT ( 'NONE',  ( -12.75761570867000039, -22.77819125662999866, -1.931043762602999925 ) ) ;
#9892 = CARTESIAN_POINT ( 'NONE',  ( 0.000000000000000000, -76.79999999999999716, 0.000000000000000000 ) ) ;
#9893 = CARTESIAN_POINT ( 'NONE',  ( -2.385010427669000066, -80.41718807822699944, -3.423711137155000195 ) ) ;
#9894 = CARTESIAN_POINT ( 'NONE',  ( -11.09105850093000001, -80.18429898691658764, 1.974238845993000258 ) ) ;
#9895 = CARTESIAN_POINT ( 'NONE',  ( 6.559997675027998909, -78.38646001420198672, 7.127949055663999722 ) ) ;
#9896 = CARTESIAN_POINT ( 'NONE',  ( 2.926762049849723102, -2.887065986493968062, 1.411820854762963595 ) ) ;
#9897 = CARTESIAN_POINT ( 'NONE',  ( 5.969195881079206956, -76.15416666614690655, -10.35833566983218113 ) ) ;
#9898 = EDGE_CURVE ( 'NONE', #12885, #47367, #52677, .T. ) ;
#9899 = CARTESIAN_POINT ( 'NONE',  ( -0.5409299486741000473, -79.13012224168299724, 1.218996123443000013 ) ) ;
#9900 = DIRECTION ( 'NONE',  ( 0.000000000000000000, -1.000000000000000000, 0.000000000000000000 ) ) ;
#9901 = CARTESIAN_POINT ( 'NONE',  ( -10.98362417419999915, -18.84999999999999787, -0.5999999999999999778 ) ) ;
#9902 = CARTESIAN_POINT ( 'NONE',  ( 10.41647365791567381, -77.20000000000001705, -2.825691430128591808 ) ) ;
#9903 = EDGE_CURVE ( 'NONE', #34968, #38188, #28172, .T. ) ;
#9904 = ORIENTED_EDGE ( 'NONE', *, *, #44488, .T. ) ;
#9905 = CARTESIAN_POINT ( 'NONE',  ( -10.79468190471742695, -78.83333333333331439, -4.801183948429945225 ) ) ;
#9906 = DIRECTION ( 'NONE',  ( 0.000000000000000000, -1.000000000000000000, 2.129426118997999821E-13 ) ) ;
#9907 = CARTESIAN_POINT ( 'NONE',  ( 9.722718241315000398, -55.54999999966999980, -7.247844507162001015 ) ) ;
#9908 = AXIS2_PLACEMENT_3D ( 'NONE', #46733, #986, #14813 ) ;
#9909 = AXIS2_PLACEMENT_3D ( 'NONE', #15387, #12113, #38106 ) ;
#9910 = CARTESIAN_POINT ( 'NONE',  ( 2.062673488410000200, -60.12452273675999947, 12.82904109066000053 ) ) ;
#9911 = CARTESIAN_POINT ( 'NONE',  ( 7.601397897754999633, -18.75000000000000000, -9.369164850722000892 ) ) ;
#9912 = CARTESIAN_POINT ( 'NONE',  ( -8.508616545356863625, -79.54773900155933575, 6.572652578013081559 ) ) ;
#9913 = CARTESIAN_POINT ( 'NONE',  ( 1.896935383555999888, -79.58371332859898928, -9.552341775358000220 ) ) ;
#9914 = CARTESIAN_POINT ( 'NONE',  ( 9.263181489341201669, -78.50004972168174788, 7.234445444280653170 ) ) ;
#9915 = VECTOR ( 'NONE', #40824, 1000.000000000000000 ) ;
#9916 = CYLINDRICAL_SURFACE ( 'NONE', #39135, 1.250000000000000000 ) ;
#9917 = CARTESIAN_POINT ( 'NONE',  ( 1.937326043969999745, -77.16792237372438024, 10.88551626581000065 ) ) ;
#9918 = CARTESIAN_POINT ( 'NONE',  ( -1.114850945326000042, -81.91137662116999252, -1.012920685771000029 ) ) ;
#9919 = FACE_OUTER_BOUND ( 'NONE', #41966, .T. ) ;
#9920 = CARTESIAN_POINT ( 'NONE',  ( 4.603815134758999505, -77.68647980950599674, -8.210729597153999748 ) ) ;
#9922 = CARTESIAN_POINT ( 'NONE',  ( 2.301364338783000285, -1.490890595155999865, -3.291430154679999998 ) ) ;
#9921 = CARTESIAN_POINT ( 'NONE',  ( 1.269372913341999976, -83.59225696173399456, -3.977222946407999782 ) ) ;
#9923 = CARTESIAN_POINT ( 'NONE',  ( 8.857115352654000517, -79.34945194988499395, -3.584237475251999872 ) ) ;
#9924 = CARTESIAN_POINT ( 'NONE',  ( 5.209925396217442994, -77.11090969355151969, -10.71737960282440838 ) ) ;
#9925 = CARTESIAN_POINT ( 'NONE',  ( 0.9236342483431000394, -80.34477190545899816, -0.9420537984437000745 ) ) ;
#9926 = ORIENTED_EDGE ( 'NONE', *, *, #23548, .F. ) ;
#9927 = CARTESIAN_POINT ( 'NONE',  ( -7.388662270317944980, -77.16469925202929403, -7.808743162194972776 ) ) ;
#9928 = CARTESIAN_POINT ( 'NONE',  ( 12.00000000000000000, -23.15000000000000213, 0.000000000000000000 ) ) ;
#9929 = CARTESIAN_POINT ( 'NONE',  ( 3.992904449609000483, -78.77851881763731967, -4.889897653514886385E-16 ) ) ;
#9930 = ORIENTED_EDGE ( 'NONE', *, *, #15670, .T. ) ;
#9931 = ORIENTED_EDGE ( 'NONE', *, *, #43956, .F. ) ;
#9932 = CARTESIAN_POINT ( 'NONE',  ( -8.734850699938000673, -79.64135281726700555, 8.271005326623001253 ) ) ;
#9933 = CARTESIAN_POINT ( 'NONE',  ( -8.359900899578630415E-07, -76.12787248224110215, -11.82848710057588626 ) ) ;
#9934 = DIRECTION ( 'NONE',  ( 1.000000000000000000, 0.000000000000000000, 0.000000000000000000 ) ) ;
#9935 = ORIENTED_EDGE ( 'NONE', *, *, #18549, .F. ) ;
#9936 = CARTESIAN_POINT ( 'NONE',  ( 4.358044849164000922, -77.27815612458898897, -11.11047130621000001 ) ) ;
#9937 = EDGE_CURVE ( 'NONE', #39245, #45676, #14993, .T. ) ;
#9938 = ORIENTED_EDGE ( 'NONE', *, *, #12812, .F. ) ;
#9939 = B_SPLINE_SURFACE_WITH_KNOTS ( 'NONE', 3, 3, ( 
 ( #51561, #19970, #15530, #1975, #33524, #28209, #41812, #37373, #24680, #28801, #19668, #50395, #11119, #37956, #50975, #37667, #20256, #55980, #37079, #29096, #47140, #15232, #2256, #10525, #6672, #55097, #41520, #9943, #42692, #32637, #38247, #14641, #50689, #46848, #27923 ),
 ( #46266, #56270, #1104, #32350, #6377, #33225, #45974, #5498, #51271, #24391, #10231, #19090, #5791, #42405, #23796, #1387, #19380, #55388, #14934, #32932, #28508, #46559, #6083, #24091, #42109, #1678, #55686, #26117, #39415, #52419, #47430, #20824, #24964, #44138, #33809 ),
 ( #20544, #11977, #48290, #6960, #2826, #7250, #43558, #38539, #3686, #29955, #21114, #43272, #21688, #25540, #25254, #11692, #7829, #3123, #39121, #56555, #42983, #48006, #38829, #56846, #16404, #7541, #2541, #11403, #34388, #57128, #16115, #16695, #39696, #34094, #3405 ),
 ( #52134, #29668, #51847, #48575, #47717, #25829, #34676, #12257, #12543, #52705, #52994, #30249, #43857, #21403, #29382, #15821, #16981, #30542, #8117, #17858, #45316, #13998, #40584, #466, #54166, #31996, #53280, #53576, #13410, #9584, #21974, #50037, #36149, #45018, #22572 ),
 ( #8699, #13113, #31701, #26984, #4572, #39985, #26399, #31410, #4274, #26689, #58297, #49453, #44421, #12826, #22270, #181, #30826, #18155, #27568, #57999, #4866, #40286, #35249, #13706, #49748, #45612, #27280, #22865, #35847, #53877, #5153, #17555, #36434, #57704, #54462 ),
 ( #48860, #23154, #31107, #17259, #9291, #8999, #40874, #18445, #8402, #49148, #44721, #3972, #35547, #49165, #58017, #30267, #31429, #40307, #48878, #17579, #199, #58316, #17000, #17877, #35868, #53592, #40602, #8420, #27005, #34981, #21425, #48308, #53897, #12563, #45039 ),
 ( #44740, #53010, #30561, #13131, #13428, #48592, #9018, #4593, #17278, #31127, #22589, #40002, #57721, #18174, #8718, #36167, #12277, #7848, #26709, #4291, #25848, #22291, #8138, #43875, #39433, #26418, #3424, #57440, #26138, #44159, #21709, #39715, #35268, #53300, #3991 ),
 ( #4883, #24042, #13724, #41470, #22880, #55341, #46215, #41763, #1055, #45922, #37033, #50343, #1341, #19043, #18462, #32590, #19332, #6033, #42057, #50926, #27298, #36742, #36452, #19618, #54480, #32013, #31720, #28460, #14015, #28165, #54760, #50639, #10474, #50055, #32882 ),
 ( #37326, #14885, #9601, #55048, #49767, #14303, #46508, #1628, #54186, #10187, #27586, #40891, #5170, #9308, #32296, #45629, #9893, #45333, #482, #23173, #41180, #5742, #771, #18748, #27875, #23750, #5456, #23458, #14596, #48734, #15769, #44013, #11354, #39573, #57575 ),
 ( #29050, #12424, #42355, #1923, #43732, #21567, #37908, #25987, #17139, #42643, #39284, #35123, #7703, #24631, #26280, #57295, #44294, #53156, #8277, #16858, #34839, #12703, #52869, #33473, #30413, #6328, #33762, #3849, #48448, #37616, #3284, #47089, #11069, #28752, #7989 ) ),
 .UNSPECIFIED., .F., .F., .F.,
 ( 4, 1, 1, 1, 1, 1, 1, 4 ),
 ( 4, 1, 1, 1, 1, 1, 1, 1, 1, 1, 1, 1, 1, 1, 1, 1, 1, 1, 1, 1, 1, 1, 1, 1, 1, 1, 1, 1, 1, 1, 1, 1, 4 ),
 ( -0.01000000000000000021, 0.000000000000000000, 0.1000000000000000056, 0.2000000000000000111, 0.2999999999999999889, 0.4000000000000000222, 0.5000000000000000000, 0.5100000000000000089 ),
 ( -0.02000360058914000053, 0.01249651413551000102, 0.04499662886017000152, 0.07749674358482000480, 0.1099968583094999980, 0.1424969730340999996, 0.1749970877587999907, 0.2074972024834000062, 0.2399973172080999972, 0.2724974319326999850, 0.3049975466574000316, 0.3374976613821000226, 0.3699977761066999826, 0.4024978908314000292, 0.4349980055560000447, 0.4674981202807000358, 0.4999982350052999958, 0.5324983497299999868, 0.5649984644546000023, 0.5974985791793000489, 0.6299986939038999534, 0.6624988086286000000, 0.6949989233532000155, 0.7274990380779000620, 0.7599991528025999976, 0.7924992675271999021, 0.8249993822518999487, 0.8574994969764999642, 0.8899996117012000107, 0.9224997264257999152, 0.9549998411504999618, 0.9874999558750999773, 1.020000070600000086 ),
 .UNSPECIFIED. ) ;
#9940 = EDGE_LOOP ( 'NONE', ( #57767, #16641, #43922, #13184 ) ) ;
#9941 = CARTESIAN_POINT ( 'NONE',  ( -1.063988671825434995, -2.699566373942746456, -3.070960408435446709 ) ) ;
#9942 = VERTEX_POINT ( 'NONE', #25339 ) ;
#9943 = CARTESIAN_POINT ( 'NONE',  ( -3.462045132322999930, -81.73367725304099451, -0.7738241070029000523 ) ) ;
#9944 = DIRECTION ( 'NONE',  ( -0.9999999999995751176, 0.000000000000000000, -9.217549100139771309E-07 ) ) ;
#9945 = VECTOR ( 'NONE', #20799, 1000.000000000000114 ) ;
#9946 = ORIENTED_EDGE ( 'NONE', *, *, #30472, .F. ) ;
#9947 = DIRECTION ( 'NONE',  ( 1.000000000000000000, 0.000000000000000000, 0.000000000000000000 ) ) ;
#9948 = VERTEX_POINT ( 'NONE', #43355 ) ;
#9949 = LINE ( 'NONE', #10832, #26173 ) ;
#9950 = CARTESIAN_POINT ( 'NONE',  ( 8.898800776725989792, -78.56725350033094912, -3.871068654289783861 ) ) ;
#9951 = CARTESIAN_POINT ( 'NONE',  ( -11.26971213774734082, -79.79999999999996874, -3.998637387020187006 ) ) ;
#9952 = FACE_BOUND ( 'NONE', #19670, .T. ) ;
#9953 = EDGE_CURVE ( 'NONE', #27527, #17474, #42834, .T. ) ;
#9954 = CARTESIAN_POINT ( 'NONE',  ( 1.849737152796000039, -76.56009456256700219, 11.02961253862999946 ) ) ;
#9955 = CARTESIAN_POINT ( 'NONE',  ( -1.821913034590999979E-14, -80.69999999923000189, 0.000000000000000000 ) ) ;
#9956 = EDGE_CURVE ( 'NONE', #25888, #23504, #44800, .T. ) ;
#9957 = CARTESIAN_POINT ( 'NONE',  ( -5.300820900011999903, -76.40928543398199224, -9.898738636383001221 ) ) ;
#9958 = B_SPLINE_CURVE_WITH_KNOTS ( 'NONE', 3,
 ( #47466, #6989, #47747, #38857, #56877, #31437, #58324, #40315, #8726, #30568, #22003, #44447, #3999, #12571, #35574, #48888, #8431, #44747, #3431, #57730, #21433, #12286, #53601, #17287, #26425, #39441, #13436, #48601, #35275, #35876, #49173, #57448, #49477, #4298, #17887, #58026, #40009, #13141, #17587, #26719, #31134, #22299, #53308, #53905, #43885, #9028, #40611, #8147, #27014, #12851, #48316, #45050, #4603, #22601, #208, #18183, #34989, #30851, #25856, #36178, #30275, #7856, #17007, #3714, #53018 ),
 .UNSPECIFIED., .F., .F.,
 ( 4, 2, 2, 2, 2, 2, 2, 2, 2, 2, 2, 2, 2, 2, 2, 2, 1, 2, 2, 2, 2, 2, 2, 2, 2, 2, 2, 2, 2, 2, 2, 2, 4 ),
 ( 0.000000000000000000, 0.03125000000000000000, 0.06250000000000000000, 0.09375000000000000000, 0.1250000000000000000, 0.1562500000000000000, 0.1875000000000000000, 0.2187500000000000000, 0.2500000000000000000, 0.2812500000000000000, 0.3125000000000000000, 0.3437500000000000000, 0.3750000000000000000, 0.4062500000000000000, 0.4375000000000000000, 0.4687500000000000000, 0.5000000000000000000, 0.5312500000000000000, 0.5625000000000000000, 0.5937500000000000000, 0.6250000000000000000, 0.6562500000000000000, 0.6875000000000000000, 0.7187500000000000000, 0.7500000000000000000, 0.7812500000000000000, 0.8125000000000000000, 0.8437500000000000000, 0.8750000000000000000, 0.9062500000000000000, 0.9375000000000000000, 0.9687500000000000000, 1.000000000000000000 ),
 .UNSPECIFIED. ) ;
#9959 = CARTESIAN_POINT ( 'NONE',  ( -1.799037492230971980, -78.70949564512361007, -9.073313084848985355 ) ) ;
#9960 = CARTESIAN_POINT ( 'NONE',  ( 2.142412200439999914, -77.42738501420200237, 9.164433333602998388 ) ) ;
#9961 = FACE_OUTER_BOUND ( 'NONE', #37952, .T. ) ;
#9962 = CARTESIAN_POINT ( 'NONE',  ( -5.636745332574527367, -80.18232361003532560, -9.445903029628405889 ) ) ;
#9963 = CARTESIAN_POINT ( 'NONE',  ( -5.600965982043615732, -78.03957589888349844, -10.69184727915017064 ) ) ;
#9964 = CARTESIAN_POINT ( 'NONE',  ( 3.319188267144999926, -79.28328455456849611, 2.165402961309999874 ) ) ;
#9965 = DIRECTION ( 'NONE',  ( -1.000000000000000000, 0.000000000000000000, 0.000000000000000000 ) ) ;
#9966 = CARTESIAN_POINT ( 'NONE',  ( 0.5200116074403198230, -79.65885271342665419, -1.150702922115795612 ) ) ;
#9967 = CARTESIAN_POINT ( 'NONE',  ( -1.053645312779857068, -83.05505849742939972, 0.6765476259604800147 ) ) ;
#9968 = DIRECTION ( 'NONE',  ( 1.000000000000000000, 0.000000000000000000, -0.000000000000000000 ) ) ;
#9969 = CARTESIAN_POINT ( 'NONE',  ( -3.962812355711000212, -78.85171438276199751, -1.662781298490902161E-14 ) ) ;
#9970 = CARTESIAN_POINT ( 'NONE',  ( 9.708203932502000200, -79.25000000000000000, -7.053423027506000587 ) ) ;
#9971 = CARTESIAN_POINT ( 'NONE',  ( -1.164523129836848581, -78.06680908019323795, 0.5225932405203995712 ) ) ;
#9972 = EDGE_CURVE ( 'NONE', #37820, #14569, #39249, .T. ) ;
#9973 = DIRECTION ( 'NONE',  ( -0.7071067811865475727, 0.000000000000000000, -0.7071067811865475727 ) ) ;
#9974 = CARTESIAN_POINT ( 'NONE',  ( 4.659053635387349956, -79.76712042365360844, -8.083800990292457911 ) ) ;
#9975 = CARTESIAN_POINT ( 'NONE',  ( -1.000000000000000000, -75.20000000000000284, -7.200000000000000178 ) ) ;
#9976 = CARTESIAN_POINT ( 'NONE',  ( 1.363667439983781371, -79.56383901316905849, -0.6545495444765823123 ) ) ;
#9977 = CARTESIAN_POINT ( 'NONE',  ( 0.000000000000000000, -78.49999999999998579, -2.600000000000000089 ) ) ;
#9978 = FACE_OUTER_BOUND ( 'NONE', #748, .T. ) ;
#9979 = CARTESIAN_POINT ( 'NONE',  ( -0.9212224518321000533, -53.98045898127999465, -12.54670315977999984 ) ) ;
#9980 = CARTESIAN_POINT ( 'NONE',  ( -8.189132907799949734, -77.39413886308913959, 6.999642771075209602 ) ) ;
#9981 = CARTESIAN_POINT ( 'NONE',  ( 7.686941364994000381, -20.24527982330999976, 10.48774103564000093 ) ) ;
#9983 = CARTESIAN_POINT ( 'NONE',  ( 10.85730540529999999, -79.11169407763458139, 1.607151491820999922 ) ) ;
#9982 = CARTESIAN_POINT ( 'NONE',  ( 10.12290050126000196, -60.04999999958999979, 7.648026767103999646 ) ) ;
#9984 = CARTESIAN_POINT ( 'NONE',  ( -5.115276909939000305, -75.75838526971999443, -10.78423561930000041 ) ) ;
#9985 = ORIENTED_EDGE ( 'NONE', *, *, #30091, .F. ) ;
#9986 = B_SPLINE_SURFACE_WITH_KNOTS ( 'NONE', 3, 3, ( 
 ( #44842, #53998, #45148, #4397, #31530, #40410, #39811, #13238, #27109, #44253, #4699, #35972, #48979, #43971, #3522, #39531, #57826, #30940, #8521, #57535, #17094, #53115, #12662, #48691, #8234, #26237, #21809, #17383, #35370, #22094, #53395, #44542, #4096, #8145, #56875 ),
 ( #43883, #12003, #39439, #57446, #25854, #7854, #34702, #16143, #48314, #53016, #38277, #34120, #34415, #3712, #39145, #21138, #30273, #57154, #48036, #12284, #15850, #29982, #6987, #7566, #43299, #7278, #38855, #3429, #25566, #43012, #12569, #3149, #11431, #16719, #26144 ),
 ( #2569, #56297, #20570, #52163, #33838, #30566, #38569, #21431, #20851, #52733, #17005, #44165, #34987, #48599, #51876, #29695, #43586, #29411, #11719, #47464, #24992, #16432, #56583, #47745, #25280, #2854, #52444, #40693, #27967, #14109, #4966, #18262, #36256, #22681, #54277 ),
 ( #14394, #284, #53980, #5258, #41274, #45131, #17964, #46018, #13814, #859, #9400, #36835, #54848, #23266, #18842, #32106, #13519, #45723, #50437, #35652, #31513, #31813, #1144, #36549, #18555, #27678, #54570, #45425, #9690, #13220, #27390, #49855, #32392, #9987, #50148 ),
 ( #5539, #49559, #23549, #4380, #22974, #41563, #53681, #31215, #40984, #4682, #9104, #26797, #49253, #22381, #27093, #576, #8804, #44825, #40392, #58401, #35954, #15278, #51605, #10274, #6128, #10571, #46892, #23839, #48267, #33271, #24434, #46601, #25803, #28842, #28553 ),
 ( #28255, #20297, #11163, #6716, #29136, #41856, #33567, #24724, #47184, #14978, #14683, #16668, #5832, #34649, #30220, #42737, #24134, #52676, #55137, #38289, #32976, #42449, #32681, #51022, #56313, #15572, #12231, #50734, #42153, #51312, #7802, #1434, #43830, #56023, #6420 ),
 ( #2017, #1723, #19714, #2300, #20015, #37998, #19424, #46309, #10871, #37712, #55734, #19131, #37125, #37416, #55435, #18123, #26654, #34933, #4242, #31671, #3659, #49419, #26371, #39388, #22241, #40253, #36118, #31376, #8968, #8371, #21943, #54135, #13674, #57969, #49717 ),
 ( #53248, #49117, #9261, #57673, #145, #17827, #39955, #26953, #44985, #4540, #17229, #12798, #44389, #27246, #58264, #31080, #3941, #17525, #48829, #35514, #8668, #3378, #22542, #8090, #40554, #21372, #44689, #57393, #53543, #16953, #26086, #12515, #52966, #30514, #21662 ),
 ( #35816, #39667, #13378, #48542, #44110, #35219, #13082, #30797, #53843, #28118, #37277, #5694, #55000, #19286, #22832, #36987, #45875, #50882, #42010, #23703, #41716, #1579, #19571, #31965, #37571, #55586, #10428, #32252, #15136, #40844, #5986, #41131, #10142, #438, #725 ),
 ( #55291, #36406, #50296, #36696, #14550, #50009, #33132, #41426, #50589, #14256, #51174, #32542, #54713, #18702, #14839, #46168, #1292, #9554, #13968, #18994, #9848, #27828, #5408, #32835, #28411, #27538, #10729, #46458, #18414, #23994, #45286, #45580, #4834, #23415, #54433 ) ),
 .UNSPECIFIED., .F., .F., .F.,
 ( 4, 1, 1, 1, 1, 1, 1, 4 ),
 ( 4, 1, 1, 1, 1, 1, 1, 1, 1, 1, 1, 1, 1, 1, 1, 1, 1, 1, 1, 1, 1, 1, 1, 1, 1, 1, 1, 1, 1, 1, 1, 1, 4 ),
 ( -0.01000000000000000021, 0.000000000000000000, 0.1000000000000000056, 0.2000000000000000111, 0.2999999999999999889, 0.4000000000000000222, 0.5000000000000000000, 0.5100000000000000089 ),
 ( -0.02000000000000000042, 0.01250000000000000069, 0.04499999999999999833, 0.07749999999999999944, 0.1100000000000000006, 0.1424999999999999878, 0.1749999999999999889, 0.2074999999999999900, 0.2399999999999999911, 0.2725000000000000200, 0.3049999999999999933, 0.3375000000000000222, 0.3699999999999999956, 0.4025000000000000244, 0.4349999999999999978, 0.4675000000000000266, 0.5000000000000000000, 0.5324999999999999734, 0.5649999999999999467, 0.5975000000000000311, 0.6300000000000000044, 0.6624999999999999778, 0.6949999999999999512, 0.7275000000000000355, 0.7600000000000000089, 0.7924999999999999822, 0.8249999999999999556, 0.8575000000000000400, 0.8900000000000000133, 0.9224999999999999867, 0.9549999999999999600, 0.9874999999999000133, 1.020000000000000018 ),
 .UNSPECIFIED. ) ;
#9987 = CARTESIAN_POINT ( 'NONE',  ( -3.357614552245999917, -86.32224116883999443, 0.9482802779118000291 ) ) ;
#9988 = EDGE_CURVE ( 'NONE', #49218, #15698, #3660, .T. ) ;
#9989 = CIRCLE ( 'NONE', #577, 2.600000000000000089 ) ;
#9990 = CARTESIAN_POINT ( 'NONE',  ( 10.10893382724000134, -80.98827613352290200, -5.281770763473000230 ) ) ;
#9991 = CARTESIAN_POINT ( 'NONE',  ( 9.011045739978872149, -78.33204682128099705, -2.089134863993796998 ) ) ;
#9992 = CARTESIAN_POINT ( 'NONE',  ( -10.07627163191000008, -55.55000000278000272, -7.601397897754999633 ) ) ;
#9993 = CARTESIAN_POINT ( 'NONE',  ( -3.633103876188000125, -77.30293106922299273, 10.61219425078000000 ) ) ;
#9994 = CARTESIAN_POINT ( 'NONE',  ( 12.50000000000000000, -23.24999999758999536, -1.750000000000000000 ) ) ;
#9995 = CARTESIAN_POINT ( 'NONE',  ( -12.56594317825999951, -60.05000001354000005, 1.750000000000000000 ) ) ;
#9996 = CARTESIAN_POINT ( 'NONE',  ( 6.694424008027000106, -76.92929967898000143, -9.543441777632999390 ) ) ;
#9997 = CARTESIAN_POINT ( 'NONE',  ( -0.2794722982914999987, -79.14806235426497949, 9.887242051013000577 ) ) ;
#9998 = CARTESIAN_POINT ( 'NONE',  ( 9.472494285633610289, -80.99999999999998579, -5.606341685433056554 ) ) ;
#9999 = ORIENTED_EDGE ( 'NONE', *, *, #3856, .F. ) ;
#10000 = AXIS2_PLACEMENT_3D ( 'NONE', #12136, #7704, #54261 ) ;
#10001 = CARTESIAN_POINT ( 'NONE',  ( -3.062995278220659756, -0.9166666666665526098, 1.359963116106802650 ) ) ;
#10002 = CARTESIAN_POINT ( 'NONE',  ( 1.980584515756000030, -55.53514849873000259, -12.76303204337999908 ) ) ;
#10003 = CARTESIAN_POINT ( 'NONE',  ( -0.5980611300388000151, -79.57311332859899267, 9.505909450771000024 ) ) ;
#10004 = CARTESIAN_POINT ( 'NONE',  ( -1.250000000000000000, -67.52659999995799467, 0.000000000000000000 ) ) ;
#10005 = ORIENTED_EDGE ( 'NONE', *, *, #42111, .T. ) ;
#10006 = CIRCLE ( 'NONE', #50541, 1.750000000000000000 ) ;
#10007 = CARTESIAN_POINT ( 'NONE',  ( -12.92181194098999875, -57.04351820043999766, -2.062502994258999856 ) ) ;
#10008 = DIRECTION ( 'NONE',  ( 0.000000000000000000, -1.000000000000000000, 0.000000000000000000 ) ) ;
#10009 = ORIENTED_EDGE ( 'NONE', *, *, #20888, .T. ) ;
#10010 = CARTESIAN_POINT ( 'NONE',  ( 10.96171043400000045, -78.53938061935399162, -5.535041421897999747 ) ) ;
#10011 = CARTESIAN_POINT ( 'NONE',  ( 10.84815226135000010, -78.23216936534500121, -1.481085459616000133 ) ) ;
#10012 = FACE_OUTER_BOUND ( 'NONE', #6204, .T. ) ;
#10013 = VERTEX_POINT ( 'NONE', #38703 ) ;
#10014 = CARTESIAN_POINT ( 'NONE',  ( 12.00000000000000000, -79.14999999999999147, 0.000000000000000000 ) ) ;
#10015 =( LENGTH_UNIT ( ) NAMED_UNIT ( * ) SI_UNIT ( .MILLI., .METRE. ) );
#10016 = B_SPLINE_CURVE_WITH_KNOTS ( 'NONE', 3,
 ( #54264, #28543, #36533, #55423, #14671, #847, #28242, #10262, #41845, #54557, #50135, #45712, #32966, #37111, #27953, #272 ),
 .UNSPECIFIED., .F., .F.,
 ( 4, 2, 2, 2, 2, 2, 2, 4 ),
 ( 0.000000000000000000, 0.2499999999999996669, 0.3750000000000010547, 0.4375000000000017764, 0.5000000000000025535, 0.6250000000000015543, 0.7500000000000006661, 1.000000000000000000 ),
 .UNSPECIFIED. ) ;
#10017 = CARTESIAN_POINT ( 'NONE',  ( -2.116314338179000387, -79.99807427152899209, -9.535298106756000536 ) ) ;
#10018 = VERTEX_POINT ( 'NONE', #1846 ) ;
#10019 = CARTESIAN_POINT ( 'NONE',  ( 0.000000000000000000, -5.899999999999999467, 0.000000000000000000 ) ) ;
#10020 = CARTESIAN_POINT ( 'NONE',  ( 2.343379474233999726, -79.93084841004029784, 10.44606179296999926 ) ) ;
#10021 = CARTESIAN_POINT ( 'NONE',  ( 4.706446445480565177E-05, -80.72503824655814242, -10.81748136418979556 ) ) ;
#10022 = CARTESIAN_POINT ( 'NONE',  ( -4.342561293556999935, -77.71725194988499652, -8.443909622126001935 ) ) ;
#10023 = CARTESIAN_POINT ( 'NONE',  ( 0.000000000000000000, -0.5000000000000000000, 0.000000000000000000 ) ) ;
#10024 = CARTESIAN_POINT ( 'NONE',  ( -0.9677429597868729694, -80.15535212655082375, -0.7945947339589979341 ) ) ;
#10025 = CARTESIAN_POINT ( 'NONE',  ( -0.2678032734925760439, -16.78567224710776529, -12.70526550769186258 ) ) ;
#10026 = CARTESIAN_POINT ( 'NONE',  ( 7.368185037057407349, -79.90209409743945912, 5.615580762807375947 ) ) ;
#10027 = CARTESIAN_POINT ( 'NONE',  ( 1.495278353479605249, -78.08869844104306424, -0.2055598165236604546 ) ) ;
#10028 =( REPRESENTATION_RELATIONSHIP ('NONE','NONE', #58051, #1422 ) REPRESENTATION_RELATIONSHIP_WITH_TRANSFORMATION ( #21045 )SHAPE_REPRESENTATION_RELATIONSHIP( ) );
#10029 = CARTESIAN_POINT ( 'NONE',  ( -1.060114799228036198, -80.51145833248038741, -3.910610943235043102 ) ) ;
#10030 = EDGE_LOOP ( 'NONE', ( #41450, #9332, #23209 ) ) ;
#10031 = CARTESIAN_POINT ( 'NONE',  ( 9.199999999968001774, -80.60000000003199716, -3.388768808660000233E-10 ) ) ;
#10032 = CARTESIAN_POINT ( 'NONE',  ( 1.328206530128999807, -76.65093621910000365, -12.23810562210000086 ) ) ;
#10033 = CIRCLE ( 'NONE', #4372, 1.750000000000000000 ) ;
#10034 = CARTESIAN_POINT ( 'NONE',  ( 2.521648037650194407, -2.160692059289706979, 2.456016280877232560 ) ) ;
#10035 = CARTESIAN_POINT ( 'NONE',  ( 12.58338334675000070, -20.25199022618999933, 1.667961445601999992 ) ) ;
#10036 = CARTESIAN_POINT ( 'NONE',  ( 4.750030159171999777, -78.67398341331998779, -11.30647155123999958 ) ) ;
#10037 = CARTESIAN_POINT ( 'NONE',  ( 11.13784153760999907, -76.41850151303799521, 5.174080857020999957 ) ) ;
#10038 = CIRCLE ( 'NONE', #6998, 11.05000000000000071 ) ;
#10039 = CARTESIAN_POINT ( 'NONE',  ( -3.451066577810062874, -1.796365364732098957, -0.5702761658243397092 ) ) ;
#10040 = VECTOR ( 'NONE', #26302, 1000.000000000000000 ) ;
#10041 = ADVANCED_FACE ( 'NONE', ( #32804 ), #30974, .F. ) ;
#10042 = CARTESIAN_POINT ( 'NONE',  ( 12.50000000000000000, -24.68359816828999698, 1.003641515614000168 ) ) ;
#10043 = CARTESIAN_POINT ( 'NONE',  ( 11.37043047323898293, -77.27374362828227561, -3.893187843879513110 ) ) ;
#10044 = CARTESIAN_POINT ( 'NONE',  ( -0.2721098858049000313, -79.12693104276253564, 11.21356619464000026 ) ) ;
#10045 = VECTOR ( 'NONE', #30272, 1000.000000000000000 ) ;
#10046 = ORIENTED_EDGE ( 'NONE', *, *, #45514, .T. ) ;
#10047 = CARTESIAN_POINT ( 'NONE',  ( 1.160935205181999885, -81.72722500425999215, -0.6914862246935000734 ) ) ;
#10048 = CARTESIAN_POINT ( 'NONE',  ( -2.891062785949999991, -76.92985585977308460, -9.145460139217000517 ) ) ;
#10049 = DIRECTION ( 'NONE',  ( -1.000000000000000000, 0.000000000000000000, 0.000000000000000000 ) ) ;
#10050 = CARTESIAN_POINT ( 'NONE',  ( -0.9995835529977281642, -82.94791666666661456, 0.7681833999686391579 ) ) ;
#10051 = CARTESIAN_POINT ( 'NONE',  ( 0.2209175225483000216, -3.423916625800000002, -3.863862947105999979 ) ) ;
#10052 = CARTESIAN_POINT ( 'NONE',  ( -3.532272164985999829, -77.47550115664098769, 11.39993665757999963 ) ) ;
#10053 = CARTESIAN_POINT ( 'NONE',  ( -5.638451105654999296, -78.28216660084999035, -7.807757622656001040 ) ) ;
#10054 = CARTESIAN_POINT ( 'NONE',  ( 8.883745460416154316, -76.00626841134847211, 7.692327491078800428 ) ) ;
#10055 = CARTESIAN_POINT ( 'NONE',  ( 3.449307203194000415, -79.30855784779899409, 10.47874105986000082 ) ) ;
#10056 = CARTESIAN_POINT ( 'NONE',  ( 1.353569424327059512, -86.10000000000019327, 3.118950113984905403 ) ) ;
#10057 = EDGE_LOOP ( 'NONE', ( #9186, #29101 ) ) ;
#10058 = CARTESIAN_POINT ( 'NONE',  ( 7.836763323858055408, -17.69488832272547185, -9.850488778970140302 ) ) ;
#10059 = EDGE_CURVE ( 'NONE', #20388, #52990, #37538, .T. ) ;
#10060 = CARTESIAN_POINT ( 'NONE',  ( 9.708203932494999577, -79.25000000000000000, 7.053423027515000499 ) ) ;
#10061 = B_SPLINE_CURVE_WITH_KNOTS ( 'NONE', 3,
 ( #9537, #13658, #44968, #35795, #53825, #22222, #31358, #4523, #41115, #4816, #21926, #40826, #17212, #53232, #22524 ),
 .UNSPECIFIED., .F., .F.,
 ( 4, 1, 1, 1, 1, 1, 1, 1, 1, 1, 1, 1, 4 ),
 ( 0.000000000000000000, 0.08333611588665000569, 0.1666676715620999949, 0.2500039875833999781, 0.3333306964953999807, 0.4166666792817999565, 0.4999999999924999994, 0.5833333197091999933, 0.6666692694150000431, 0.7499959719902999922, 0.8333323089881000678, 0.9166638425153998959, 1.000000000000000000 ),
 .UNSPECIFIED. ) ;
#10062 = CARTESIAN_POINT ( 'NONE',  ( -9.871730464199000465, -79.95445777275799060, 4.797141237513000256 ) ) ;
#10063 = CARTESIAN_POINT ( 'NONE',  ( -10.25000000000000000, -82.09999999999999432, 0.000000000000000000 ) ) ;
#10064 = CARTESIAN_POINT ( 'NONE',  ( -11.68767212001980127, -77.87916666666664867, 3.140974612311317138 ) ) ;
#10065 = CARTESIAN_POINT ( 'NONE',  ( 1.980584515756000030, -23.26485150094000076, 12.76303204340999997 ) ) ;
#10066 = CARTESIAN_POINT ( 'NONE',  ( 7.633403241821000051, -18.61350283651999860, -10.18127013549000104 ) ) ;
#10067 = CARTESIAN_POINT ( 'NONE',  ( -5.827740701927429434, -78.31867367200482022, 10.39237278454248958 ) ) ;
#10068 = ORIENTED_EDGE ( 'NONE', *, *, #28273, .F. ) ;
#10069 = CARTESIAN_POINT ( 'NONE',  ( 5.709935245961999861, -78.54106733076498870, 9.573465417320001336 ) ) ;
#10070 = LINE ( 'NONE', #22762, #22004 ) ;
#10071 = CARTESIAN_POINT ( 'NONE',  ( -2.813789756862300262, -79.89583333333330017, 10.47020627418438465 ) ) ;
#10072 = CARTESIAN_POINT ( 'NONE',  ( 10.70395128840999988, -78.11714908313399519, -0.4932637219220999958 ) ) ;
#10074 = CARTESIAN_POINT ( 'NONE',  ( -0.8938566341920096692, -81.53894037312349496, 0.8733612504233605467 ) ) ;
#10073 = CARTESIAN_POINT ( 'NONE',  ( 0.6718344995053999735, -81.32557530614698749, -1.135431202457000133 ) ) ;
#10075 = DIRECTION ( 'NONE',  ( 0.000000000000000000, -1.000000000000000000, 0.000000000000000000 ) ) ;
#10076 = DIRECTION ( 'NONE',  ( 0.000000000000000000, -0.7071067811866525998, -0.7071067811864425456 ) ) ;
#10077 = EDGE_CURVE ( 'NONE', #24848, #40579, #6246, .T. ) ;
#10078 = AXIS2_PLACEMENT_3D ( 'NONE', #13489, #13189, #31479 ) ;
#10079 = CARTESIAN_POINT ( 'NONE',  ( 1.306140625255000076, -78.33423293213999727, 0.06913166271809000063 ) ) ;
#10080 = CARTESIAN_POINT ( 'NONE',  ( -9.009247259181927703, -79.97916666666664298, 2.421167930323307793 ) ) ;
#10081 = CIRCLE ( 'NONE', #5349, 10.14999999999999858 ) ;
#10082 = CARTESIAN_POINT ( 'NONE',  ( 0.2613628514566687655, -79.57699692416433379, -10.97267097489929810 ) ) ;
#10083 = DIRECTION ( 'NONE',  ( 0.7071067811865474617, 0.000000000000000000, -0.7071067811865474617 ) ) ;
#10084 = ORIENTED_EDGE ( 'NONE', *, *, #3384, .F. ) ;
#10085 = AXIS2_PLACEMENT_3D ( 'NONE', #58247, #49991, #54414 ) ;
#10086 = VERTEX_POINT ( 'NONE', #37833 ) ;
#10087 = CARTESIAN_POINT ( 'NONE',  ( 6.682297893293000612, -79.06613998579798874, -6.800905403285999462 ) ) ;
#10088 = CARTESIAN_POINT ( 'NONE',  ( 9.947560812465606972, -78.81912883275374782, -4.075256179118199817 ) ) ;
#10089 = AXIS2_PLACEMENT_3D ( 'NONE', #30674, #27426, #49596 ) ;
#10090 = ORIENTED_EDGE ( 'NONE', *, *, #29266, .F. ) ;
#10091 = CARTESIAN_POINT ( 'NONE',  ( 0.000000000000000000, -75.67500000000001137, 0.000000000000000000 ) ) ;
#10092 = CARTESIAN_POINT ( 'NONE',  ( 3.103766772394584539, -84.05729167874393681, 1.491608599317842065 ) ) ;
#10093 = CARTESIAN_POINT ( 'NONE',  ( 8.284635637516000628, -61.84861451525000575, 9.778492910201000754 ) ) ;
#10094 = CARTESIAN_POINT ( 'NONE',  ( 11.41797009976014365, -76.32802149572208350, 4.296752358342962985 ) ) ;
#10095 = CARTESIAN_POINT ( 'NONE',  ( 11.81395210335005608, -77.31316753185872415, 1.987591828291500384 ) ) ;
#10096 = CARTESIAN_POINT ( 'NONE',  ( -11.20683111097000051, -79.83726082427419612, -0.4743912329535999728 ) ) ;
#10097 = ORIENTED_EDGE ( 'NONE', *, *, #17538, .T. ) ;
#10098 = CARTESIAN_POINT ( 'NONE',  ( -10.41172477448170497, -23.52013115057688353, 7.610718073406644635 ) ) ;
#10099 = ORIENTED_EDGE ( 'NONE', *, *, #30027, .F. ) ;
#10100 = CARTESIAN_POINT ( 'NONE',  ( 9.249668415229836071, -77.35072839144281431, 0.08481753625212125336 ) ) ;
#10101 = CARTESIAN_POINT ( 'NONE',  ( 9.507661145905998978, -77.57741896181198626, -5.611464101879999333 ) ) ;
#10102 = CARTESIAN_POINT ( 'NONE',  ( 11.00000000012632739, -76.04999999999999716, 1.151917305286630722 ) ) ;
#10103 = CARTESIAN_POINT ( 'NONE',  ( 0.7608607662309999631, -78.15598835058560212, -1.424185669224000028 ) ) ;
#10104 = CARTESIAN_POINT ( 'NONE',  ( -11.68767212001978706, -77.42083333333333428, -3.140974612311364655 ) ) ;
#10105 = CARTESIAN_POINT ( 'NONE',  ( 0.6677177572643692161, -2.141389681057874306, -3.206128740696444268 ) ) ;
#10106 = CARTESIAN_POINT ( 'NONE',  ( -0.6580604922749000441, -79.42147124369999744, -1.488334326434000099 ) ) ;
#10107 = CARTESIAN_POINT ( 'NONE',  ( 3.979199129784999567, -82.49282046129098944, 0.4013858386831000158 ) ) ;
#10108 = CARTESIAN_POINT ( 'NONE',  ( -8.603527126503999867, -78.37620263911298935, 6.757746467621000619 ) ) ;
#10109 = EDGE_CURVE ( 'NONE', #46363, #49572, #10310, .T. ) ;
#10110 = CARTESIAN_POINT ( 'NONE',  ( -7.646944885436999684, -23.19635956544000166, -10.19022188674999896 ) ) ;
#10111 = CARTESIAN_POINT ( 'NONE',  ( 12.87024489159000140, -59.58461666436000570, -2.062597265787999845 ) ) ;
#10112 = CARTESIAN_POINT ( 'NONE',  ( 1.948737297906999899, -85.02368520868098756, -3.014327109634999502 ) ) ;
#10113 = VERTEX_POINT ( 'NONE', #2991 ) ;
#10114 = EDGE_CURVE ( 'NONE', #37542, #38384, #22491, .T. ) ;
#10115 = CARTESIAN_POINT ( 'NONE',  ( 4.822953412158000219, -79.03010945140999866, -11.45989370067999857 ) ) ;
#10116 = CARTESIAN_POINT ( 'NONE',  ( 7.124885535347999621, -76.25294931795998821, -8.714606029085999239 ) ) ;
#10117 = CARTESIAN_POINT ( 'NONE',  ( 10.05221862648209274, -77.87898788867025246, 3.817045573893846022 ) ) ;
#10118 = CARTESIAN_POINT ( 'NONE',  ( 2.956870837876000468, -78.92095621112599702, 11.44999256673999888 ) ) ;
#10119 = LINE ( 'NONE', #54980, #57009 ) ;
#10120 = VECTOR ( 'NONE', #47455, 1000.000000000000114 ) ;
#10122 = DIRECTION ( 'NONE',  ( 0.000000000000000000, 1.000000000000000000, 0.000000000000000000 ) ) ;
#10121 = CARTESIAN_POINT ( 'NONE',  ( 10.61050599188999932, -78.32876026662599145, -2.901234667509999809 ) ) ;
#10123 = CARTESIAN_POINT ( 'NONE',  ( -1.707856248730948989, -3.165271797717385205, 3.077356143116399601 ) ) ;
#10124 = CARTESIAN_POINT ( 'NONE',  ( 6.018017909193484449, -80.92806936818854524, 8.908428929804006913 ) ) ;
#10125 = CARTESIAN_POINT ( 'NONE',  ( -8.883074525067000238, -78.55234872708999205, 3.114832498031999908 ) ) ;
#10126 = DIRECTION ( 'NONE',  ( -0.6562721000522208081, 0.7545243075561237633, 7.878854448478247525E-10 ) ) ;
#10127 = CARTESIAN_POINT ( 'NONE',  ( -10.89229298341999908, -77.37409373610799435, 2.369082973246999568 ) ) ;
#10128 = DIRECTION ( 'NONE',  ( 0.000000000000000000, -1.000000000000000000, 0.000000000000000000 ) ) ;
#10129 = CARTESIAN_POINT ( 'NONE',  ( -5.340898366833999766, -80.30592291261719140, 9.777117507691999165 ) ) ;
#10130 = EDGE_LOOP ( 'NONE', ( #11461, #46846, #31032 ) ) ;
#10131 = CYLINDRICAL_SURFACE ( 'NONE', #13634, 3.000000000000000000 ) ;
#10132 = ADVANCED_FACE ( 'NONE', ( #11854 ), #4544, .F. ) ;
#10133 = AXIS2_PLACEMENT_3D ( 'NONE', #11816, #47846, #21240 ) ;
#10134 = CARTESIAN_POINT ( 'NONE',  ( -4.999999999872000167, -80.49999999987198862, 4.857408280386999624E-10 ) ) ;
#10135 = CARTESIAN_POINT ( 'NONE',  ( 11.19180402071999936, -77.45363786841799936, 0.7494220128532999015 ) ) ;
#10136 = CARTESIAN_POINT ( 'NONE',  ( -6.920341278396000106, -79.38025603508899053, -8.518972542050999408 ) ) ;
#10137 = AXIS2_PLACEMENT_3D ( 'NONE', #15203, #28773, #1944 ) ;
#10138 = CARTESIAN_POINT ( 'NONE',  ( 9.778543098479998363, -25.04857981702999936, -8.284584910395000890 ) ) ;
#10139 = CARTESIAN_POINT ( 'NONE',  ( 3.979318866615385364, -82.41927081334193872, -0.5157333616409632837 ) ) ;
#10140 = CARTESIAN_POINT ( 'NONE',  ( 2.598748023862139878, -1.903594524732164617, 1.996140164127287786 ) ) ;
#10141 = CARTESIAN_POINT ( 'NONE',  ( -9.697390092234948966, -53.82767731322027771, -8.266602378481318070 ) ) ;
#10142 = CARTESIAN_POINT ( 'NONE',  ( -3.413772187608999698, -86.04119503318798934, 2.399116304729999705 ) ) ;
#10143 = CARTESIAN_POINT ( 'NONE',  ( 7.954951288349001004, -18.75000000000000000, 9.722718241315000398 ) ) ;
#10144 = CARTESIAN_POINT ( 'NONE',  ( -11.40747292386999945, -78.95515814038999736, 6.126595231985000112 ) ) ;
#10145 = CARTESIAN_POINT ( 'NONE',  ( -7.743768518152000624, -77.34125689393900416, -8.177286450628999503 ) ) ;
#10146 = CARTESIAN_POINT ( 'NONE',  ( -0.5432945554243000519, -81.36589858243000606, -1.398152719143000100 ) ) ;
#10147 = CARTESIAN_POINT ( 'NONE',  ( 0.3509080281557999670, -79.16638555667999810, -1.272612056386999813 ) ) ;
#10148 = CARTESIAN_POINT ( 'NONE',  ( -7.850076763451487416, -24.31471441246267062, 9.837736658179169424 ) ) ;
#10149 = CARTESIAN_POINT ( 'NONE',  ( -0.6588690626962807606, -81.66089795315696165, 1.359795660138139350 ) ) ;
#10150 = CARTESIAN_POINT ( 'NONE',  ( -12.54976804513999866, -61.84775476195000010, -0.05637402076004000007 ) ) ;
#10151 = CARTESIAN_POINT ( 'NONE',  ( -7.590654613722642274, -80.16307491009121122, -7.611717479442802414 ) ) ;
#10152 = LINE ( 'NONE', #45593, #22107 ) ;
#10153 = CARTESIAN_POINT ( 'NONE',  ( 1.500000000000001110, -78.13958333333334849, -0.1963495408493590721 ) ) ;
#10154 = VERTEX_POINT ( 'NONE', #35409 ) ;
#10155 = CARTESIAN_POINT ( 'NONE',  ( 13.99609303072000088, -45.84137733102999590, 3.303213538507999633E-05 ) ) ;
#10156 = DIRECTION ( 'NONE',  ( 0.000000000000000000, 0.000000000000000000, 1.000000000000000000 ) ) ;
#10157 = CARTESIAN_POINT ( 'NONE',  ( 7.779872909029999839, -79.77157567883000411, 7.821464818102998429 ) ) ;
#10158 = DIRECTION ( 'NONE',  ( 0.000000000000000000, 1.000000000000000000, 0.000000000000000000 ) ) ;
#10159 = ORIENTED_EDGE ( 'NONE', *, *, #54449, .T. ) ;
#10160 = ORIENTED_EDGE ( 'NONE', *, *, #1337, .F. ) ;
#10161 = CARTESIAN_POINT ( 'NONE',  ( -1.098028760202000020, -82.10785915155000225, -1.045495904960999978 ) ) ;
#10162 = ORIENTED_EDGE ( 'NONE', *, *, #33398, .F. ) ;
#10163 = AXIS2_PLACEMENT_3D ( 'NONE', #54967, #41396, #36374 ) ;
#10165 = EDGE_CURVE ( 'NONE', #38582, #10018, #53440, .T. ) ;
#10164 = VERTEX_POINT ( 'NONE', #16282 ) ;
#10166 = CARTESIAN_POINT ( 'NONE',  ( 0.4450739772391999471, -17.12186785197999939, 12.43586747594999942 ) ) ;
#10167 = CARTESIAN_POINT ( 'NONE',  ( 0.000000000000000000, -73.00000000000001421, 0.000000000000000000 ) ) ;
#10168 = CARTESIAN_POINT ( 'NONE',  ( 0.000000000000000000, 0.000000000000000000, 0.000000000000000000 ) ) ;
#10169 = CARTESIAN_POINT ( 'NONE',  ( -0.3139459252241110221, -82.05312498411764466, -3.417871720250339251 ) ) ;
#10170 = CARTESIAN_POINT ( 'NONE',  ( 5.142492926713607027, -78.27207518130937558, -7.688654696769305019 ) ) ;
#10171 = CARTESIAN_POINT ( 'NONE',  ( 8.596418555780450887, -78.19791666666668561, -6.606377239730321982 ) ) ;
#10172 = AXIS2_PLACEMENT_3D ( 'NONE', #5713, #15457, #28431 ) ;
#10173 = ORIENTED_EDGE ( 'NONE', *, *, #15089, .F. ) ;
#10174 = ORIENTED_EDGE ( 'NONE', *, *, #26394, .T. ) ;
#10175 = DIRECTION ( 'NONE',  ( -1.000000000000000000, 0.000000000000000000, 0.000000000000000000 ) ) ;
#10176 = DIRECTION ( 'NONE',  ( -1.000000000000000000, 0.000000000000000000, 0.000000000000000000 ) ) ;
#10177 = DIRECTION ( 'NONE',  ( -1.205798305761979436E-11, -1.868137355152963707E-07, -0.9999999999999824585 ) ) ;
#10178 = CARTESIAN_POINT ( 'NONE',  ( 1.689459950995380044, -61.09188253861194084, -12.71013585614447194 ) ) ;
#10179 = CARTESIAN_POINT ( 'NONE',  ( -9.282419925074000489, -77.23309266417999197, -2.829762163499999872 ) ) ;
#10180 = DIRECTION ( 'NONE',  ( -1.000000000000000000, 0.000000000000000000, 0.000000000000000000 ) ) ;
#10181 = CARTESIAN_POINT ( 'NONE',  ( -10.01332844637000008, -23.28056692670000061, 7.654537085030000299 ) ) ;
#10182 = CARTESIAN_POINT ( 'NONE',  ( 9.024219425886000678, -76.52363952651001000, -8.086445476350000661 ) ) ;
#10183 = CARTESIAN_POINT ( 'NONE',  ( 1.476447168807000221, -80.98636901320000447, 0.5783644924166000401 ) ) ;
#10184 = DIRECTION ( 'NONE',  ( 0.000000000000000000, 1.000000000000000000, 0.000000000000000000 ) ) ;
#10185 = B_SPLINE_CURVE_WITH_KNOTS ( 'NONE', 3,
 ( #1624, #37904, #28456, #46504, #37320, #5738, #42638, #15479, #15764, #55337, #33470, #42352, #47376, #23745, #33759, #42052, #19615, #37613 ),
 .UNSPECIFIED., .F., .F.,
 ( 4, 2, 2, 2, 2, 2, 2, 2, 4 ),
 ( 0.000000000000000000, 0.1250000000000000000, 0.2500000000000000000, 0.3750000000000000000, 0.5000000000000000000, 0.6250000000000000000, 0.7500000000000000000, 0.8750000000000000000, 1.000000000000000000 ),
 .UNSPECIFIED. ) ;
#10186 = EDGE_CURVE ( 'NONE', #2185, #52707, #38552, .T. ) ;
#10187 = CARTESIAN_POINT ( 'NONE',  ( 3.494712293981999895, -79.57543510685839294, 2.279705814203000003 ) ) ;
#10188 = CARTESIAN_POINT ( 'NONE',  ( -2.895922040489999905, -80.16179448218190373, 10.88681414971999928 ) ) ;
#10189 = CARTESIAN_POINT ( 'NONE',  ( -7.502741683071000089, -78.12516001420199530, -6.127813063941999872 ) ) ;
#10190 = DIRECTION ( 'NONE',  ( 1.000000000000000000, 0.000000000000000000, 0.000000000000000000 ) ) ;
#10191 = CARTESIAN_POINT ( 'NONE',  ( -3.405576000112999768, -81.65107046129099899, 0.9932798323076000857 ) ) ;
#10192 = CARTESIAN_POINT ( 'NONE',  ( 0.5704417986824000808, -78.88205912477799586, -1.205475954488999912 ) ) ;
#10193 = DIRECTION ( 'NONE',  ( 0.000000000000000000, -1.000000000000000000, 0.000000000000000000 ) ) ;
#10194 = CARTESIAN_POINT ( 'NONE',  ( -1.980584515752000119, -23.26485146623999967, 12.76303204602000108 ) ) ;
#10195 = CARTESIAN_POINT ( 'NONE',  ( 0.6295237254636258939, -79.16666666666665719, -1.092232985442821658 ) ) ;
#10196 = VERTEX_POINT ( 'NONE', #52583 ) ;
#10197 = CARTESIAN_POINT ( 'NONE',  ( -2.169990332168064473, -3.499999999999999112, -2.587771324678439733 ) ) ;
#10198 = CARTESIAN_POINT ( 'NONE',  ( 0.5999381870721750554, -18.76980390685249844, -10.98362755083787334 ) ) ;
#10199 = DIRECTION ( 'NONE',  ( -1.156375342703999878E-13, -0.000000000000000000, -1.000000000000000000 ) ) ;
#10200 = ADVANCED_FACE ( 'NONE', ( #8565 ), #53154, .F. ) ;
#10201 = CARTESIAN_POINT ( 'NONE',  ( 3.042616888044999968, -79.17893513191498300, 9.264577239222999694 ) ) ;
#10202 = CARTESIAN_POINT ( 'NONE',  ( 12.54435570283317780, -18.47582218226679274, -1.733918077769244448 ) ) ;
#10203 = CARTESIAN_POINT ( 'NONE',  ( 8.082598614575715601, -79.40746475772557744, 7.120178426330225463 ) ) ;
#10204 = FACE_OUTER_BOUND ( 'NONE', #55768, .T. ) ;
#10205 = CARTESIAN_POINT ( 'NONE',  ( 0.000000000000000000, -46.43897132165000130, 0.000000000000000000 ) ) ;
#10206 = CARTESIAN_POINT ( 'NONE',  ( 9.419185743363001961, -77.38288739614199585, -6.195553150604999892 ) ) ;
#10207 = CARTESIAN_POINT ( 'NONE',  ( 1.294956495611000014, -82.10782256861200779, -0.9466954001098000226 ) ) ;
#10208 = CARTESIAN_POINT ( 'NONE',  ( -1.247385801055000076, -17.52277743740000204, 12.50301438876999960 ) ) ;
#10209 = CARTESIAN_POINT ( 'NONE',  ( 1.222863591967999985, -77.88544661340898756, 9.333584474513999751 ) ) ;
#10211 = CARTESIAN_POINT ( 'NONE',  ( -1.997276839918484148, -2.927083333333333481, 2.598917237794077018 ) ) ;
#10210 = CARTESIAN_POINT ( 'NONE',  ( -3.926978343844999664, -82.86303720588698241, 0.5336957764997000142 ) ) ;
#10212 = CARTESIAN_POINT ( 'NONE',  ( 7.507056363060000237, -79.82915194988498797, -5.572808305725000189 ) ) ;
#10213 = CARTESIAN_POINT ( 'NONE',  ( -0.6295237254636235624, -82.58333333333332860, -1.092232985442822990 ) ) ;
#10214 = CARTESIAN_POINT ( 'NONE',  ( -1.172662378873000177, -80.19593403531600018, -0.6045068694098000295 ) ) ;
#10215 = CARTESIAN_POINT ( 'NONE',  ( 11.79999999988000070, -23.14999999478999726, -0.5999999998848000171 ) ) ;
#10216 = CARTESIAN_POINT ( 'NONE',  ( 4.888751005523273463, -79.67187500068790484, -7.978256377688620837 ) ) ;
#10217 = CIRCLE ( 'NONE', #58293, 9.199999999999999289 ) ;
#10218 = CARTESIAN_POINT ( 'NONE',  ( 3.999999999999674927, -78.69999999999997442, -4.898587196589014454E-16 ) ) ;
#10219 = ORIENTED_EDGE ( 'NONE', *, *, #51188, .F. ) ;
#10220 = ORIENTED_EDGE ( 'NONE', *, *, #37768, .T. ) ;
#10221 = CARTESIAN_POINT ( 'NONE',  ( -7.858171174022000827, -79.13333109285899525, 9.108036400545000077 ) ) ;
#10222 = FACE_OUTER_BOUND ( 'NONE', #41055, .T. ) ;
#10223 = CARTESIAN_POINT ( 'NONE',  ( 0.000000000000000000, 4.040000000000000036, 0.000000000000000000 ) ) ;
#10224 = EDGE_LOOP ( 'NONE', ( #9102, #12811, #5581, #31731 ) ) ;
#10225 = CARTESIAN_POINT ( 'NONE',  ( -9.926966510012999123, -77.57657859425000879, 6.625016102256999773 ) ) ;
#10226 = ORIENTED_EDGE ( 'NONE', *, *, #37737, .F. ) ;
#10228 = ADVANCED_FACE ( 'NONE', ( #48446 ), #17828, .T. ) ;
#10227 = ORIENTED_EDGE ( 'NONE', *, *, #33846, .T. ) ;
#10229 = ORIENTED_EDGE ( 'NONE', *, *, #10230, .T. ) ;
#10230 = EDGE_CURVE ( 'NONE', #44757, #47059, #34955, .T. ) ;
#10231 = CARTESIAN_POINT ( 'NONE',  ( 1.666457266735999809, -79.69568553133959199, 3.131212234982999831 ) ) ;
#10232 = CARTESIAN_POINT ( 'NONE',  ( 10.42531124908000173, -60.06485148440999922, 7.624341765471999821 ) ) ;
#10233 = B_SPLINE_SURFACE_WITH_KNOTS ( 'NONE', 3, 3, ( 
 ( #52633, #12190, #20757, #30749 ),
 ( #52066, #38758, #29882, #11620 ),
 ( #25760, #29596, #56776, #47652 ),
 ( #36647, #26604, #18363, #31324 ),
 ( #23070, #26327, #9502, #17477 ),
 ( #4492, #49071, #49958, #45234 ),
 ( #35766, #57919, #35466, #44935 ),
 ( #21897, #54665, #26907, #48783 ),
 ( #8327, #53493, #36355, #49367 ),
 ( #676, #40791, #27488, #53795 ),
 ( #54384, #13921, #58214, #8917 ),
 ( #18072, #36066, #97, #22490 ),
 ( #45530, #18660, #41084, #54086 ),
 ( #13329, #13624, #8619, #44341 ),
 ( #5074, #49665, #13035, #31914 ),
 ( #3894, #31622, #40501, #9208 ),
 ( #385, #14206, #39905, #22191 ) ),
 .UNSPECIFIED., .F., .F., .F.,
 ( 4, 1, 1, 1, 1, 1, 1, 1, 1, 1, 1, 1, 1, 1, 4 ),
 ( 4, 4 ),
 ( -0.01011400514350000064, 0.000000000000000000, 0.08333333333333001192, 0.1666666666667000196, 0.2500000000000000000, 0.3333333333333000081, 0.4166666666666999919, 0.5000000000000000000, 0.5833333333333000637, 0.6666666666667000474, 0.7500000000000000000, 0.8333333333333000637, 0.9166666666667000474, 1.000000000000000000, 1.010365328128000062 ),
 ( -0.3559705546945999832, 1.357612395619000045 ),
 .UNSPECIFIED. ) ;
#10234 = ORIENTED_EDGE ( 'NONE', *, *, #40514, .T. ) ;
#10235 = CARTESIAN_POINT ( 'NONE',  ( 0.000000000000000000, -75.10000000284179578, 6.100000002841999169 ) ) ;
#10236 = ORIENTED_EDGE ( 'NONE', *, *, #2040, .F. ) ;
#10237 = FACE_OUTER_BOUND ( 'NONE', #39176, .T. ) ;
#10238 = CARTESIAN_POINT ( 'NONE',  ( 4.545340142815106788, -77.68611479733223746, 8.574013691167166940 ) ) ;
#10239 = CARTESIAN_POINT ( 'NONE',  ( -6.332001867507876192, -79.79999999999999716, -10.05727774830502952 ) ) ;
#10240 = CARTESIAN_POINT ( 'NONE',  ( 0.000000000000000000, -74.64999999999999147, 0.000000000000000000 ) ) ;
#10241 = CARTESIAN_POINT ( 'NONE',  ( -11.38694148309949128, -78.98049139715394062, -4.554723408025081355 ) ) ;
#10242 = AXIS2_PLACEMENT_3D ( 'NONE', #43428, #53436, #12698 ) ;
#10243 = CARTESIAN_POINT ( 'NONE',  ( 8.154961773732001262, -76.00829183880699702, 7.653135223926000208 ) ) ;
#10244 = CARTESIAN_POINT ( 'NONE',  ( -8.768124086712999699, -59.94999999969000015, 7.919595949288999570 ) ) ;
#10245 = CARTESIAN_POINT ( 'NONE',  ( -7.718346056099999686, -58.54888345776999614, -10.07719973192999952 ) ) ;
#10246 = CARTESIAN_POINT ( 'NONE',  ( 7.205376029061446808, -78.79611051935776800, -5.800537444989805280 ) ) ;
#10247 = CARTESIAN_POINT ( 'NONE',  ( -0.5999381870721927079, -23.23019609315233325, -10.98362755083787690 ) ) ;
#10248 = ADVANCED_FACE ( 'NONE', ( #45776 ), #36012, .F. ) ;
#10249 = CARTESIAN_POINT ( 'NONE',  ( -1.213636094208999872, -80.66834171116700247, -0.5527192377158001158 ) ) ;
#10250 = CARTESIAN_POINT ( 'NONE',  ( -7.396665944778026969, -80.16677562652540701, -8.142152547388292305 ) ) ;
#10251 = DIRECTION ( 'NONE',  ( 0.000000000000000000, 0.000000000000000000, -1.000000000000000000 ) ) ;
#10252 = CARTESIAN_POINT ( 'NONE',  ( -3.037679868588000431, -78.56178455456850429, -2.545324682163999874 ) ) ;
#10253 = CARTESIAN_POINT ( 'NONE',  ( 0.000000000000000000, -79.66562500002999059, 0.000000000000000000 ) ) ;
#10254 = CARTESIAN_POINT ( 'NONE',  ( 0.000000000000000000, -86.20000000000000284, -9.950000000000001066 ) ) ;
#10255 = AXIS2_PLACEMENT_3D ( 'NONE', #5097, #41689, #14228 ) ;
#10256 = CARTESIAN_POINT ( 'NONE',  ( 0.1216125091987902140, -82.96767066915866451, 1.244084642679034625 ) ) ;
#10257 = CARTESIAN_POINT ( 'NONE',  ( 2.223069596159087169, -77.04374999999998863, -9.266319061195876117 ) ) ;
#10258 = CARTESIAN_POINT ( 'NONE',  ( -6.043427764450833628, -79.31666666666667709, 10.48543666025107335 ) ) ;
#10259 = CARTESIAN_POINT ( 'NONE',  ( -9.929702205026998740, -61.43097880247000120, -7.973987073312001073 ) ) ;
#10260 = CARTESIAN_POINT ( 'NONE',  ( 1.247385798810000113, -54.32277743478999810, -12.50301438874000048 ) ) ;
#10261 = EDGE_CURVE ( 'NONE', #17264, #18726, #50831, .T. ) ;
#10262 = CARTESIAN_POINT ( 'NONE',  ( 12.70455691843822343, -24.56014620597932918, -1.489817752280619967 ) ) ;
#10263 = FACE_OUTER_BOUND ( 'NONE', #33903, .T. ) ;
#10264 = CARTESIAN_POINT ( 'NONE',  ( 7.651147547618999845, -56.03743349692000209, -10.45204383579000051 ) ) ;
#10265 = CARTESIAN_POINT ( 'NONE',  ( -1.541016483300999829, -2.132935987229999775, -3.126416733747999999 ) ) ;
#10266 = EDGE_CURVE ( 'NONE', #822, #26684, #5384, .T. ) ;
#10267 = CARTESIAN_POINT ( 'NONE',  ( 12.82230166703000052, -23.42260938006999993, 2.065916748305000272 ) ) ;
#10268 = CARTESIAN_POINT ( 'NONE',  ( 4.570427068259999892, -77.21806133255499560, 11.39767413300000065 ) ) ;
#10269 = LINE ( 'NONE', #32101, #40134 ) ;
#10271 = CARTESIAN_POINT ( 'NONE',  ( 9.304500756975000897, -79.05550936896946723, -5.821536072646999571 ) ) ;
#10270 = CARTESIAN_POINT ( 'NONE',  ( 1.798944584240000255, -60.01533228248000285, 12.61116916001999932 ) ) ;
#10272 = CARTESIAN_POINT ( 'NONE',  ( -0.4579595194372000355, -76.87759916035999197, -12.05314280177999997 ) ) ;
#10273 = ORIENTED_EDGE ( 'NONE', *, *, #25310, .F. ) ;
#10274 = CARTESIAN_POINT ( 'NONE',  ( -1.578055943689000040, -85.27621544543099219, -3.408973675753000254 ) ) ;
#10275 = CARTESIAN_POINT ( 'NONE',  ( 11.36098558129999958, -80.53363121547570813, 1.007794481568000222 ) ) ;
#10276 = CARTESIAN_POINT ( 'NONE',  ( 8.780887922207014640, -78.32464479236936938, -2.908481940203349048 ) ) ;
#10277 = CYLINDRICAL_SURFACE ( 'NONE', #46942, 1.250000000000000000 ) ;
#10278 = CARTESIAN_POINT ( 'NONE',  ( 6.329984427697000093, -78.22896673128499856, 9.260097609460000712 ) ) ;
#10279 = CARTESIAN_POINT ( 'NONE',  ( -7.247844507162001015, -23.25000000000000000, 9.722718241315000398 ) ) ;
#10280 = CONICAL_SURFACE ( 'NONE', #17820, 10.04999999996000071, 0.7853981633972997312 ) ;
#10281 = CARTESIAN_POINT ( 'NONE',  ( 9.589208240076997569, -79.15046275916299123, 0.8944121949827000817 ) ) ;
#10282 = CARTESIAN_POINT ( 'NONE',  ( -1.588687380433000174, -83.36453247999199334, 0.5002921117598999601 ) ) ;
#10283 = CARTESIAN_POINT ( 'NONE',  ( 3.992904449609000483, -78.77851881763731967, 0.000000000000000000 ) ) ;
#10284 = CARTESIAN_POINT ( 'NONE',  ( 10.49753343895564228, -81.00000000000001421, -3.287627937531071964 ) ) ;
#10285 = VERTEX_POINT ( 'NONE', #43652 ) ;
#10286 = CARTESIAN_POINT ( 'NONE',  ( -2.539546420801134019, -0.8541666666665600482, 2.281950960269295337 ) ) ;
#10287 = CARTESIAN_POINT ( 'NONE',  ( 0.8804656548135700866, -53.77196605261325857, -12.70299681147314708 ) ) ;
#10288 = CARTESIAN_POINT ( 'NONE',  ( 10.07210119001000059, -80.48527584695288795, 5.045985883512999592 ) ) ;
#10290 = ADVANCED_FACE ( 'NONE', ( #38634 ), #35046, .F. ) ;
#10289 = AXIS2_PLACEMENT_3D ( 'NONE', #7055, #43077, #16207 ) ;
#10291 = CARTESIAN_POINT ( 'NONE',  ( 10.04953137661648199, -75.90590377007603706, -6.156255326924525484 ) ) ;
#10292 = ORIENTED_EDGE ( 'NONE', *, *, #18627, .T. ) ;
#10293 = CARTESIAN_POINT ( 'NONE',  ( 0.5704417986824000808, -78.83828510719899896, -1.205475954488999912 ) ) ;
#10294 = DIRECTION ( 'NONE',  ( -1.000000000000000000, 0.000000000000000000, 1.400053062821000146E-14 ) ) ;
#10295 = LINE ( 'NONE', #28573, #24706 ) ;
#10296 = VERTEX_POINT ( 'NONE', #44224 ) ;
#10297 = CARTESIAN_POINT ( 'NONE',  ( -0.8050603620646999969, -78.87859328629799904, -12.13813858862000217 ) ) ;
#10298 = CARTESIAN_POINT ( 'NONE',  ( 9.270530027976999321, -77.29059517626798481, 6.305874881421999589 ) ) ;
#10299 = LINE ( 'NONE', #22995, #18643 ) ;
#10300 = AXIS2_PLACEMENT_3D ( 'NONE', #18490, #54512, #50088 ) ;
#10301 = VERTEX_POINT ( 'NONE', #3211 ) ;
#10302 = ORIENTED_EDGE ( 'NONE', *, *, #2462, .F. ) ;
#10303 = CONICAL_SURFACE ( 'NONE', #56488, 0.6999999997695030007, 0.7853981633972997312 ) ;
#10304 = DIRECTION ( 'NONE',  ( -0.07798810159117737506, -0.04890177459366838036, -0.9957542229143666601 ) ) ;
#10305 = EDGE_CURVE ( 'NONE', #37146, #11113, #39153, .T. ) ;
#10306 = CARTESIAN_POINT ( 'NONE',  ( 8.985706068735000329, -79.60840237243299100, -3.828549499589000149 ) ) ;
#10307 = EDGE_LOOP ( 'NONE', ( #14275, #22933, #20182, #48286 ) ) ;
#10308 = FACE_OUTER_BOUND ( 'NONE', #31752, .T. ) ;
#10309 = CARTESIAN_POINT ( 'NONE',  ( 11.79999999988000070, -23.14999999478999726, -0.5999999998848000171 ) ) ;
#10310 = B_SPLINE_CURVE_WITH_KNOTS ( 'NONE', 3,
 ( #15406, #6544, #24553, #42568, #7701, #48732 ),
 .UNSPECIFIED., .F., .F.,
 ( 4, 1, 1, 4 ),
 ( 0.000000000000000000, 0.3333333333333000081, 0.6666666666667000474, 1.000000000000000000 ),
 .UNSPECIFIED. ) ;
#10311 = ORIENTED_EDGE ( 'NONE', *, *, #41008, .F. ) ;
#10312 = CARTESIAN_POINT ( 'NONE',  ( -1.408973282649000014, -77.73770945175000691, 0.6047956624285000249 ) ) ;
#10313 = CARTESIAN_POINT ( 'NONE',  ( 9.475051992780000987, -77.87487694988500664, -0.6170397550469999270 ) ) ;
#10314 = CARTESIAN_POINT ( 'NONE',  ( -0.4716021410008969794, -80.19438574499905314, -1.157506175934070347 ) ) ;
#10315 = CARTESIAN_POINT ( 'NONE',  ( 8.768124086549999419, -59.94999999446000771, 7.919595949288999570 ) ) ;
#10316 = CARTESIAN_POINT ( 'NONE',  ( -10.86658628928999981, -76.76993982145202722, -2.781249891074999869 ) ) ;
#10317 = CARTESIAN_POINT ( 'NONE',  ( -12.71466563516724158, -17.86210710701672610, -1.778810201854685857 ) ) ;
#10318 = CARTESIAN_POINT ( 'NONE',  ( 1.258015307303396391, -78.05300461876107931, -0.8356367902642429790 ) ) ;
#10319 = CARTESIAN_POINT ( 'NONE',  ( 10.27342224349336419, -17.93842478175138311, 7.712153330322453648 ) ) ;
#10320 = VERTEX_POINT ( 'NONE', #30911 ) ;
#10321 = CARTESIAN_POINT ( 'NONE',  ( 11.88049207238000093, -76.24625088658999061, -3.223263369271999856 ) ) ;
#10322 = CARTESIAN_POINT ( 'NONE',  ( -2.150973351021207236, -1.921964726325504413, -2.785944457644208949 ) ) ;
#10323 = AXIS2_PLACEMENT_3D ( 'NONE', #47579, #52556, #25389 ) ;
#10324 = FACE_OUTER_BOUND ( 'NONE', #14467, .T. ) ;
#10325 = CARTESIAN_POINT ( 'NONE',  ( 11.81418954875000082, -78.78894628561999980, 3.289986436736999753 ) ) ;
#10326 = CARTESIAN_POINT ( 'NONE',  ( 11.61133755414000035, -76.91029437269800439, 3.999933378912999604 ) ) ;
#10327 = CARTESIAN_POINT ( 'NONE',  ( 12.74365836114991346, -18.47810168886552162, -1.980611005600054986 ) ) ;
#10328 = CARTESIAN_POINT ( 'NONE',  ( 2.557969438714201349, -2.797342906287011655, -2.007748672213171215 ) ) ;
#10329 = CARTESIAN_POINT ( 'NONE',  ( -11.97917456330697838, -78.05650138543988703, -0.9813211398764013493 ) ) ;
#10330 = CARTESIAN_POINT ( 'NONE',  ( 3.113304451009999863, -78.39783470746900207, -10.55022916317000181 ) ) ;
#10331 = VERTEX_POINT ( 'NONE', #48946 ) ;
#10332 = CARTESIAN_POINT ( 'NONE',  ( 1.307088170492999968, -81.79038421936999725, 0.3427697847655999941 ) ) ;
#10333 = CARTESIAN_POINT ( 'NONE',  ( -5.917523019358058356, -77.88333333333329733, -10.26699006316253282 ) ) ;
#10334 = DIRECTION ( 'NONE',  ( 0.7071067811865475727, 0.000000000000000000, -0.7071067811865475727 ) ) ;
#10335 = CIRCLE ( 'NONE', #52726, 1.199999999999999956 ) ;
#10336 = DIRECTION ( 'NONE',  ( -1.000000000000000000, 0.000000000000000000, 0.000000000000000000 ) ) ;
#10337 = CARTESIAN_POINT ( 'NONE',  ( -1.859685218087000047, -3.298191639609999726, 3.214968926965999785 ) ) ;
#10338 = AXIS2_PLACEMENT_3D ( 'NONE', #52132, #57124, #48004 ) ;
#10339 = CARTESIAN_POINT ( 'NONE',  ( 10.38571723084000098, -77.28559594867499527, -5.879822389739000066 ) ) ;
#10340 = CARTESIAN_POINT ( 'NONE',  ( -9.070848764158998989, -77.18311187452979993, 2.805586010018000120 ) ) ;
#10341 = CARTESIAN_POINT ( 'NONE',  ( -10.76168635603615975, -76.16692037179028318, 4.717286685116878431 ) ) ;
#10342 = CARTESIAN_POINT ( 'NONE',  ( 10.84306248592000088, -79.26733954020500050, -1.266239280945999912 ) ) ;
#10343 = CARTESIAN_POINT ( 'NONE',  ( 1.356394222568863217, -86.02148120184399716, 3.125459129808134229 ) ) ;
#10344 = VERTEX_POINT ( 'NONE', #56652 ) ;
#10345 = CARTESIAN_POINT ( 'NONE',  ( 12.70556836328846373, -25.22772277325712764, 0.2642470010264758584 ) ) ;
#10346 = CARTESIAN_POINT ( 'NONE',  ( 10.98648384835751024, -79.20851479812272089, 4.884329123650943849 ) ) ;
#10347 = CARTESIAN_POINT ( 'NONE',  ( 1.538071403320016461, -76.93541666666665435, -11.74999999999999822 ) ) ;
#10348 = CARTESIAN_POINT ( 'NONE',  ( -2.169167664939000151, -78.38128593012899614, 10.75912301088999889 ) ) ;
#10349 = CARTESIAN_POINT ( 'NONE',  ( -9.596002108778193929, -77.84791666666664867, 7.374560639698937159 ) ) ;
#10350 = CARTESIAN_POINT ( 'NONE',  ( 8.664202219160999974, -79.35643979701998774, -4.294932555920000006 ) ) ;
#10351 = CARTESIAN_POINT ( 'NONE',  ( 8.284626357352999904, -16.95139346842000094, -9.778502130864000108 ) ) ;
#10352 = DIRECTION ( 'NONE',  ( 0.000000000000000000, -1.000000000000000000, 0.000000000000000000 ) ) ;
#10353 = EDGE_LOOP ( 'NONE', ( #20691, #48047, #2107, #33802, #53937 ) ) ;
#10354 = CARTESIAN_POINT ( 'NONE',  ( -6.612779597103238594, -77.43740819862406966, 6.629663389723390310 ) ) ;
#10355 = CARTESIAN_POINT ( 'NONE',  ( -9.839357990653688546, -79.50291255989223771, 6.574323847643208651 ) ) ;
#10356 = EDGE_CURVE ( 'NONE', #36426, #21041, #16785, .T. ) ;
#10357 = CARTESIAN_POINT ( 'NONE',  ( 12.01773220436371403, -77.71045720483247976, 1.122334885944337168 ) ) ;
#10359 = CARTESIAN_POINT ( 'NONE',  ( -1.219338165725585066, -81.58269073872453703, 0.2774308609236747492 ) ) ;
#10358 = CARTESIAN_POINT ( 'NONE',  ( 0.2130225254155999892, -82.02015203348199179, 1.301993463592000078 ) ) ;
#10360 = CARTESIAN_POINT ( 'NONE',  ( -1.639985762054531282, -78.73658472870678793, 11.09648843833229925 ) ) ;
#10361 = CARTESIAN_POINT ( 'NONE',  ( -8.888234858626997692, -77.00000000000000000, -2.992064833292889858 ) ) ;
#10362 = CARTESIAN_POINT ( 'NONE',  ( 13.94241847916999966, -9.539970597796999741, 4.312626734329999762E-05 ) ) ;
#10363 = CARTESIAN_POINT ( 'NONE',  ( -0.1995282058519000090, -77.96721194367999885, 1.292660429007000067 ) ) ;
#10364 = CARTESIAN_POINT ( 'NONE',  ( -8.485281374238999419, -59.94999999967000548, -8.485281374238999419 ) ) ;
#10365 = CARTESIAN_POINT ( 'NONE',  ( 11.00000000000000000, -79.44999999999998863, 0.000000000000000000 ) ) ;
#10366 = EDGE_CURVE ( 'NONE', #40915, #38307, #30019, .T. ) ;
#10367 = DIRECTION ( 'NONE',  ( 0.000000000000000000, -0.7071067811866525998, -0.7071067811864425456 ) ) ;
#10368 = VERTEX_POINT ( 'NONE', #7914 ) ;
#10369 = ORIENTED_EDGE ( 'NONE', *, *, #1869, .T. ) ;
#10370 = CARTESIAN_POINT ( 'NONE',  ( 4.582566119076999733, -77.77986332859900642, 8.787281441338999244 ) ) ;
#10371 = CARTESIAN_POINT ( 'NONE',  ( 8.590462643448541158, -78.79883893288808849, -6.463108130307494648 ) ) ;
#10372 = AXIS2_PLACEMENT_3D ( 'NONE', #37794, #46974, #25085 ) ;
#10373 = EDGE_LOOP ( 'NONE', ( #20121, #30454, #15825 ) ) ;
#10374 = CARTESIAN_POINT ( 'NONE',  ( -10.07624512687999996, -76.28571183916568543, -4.852130239470000106 ) ) ;
#10375 = CARTESIAN_POINT ( 'NONE',  ( -2.669304356624397467, -83.36354168090352346, -2.174774419161705552 ) ) ;
#10376 = CIRCLE ( 'NONE', #30163, 12.69999999999999929 ) ;
#10377 = CARTESIAN_POINT ( 'NONE',  ( -9.099455430112048049, -79.37646600500266914, 2.730131614506341009 ) ) ;
#10378 = EDGE_CURVE ( 'NONE', #50691, #54307, #53080, .T. ) ;
#10379 = CARTESIAN_POINT ( 'NONE',  ( 7.620012114232000755, -60.00560398617000146, 10.53562503196000044 ) ) ;
#10380 = CARTESIAN_POINT ( 'NONE',  ( -11.75000000000000000, -76.04999999999999716, -3.652443742841000169E-09 ) ) ;
#10381 = CARTESIAN_POINT ( 'NONE',  ( -10.26957973897401288, -78.50685741050436661, 6.168932106361120660 ) ) ;
#10382 = CARTESIAN_POINT ( 'NONE',  ( -8.286771986066998608, -78.70725489392698648, 7.559597915363999832 ) ) ;
#10383 = EDGE_CURVE ( 'NONE', #20614, #17190, #25351, .T. ) ;
#10384 = EDGE_LOOP ( 'NONE', ( #11326, #5352, #56207, #24960, #24094, #17497 ) ) ;
#10385 = CARTESIAN_POINT ( 'NONE',  ( -7.610436523679670273, -23.52540704710936126, 10.41144397132592836 ) ) ;
#10386 = EDGE_LOOP ( 'NONE', ( #18505, #23185, #50809, #49279 ) ) ;
#10387 = CARTESIAN_POINT ( 'NONE',  ( 9.192586965176360536, -77.35899963357374531, 1.030861253847850101 ) ) ;
#10388 = CARTESIAN_POINT ( 'NONE',  ( 0.5117640625906000329, -79.58524224479700138, 1.216002981391000048 ) ) ;
#10389 = CARTESIAN_POINT ( 'NONE',  ( 8.485281374238999419, -55.64999999967000122, 8.485281374238999419 ) ) ;
#10390 = CARTESIAN_POINT ( 'NONE',  ( 1.603441158369999897, -78.75133983115900094, 0.1902368389766999901 ) ) ;
#10391 = DIRECTION ( 'NONE',  ( -1.000000000000000000, 0.000000000000000000, 0.000000000000000000 ) ) ;
#10392 = CARTESIAN_POINT ( 'NONE',  ( 12.00000000000000711, -78.63958333333333428, -1.570796326794872355 ) ) ;
#10393 = CARTESIAN_POINT ( 'NONE',  ( -1.481905647302000029, -78.30430509401999473, -0.6727694308694001091 ) ) ;
#10394 = CARTESIAN_POINT ( 'NONE',  ( -7.941067684623824618, -79.34731494385309247, -5.274242742192593703 ) ) ;
#10395 = CARTESIAN_POINT ( 'NONE',  ( -0.6813111686677723045, -79.17942873427989525, -1.051713183095109416 ) ) ;
#10396 = CARTESIAN_POINT ( 'NONE',  ( 6.696351723200000272, -79.10660385176299769, -8.651398149159000184 ) ) ;
#10397 = CARTESIAN_POINT ( 'NONE',  ( -8.478749451758998745, -24.87812788920000173, -9.108222796172999125 ) ) ;
#10398 = CARTESIAN_POINT ( 'NONE',  ( 12.75761570867999950, -56.02180874340999850, -1.931043762602999925 ) ) ;
#10399 = CARTESIAN_POINT ( 'NONE',  ( 1.861448431883999888, -85.63651402127000267, 3.016619445684999956 ) ) ;
#10400 = CIRCLE ( 'NONE', #21681, 12.50000000000000000 ) ;
#10401 = ORIENTED_EDGE ( 'NONE', *, *, #57193, .F. ) ;
#10402 = CARTESIAN_POINT ( 'NONE',  ( -10.79944190718824082, -77.20000000000001705, 1.961979764079434752 ) ) ;
#10403 = CARTESIAN_POINT ( 'NONE',  ( 1.449190734180999973, -80.03602897879000011, -0.8942388842271000726 ) ) ;
#10404 = CARTESIAN_POINT ( 'NONE',  ( -0.7463658975004607843, -77.98057452693001323, 10.72557968341309120 ) ) ;
#10405 = CARTESIAN_POINT ( 'NONE',  ( 7.483561698776000526, -78.38741300779199150, 9.354804580292000793 ) ) ;
#10406 = ADVANCED_FACE ( 'NONE', ( #25916 ), #12519, .F. ) ;
#10407 = CARTESIAN_POINT ( 'NONE',  ( -7.981651535810999398, -17.28135615487000010, 10.08154952397000059 ) ) ;
#10408 = CARTESIAN_POINT ( 'NONE',  ( -0.3528755875620728233, -78.14773221022913674, 1.224383399418459861 ) ) ;
#10409 = CARTESIAN_POINT ( 'NONE',  ( 3.582811860122647296, -2.504862101322317347, 0.2337939847196791321 ) ) ;
#10410 = CARTESIAN_POINT ( 'NONE',  ( 9.552523027918807585, -80.88808154937647998, 4.930511287832971767 ) ) ;
#10411 = CARTESIAN_POINT ( 'NONE',  ( 6.053520011479999852, -77.89860065712299786, 7.208750930507999755 ) ) ;
#10412 = CARTESIAN_POINT ( 'NONE',  ( 3.518657424384977084, -85.83735716284299144, -1.566607219110052629 ) ) ;
#10413 = CARTESIAN_POINT ( 'NONE',  ( -7.719769492146999923, -76.89709394048399815, 7.579341418041000367 ) ) ;
#10414 = CARTESIAN_POINT ( 'NONE',  ( 1.710992592906253718, -0.8541666519182247175, -2.966907352992771862 ) ) ;
#10415 = CARTESIAN_POINT ( 'NONE',  ( -1.680151650566999999, -81.07168981312450740, -10.89699058823000044 ) ) ;
#10416 = ORIENTED_EDGE ( 'NONE', *, *, #58012, .T. ) ;
#10417 = CARTESIAN_POINT ( 'NONE',  ( 0.9212224518285999642, -61.61954101805999784, -12.54670315985999984 ) ) ;
#10418 = CARTESIAN_POINT ( 'NONE',  ( 7.103480459865705754, -80.41785787807644681, 8.098525061049892670 ) ) ;
#10419 = B_SPLINE_CURVE_WITH_KNOTS ( 'NONE', 3,
 ( #32831, #55286, #23699, #55582 ),
 .UNSPECIFIED., .F., .F.,
 ( 4, 4 ),
 ( 0.000000000000000000, 1.000000000000000000 ),
 .UNSPECIFIED. ) ;
#10420 = CARTESIAN_POINT ( 'NONE',  ( -7.849238557987999521, -76.70433613164000519, 7.706455349885999340 ) ) ;
#10421 = CARTESIAN_POINT ( 'NONE',  ( 9.028681611143001717, -78.07339771656899075, -5.970393136294000591 ) ) ;
#10422 = CARTESIAN_POINT ( 'NONE',  ( 7.618394338636999663, -23.22713821270000167, -10.53494418059000104 ) ) ;
#10423 = CARTESIAN_POINT ( 'NONE',  ( 0.3297891718556331120, -83.59479165932887668, -4.037289259723059409 ) ) ;
#10424 = CARTESIAN_POINT ( 'NONE',  ( 3.552101903221845713, -79.75000000000000000, -8.571631383469688004 ) ) ;
#10425 = LINE ( 'NONE', #14255, #6854 ) ;
#10426 = B_SPLINE_SURFACE_WITH_KNOTS ( 'NONE', 3, 3, ( 
 ( #51081, #46365, #32449, #42502, #6770, #55493, #5889, #56082, #15628, #1489, #32741, #50494, #10629, #33624, #6185, #51667, #24779, #10048, #28029 ),
 ( #23898, #46074, #5596, #23608, #19479, #28613, #41622, #33334, #15341, #19193, #51369, #42214, #6477, #37185, #24197, #19774, #37771, #55792, #46951 ),
 ( #38921, #39502, #52795, #25061, #35049, #7918, #3493, #3215, #7632, #57223, #12067, #12350, #30048, #20637, #2920, #21496, #26210, #3775, #12638 ),
 ( #56939, #38639, #39783, #56656, #52227, #51947, #48663, #16212, #48380, #34480, #30338, #53084, #21779, #25919, #8208, #57506, #7345, #21203, #15920 ) ),
 .UNSPECIFIED., .F., .F., .F.,
 ( 4, 4 ),
 ( 4, 1, 1, 1, 1, 1, 1, 1, 1, 1, 1, 1, 1, 1, 1, 1, 4 ),
 ( -0.1387574078320000237, 1.138757407831999968 ),
 ( -0.004592865874913999551, 0.01033394821856000075, 0.02526076231202999817, 0.04018757640548999838, 0.05511439049895999753, 0.07004120459242998975, 0.08496801868589999585, 0.09989483277937000194, 0.1148216468727999984, 0.1297484609662999944, 0.1446752750597999904, 0.1596020891533000141, 0.1745289032467000068, 0.1894557173402000028, 0.2043825314336999988, 0.2193093455270999914, 0.2342361596205999874 ),
 .UNSPECIFIED. ) ;
#10427 = PRESENTATION_LAYER_ASSIGNMENT (  '', '', ( #38679 ) ) ;
#10428 = CARTESIAN_POINT ( 'NONE',  ( 3.675204158029000023, -85.31969503318799752, -1.975585186543999949 ) ) ;
#10429 = CARTESIAN_POINT ( 'NONE',  ( -0.1963495408493605987, -79.61458333333334281, -1.500000000000000444 ) ) ;
#10430 = CARTESIAN_POINT ( 'NONE',  ( 4.750168553339000788, -78.64926952346999656, -12.04580866360999991 ) ) ;
#10431 = CARTESIAN_POINT ( 'NONE',  ( 5.172078487859000262, -77.61362032395699373, 10.00417756108999967 ) ) ;
#10432 = CARTESIAN_POINT ( 'NONE',  ( -0.6332123272625999055, -81.23563726096999460, 1.540853336418999797 ) ) ;
#10433 = CARTESIAN_POINT ( 'NONE',  ( 0.000000000000000000, -76.39999999999999147, 0.000000000000000000 ) ) ;
#10434 = CARTESIAN_POINT ( 'NONE',  ( 7.919595949288999570, -55.64999999964999233, -9.050966799188000067 ) ) ;
#10435 = CARTESIAN_POINT ( 'NONE',  ( -0.5897947633678554125, -81.84308799674356294, -1.392029655722818671 ) ) ;
#10436 = CARTESIAN_POINT ( 'NONE',  ( -13.86363636363000218, -32.36102867817999851, -1.277888278874999896E-05 ) ) ;
#10437 = ORIENTED_EDGE ( 'NONE', *, *, #24128, .T. ) ;
#10438 = CARTESIAN_POINT ( 'NONE',  ( 1.250000000000000000, -79.84999999999999432, 0.000000000000000000 ) ) ;
#10439 = EDGE_LOOP ( 'NONE', ( #2610, #51209, #51195, #42924, #5084, #33593, #57466, #46339 ) ) ;
#10440 = CARTESIAN_POINT ( 'NONE',  ( 0.1765468244193108827, -81.73664919909492710, -1.237851851414618176 ) ) ;
#10441 = EDGE_CURVE ( 'NONE', #37950, #237, #24403, .T. ) ;
#10442 = FILL_AREA_STYLE_COLOUR ( '', #27482 ) ;
#10443 = CARTESIAN_POINT ( 'NONE',  ( 8.679422240859999249, -78.58715855134300909, -6.994438423095999724 ) ) ;
#10444 = FACE_OUTER_BOUND ( 'NONE', #54942, .T. ) ;
#10445 = EDGE_LOOP ( 'NONE', ( #18448, #28048, #36579, #38073 ) ) ;
#10446 = VERTEX_POINT ( 'NONE', #37400 ) ;
#10447 = AXIS2_PLACEMENT_3D ( 'NONE', #10711, #28689, #51449 ) ;
#10448 = EDGE_CURVE ( 'NONE', #42344, #15053, #34222, .T. ) ;
#10449 = CARTESIAN_POINT ( 'NONE',  ( -1.404437343888000012, -82.11361821589699161, -0.1941552913445999951 ) ) ;
#10450 = VERTEX_POINT ( 'NONE', #1130 ) ;
#10451 = ORIENTED_EDGE ( 'NONE', *, *, #12741, .F. ) ;
#10452 = CARTESIAN_POINT ( 'NONE',  ( 1.466594960159999905, -17.91841800947999985, 12.44238958332999800 ) ) ;
#10453 = DIRECTION ( 'NONE',  ( 0.000000000000000000, -1.000000000000000000, -1.369275063704000118E-14 ) ) ;
#10454 = DIRECTION ( 'NONE',  ( 0.000000000000000000, 0.000000000000000000, 1.000000000000000000 ) ) ;
#10455 = CARTESIAN_POINT ( 'NONE',  ( -2.409906529986267643, -80.01041665875527542, 2.459253724518165818 ) ) ;
#10456 = CARTESIAN_POINT ( 'NONE',  ( -9.927618387633998509, -78.33161001420199909, -1.374747298418999897 ) ) ;
#10457 = CARTESIAN_POINT ( 'NONE',  ( 6.818911827320396135, -78.29096144711863303, -6.251674546281022593 ) ) ;
#10458 = CARTESIAN_POINT ( 'NONE',  ( -6.606377239730330864, -78.07291666666665719, -8.596418555780440229 ) ) ;
#10459 = EDGE_CURVE ( 'NONE', #35553, #32105, #10558, .T. ) ;
#10460 = ORIENTED_EDGE ( 'NONE', *, *, #41760, .F. ) ;
#10461 = ORIENTED_EDGE ( 'NONE', *, *, #24334, .T. ) ;
#10462 = CARTESIAN_POINT ( 'NONE',  ( -7.652281944047452100, -77.55252551045413156, 5.196868011323922509 ) ) ;
#10463 = AXIS2_PLACEMENT_3D ( 'NONE', #2532, #39403, #16394 ) ;
#10464 = CARTESIAN_POINT ( 'NONE',  ( -8.012523733904361123, -76.96708638852499007, -8.990154430768209082 ) ) ;
#10465 = CARTESIAN_POINT ( 'NONE',  ( -1.217465845835396188, -81.47916666666668561, 0.3271848554490955907 ) ) ;
#10466 = CARTESIAN_POINT ( 'NONE',  ( 1.001315002179999913, -17.31477588286000113, 12.50000000000000000 ) ) ;
#10467 = CARTESIAN_POINT ( 'NONE',  ( -1.182190922889000184, -78.88513002107399075, -9.631881180458998770 ) ) ;
#10468 = FACE_OUTER_BOUND ( 'NONE', #35664, .T. ) ;
#10469 = CARTESIAN_POINT ( 'NONE',  ( -3.234946784983960821, -86.07408421428944223, 2.385846890079581062 ) ) ;
#10470 = DIRECTION ( 'NONE',  ( 0.000000000000000000, 1.000000000000000000, 0.000000000000000000 ) ) ;
#10471 = CARTESIAN_POINT ( 'NONE',  ( 0.3265465218672000125, -79.78618645244999641, -1.431717670164000200 ) ) ;
#10472 = CARTESIAN_POINT ( 'NONE',  ( -4.765392682094479859, -77.63277193750339222, -8.156953009811001465 ) ) ;
#10473 = CARTESIAN_POINT ( 'NONE',  ( -8.293363313813765458, -76.63724320113942667, 8.323509784614648410 ) ) ;
#10474 = CARTESIAN_POINT ( 'NONE',  ( 3.840130302921999750, -82.41024718738999866, -1.637848040457000165 ) ) ;
#10475 = CARTESIAN_POINT ( 'NONE',  ( -0.8293389441169838339, -79.82887584819658855, -1.264652115086847939 ) ) ;
#10476 = CARTESIAN_POINT ( 'NONE',  ( 2.202483111904999902, -79.21391001420199984, -9.433251486511000650 ) ) ;
#10477 = CARTESIAN_POINT ( 'NONE',  ( 8.596187401860602151, -76.79807390516880616, -6.606220740437996675 ) ) ;
#10478 = ADVANCED_FACE ( 'NONE', ( #55420 ), #37582, .F. ) ;
#10479 = CARTESIAN_POINT ( 'NONE',  ( -7.633502222236000279, -18.79895684643999942, -10.36289759016999845 ) ) ;
#10481 = CARTESIAN_POINT ( 'NONE',  ( 0.9834589317531000630, -79.03089699492099385, 0.9007689179829999615 ) ) ;
#10480 = DIRECTION ( 'NONE',  ( 0.000000000000000000, 0.000000000000000000, 1.000000000000000000 ) ) ;
#10482 = DIRECTION ( 'NONE',  ( -0.7592504788685878747, 0.04890177849880918831, 0.6489586476790899505 ) ) ;
#10483 = CARTESIAN_POINT ( 'NONE',  ( 2.935661446561999899, -79.99999999999998579, -9.035036904803998681 ) ) ;
#10484 = DIRECTION ( 'NONE',  ( 0.000000000000000000, 1.000000000000000000, 6.735284179502000863E-11 ) ) ;
#10485 = CARTESIAN_POINT ( 'NONE',  ( -0.1636246173744673738, -79.11458333333331439, -1.249999999999999778 ) ) ;
#10486 = ORIENTED_EDGE ( 'NONE', *, *, #19517, .T. ) ;
#10487 = CARTESIAN_POINT ( 'NONE',  ( -2.460715419380010260, -78.90833333333333144, -11.55514622821886839 ) ) ;
#10488 = DIRECTION ( 'NONE',  ( 0.000000000000000000, 1.000000000000000000, 0.000000000000000000 ) ) ;
#10489 = DIRECTION ( 'NONE',  ( 0.000000000000000000, 1.000000000000000000, 0.000000000000000000 ) ) ;
#10490 = CARTESIAN_POINT ( 'NONE',  ( 12.43569926720000041, -61.68202092968000727, -0.4277578398253000236 ) ) ;
#10491 = VECTOR ( 'NONE', #41802, 1000.000000000000000 ) ;
#10492 = CARTESIAN_POINT ( 'NONE',  ( 1.931043762602999925, -56.02180874340999850, 12.75761570867999950 ) ) ;
#10493 = CARTESIAN_POINT ( 'NONE',  ( 12.51033564907000084, -78.17580835132000061, -3.582046052171000028 ) ) ;
#10494 = CARTESIAN_POINT ( 'NONE',  ( -2.494193680512617473, -79.49363092753210935, 10.45664570855439912 ) ) ;
#10495 = EDGE_CURVE ( 'NONE', #2535, #12885, #28541, .T. ) ;
#10496 = CARTESIAN_POINT ( 'NONE',  ( 5.858810443405999990, -79.55503998579798974, -7.916359134618999427 ) ) ;
#10497 = B_SPLINE_CURVE_WITH_KNOTS ( 'NONE', 3,
 ( #46580, #38270, #15844, #6107, #11424, #1698, #47456, #24114, #19992, #42133, #19692, #37692, #29117, #15258, #55711, #51292, #10848, #28822, #37979, #15553, #33546, #43582, #3426, #58020, #11999, #40004, #26140, #34983, #12566, #48594, #44161, #17002, #53013, #56868, #48880, #39717, #35270, #30563, #39435, #8140, #43878, #57724, #57442, #52439, #3994, #3708, #20846, #21711, #17581, #48030, #53303, #12279, #25274, #17280, #12846, #21996, #30845, #8423, #52728, #7850, #35568, #53594, #26420, #13134, #25851, #30269, #29977, #47740, #3144, #44442, #7273, #21427, #43293, #2849, #38850, #21132, #57151, #48311, #16427, #34410, #7562, #25562, #39141, #16716, #34698, #23176, #9896, #36170, #49472, #774, #36746, #40605, #13431, #41474, #9311, #54763, #4886, #32300, #50347 ),
 .UNSPECIFIED., .F., .F.,
 ( 4, 2, 2, 2, 1, 1, 1, 1, 2, 2, 2, 2, 2, 1, 1, 1, 1, 2, 2, 2, 2, 2, 1, 1, 1, 1, 2, 2, 2, 2, 2, 1, 1, 1, 2, 2, 2, 2, 1, 1, 1, 1, 2, 2, 2, 2, 2, 1, 1, 1, 2, 2, 2, 2, 2, 1, 1, 1, 2, 2, 2, 4 ),
 ( 0.000000000000000000, 0.06250000000000603684, 0.09375000000000904832, 0.1093750000000105194, 0.1171875000000112688, 0.1210937500000117129, 0.1230468750000119349, 0.1240234375000121014, 0.1245117187500121569, 0.1250000000000121847, 0.1875000000000133504, 0.2187500000000138500, 0.2343750000000139888, 0.2421875000000140443, 0.2460937500000140721, 0.2480468750000141831, 0.2490234375000141553, 0.2495117187500141276, 0.2500000000000140998, 0.3125000000000109912, 0.3437500000000094369, 0.3593750000000087153, 0.3671875000000083822, 0.3710937500000082157, 0.3730468750000080491, 0.3740234375000080491, 0.3745117187500080491, 0.3750000000000079936, 0.4375000000000078826, 0.4687500000000078826, 0.4843750000000078271, 0.4921875000000077716, 0.4960937500000077716, 0.4980468750000077716, 0.4990234375000077161, 0.5000000000000076605, 0.5625000000000073275, 0.5937500000000072164, 0.6093750000000069944, 0.6171875000000069944, 0.6210937500000068834, 0.6230468750000069944, 0.6240234375000069944, 0.6250000000000069944, 0.6875000000000058842, 0.7187500000000053291, 0.7343750000000051070, 0.7421875000000048850, 0.7460937500000047740, 0.7480468750000047740, 0.7490234375000047740, 0.7500000000000046629, 0.8125000000000039968, 0.8437500000000036637, 0.8593750000000035527, 0.8671875000000033307, 0.8710937500000033307, 0.8730468750000033307, 0.8740234375000032196, 0.8750000000000032196, 0.9375000000000016653, 1.000000000000000000 ),
 .UNSPECIFIED. ) ;
#10498 = DIRECTION ( 'NONE',  ( -1.000000000000000000, 0.000000000000000000, 0.000000000000000000 ) ) ;
#10499 = CARTESIAN_POINT ( 'NONE',  ( 4.403823373056999557, -77.14888256794749566, 9.969607752326000494 ) ) ;
#10500 = CARTESIAN_POINT ( 'NONE',  ( -2.690539317418799925, -76.30618315013305164, -11.43924176612597421 ) ) ;
#10501 = CARTESIAN_POINT ( 'NONE',  ( 1.423274683982999944, -81.62922810174299570, 0.4931431035810000529 ) ) ;
#10502 = CARTESIAN_POINT ( 'NONE',  ( -0.6471704932797999188, -78.03029514476064321, 9.701898969124000516 ) ) ;
#10503 = AXIS2_PLACEMENT_3D ( 'NONE', #11762, #47512, #28590 ) ;
#10504 = CARTESIAN_POINT ( 'NONE',  ( -1.900968108529000000, -77.62963215124798921, -9.219409434742001253 ) ) ;
#10506 = CARTESIAN_POINT ( 'NONE',  ( -2.598917237794094337, -2.947916666666666519, 1.997276839918461722 ) ) ;
#10505 = CARTESIAN_POINT ( 'NONE',  ( -3.027399109997999993, -84.54654301962300167, -2.224011006729000428 ) ) ;
#10507 = CARTESIAN_POINT ( 'NONE',  ( -2.364557222828000072, -79.46484805011499475, 9.257622954664000758 ) ) ;
#10508 = DIRECTION ( 'NONE',  ( 0.000000000000000000, 1.000000000000000000, 0.000000000000000000 ) ) ;
#10509 = FACE_BOUND ( 'NONE', #10993, .T. ) ;
#10510 = CARTESIAN_POINT ( 'NONE',  ( -4.807621802239022912, -76.07083333332734298, 10.81449558221754970 ) ) ;
#10511 = CARTESIAN_POINT ( 'NONE',  ( 0.7412195882237281319, -79.57812500151310076, -9.421874992337064825 ) ) ;
#10512 = CIRCLE ( 'NONE', #30284, 8.500000000000000000 ) ;
#10513 = ORIENTED_EDGE ( 'NONE', *, *, #26492, .T. ) ;
#10514 = CARTESIAN_POINT ( 'NONE',  ( 11.90415444617999974, -79.87240057246600600, -1.731350929957999885 ) ) ;
#10515 = EDGE_CURVE ( 'NONE', #25083, #44710, #42140, .T. ) ;
#10516 = DIRECTION ( 'NONE',  ( 0.000000000000000000, 1.000000000000000000, 0.000000000000000000 ) ) ;
#10517 = CARTESIAN_POINT ( 'NONE',  ( -11.70000000000000107, -76.00000000000000000, 0.000000000000000000 ) ) ;
#10518 = ORIENTED_EDGE ( 'NONE', *, *, #7016, .F. ) ;
#10519 = EDGE_CURVE ( 'NONE', #31399, #14569, #34738, .T. ) ;
#10520 = CARTESIAN_POINT ( 'NONE',  ( -8.118170145944999305, -78.68888052662400412, -8.748189294319999476 ) ) ;
#10521 = ORIENTED_EDGE ( 'NONE', *, *, #10974, .T. ) ;
#10522 = ORIENTED_EDGE ( 'NONE', *, *, #50298, .T. ) ;
#10523 = CARTESIAN_POINT ( 'NONE',  ( -1.407171709420465211, -78.88541666666664298, 10.74999999999999467 ) ) ;
#10524 = ORIENTED_EDGE ( 'NONE', *, *, #10441, .T. ) ;
#10525 = CARTESIAN_POINT ( 'NONE',  ( 0.7884097517636999841, -81.25267555511598516, 3.458752693022000280 ) ) ;
#10526 = CARTESIAN_POINT ( 'NONE',  ( 9.491245595196989626, -79.15441013100512180, 0.5281570930040961898 ) ) ;
#10527 = ORIENTED_EDGE ( 'NONE', *, *, #1954, .F. ) ;
#10529 = ADVANCED_FACE ( 'NONE', ( #5820 ), #14967, .F. ) ;
#10528 = LINE ( 'NONE', #19671, #26154 ) ;
#10530 = CIRCLE ( 'NONE', #57622, 0.5000000000000000000 ) ;
#10531 = CARTESIAN_POINT ( 'NONE',  ( -7.654537085013999764, -55.51943307300000185, 10.01332844635999919 ) ) ;
#10532 = ORIENTED_EDGE ( 'NONE', *, *, #55315, .T. ) ;
#10533 = CARTESIAN_POINT ( 'NONE',  ( -2.421342480286628795, -79.20438042701073300, -9.010110489339714590 ) ) ;
#10534 = CARTESIAN_POINT ( 'NONE',  ( 9.259200219731782866, -78.62410115858894244, 2.905346636976683605 ) ) ;
#10535 = CARTESIAN_POINT ( 'NONE',  ( -5.243548408265479743, -79.79999999999998295, -10.63019555954501705 ) ) ;
#10536 = FACE_OUTER_BOUND ( 'NONE', #37584, .T. ) ;
#10537 = CARTESIAN_POINT ( 'NONE',  ( -5.950974066117157513, -78.86552852484902587, 10.72351851458284955 ) ) ;
#10538 = CARTESIAN_POINT ( 'NONE',  ( -3.536681740116999872, -78.15468623100123580, 9.036735673663999435 ) ) ;
#10539 = CARTESIAN_POINT ( 'NONE',  ( -8.075725583014000009, -76.25911125869799889, -7.736700848913999451 ) ) ;
#10540 = CARTESIAN_POINT ( 'NONE',  ( 5.112147531402400524, -76.43689203955935341, 9.547208415643030577 ) ) ;
#10541 = CARTESIAN_POINT ( 'NONE',  ( -7.653559626076999578, -55.50151115525000023, -10.01235002620999914 ) ) ;
#10542 = CARTESIAN_POINT ( 'NONE',  ( -7.608820801282668356, -78.64829813045270157, -5.263042126654066344 ) ) ;
#10543 = CARTESIAN_POINT ( 'NONE',  ( 4.934236507922636683, -76.54027943633899156, 10.66431010429060500 ) ) ;
#10544 = CARTESIAN_POINT ( 'NONE',  ( 6.931088847199000647, -77.87978501420199962, 6.366826336012000098 ) ) ;
#10545 = CARTESIAN_POINT ( 'NONE',  ( -1.000649921775999873, -79.57686399678399880, 0.8816325131470000853 ) ) ;
#10546 = VECTOR ( 'NONE', #25620, 1000.000000000000000 ) ;
#10547 = CARTESIAN_POINT ( 'NONE',  ( 0.000000000000000000, -75.00000000000001421, 0.000000000000000000 ) ) ;
#10548 = CARTESIAN_POINT ( 'NONE',  ( -0.9356112540347810702, -61.54107830070422125, -12.50329130249530962 ) ) ;
#10549 = CARTESIAN_POINT ( 'NONE',  ( 0.6589163185399000700, -81.92492549782599554, -4.077286533258999590 ) ) ;
#10550 = AXIS2_PLACEMENT_3D ( 'NONE', #29373, #11109, #56260 ) ;
#10551 = CARTESIAN_POINT ( 'NONE',  ( -3.620936601582000147, -77.59871332859898985, 8.947741361997000098 ) ) ;
#10552 = CARTESIAN_POINT ( 'NONE',  ( -9.075114011589430874, -78.05511120107294687, 5.762976831777519848 ) ) ;
#10553 = CARTESIAN_POINT ( 'NONE',  ( 1.065041349166195195, -82.89404281940629460, 0.6558440019770916951 ) ) ;
#10554 = SURFACE_STYLE_FILL_AREA ( #2853 ) ;
#10555 = CARTESIAN_POINT ( 'NONE',  ( -3.621447497675000182, -78.99318692614357929, -1.519545876029819695E-14 ) ) ;
#10556 = DIRECTION ( 'NONE',  ( -0.6489586469528950685, -0.04890178981570961203, 0.7592504787603941985 ) ) ;
#10557 = CARTESIAN_POINT ( 'NONE',  ( -1.570796326794937636, -79.28541666666666288, 11.99999999999999467 ) ) ;
#10558 = LINE ( 'NONE', #28241, #36648 ) ;
#10559 = CARTESIAN_POINT ( 'NONE',  ( -1.004305231718999991, -3.500000000000000000, 3.090933677959000203 ) ) ;
#10560 = CARTESIAN_POINT ( 'NONE',  ( 7.648026766715999791, -55.54999999381000464, 10.12290050087000104 ) ) ;
#10561 = CARTESIAN_POINT ( 'NONE',  ( -0.03126777369098861226, -79.47274184274870379, -1.511873468966818734 ) ) ;
#10562 = DIRECTION ( 'NONE',  ( 1.000000000000000000, 0.000000000000000000, 0.000000000000000000 ) ) ;
#10563 = CARTESIAN_POINT ( 'NONE',  ( 9.722066209057999231, -78.82124805011498836, 0.1588365413100999990 ) ) ;
#10564 = LINE ( 'NONE', #37705, #9395 ) ;
#10565 = ADVANCED_FACE ( 'NONE', ( #23826 ), #31381, .F. ) ;
#10566 = CARTESIAN_POINT ( 'NONE',  ( 4.484119338316999936, -77.02815612458898897, -11.43188768503999952 ) ) ;
#10567 =( NAMED_UNIT ( * ) PLANE_ANGLE_UNIT ( ) SI_UNIT ( $, .RADIAN. ) );
#10568 = CARTESIAN_POINT ( 'NONE',  ( -0.2584144827219213014, -25.22845396921143646, -12.70558781488152178 ) ) ;
#10569 = CARTESIAN_POINT ( 'NONE',  ( -12.11766251513999926, -76.17843941428000676, -1.515192406448999884 ) ) ;
#10570 = ORIENTED_EDGE ( 'NONE', *, *, #17371, .F. ) ;
#10571 = CARTESIAN_POINT ( 'NONE',  ( 2.039338779652999811, -85.51671544543098946, -3.154751871486999981 ) ) ;
#10572 = CARTESIAN_POINT ( 'NONE',  ( 7.638540051645000162, -81.09319419153379727, 8.469952564609000589 ) ) ;
#10573 = DIRECTION ( 'NONE',  ( -1.000000000000000000, 0.000000000000000000, 0.000000000000000000 ) ) ;
#10574 = CARTESIAN_POINT ( 'NONE',  ( 8.894932048652069767, -53.57190732449146253, 9.073469156702891780 ) ) ;
#10575 = CARTESIAN_POINT ( 'NONE',  ( 10.29113596735999892, -77.68423987124899099, 4.462133020506000136 ) ) ;
#10576 = CARTESIAN_POINT ( 'NONE',  ( 8.485281374238999419, -23.25000000000000000, 8.485281374238999419 ) ) ;
#10577 = CARTESIAN_POINT ( 'NONE',  ( -7.400482488103000023, -78.83780063874398536, 6.163283938603000500 ) ) ;
#10578 = CARTESIAN_POINT ( 'NONE',  ( -0.8762103189736000219, -81.46975602669000693, -1.416501064863000092 ) ) ;
#10579 = CARTESIAN_POINT ( 'NONE',  ( 3.699999999670000150, -79.00321104920828930, 0.000000000000000000 ) ) ;
#10580 = CARTESIAN_POINT ( 'NONE',  ( 4.483565756030909455, -76.07604166666334322, 10.08190381434128824 ) ) ;
#10581 = ORIENTED_EDGE ( 'NONE', *, *, #11187, .F. ) ;
#10582 = DIRECTION ( 'NONE',  ( 1.000000000000000000, 0.000000000000000000, 0.000000000000000000 ) ) ;
#10583 = CARTESIAN_POINT ( 'NONE',  ( 1.618170588614999961, -80.33478741693470226, -11.14857479085000058 ) ) ;
#10584 = CARTESIAN_POINT ( 'NONE',  ( 2.763362037843241303, -78.98488928704560408, -2.600174304222677701 ) ) ;
#10585 = ORIENTED_EDGE ( 'NONE', *, *, #44937, .T. ) ;
#10586 = CARTESIAN_POINT ( 'NONE',  ( -0.1765672563250000049, -78.29254625000710632, -1.321892640673999919 ) ) ;
#10587 = CARTESIAN_POINT ( 'NONE',  ( -9.247932426686000795, -77.50168256874098915, -0.1955654147372000162 ) ) ;
#10588 = DIRECTION ( 'NONE',  ( 0.7071067811865475727, 0.000000000000000000, 0.7071067811865475727 ) ) ;
#10589 = EDGE_LOOP ( 'NONE', ( #19300, #46272, #29880, #42923 ) ) ;
#10590 = EDGE_CURVE ( 'NONE', #41082, #49440, #52736, .T. ) ;
#10591 = CARTESIAN_POINT ( 'NONE',  ( 3.002529760384999857, -79.11371401997000419, 11.62679918156999825 ) ) ;
#10592 = CARTESIAN_POINT ( 'NONE',  ( 8.081843650394000989, -77.30829253183799210, -8.086130236420000728 ) ) ;
#10593 = DIRECTION ( 'NONE',  ( 0.000000000000000000, -1.000000000000000000, 0.000000000000000000 ) ) ;
#10594 = ORIENTED_EDGE ( 'NONE', *, *, #16825, .F. ) ;
#10595 = VERTEX_POINT ( 'NONE', #30276 ) ;
#10596 = CARTESIAN_POINT ( 'NONE',  ( -1.217612721212264049, -80.58218577482048772, 0.2845431953339345177 ) ) ;
#10597 = AXIS2_PLACEMENT_3D ( 'NONE', #22384, #45428, #22080 ) ;
#10598 = CARTESIAN_POINT ( 'NONE',  ( -6.605942102368285163, -77.67293223250510437, -8.595925543322636031 ) ) ;
#10599 = CARTESIAN_POINT ( 'NONE',  ( 6.728605944993000243, -79.57592971417498973, -7.080011783993000130 ) ) ;
#10600 = EDGE_LOOP ( 'NONE', ( #20585, #56275, #40903, #17611 ) ) ;
#10602 = EDGE_CURVE ( 'NONE', #4925, #44663, #49738, .T. ) ;
#10601 = CARTESIAN_POINT ( 'NONE',  ( 1.199999999999999956, -75.00000000000000000, 7.200000000000000178 ) ) ;
#10603 = CARTESIAN_POINT ( 'NONE',  ( 8.620921567869039848, -25.16528830419391838, -9.346042574068809117 ) ) ;
#10604 = VERTEX_POINT ( 'NONE', #14027 ) ;
#10605 = CARTESIAN_POINT ( 'NONE',  ( -1.541801436820000148, -77.75518664167998395, 0.2953501223290999622 ) ) ;
#10606 = ADVANCED_FACE ( 'NONE', ( #54196 ), #31915, .F. ) ;
#10607 = CARTESIAN_POINT ( 'NONE',  ( 1.009320482739999969, -77.37636915034599383, 9.441330439200999791 ) ) ;
#10608 = CARTESIAN_POINT ( 'NONE',  ( 0.000000000000000000, -76.10312499993298729, -11.80312499993000053 ) ) ;
#10609 = AXIS2_PLACEMENT_3D ( 'NONE', #4625, #22625, #231 ) ;
#10610 = CARTESIAN_POINT ( 'NONE',  ( 10.07627163191000008, -55.55000000209000177, -7.601397897754999633 ) ) ;
#10611 = CARTESIAN_POINT ( 'NONE',  ( 0.2584144826998103217, -16.77154603077302752, -12.70558781487933153 ) ) ;
#10612 = DIRECTION ( 'NONE',  ( 0.000000000000000000, -0.7071067811866525998, -0.7071067811864425456 ) ) ;
#10613 = DIRECTION ( 'NONE',  ( 0.000000000000000000, 1.000000000000000000, 0.000000000000000000 ) ) ;
#10614 = CARTESIAN_POINT ( 'NONE',  ( 0.6984937801707818972, -79.18628347620142449, 1.337435529320990302 ) ) ;
#10615 = CARTESIAN_POINT ( 'NONE',  ( 3.374767226311075952, -81.08958333892509529, 2.240547216630219829 ) ) ;
#10616 = CARTESIAN_POINT ( 'NONE',  ( 7.331368884251999951, -75.80689888741999027, 9.888700222343000945 ) ) ;
#10617 = CARTESIAN_POINT ( 'NONE',  ( 1.452792874191000116, -80.69399715222199632, 0.7047031062512999489 ) ) ;
#10618 = CARTESIAN_POINT ( 'NONE',  ( 9.500000000000000000, -78.14999999999999147, 0.000000000000000000 ) ) ;
#10619 = ADVANCED_FACE ( 'NONE', ( #13438 ), #45642, .F. ) ;
#10620 = CARTESIAN_POINT ( 'NONE',  ( 10.00844230538000090, -60.16891112520000462, -7.647097279411999793 ) ) ;
#10621 = CARTESIAN_POINT ( 'NONE',  ( -12.02296678431999943, -78.50153910486000086, 2.418109797047000242 ) ) ;
#10622 = CARTESIAN_POINT ( 'NONE',  ( -3.164411967817999827, -77.23815627913698734, -11.86639179494000018 ) ) ;
#10623 = CARTESIAN_POINT ( 'NONE',  ( 12.70451796517036236, -16.82354927384910326, -0.5205401191694412066 ) ) ;
#10624 = CARTESIAN_POINT ( 'NONE',  ( 3.011380544091495359, -2.820368407733745197, -1.220682024450374659 ) ) ;
#10625 = CARTESIAN_POINT ( 'NONE',  ( -12.21774757455541227, -77.54059286367716197, 1.402801556591745102 ) ) ;
#10626 = CARTESIAN_POINT ( 'NONE',  ( -11.06493808903000087, -79.26311275777169385, -1.839906431680000010 ) ) ;
#10627 = EDGE_LOOP ( 'NONE', ( #30384, #50389, #33597, #41007 ) ) ;
#10628 = CARTESIAN_POINT ( 'NONE',  ( 0.000000000000000000, -76.10312499993298729, 0.000000000000000000 ) ) ;
#10629 = CARTESIAN_POINT ( 'NONE',  ( 9.133953537529999167, -77.05169957229118438, -3.286716366334999861 ) ) ;
#10630 = CARTESIAN_POINT ( 'NONE',  ( -8.343860018000999190, -59.94999999967000548, 8.343860018000999190 ) ) ;
#10631 = CIRCLE ( 'NONE', #45527, 4.999999999999996447 ) ;
#10632 = CARTESIAN_POINT ( 'NONE',  ( -0.6295237254636286695, -78.91666666666665719, 1.092232985442819881 ) ) ;
#10633 = CARTESIAN_POINT ( 'NONE',  ( 3.682706024758999774, -2.519491823149000442, -1.190799860096000140 ) ) ;
#10634 = EDGE_CURVE ( 'NONE', #52467, #48012, #9030, .T. ) ;
#10635 = CARTESIAN_POINT ( 'NONE',  ( -8.937463246932001226, -77.95036040070399963, 8.081925660605000061 ) ) ;
#10636 = CARTESIAN_POINT ( 'NONE',  ( 5.883202309618000392, -77.88423299304498926, -7.625033806424000637 ) ) ;
#10638 = CARTESIAN_POINT ( 'NONE',  ( -1.229229940090210249, -77.06588541667790082, 9.384114583052001635 ) ) ;
#10637 = CARTESIAN_POINT ( 'NONE',  ( -7.649652380981335043, -76.13136791021121041, 8.919978599461032331 ) ) ;
#10639 = CARTESIAN_POINT ( 'NONE',  ( 0.5739952604901000788, -82.73993688548499392, -1.223314898041000021 ) ) ;
#10640 = CARTESIAN_POINT ( 'NONE',  ( -3.268206247460838210, -85.83735717367099483, 1.381888203335638332 ) ) ;
#10641 = ORIENTED_EDGE ( 'NONE', *, *, #6214, .F. ) ;
#10642 = EDGE_CURVE ( 'NONE', #55505, #22441, #11220, .T. ) ;
#10643 = CARTESIAN_POINT ( 'NONE',  ( 1.500000000000000000, -81.15000000000000568, 0.000000000000000000 ) ) ;
#10644 = CONICAL_SURFACE ( 'NONE', #50250, 2.149999999947999729, 0.7853981633972997312 ) ;
#10645 = B_SPLINE_CURVE_WITH_KNOTS ( 'NONE', 3,
 ( #39166, #57176, #16742, #25876, #43903, #54511 ),
 .UNSPECIFIED., .F., .F.,
 ( 4, 1, 1, 4 ),
 ( 0.000000000000000000, 0.3333333333333000081, 0.6666666666667000474, 1.000000000000000000 ),
 .UNSPECIFIED. ) ;
#10646 = CARTESIAN_POINT ( 'NONE',  ( -12.11464257907000075, -79.76545167379698853, -1.005257255610999989 ) ) ;
#10647 = CARTESIAN_POINT ( 'NONE',  ( 9.503328962285682024, -79.49493491590959593, -0.6046619501317949119 ) ) ;
#10648 = CARTESIAN_POINT ( 'NONE',  ( -1.250000000000000000, -82.25000000000000000, 8.279869130157999738E-11 ) ) ;
#10649 = CARTESIAN_POINT ( 'NONE',  ( 3.915498778898000687, -79.33642597743899216, 10.25343288338999947 ) ) ;
#10650 = CARTESIAN_POINT ( 'NONE',  ( -0.5870567661726286968, -79.18616477877183968, -1.103542300118057984 ) ) ;
#10651 = CARTESIAN_POINT ( 'NONE',  ( -10.44613170738330332, -80.07483812962188097, 3.446999337742282510 ) ) ;
#10652 = CARTESIAN_POINT ( 'NONE',  ( 9.248423471988997946, -79.91665467088898822, 2.825168219357999888 ) ) ;
#10653 = CARTESIAN_POINT ( 'NONE',  ( 8.870405106263998363, -16.93036971772000143, -8.878274241758997931 ) ) ;
#10654 = DIRECTION ( 'NONE',  ( -1.000000000000000000, 0.000000000000000000, 0.000000000000000000 ) ) ;
#10655 = EDGE_LOOP ( 'NONE', ( #12259, #41964, #41739, #4145, #42471, #14538, #52640, #55016, #28094, #16860, #40119, #22029 ) ) ;
#10657 = AXIS2_PLACEMENT_3D ( 'NONE', #54057, #31587, #22457 ) ;
#10656 = CARTESIAN_POINT ( 'NONE',  ( -0.2732061834123999944, -79.15352125521398818, 11.25874428786999992 ) ) ;
#10658 = CARTESIAN_POINT ( 'NONE',  ( -11.08419787132735124, -76.36051769991946969, -1.489531927970142000 ) ) ;
#10659 = CARTESIAN_POINT ( 'NONE',  ( 10.75000000000000000, -79.75000000000000000, 0.000000000000000000 ) ) ;
#10660 = CARTESIAN_POINT ( 'NONE',  ( -13.95956770371999944, -45.71924237694000226, -5.182383547034000008E-05 ) ) ;
#10661 = CARTESIAN_POINT ( 'NONE',  ( -10.35422612692059197, -77.91059695121818152, 6.109131574142480758 ) ) ;
#10662 = B_SPLINE_SURFACE_WITH_KNOTS ( 'NONE', 3, 3, ( 
 ( #33932, #51970, #21230, #18205, #9630, #32041, #40631, #226, #31155, #39234, #27618, #53926, #53620, #27904, #50086, #45658, #5201, #54214, #18488 ),
 ( #36481, #9045, #35894, #23202, #49193, #27329, #58342, #41207, #8745, #36771, #49794, #13749, #9340, #54510, #512, #54789, #22619, #45363, #50375 ),
 ( #26736, #797, #18779, #4912, #22316, #22911, #9922, #31749, #40924, #13458, #14331, #14047, #32328, #3238, #58043, #17603, #35592, #27031, #13158 ),
 ( #44767, #4316, #40333, #17905, #4620, #31454, #49496, #45068, #36196, #46540, #19648, #23778, #37937, #55960, #45950, #19361, #55370, #41500, #24373 ) ),
 .UNSPECIFIED., .F., .F., .F.,
 ( 4, 4 ),
 ( 4, 1, 1, 1, 1, 1, 1, 1, 1, 1, 1, 1, 1, 1, 1, 1, 4 ),
 ( -0.02000000000000999936, 1.020000000000000018 ),
 ( -0.01116670151518999940, 0.02512507840917000204, 0.06141685833353999896, 0.09770863825790000734, 0.1340004181822999907, 0.1702921981065999846, 0.2065839780310000096, 0.2428757579554000068, 0.2791675378797000007, 0.3154593178041000257, 0.3517510977284000195, 0.3880428776527999890, 0.4243346575772000140, 0.4606264375015000079, 0.4969182174258999773, 0.5332099973503000578, 0.5695017772746000517 ),
 .UNSPECIFIED. ) ;
#10663 = AXIS2_PLACEMENT_3D ( 'NONE', #13967, #22831, #13377 ) ;
#10664 = CARTESIAN_POINT ( 'NONE',  ( -0.5999999999999999778, -5.000000000000000000, 4.000000000000000000 ) ) ;
#10665 = CARTESIAN_POINT ( 'NONE',  ( 9.376568502766771118, -79.55367501876179404, -6.156425267692819503 ) ) ;
#10666 = CARTESIAN_POINT ( 'NONE',  ( 12.50745077494999968, -61.79994448255000350, 2.662030659623000237E-09 ) ) ;
#10667 = FACE_OUTER_BOUND ( 'NONE', #8292, .T. ) ;
#10668 = CARTESIAN_POINT ( 'NONE',  ( 0.7508852574861999418, -78.75368549038000765, -1.070959314402999851 ) ) ;
#10669 = CARTESIAN_POINT ( 'NONE',  ( 1.980464483675000054, -20.24439829391000245, 12.85140862646999871 ) ) ;
#10670 = CARTESIAN_POINT ( 'NONE',  ( 6.718136267461014555, -79.12751925484205628, -8.679542842522213419 ) ) ;
#10671 = CARTESIAN_POINT ( 'NONE',  ( -9.312500000004000356, -79.68749999999599254, 6.570867420027000168E-10 ) ) ;
#10672 = ORIENTED_EDGE ( 'NONE', *, *, #51508, .T. ) ;
#10673 = ORIENTED_EDGE ( 'NONE', *, *, #15474, .F. ) ;
#10674 = CARTESIAN_POINT ( 'NONE',  ( 7.265173101945999967, -77.68705665246400827, 6.414655419558000560 ) ) ;
#10675 = CARTESIAN_POINT ( 'NONE',  ( 8.973809496257258544, -78.80375026939715610, -5.918774935595488174 ) ) ;
#10676 = ORIENTED_EDGE ( 'NONE', *, *, #683, .F. ) ;
#10677 = CARTESIAN_POINT ( 'NONE',  ( 9.788022091682998749, -17.47120090402999892, 7.956349397064001572 ) ) ;
#10678 = CARTESIAN_POINT ( 'NONE',  ( -8.833271293965303528, -79.36966988906971210, 3.510040627682449177 ) ) ;
#10679 = CARTESIAN_POINT ( 'NONE',  ( -11.90254689395000121, -78.34440606474001356, -1.953697528535000005 ) ) ;
#10680 = CARTESIAN_POINT ( 'NONE',  ( 8.533826143256000307, -61.80526450216999734, 9.213084459935000581 ) ) ;
#10681 = CARTESIAN_POINT ( 'NONE',  ( 1.249647686960656756, -82.36107796002586667, 0.1638768531599422151 ) ) ;
#10682 = CARTESIAN_POINT ( 'NONE',  ( -8.149016987013476765, -78.61537467219939401, -8.781430036993665311 ) ) ;
#10683 = AXIS2_PLACEMENT_3D ( 'NONE', #9884, #11061, #41755 ) ;
#10684 = CARTESIAN_POINT ( 'NONE',  ( 11.21485848424000054, -80.15017646456679756, -0.2123177049684000228 ) ) ;
#10685 = ORIENTED_EDGE ( 'NONE', *, *, #39465, .T. ) ;
#10686 = CARTESIAN_POINT ( 'NONE',  ( -9.697372265328400687, -24.97233735039882063, 8.266620275706634047 ) ) ;
#10687 = ORIENTED_EDGE ( 'NONE', *, *, #46657, .F. ) ;
#10688 = CARTESIAN_POINT ( 'NONE',  ( 7.479723288845285367, -77.40016007753332872, 5.441954638049121940 ) ) ;
#10689 = CARTESIAN_POINT ( 'NONE',  ( -9.177034484502000211, -77.44354714383098326, 6.137278520473000043 ) ) ;
#10690 = CARTESIAN_POINT ( 'NONE',  ( 11.19195961368080461, -77.60522894247633019, 0.7494324316197222835 ) ) ;
#10691 = CARTESIAN_POINT ( 'NONE',  ( 9.131029190779001325, -77.61296824509499004, -3.285576857342999979 ) ) ;
#10692 = AXIS2_PLACEMENT_3D ( 'NONE', #33048, #2085, #20083 ) ;
#10693 = CARTESIAN_POINT ( 'NONE',  ( -7.374560639698973574, -77.47291666666666288, -9.596002108778167283 ) ) ;
#10694 = ADVANCED_FACE ( 'NONE', ( #35879 ), #22603, .F. ) ;
#10695 = CARTESIAN_POINT ( 'NONE',  ( 0.000000000000000000, -60.04999999966999980, -12.50000000000000000 ) ) ;
#10696 = CARTESIAN_POINT ( 'NONE',  ( 1.169626569868999821, -78.20001146263999203, 1.131652196797999999 ) ) ;
#10697 = CIRCLE ( 'NONE', #30431, 1.749999999999999556 ) ;
#10698 = CARTESIAN_POINT ( 'NONE',  ( 8.926269970182000080, -78.69290956889000199, -6.511497375149000177 ) ) ;
#10699 = ADVANCED_FACE ( 'NONE', ( #35277 ), #30853, .F. ) ;
#10700 = CARTESIAN_POINT ( 'NONE',  ( 12.70556836352000118, -62.02772277195000328, 2.424222323408999617E-09 ) ) ;
#10701 = CARTESIAN_POINT ( 'NONE',  ( 12.60552522438000089, -60.08917565288000162, -1.799501877759999813 ) ) ;
#10702 = CARTESIAN_POINT ( 'NONE',  ( 1.941182638762999790, -82.69930595706300380, 2.968725317687999965 ) ) ;
#10703 = EDGE_LOOP ( 'NONE', ( #38288, #24157, #39616, #39345, #10673, #56164 ) ) ;
#10704 = CARTESIAN_POINT ( 'NONE',  ( -10.22338514145507737, -77.19999999999998863, 3.927200133048044606 ) ) ;
#10705 = CARTESIAN_POINT ( 'NONE',  ( 6.194304543013999798, -76.10681943937400717, 9.822204756253000824 ) ) ;
#10706 = CARTESIAN_POINT ( 'NONE',  ( 9.532032162674793696, -77.88842254387341768, 4.970338045911559810 ) ) ;
#10707 = CARTESIAN_POINT ( 'NONE',  ( 2.228685126279000173, -77.99400319886400723, 11.77068507108999995 ) ) ;
#10708 = CARTESIAN_POINT ( 'NONE',  ( -7.634437838915999919, -18.25219468451000182, 10.30764259110000047 ) ) ;
#10709 = CARTESIAN_POINT ( 'NONE',  ( -1.267102727772119630, -78.25904358090664914, -0.1447965901780092768 ) ) ;
#10710 = CARTESIAN_POINT ( 'NONE',  ( -3.572991711198483245, -2.758169930076621146, -0.3534553494227741233 ) ) ;
#10711 = CARTESIAN_POINT ( 'NONE',  ( 0.000000000000000000, -60.04999999966999980, -12.00000000000000000 ) ) ;
#10712 = CARTESIAN_POINT ( 'NONE',  ( 2.781615572646999990, -77.72805768234898949, -8.992986673707997980 ) ) ;
#10713 = CARTESIAN_POINT ( 'NONE',  ( -6.651871862604989083, -85.83735716284299144, -5.470707629659896654 ) ) ;
#10714 = CARTESIAN_POINT ( 'NONE',  ( -9.301504212792000459, -78.50403817759199399, -5.931589059777999218 ) ) ;
#10715 = CARTESIAN_POINT ( 'NONE',  ( 2.700519054749793924, -0.8736979072298788340, -2.074293297084300214 ) ) ;
#10716 = FACE_OUTER_BOUND ( 'NONE', #31227, .T. ) ;
#10717 = ORIENTED_EDGE ( 'NONE', *, *, #20456, .T. ) ;
#10718 = EDGE_CURVE ( 'NONE', #35763, #32105, #20857, .T. ) ;
#10719 = CARTESIAN_POINT ( 'NONE',  ( -0.1832406609208000192, -81.87969241135199638, -1.320984106490000087 ) ) ;
#10720 = CARTESIAN_POINT ( 'NONE',  ( 1.669724228651999987, -60.16897676502000536, -12.48434610070000161 ) ) ;
#10721 = CARTESIAN_POINT ( 'NONE',  ( -10.75000000000000000, -80.59999999999999432, 0.000000000000000000 ) ) ;
#10722 = CARTESIAN_POINT ( 'NONE',  ( 0.2654799511899000319, -78.46077795102900154, -11.21373274707999990 ) ) ;
#10723 = CARTESIAN_POINT ( 'NONE',  ( -2.928603948516999900, -78.70603953110398265, 10.57767911662999971 ) ) ;
#10724 = CARTESIAN_POINT ( 'NONE',  ( 7.605690822180000588, -23.42565082156999878, -10.52682217035000001 ) ) ;
#10725 = CARTESIAN_POINT ( 'NONE',  ( -1.356913547520186114, -85.90729168422163298, 3.776425161692174903 ) ) ;
#10726 = CARTESIAN_POINT ( 'NONE',  ( -2.486393044377000372, -77.11762553470499881, -12.01527121392999931 ) ) ;
#10727 = CARTESIAN_POINT ( 'NONE',  ( -10.25203062048491987, -54.67822876342075489, -7.730397977250241581 ) ) ;
#10728 = ORIENTED_EDGE ( 'NONE', *, *, #34778, .T. ) ;
#10729 = CARTESIAN_POINT ( 'NONE',  ( 3.674832906577000013, -85.31342953870898782, -1.975385622428000199 ) ) ;
#10730 = CARTESIAN_POINT ( 'NONE',  ( -1.310679582531389498, -80.45833333333332860, 0.7554284705563444335 ) ) ;
#10731 = ADVANCED_FACE ( 'NONE', ( #26722 ), #36464, .T. ) ;
#10732 = AXIS2_PLACEMENT_3D ( 'NONE', #48758, #3875, #39883 ) ;
#10734 = EDGE_CURVE ( 'NONE', #42913, #37628, #57432, .T. ) ;
#10733 = CARTESIAN_POINT ( 'NONE',  ( 8.478741751108000102, -53.92187496570999627, -9.108230428579000559 ) ) ;
#10735 = CARTESIAN_POINT ( 'NONE',  ( 7.228832758458999308, -77.09612980692300255, 8.635852100895000660 ) ) ;
#10736 = CARTESIAN_POINT ( 'NONE',  ( 0.8512149552595998925, -80.10271428023000340, 1.432023780608000063 ) ) ;
#10737 = CARTESIAN_POINT ( 'NONE',  ( 0.9221831299987999220, -79.33343026601998815, 0.9445928090476000127 ) ) ;
#10738 = DIRECTION ( 'NONE',  ( 0.000000000000000000, 1.000000000000000000, 0.000000000000000000 ) ) ;
#10739 = FACE_OUTER_BOUND ( 'NONE', #2504, .T. ) ;
#10740 = CARTESIAN_POINT ( 'NONE',  ( 1.250000000000000000, -82.74999999999998579, 0.000000000000000000 ) ) ;
#10741 = EDGE_LOOP ( 'NONE', ( #27598, #8469, #7602, #23723, #32272, #46769, #8690, #3327, #42343 ) ) ;
#10742 = CARTESIAN_POINT ( 'NONE',  ( -8.485281374238999419, -60.04999999966999980, 8.485281374238999419 ) ) ;
#10743 = AXIS2_PLACEMENT_3D ( 'NONE', #25782, #43808, #20779 ) ;
#10744 = CARTESIAN_POINT ( 'NONE',  ( -0.7554284705563483193, -77.98333333333334849, -1.310679582531387721 ) ) ;
#10745 = ORIENTED_EDGE ( 'NONE', *, *, #50924, .T. ) ;
#10746 = CARTESIAN_POINT ( 'NONE',  ( 0.4716226049498870587, -81.75588184218486276, -1.157571032113124954 ) ) ;
#10747 = CARTESIAN_POINT ( 'NONE',  ( 11.02987528609000023, -80.20735716685899774, -0.2088156359816000229 ) ) ;
#10748 = CARTESIAN_POINT ( 'NONE',  ( 0.000000000000000000, -75.67500000000001137, 0.000000000000000000 ) ) ;
#10749 = ORIENTED_EDGE ( 'NONE', *, *, #43021, .T. ) ;
#10750 = VERTEX_POINT ( 'NONE', #8433 ) ;
#10751 = CARTESIAN_POINT ( 'NONE',  ( -0.2083289567832000144, -81.66134554112100830, -1.501845930097000181 ) ) ;
#10752 = ORIENTED_EDGE ( 'NONE', *, *, #497, .T. ) ;
#10753 = ORIENTED_EDGE ( 'NONE', *, *, #28766, .F. ) ;
#10754 = CARTESIAN_POINT ( 'NONE',  ( 1.814305421036000121, -17.71058030669000161, 12.78003582253000125 ) ) ;
#10755 = APPLICATION_PROTOCOL_DEFINITION ( 'draft international standard', 'automotive_design', 1998, #45119 ) ;
#10756 = CARTESIAN_POINT ( 'NONE',  ( 0.000000000000000000, -39.30476017083000073, 0.000000000000000000 ) ) ;
#10757 = CARTESIAN_POINT ( 'NONE',  ( -7.629208874607999569, -79.37681001420199323, -6.499394396314999156 ) ) ;
#10758 = CARTESIAN_POINT ( 'NONE',  ( 5.918406792461694543, -78.28036926306923249, -7.108720655904040342 ) ) ;
#10759 = CARTESIAN_POINT ( 'NONE',  ( -1.500000000000000000, -80.90000000000000568, 0.000000000000000000 ) ) ;
#10760 = ORIENTED_EDGE ( 'NONE', *, *, #24981, .F. ) ;
#10761 = ORIENTED_EDGE ( 'NONE', *, *, #27057, .T. ) ;
#10762 = CARTESIAN_POINT ( 'NONE',  ( -9.137085346172289846, -77.58769485083752215, 1.440358904308211674 ) ) ;
#10763 = CARTESIAN_POINT ( 'NONE',  ( -12.70556836347999941, -25.22772277227999993, -2.424223956931999920E-09 ) ) ;
#10764 = CARTESIAN_POINT ( 'NONE',  ( 0.3271848554490964789, -81.35416666666667140, 1.217465845835395521 ) ) ;
#10765 = CARTESIAN_POINT ( 'NONE',  ( 1.782734487938277379, -60.92245368521658122, -12.71547286929869180 ) ) ;
#10766 = CARTESIAN_POINT ( 'NONE',  ( -9.346518596363001308, -77.74817685591499128, 2.610229778083999808 ) ) ;
#10767 = CYLINDRICAL_SURFACE ( 'NONE', #47355, 0.5999999999999999778 ) ;
#10768 = CARTESIAN_POINT ( 'NONE',  ( 10.75000000000000000, -76.85000000000000853, 0.000000000000000000 ) ) ;
#10769 = CARTESIAN_POINT ( 'NONE',  ( 0.000000000000000000, -80.74999999986198418, 0.000000000000000000 ) ) ;
#10770 = CARTESIAN_POINT ( 'NONE',  ( -1.418768848999000021, -79.72334218465999811, 0.9417588900106000915 ) ) ;
#10771 = VECTOR ( 'NONE', #25446, 1000.000000000000000 ) ;
#10772 = CARTESIAN_POINT ( 'NONE',  ( 9.416651550578160723, -77.29347193750339784, -0.7559916624287352782 ) ) ;
#10773 = CARTESIAN_POINT ( 'NONE',  ( -5.863032908986463454, -76.61570338723420548, 10.21229380548447274 ) ) ;
#10774 = CARTESIAN_POINT ( 'NONE',  ( 8.504267844457428893, -79.24218749521728000, -8.507439143850103136 ) ) ;
#10775 = CARTESIAN_POINT ( 'NONE',  ( -1.118026905147402328, -79.80863251002027425, -1.015872027318809101 ) ) ;
#10776 = CARTESIAN_POINT ( 'NONE',  ( 7.022198843594999573, -77.87837668086899612, 6.200125618097000135 ) ) ;
#10777 = CARTESIAN_POINT ( 'NONE',  ( -1.750000000000000000, -20.24935285954000008, -12.65372179284999810 ) ) ;
#10778 = CARTESIAN_POINT ( 'NONE',  ( 2.062502994258999856, -20.24351820077000141, -12.92181194099999963 ) ) ;
#10780 = CARTESIAN_POINT ( 'NONE',  ( 1.930628539545000022, -18.77875555914000216, -12.72375828104000028 ) ) ;
#10779 = CARTESIAN_POINT ( 'NONE',  ( 0.3926218265389159745, -78.75416666666666288, 1.460959015002474493 ) ) ;
#10781 = CARTESIAN_POINT ( 'NONE',  ( -4.657764537801160287, -79.51694645399435046, 8.081867300299901302 ) ) ;
#10782 = CARTESIAN_POINT ( 'NONE',  ( -7.624341764943999955, -60.06485149430999826, 10.42531124854999902 ) ) ;
#10783 = CARTESIAN_POINT ( 'NONE',  ( -10.97713377773999888, -78.34134770576399376, -2.517240518847000175 ) ) ;
#10784 = CARTESIAN_POINT ( 'NONE',  ( -14.00000000000000000, -69.50420297070000686, 0.000000000000000000 ) ) ;
#10785 = CARTESIAN_POINT ( 'NONE',  ( 8.385799987749599893, -61.68809827201926055, 9.298537617308133107 ) ) ;
#10786 = EDGE_CURVE ( 'NONE', #52834, #36325, #8941, .T. ) ;
#10787 = CARTESIAN_POINT ( 'NONE',  ( -8.485281374238999419, -23.25000000000000000, 8.485281374238999419 ) ) ;
#10788 = FACE_OUTER_BOUND ( 'NONE', #4194, .T. ) ;
#10789 = CARTESIAN_POINT ( 'NONE',  ( -0.001976671226007847143, -78.47534806730480739, 1.249865324143346168 ) ) ;
#10790 = CARTESIAN_POINT ( 'NONE',  ( 5.228979477480000249, -79.62813585431899810, -7.971711000620000043 ) ) ;
#10791 = CARTESIAN_POINT ( 'NONE',  ( 5.647598101448999763, -77.78727586459000065, 11.72364604052000203 ) ) ;
#10792 = CARTESIAN_POINT ( 'NONE',  ( -9.703099203832849184, -79.34568276157449418, 0.5050087370209813686 ) ) ;
#10793 = CARTESIAN_POINT ( 'NONE',  ( 7.344871482613403835, -79.41513455956103940, 7.849784798595977442 ) ) ;
#10794 = CARTESIAN_POINT ( 'NONE',  ( 1.250000000000000000, -79.34999999999999432, 0.000000000000000000 ) ) ;
#10795 = CARTESIAN_POINT ( 'NONE',  ( 4.000000000000000000, -75.00000000000001421, 0.5999999999999999778 ) ) ;
#10796 = CARTESIAN_POINT ( 'NONE',  ( 10.36233872082999774, -77.89696215211898789, -4.441556149583999691 ) ) ;
#10797 = EDGE_CURVE ( 'NONE', #18403, #30305, #27220, .T. ) ;
#10798 = VECTOR ( 'NONE', #27946, 1000.000000000000000 ) ;
#10799 = CARTESIAN_POINT ( 'NONE',  ( -1.004225369717999916, -80.97922849090299735, -1.250800220804000107 ) ) ;
#10800 = CARTESIAN_POINT ( 'NONE',  ( -9.631455446501000495, -78.16094514476064603, -1.333735528292999906 ) ) ;
#10801 = CARTESIAN_POINT ( 'NONE',  ( -8.485281374238999419, -55.64999999967000122, -8.485281374238999419 ) ) ;
#10803 = CARTESIAN_POINT ( 'NONE',  ( -3.206516299415000049, -1.613032031399000088, -0.5298615117031000299 ) ) ;
#10802 = CARTESIAN_POINT ( 'NONE',  ( -0.7270104252018999569, -83.22378845168798023, -3.685488592395000040 ) ) ;
#10804 = DIRECTION ( 'NONE',  ( 0.000000000000000000, 1.000000000000000000, 0.000000000000000000 ) ) ;
#10805 = CARTESIAN_POINT ( 'NONE',  ( 5.137083998358000336, -77.21100733245999947, -10.56753840748999984 ) ) ;
#10806 = CARTESIAN_POINT ( 'NONE',  ( 5.627879961911095741, -80.26928327484587555, -9.165441168818450279 ) ) ;
#10807 = AXIS2_PLACEMENT_3D ( 'NONE', #8362, #26360, #3932 ) ;
#10808 = CARTESIAN_POINT ( 'NONE',  ( -6.241704289952512141, -77.17585973208710470, -8.752229220649864416 ) ) ;
#10809 = DIRECTION ( 'NONE',  ( 0.7071067811865475727, 0.000000000000000000, 0.7071067811865475727 ) ) ;
#10810 = VERTEX_POINT ( 'NONE', #46230 ) ;
#10811 = ORIENTED_EDGE ( 'NONE', *, *, #51087, .F. ) ;
#10812 = CARTESIAN_POINT ( 'NONE',  ( 10.52307592342000042, -79.42414610975299638, 5.828552047478999576 ) ) ;
#10813 = CONICAL_SURFACE ( 'NONE', #43804, 2.949999999500999781, 0.7853981633972997312 ) ;
#10814 = CARTESIAN_POINT ( 'NONE',  ( 0.000000000000000000, -76.79999999999999716, 0.000000000000000000 ) ) ;
#10815 = LINE ( 'NONE', #28794, #30319 ) ;
#10816 = B_SPLINE_CURVE_WITH_KNOTS ( 'NONE', 3,
 ( #36607, #54630, #54341, #13880 ),
 .UNSPECIFIED., .F., .F.,
 ( 4, 4 ),
 ( 0.000000000000000000, 1.000000000000000000 ),
 .UNSPECIFIED. ) ;
#10817 = ORIENTED_EDGE ( 'NONE', *, *, #47097, .F. ) ;
#10818 =( REPRESENTATION_RELATIONSHIP ('NONE','NONE', #58051, #4074 ) REPRESENTATION_RELATIONSHIP_WITH_TRANSFORMATION ( #16911 )SHAPE_REPRESENTATION_RELATIONSHIP( ) );
#10819 = CARTESIAN_POINT ( 'NONE',  ( -11.88268207399999987, -77.63083722509800566, -1.112370969927999997 ) ) ;
#10820 = EDGE_CURVE ( 'NONE', #18938, #2185, #13847, .T. ) ;
#10821 = EDGE_LOOP ( 'NONE', ( #5208, #35022, #10518, #28958 ) ) ;
#10822 = ORIENTED_EDGE ( 'NONE', *, *, #5924, .T. ) ;
#10823 = CARTESIAN_POINT ( 'NONE',  ( 8.137215171343381570, -60.25155696365702340, 7.401770473315491650 ) ) ;
#10824 = ORIENTED_EDGE ( 'NONE', *, *, #7171, .T. ) ;
#10825 = FACE_OUTER_BOUND ( 'NONE', #42513, .T. ) ;
#10826 = CARTESIAN_POINT ( 'NONE',  ( 8.730844907503701791, -79.18198688127804985, 3.749782986556219111 ) ) ;
#10827 = VERTEX_POINT ( 'NONE', #55945 ) ;
#10828 = CARTESIAN_POINT ( 'NONE',  ( -0.9992933932515307704, -82.65243683341363123, -0.7674328717235032737 ) ) ;
#10829 = VERTEX_POINT ( 'NONE', #14314 ) ;
#10830 = CARTESIAN_POINT ( 'NONE',  ( 2.568255498652000313, -2.248719782538000089, -2.230126530280999830 ) ) ;
#10831 = VERTEX_POINT ( 'NONE', #41482 ) ;
#10832 = CARTESIAN_POINT ( 'NONE',  ( -1.199999995321999968, -75.00000000467838390, 7.199999972488000388 ) ) ;
#10833 = CARTESIAN_POINT ( 'NONE',  ( 0.8523209396086280920, -78.42219961258000183, -1.272697597679407933 ) ) ;
#10834 = CARTESIAN_POINT ( 'NONE',  ( -9.614379292984539305, -79.79999999999998295, -7.044348044756020499 ) ) ;
#10835 = PLANE ( 'NONE',  #15220 ) ;
#10836 = CARTESIAN_POINT ( 'NONE',  ( 0.000000000000000000, -80.79999999999999716, 0.000000000000000000 ) ) ;
#10837 = CARTESIAN_POINT ( 'NONE',  ( 9.499178638196321245, -79.00092112126561972, 0.1004274591880019996 ) ) ;
#10838 = CARTESIAN_POINT ( 'NONE',  ( 7.995633008690000487, -76.50993067858900076, 7.819446035993999899 ) ) ;
#10839 = CARTESIAN_POINT ( 'NONE',  ( -0.09237677837556851346, -79.72557714387301075, 9.715793344066241843 ) ) ;
#10840 = AXIS2_PLACEMENT_3D ( 'NONE', #13369, #31367, #22233 ) ;
#10841 = CARTESIAN_POINT ( 'NONE',  ( 7.809513865093999918, -76.50961320193900406, -8.068161004599000208 ) ) ;
#10842 = CARTESIAN_POINT ( 'NONE',  ( -6.203490556899441621, -78.66660757515437297, -6.861839749120386855 ) ) ;
#10843 = CARTESIAN_POINT ( 'NONE',  ( 6.551839081868985559, -76.52774692925073907, 9.753635134337040213 ) ) ;
#10844 = CARTESIAN_POINT ( 'NONE',  ( -7.901745553563000790, -77.11636001420200159, -5.112651159007999269 ) ) ;
#10845 = CARTESIAN_POINT ( 'NONE',  ( -1.154258600661999923, -79.67608924354598798, -0.6680293646364998672 ) ) ;
#10846 = AXIS2_PLACEMENT_3D ( 'NONE', #32814, #50861, #5967 ) ;
#10847 = CARTESIAN_POINT ( 'NONE',  ( -5.338532579233360664, -80.18476939357704225, -9.618388971371432561 ) ) ;
#10848 = CARTESIAN_POINT ( 'NONE',  ( -2.723040898605983084, -3.054315476261060258, 1.788012656602580019 ) ) ;
#10849 = B_SPLINE_CURVE_WITH_KNOTS ( 'NONE', 3,
 ( #54700, #46744, #37555, #33119, #32823, #37264, #28400, #41704, #41997, #1280, #50283, #32530, #51161, #55872, #15423, #42297, #19273, #19557, #5112, #55278, #27815, #46446, #19857, #15121, #1862, #9834, #28106, #713, #33415, #14824, #51453, #50868, #14244, #50573, #32240 ),
 .UNSPECIFIED., .F., .F.,
 ( 4, 1, 1, 1, 1, 1, 1, 1, 1, 1, 1, 1, 1, 1, 1, 1, 1, 1, 1, 1, 1, 1, 1, 1, 1, 1, 1, 1, 1, 1, 1, 1, 4 ),
 ( 0.000000000000000000, 0.01250277026799517452, 0.04500258559214889015, 0.07750240091630128392, 0.1100022162404669240, 0.1425020315645531277, 0.1750018468888378809, 0.2075016622129902677, 0.2400014775371426823, 0.2725012928612950969, 0.3050011081854474559, 0.3375009235095998705, 0.3700007388337522296, 0.4025005541579046442, 0.4350003694820570588, 0.4675001848062094179, 0.5000000001303618324, 0.5324998154545141915, 0.5649996307786665506, 0.5974994461028189097, 0.6299992614269713798, 0.6624990767511239609, 0.6949988920752763200, 0.7274987073994286790, 0.7599985227235809271, 0.7924983380477335082, 0.8249981533718857563, 0.8574979686960381153, 0.8899977840201905854, 0.9224975993443429445, 0.9549974146684953036, 0.9874972299926477737, 1.000000000000000000 ),
 .UNSPECIFIED. ) ;
#10850 = CARTESIAN_POINT ( 'NONE',  ( -0.05262135556323999791, -79.64017549782629146, 3.589006617443000202 ) ) ;
#10851 = CARTESIAN_POINT ( 'NONE',  ( -3.771648689937000309, -79.40887399616899245, 11.60274953364999995 ) ) ;
#10852 = CARTESIAN_POINT ( 'NONE',  ( -9.469160009696521385, -78.06080311739077615, 5.094555813102688013 ) ) ;
#10853 = CARTESIAN_POINT ( 'NONE',  ( 0.4492946238560011629, -82.94576776959728193, 1.166509796814039213 ) ) ;
#10854 = CARTESIAN_POINT ( 'NONE',  ( 7.714303428875997959, -52.49705297113997204, 12.53545825868000385 ) ) ;
#10855 = CARTESIAN_POINT ( 'NONE',  ( -11.65013480063129059, -76.21076195607875547, -1.612759596057231848 ) ) ;
#10856 = CARTESIAN_POINT ( 'NONE',  ( 3.931521788677165397, -79.99999999999997158, 8.490588278901316954 ) ) ;
#10857 = CARTESIAN_POINT ( 'NONE',  ( -10.47513974136000137, -60.60361494148999384, -7.624776006180999488 ) ) ;
#10858 = EDGE_CURVE ( 'NONE', #55619, #18438, #32135, .T. ) ;
#10859 = CIRCLE ( 'NONE', #11768, 1.250000000000000444 ) ;
#10860 = DIRECTION ( 'NONE',  ( 1.996950752507999982E-10, 1.000000000000000000, -5.653827411922000189E-11 ) ) ;
#10861 = CARTESIAN_POINT ( 'NONE',  ( 0.1510373474112000070, -81.50030724171101326, 1.325052402434999888 ) ) ;
#10862 = EDGE_CURVE ( 'NONE', #16112, #52194, #43457, .T. ) ;
#10863 = CARTESIAN_POINT ( 'NONE',  ( 3.250000000000000000, -2.250000000000000000, 0.000000000000000000 ) ) ;
#10864 = DIRECTION ( 'NONE',  ( 1.000000000000000000, 0.000000000000000000, 0.000000000000000000 ) ) ;
#10865 = CARTESIAN_POINT ( 'NONE',  ( -8.792818914773597783, -25.22696626442860790, -9.175540344814811178 ) ) ;
#10866 = CARTESIAN_POINT ( 'NONE',  ( 2.464155593302254754, -77.80709632922713581, 10.48634603565272627 ) ) ;
#10867 = FILL_AREA_STYLE ('',( #37993 ) ) ;
#10868 = CARTESIAN_POINT ( 'NONE',  ( 7.318097147681000614, -79.53307939262458603, -8.179820946710000484 ) ) ;
#10869 = CARTESIAN_POINT ( 'NONE',  ( 10.40273743810999996, -75.96241156850999232, 6.396609211732999789 ) ) ;
#10870 = VERTEX_POINT ( 'NONE', #29918 ) ;
#10871 = CARTESIAN_POINT ( 'NONE',  ( -4.092565674317000024, -83.35607450217399617, 0.5562462044220999324 ) ) ;
#10872 = CARTESIAN_POINT ( 'NONE',  ( 10.00561547635000004, -80.92054906910999534, -5.227788429194999864 ) ) ;
#10873 = CARTESIAN_POINT ( 'NONE',  ( 8.720468637437409853, -78.32301164407923011, -3.084721045281239249 ) ) ;
#10874 = DIRECTION ( 'NONE',  ( 0.000000000000000000, -1.000000000000000000, 0.000000000000000000 ) ) ;
#10875 = CARTESIAN_POINT ( 'NONE',  ( -4.647088938219000376, -78.31067576028999611, 10.20895072913000057 ) ) ;
#10876 = CARTESIAN_POINT ( 'NONE',  ( 12.43421868114999995, -54.36340276600000010, -1.197355605038999959 ) ) ;
#10877 = CARTESIAN_POINT ( 'NONE',  ( -5.638451105654999296, -78.46829086006698617, -7.807757622656001040 ) ) ;
#10878 = CARTESIAN_POINT ( 'NONE',  ( 0.6304340365998000184, -82.73294032889000960, 1.542015542100000136 ) ) ;
#10879 = DIRECTION ( 'NONE',  ( 0.000000000000000000, -1.000000000000000000, 0.000000000000000000 ) ) ;
#10880 = CARTESIAN_POINT ( 'NONE',  ( 2.858407197969000002, -77.00000000000000000, 8.797272775729998884 ) ) ;
#10881 = ORIENTED_EDGE ( 'NONE', *, *, #53680, .F. ) ;
#10882 = DIRECTION ( 'NONE',  ( 0.000000000000000000, -1.000000000000000000, 0.000000000000000000 ) ) ;
#10883 = CARTESIAN_POINT ( 'NONE',  ( 1.232169104480089317, -78.93020734066399768, -3.305722366503252019 ) ) ;
#10884 = VERTEX_POINT ( 'NONE', #43233 ) ;
#10885 = CARTESIAN_POINT ( 'NONE',  ( -1.182296476285000120, -78.59606059609599527, 0.6170503964917000150 ) ) ;
#10886 = CARTESIAN_POINT ( 'NONE',  ( -7.069392057028999865, -79.23718652232298609, 8.491265488204000178 ) ) ;
#10887 = CARTESIAN_POINT ( 'NONE',  ( -8.975709286823001065, -80.12499131680598907, 7.273687588511000612 ) ) ;
#10888 = ORIENTED_EDGE ( 'NONE', *, *, #55553, .F. ) ;
#10889 = CARTESIAN_POINT ( 'NONE',  ( 10.85897810694999954, -78.47165355494099970, -5.483167429328999809 ) ) ;
#10890 = CARTESIAN_POINT ( 'NONE',  ( 3.641219478425000045, -77.27160782317299947, -10.83718297704999856 ) ) ;
#10891 = CIRCLE ( 'NONE', #43876, 0.5000000000000001110 ) ;
#10892 = CARTESIAN_POINT ( 'NONE',  ( 8.768124086712999699, -59.94999999967000548, -7.919595949288999570 ) ) ;
#10893 = ORIENTED_EDGE ( 'NONE', *, *, #56086, .F. ) ;
#10894 = EDGE_LOOP ( 'NONE', ( #7418, #41672, #13119, #968 ) ) ;
#10895 = EDGE_LOOP ( 'NONE', ( #20438, #1094, #5789, #22578, #17697 ) ) ;
#10896 = CARTESIAN_POINT ( 'NONE',  ( 0.8387602819694093270, -80.41695080943928531, 0.9265839650083794732 ) ) ;
#10897 = CARTESIAN_POINT ( 'NONE',  ( -9.522203062526999773, -77.13453998579799986, -0.6231167251167999410 ) ) ;
#10898 = CARTESIAN_POINT ( 'NONE',  ( -5.809791519574999619, -79.55585413501300707, 7.851562197947999699 ) ) ;
#10899 = VERTEX_POINT ( 'NONE', #43522 ) ;
#10900 = CARTESIAN_POINT ( 'NONE',  ( 12.66235371494999917, -53.66260492101000068, 0.4957155363043999619 ) ) ;
#10901 = CARTESIAN_POINT ( 'NONE',  ( 8.414343270883998471, -78.37837685893698847, 6.955155862361000807 ) ) ;
#10902 = EDGE_LOOP ( 'NONE', ( #3453, #12548, #34200, #29026 ) ) ;
#10903 = CARTESIAN_POINT ( 'NONE',  ( -12.66315196848000113, -25.17802884708999756, 0.06065366946595000114 ) ) ;
#10904 = CARTESIAN_POINT ( 'NONE',  ( -0.03204405817075929586, -78.69999999999998863, -3.399848993460456548 ) ) ;
#10905 = ADVANCED_FACE ( 'NONE', ( #6923 ), #56235, .T. ) ;
#10906 = CARTESIAN_POINT ( 'NONE',  ( 9.549999999999998934, -80.99999999999998579, 0.000000000000000000 ) ) ;
#10907 = CARTESIAN_POINT ( 'NONE',  ( 3.325701842495000005, -82.39999999999999147, -0.7068997487804000723 ) ) ;
#10908 = CARTESIAN_POINT ( 'NONE',  ( -4.099999999699000419, -75.20000000030088927, 8.298667500436000154E-10 ) ) ;
#10909 = PLANE ( 'NONE',  #26862 ) ;
#10910 = CARTESIAN_POINT ( 'NONE',  ( 2.968094753861000079, -77.12165489554539022, 9.474519209979000323 ) ) ;
#10911 = CARTESIAN_POINT ( 'NONE',  ( 0.2177847895985361160, -79.21305384291285634, 1.494441264229401378 ) ) ;
#10912 = CARTESIAN_POINT ( 'NONE',  ( 2.868529044229433111, -82.26510418536243208, -2.805596100957504557 ) ) ;
#10913 = CARTESIAN_POINT ( 'NONE',  ( -10.62397638184999948, -76.02480637415999354, -6.218250916117999516 ) ) ;
#10914 = CARTESIAN_POINT ( 'NONE',  ( -0.5999999999999999778, -23.15000000000000213, 11.79999999999999893 ) ) ;
#10915 = CARTESIAN_POINT ( 'NONE',  ( 9.523353692561999040, -61.61947015589999666, -8.220363114712000652 ) ) ;
#10916 = CARTESIAN_POINT ( 'NONE',  ( 11.81418954875000082, -78.75427961895999829, 3.289986436736999753 ) ) ;
#10917 = CARTESIAN_POINT ( 'NONE',  ( 10.16964605767000052, -76.33653603642800078, -6.884832982024000181 ) ) ;
#10918 = FACE_BOUND ( 'NONE', #38320, .T. ) ;
#10919 = CARTESIAN_POINT ( 'NONE',  ( 3.134197176858777301, -2.830045019308922605, -0.8619150459417437293 ) ) ;
#10920 = CARTESIAN_POINT ( 'NONE',  ( -11.51192706679896816, -78.07429133446665048, -3.621052222003904308 ) ) ;
#10921 = FACE_OUTER_BOUND ( 'NONE', #48985, .T. ) ;
#10922 = AXIS2_PLACEMENT_3D ( 'NONE', #38067, #11508, #56088 ) ;
#10923 = ORIENTED_EDGE ( 'NONE', *, *, #20680, .T. ) ;
#10925 = EDGE_CURVE ( 'NONE', #35206, #45023, #34349, .T. ) ;
#10924 = DIRECTION ( 'NONE',  ( 1.000000000000000000, 0.000000000000000000, 0.000000000000000000 ) ) ;
#10926 = DIRECTION ( 'NONE',  ( -2.273758747900730032E-11, -6.364523519691810633E-20, 1.000000000000000000 ) ) ;
#10927 = DIRECTION ( 'NONE',  ( -2.678934596778999979E-11, 1.000000000000000000, 2.678911359553000079E-11 ) ) ;
#10928 = CARTESIAN_POINT ( 'NONE',  ( -1.250000000000000000, -82.99999999999998579, 0.000000000000000000 ) ) ;
#10929 = CARTESIAN_POINT ( 'NONE',  ( -0.3056021915128999678, -2.413088905188999878, -3.858359142670999997 ) ) ;
#10930 = CARTESIAN_POINT ( 'NONE',  ( -10.42801618316999956, -78.39809032934199706, 6.264104809848999977 ) ) ;
#10931 = CARTESIAN_POINT ( 'NONE',  ( -2.191084135724000070, -77.66387044253798422, 9.489933931099999498 ) ) ;
#10933 = CARTESIAN_POINT ( 'NONE',  ( -11.00000000000000000, -77.69999999999998863, 0.000000000000000000 ) ) ;
#10932 = CARTESIAN_POINT ( 'NONE',  ( -10.84377968468480979, -76.16840065501064316, 4.524662071590493717 ) ) ;
#10934 = CARTESIAN_POINT ( 'NONE',  ( 1.281517705925000028, -81.85570787394000547, 0.4285832374949000156 ) ) ;
#10935 = CARTESIAN_POINT ( 'NONE',  ( -7.686941364959000822, -21.75472017805000036, 10.48774103561000182 ) ) ;
#10936 = ORIENTED_EDGE ( 'NONE', *, *, #36282, .F. ) ;
#10937 = CARTESIAN_POINT ( 'NONE',  ( -12.22985280536000019, -76.55908522753409784, -1.402219185754999486 ) ) ;
#10938 = CARTESIAN_POINT ( 'NONE',  ( 11.85356139282347954, -79.10427114674126869, -1.243530160672429163 ) ) ;
#10939 = EDGE_CURVE ( 'NONE', #15494, #4925, #2575, .T. ) ;
#10940 = CARTESIAN_POINT ( 'NONE',  ( -0.8506806241676722058, -2.395833333333332149, 3.165411199172022627 ) ) ;
#10941 = CARTESIAN_POINT ( 'NONE',  ( -7.636246406707999590, -60.56323123069000047, 10.30460653227000023 ) ) ;
#10942 = EDGE_CURVE ( 'NONE', #19958, #15969, #12176, .T. ) ;
#10943 = CARTESIAN_POINT ( 'NONE',  ( -10.91764451743335762, -80.09049157782284567, 1.351593570394689081 ) ) ;
#10944 = CARTESIAN_POINT ( 'NONE',  ( 9.669905736194998269, -79.39378745527798742, 0.08814083877134999689 ) ) ;
#10945 = CARTESIAN_POINT ( 'NONE',  ( 10.00831378477999856, -18.62769332291999902, -7.646786280044999273 ) ) ;
#10946 = CARTESIAN_POINT ( 'NONE',  ( 12.51072239526000196, -52.49705297114005020, 0.7871079366006996647 ) ) ;
#10947 = CARTESIAN_POINT ( 'NONE',  ( 3.385018580295000135, -79.42588468523199197, -10.74130410002999980 ) ) ;
#10948 = DIRECTION ( 'NONE',  ( 1.000000000000000000, 0.000000000000000000, 0.000000000000000000 ) ) ;
#10949 = CARTESIAN_POINT ( 'NONE',  ( -11.71599595481501765, -79.05733145785083593, -1.136090037544484233 ) ) ;
#10950 = CARTESIAN_POINT ( 'NONE',  ( -0.03239434199580018547, -78.54828564506388489, 3.437034971988155441 ) ) ;
#10951 = CARTESIAN_POINT ( 'NONE',  ( 10.30793518295451960, -77.74603760418852971, 6.185760751847420913 ) ) ;
#10953 = CARTESIAN_POINT ( 'NONE',  ( 0.8649096616148368444, -81.41463932042252338, 0.9021248153222395372 ) ) ;
#10952 = CARTESIAN_POINT ( 'NONE',  ( 0.6157886138241999152, -81.82170153995799922, -1.166777612888000082 ) ) ;
#10954 = CARTESIAN_POINT ( 'NONE',  ( -0.2497519934274041176, -78.54048298376281423, 1.249453341561128195 ) ) ;
#10955 = DIRECTION ( 'NONE',  ( 0.000000000000000000, 1.000000000000000000, 0.000000000000000000 ) ) ;
#10956 = CARTESIAN_POINT ( 'NONE',  ( 3.325193802675403543, -82.33721875853790095, -0.7067914353816346917 ) ) ;
#10957 = PRODUCT_DEFINITION ( 'UNKNOWN', '', #4669, #26258 ) ;
#10958 = CARTESIAN_POINT ( 'NONE',  ( -1.108895999262000220, -78.12450665301999209, -0.6936369237491999407 ) ) ;
#10959 = CARTESIAN_POINT ( 'NONE',  ( -12.60413652829999975, -55.49283065365000311, 1.799502287743000029 ) ) ;
#10960 = CARTESIAN_POINT ( 'NONE',  ( 10.80348683896752959, -79.46729337777097157, 2.390241153868424284 ) ) ;
#10961 = CARTESIAN_POINT ( 'NONE',  ( 12.70299804973600466, -53.77411689947622619, -0.8844418155219602173 ) ) ;
#10962 = ORIENTED_EDGE ( 'NONE', *, *, #54374, .F. ) ;
#10963 = ORIENTED_EDGE ( 'NONE', *, *, #54936, .T. ) ;
#10964 = CARTESIAN_POINT ( 'NONE',  ( -3.442307367123000450, -78.28223998579800025, 9.412654989800000038 ) ) ;
#10965 = CARTESIAN_POINT ( 'NONE',  ( 5.261237598753935707, -78.76578525366345218, -9.374798830089835278 ) ) ;
#10966 = VERTEX_POINT ( 'NONE', #56811 ) ;
#10967 = CARTESIAN_POINT ( 'NONE',  ( 8.260145278149000347, -17.05964900975000020, 9.643338479001000607 ) ) ;
#10968 = AXIS2_PLACEMENT_3D ( 'NONE', #36544, #5254, #17661 ) ;
#10969 = EDGE_CURVE ( 'NONE', #29213, #12675, #27247, .T. ) ;
#10970 = CARTESIAN_POINT ( 'NONE',  ( -11.75000000000000000, -75.80000000000001137, -9.948686767780999254E-14 ) ) ;
#10971 = AXIS2_PLACEMENT_3D ( 'NONE', #15070, #42246, #10075 ) ;
#10972 = CARTESIAN_POINT ( 'NONE',  ( 9.726612558640999495, -78.63181324549999829, 7.133059342380000167 ) ) ;
#10973 = AXIS2_PLACEMENT_3D ( 'NONE', #3656, #12794, #49416 ) ;
#10974 = EDGE_CURVE ( 'NONE', #31953, #19148, #25390, .T. ) ;
#10975 = CARTESIAN_POINT ( 'NONE',  ( -10.47031859815319343, -79.62086369140376974, -2.813909006929614431 ) ) ;
#10976 = CARTESIAN_POINT ( 'NONE',  ( -12.00000000000000000, -23.15000000000000213, 0.5999999999999999778 ) ) ;
#10977 = CARTESIAN_POINT ( 'NONE',  ( -1.460959015002474937, -79.97916666666665719, 0.3926218265389144757 ) ) ;
#10978 = CARTESIAN_POINT ( 'NONE',  ( 10.63562707217000103, -80.17741280756860078, 3.563914325689000240 ) ) ;
#10979 = ORIENTED_EDGE ( 'NONE', *, *, #6666, .T. ) ;
#10980 = LINE ( 'NONE', #42554, #6746 ) ;
#10981 = VERTEX_POINT ( 'NONE', #29633 ) ;
#10982 = CARTESIAN_POINT ( 'NONE',  ( 8.238405875913969112, -77.38767930335906442, 4.205914151111458388 ) ) ;
#10983 = DIRECTION ( 'NONE',  ( 0.9903465037206092836, -0.1386138613861012392, 0.000000000000000000 ) ) ;
#10984 = CARTESIAN_POINT ( 'NONE',  ( 6.433884635080341141, -77.52351991347129001, -9.188402334806731631 ) ) ;
#10985 = CARTESIAN_POINT ( 'NONE',  ( -1.431457626485999945, -78.45366409087199600, 0.7470896798747000966 ) ) ;
#10986 = CARTESIAN_POINT ( 'NONE',  ( 3.140974612311376646, -77.54583333333334849, -11.68767212001978706 ) ) ;
#10987 = DIRECTION ( 'NONE',  ( -0.7071067811865475727, 0.000000000000000000, 0.7071067811865475727 ) ) ;
#10988 = CARTESIAN_POINT ( 'NONE',  ( 1.619712389308999967, -79.14659814888999279, 0.1587296492880999887 ) ) ;
#10989 = CARTESIAN_POINT ( 'NONE',  ( -9.878709405926999310, -79.03001782088199434, -4.948635581693999974 ) ) ;
#10990 = SURFACE_STYLE_USAGE ( .BOTH. , #33689 ) ;
#10991 = CARTESIAN_POINT ( 'NONE',  ( -7.342377162852876005, -60.03019609282243607, 8.190817883596773541 ) ) ;
#10992 = CARTESIAN_POINT ( 'NONE',  ( 3.133030782380000101, -82.57905554179599505, 1.663082909639999940 ) ) ;
#10993 = EDGE_LOOP ( 'NONE', ( #12308, #23727, #28422 ) ) ;
#10994 = CARTESIAN_POINT ( 'NONE',  ( -10.16722439191025629, -77.19999999999998863, 4.064972966511320784 ) ) ;
#10995 = CARTESIAN_POINT ( 'NONE',  ( -1.418768848999000021, -79.78339211834999389, 0.9417588900106000915 ) ) ;
#10996 = CARTESIAN_POINT ( 'NONE',  ( -0.03076778114328541577, -77.97532005365077623, 10.74994462762427716 ) ) ;
#10997 = CARTESIAN_POINT ( 'NONE',  ( 9.148490208346998998, -77.93974456801599615, 7.734416031130999514 ) ) ;
#10998 = CARTESIAN_POINT ( 'NONE',  ( -9.102137319215390932, -53.82814024814979348, 8.583672456483473212 ) ) ;
#10999 = CARTESIAN_POINT ( 'NONE',  ( 10.68072966837468130, -78.86055855974642270, 1.407246846443371613 ) ) ;
#11000 = CARTESIAN_POINT ( 'NONE',  ( 0.3283580454435180429, -3.382392793792461383, -3.504945231587735410 ) ) ;
#11001 = CARTESIAN_POINT ( 'NONE',  ( 8.172550279481720636, -80.90660285001109742, 6.983378171755568076 ) ) ;
#11002 = CARTESIAN_POINT ( 'NONE',  ( 9.085337660295000006, -78.41725766396999120, 2.850792140868000146 ) ) ;
#11003 = ADVANCED_BREP_SHAPE_REPRESENTATION ( '', ( #36141, #43526 ), #23620 ) ;
#11004 = CARTESIAN_POINT ( 'NONE',  ( 2.061613410425999771, -55.59429985491999560, -12.83797036852999796 ) ) ;
#11005 = CARTESIAN_POINT ( 'NONE',  ( 0.5383385070467999745, -77.08774834149699018, -11.01870799087000030 ) ) ;
#11006 = CARTESIAN_POINT ( 'NONE',  ( 3.343750000583999960, -0.9062499994161000716, -3.925818329445000231E-08 ) ) ;
#11007 = CARTESIAN_POINT ( 'NONE',  ( 1.570796326794909881, -78.43541666666668277, -11.99999999999999822 ) ) ;
#11008 = CARTESIAN_POINT ( 'NONE',  ( 0.9388019354105423542, -81.95930158213857908, 0.8620481451250026073 ) ) ;
#11009 = EDGE_LOOP ( 'NONE', ( #34006, #2112, #32056, #28151 ) ) ;
#11010 = CARTESIAN_POINT ( 'NONE',  ( 1.193978368322000216, -81.93514364053599763, -0.5941311122250999555 ) ) ;
#11011 = CARTESIAN_POINT ( 'NONE',  ( 1.761265949705000056, -60.50858218752999562, -12.57448205046000034 ) ) ;
#11012 = DIRECTION ( 'NONE',  ( 0.000000000000000000, 0.7071067811866525998, -0.7071067811864425456 ) ) ;
#11013 = EDGE_CURVE ( 'NONE', #34724, #35383, #20682, .T. ) ;
#11014 = CARTESIAN_POINT ( 'NONE',  ( 7.508079800428999917, -76.94946321865599259, -8.333477563431999968 ) ) ;
#11015 = CARTESIAN_POINT ( 'NONE',  ( 10.94409238582999855, -78.56557775944099831, 0.8311789410725000105 ) ) ;
#11016 = CARTESIAN_POINT ( 'NONE',  ( 8.194866293440998817, -24.71043252651000088, -9.389192598794000588 ) ) ;
#11017 = EDGE_CURVE ( 'NONE', #7313, #51480, #58395, .T. ) ;
#11018 = CARTESIAN_POINT ( 'NONE',  ( 3.723742114431606520, -85.54114584694690393, 1.494555256775147889 ) ) ;
#11019 = CARTESIAN_POINT ( 'NONE',  ( 12.07337922597999835, -76.31749961810498917, -1.385301795592000174 ) ) ;
#11020 = DIRECTION ( 'NONE',  ( -0.7071067811865475727, 0.000000000000000000, 0.7071067811865475727 ) ) ;
#11021 = CARTESIAN_POINT ( 'NONE',  ( -1.250000000000000000, -80.09999999999999432, 0.000000000000000000 ) ) ;
#11022 = ORIENTED_EDGE ( 'NONE', *, *, #28354, .F. ) ;
#11023 = CIRCLE ( 'NONE', #32673, 1.199999999999999956 ) ;
#11024 = CARTESIAN_POINT ( 'NONE',  ( -0.4796072403373097814, -80.00656463011694086, 1.154180156579423189 ) ) ;
#11025 = CARTESIAN_POINT ( 'NONE',  ( 12.09999999997999964, -92.79999999999999716, 2.688172647412999614E-10 ) ) ;
#11026 = VECTOR ( 'NONE', #21522, 1000.000000000000000 ) ;
#11027 = CARTESIAN_POINT ( 'NONE',  ( 7.645391692591000599, -55.58469634128999814, -10.18949678826999872 ) ) ;
#11028 = AXIS2_PLACEMENT_3D ( 'NONE', #51518, #46225, #41478 ) ;
#11029 = CARTESIAN_POINT ( 'NONE',  ( -7.707335466132000157, -78.74423443443198778, -8.217415310065000256 ) ) ;
#11030 = CARTESIAN_POINT ( 'NONE',  ( -1.194132053304999941, -79.05502241712000000, -0.5627846202731000558 ) ) ;
#11031 = CARTESIAN_POINT ( 'NONE',  ( 7.919595949288999570, -59.94999999969000015, 8.768124086712999699 ) ) ;
#11032 = CARTESIAN_POINT ( 'NONE',  ( 0.6447284801462368486, -81.59004626953988293, 1.368070997584296844 ) ) ;
#11033 = VECTOR ( 'NONE', #35613, 1000.000000000000000 ) ;
#11034 = CARTESIAN_POINT ( 'NONE',  ( -7.954951288349001004, -55.54999999966999980, 9.722718241315000398 ) ) ;
#11035 = CARTESIAN_POINT ( 'NONE',  ( -0.8005651750373993236, -79.66990695520425447, -0.9602051216220701679 ) ) ;
#11036 = EDGE_CURVE ( 'NONE', #50169, #40498, #48255, .T. ) ;
#11037 = CARTESIAN_POINT ( 'NONE',  ( -9.346058022005980348, -53.63471832377268100, 8.620905970535309493 ) ) ;
#11038 = VERTEX_POINT ( 'NONE', #25792 ) ;
#11039 = CARTESIAN_POINT ( 'NONE',  ( -0.09604542572962751490, -81.71951835724753721, -1.248441681024932803 ) ) ;
#11040 = FILL_AREA_STYLE ('',( #51482 ) ) ;
#11041 = CARTESIAN_POINT ( 'NONE',  ( -8.235122208958999934, -78.83228563835899649, 7.512480467459000444 ) ) ;
#11042 = CARTESIAN_POINT ( 'NONE',  ( 0.000000000000000000, -76.30000000005068728, 0.000000000000000000 ) ) ;
#11043 = EDGE_LOOP ( 'NONE', ( #39927, #16626, #6127, #11751 ) ) ;
#11044 = VERTEX_POINT ( 'NONE', #2790 ) ;
#11045 = CARTESIAN_POINT ( 'NONE',  ( -1.311997437969999902, -81.07175312489499674, 0.5373286780417999564 ) ) ;
#11046 = EDGE_LOOP ( 'NONE', ( #26393, #25447, #26248, #12015, #43966 ) ) ;
#11047 = CARTESIAN_POINT ( 'NONE',  ( 8.974834626914359959, -79.97252914747060970, -3.225705101019638033 ) ) ;
#11048 = VERTEX_POINT ( 'NONE', #43820 ) ;
#11049 = CARTESIAN_POINT ( 'NONE',  ( 1.930638663166000191, -18.77877936711000117, 12.72375916873000001 ) ) ;
#11050 = CARTESIAN_POINT ( 'NONE',  ( -9.713030931734584428, -54.27705886621604492, -7.970419577022142654 ) ) ;
#11051 = DIRECTION ( 'NONE',  ( 0.000000000000000000, 0.000000000000000000, 1.000000000000000000 ) ) ;
#11052 = CARTESIAN_POINT ( 'NONE',  ( -7.634645133894798263, -60.27584427251471055, 10.10912661257252410 ) ) ;
#11053 = EDGE_CURVE ( 'NONE', #34958, #26247, #57383, .T. ) ;
#11054 = CARTESIAN_POINT ( 'NONE',  ( 3.541417221457102915, -78.25630717469576325, -8.545189235367685043 ) ) ;
#11055 = CARTESIAN_POINT ( 'NONE',  ( -8.982117338527000783, -79.64721103171800110, 6.718606902359000266 ) ) ;
#11056 = ORIENTED_EDGE ( 'NONE', *, *, #23435, .F. ) ;
#11057 = VERTEX_POINT ( 'NONE', #48532 ) ;
#11058 = CARTESIAN_POINT ( 'NONE',  ( -8.823116529173212541, -77.57575035185114132, 2.777645208995981996 ) ) ;
#11059 = FACE_OUTER_BOUND ( 'NONE', #52762, .T. ) ;
#11060 = CIRCLE ( 'NONE', #25192, 13.86363636363999952 ) ;
#11061 = DIRECTION ( 'NONE',  ( 0.000000000000000000, -1.000000000000000000, 0.000000000000000000 ) ) ;
#11062 = CARTESIAN_POINT ( 'NONE',  ( 6.240531904507999883, -78.08926280546299381, 7.431451467605000083 ) ) ;
#11063 = FACE_OUTER_BOUND ( 'NONE', #8386, .T. ) ;
#11064 = CARTESIAN_POINT ( 'NONE',  ( 1.750000000001000089, -22.75077028492999887, 12.60356226393999890 ) ) ;
#11065 = VECTOR ( 'NONE', #32378, 1000.000000000000000 ) ;
#11066 = CARTESIAN_POINT ( 'NONE',  ( -1.500000000000000000, -80.50000000000000000, 0.000000000000000000 ) ) ;
#11067 = CARTESIAN_POINT ( 'NONE',  ( -1.639384890095999969, -80.29177512065000144, -0.4606887641594999971 ) ) ;
#11068 = AXIS2_PLACEMENT_3D ( 'NONE', #27576, #5159, #23160 ) ;
#11069 = CARTESIAN_POINT ( 'NONE',  ( 3.837589733631999955, -82.33492937544698975, -1.636764466176000132 ) ) ;
#11070 = AXIS2_PLACEMENT_3D ( 'NONE', #55942, #15492, #37917 ) ;
#11071 = CARTESIAN_POINT ( 'NONE',  ( -10.53559655342999868, -55.59430957992999822, 7.620036381585000740 ) ) ;
#11072 = CARTESIAN_POINT ( 'NONE',  ( 1.936520525790000002, -78.30246332859900349, 9.719586767747999900 ) ) ;
#11073 = CARTESIAN_POINT ( 'NONE',  ( -12.00000000000000000, -77.39999999999999147, 0.000000000000000000 ) ) ;
#11074 = CARTESIAN_POINT ( 'NONE',  ( 2.062673488410000200, -18.67547726287999765, -12.82904109062999964 ) ) ;
#11076 = CARTESIAN_POINT ( 'NONE',  ( 1.691611010928000036, -17.76917308770000048, -12.66722148969999928 ) ) ;
#11075 = CARTESIAN_POINT ( 'NONE',  ( 0.7554284705563452107, -78.73333333333332007, 1.310679582531388609 ) ) ;
#11077 = FACE_OUTER_BOUND ( 'NONE', #18584, .T. ) ;
#11078 = CYLINDRICAL_SURFACE ( 'NONE', #17514, 9.500000000000000000 ) ;
#11079 = DIRECTION ( 'NONE',  ( 0.000000000000000000, -1.000000000000000000, 0.000000000000000000 ) ) ;
#11080 = CARTESIAN_POINT ( 'NONE',  ( 0.000000000000000000, -86.20000000000000284, 0.000000000000000000 ) ) ;
#11081 = CARTESIAN_POINT ( 'NONE',  ( -2.949966724422874886, -1.203753930650452109, 1.940841882792249118 ) ) ;
#11082 = ORIENTED_EDGE ( 'NONE', *, *, #54019, .T. ) ;
#11083 = CARTESIAN_POINT ( 'NONE',  ( 8.782705133632456196, -78.99166666666667425, -7.901937437512484230 ) ) ;
#11084 = FACE_OUTER_BOUND ( 'NONE', #8535, .T. ) ;
#11085 = FACE_OUTER_BOUND ( 'NONE', #37877, .T. ) ;
#11086 = CARTESIAN_POINT ( 'NONE',  ( -0.0002385852177439338659, -78.47523597995287048, 1.249867994843831376 ) ) ;
#11087 = CARTESIAN_POINT ( 'NONE',  ( -5.134431902050000218, -79.97337732914698449, -8.161852231781001166 ) ) ;
#11088 = CARTESIAN_POINT ( 'NONE',  ( 11.82764905900999963, -77.23222945497001035, 5.426413045081000419 ) ) ;
#11089 = CARTESIAN_POINT ( 'NONE',  ( -9.700000000000001066, -87.20000000000000284, 0.000000000000000000 ) ) ;
#11090 = CARTESIAN_POINT ( 'NONE',  ( 7.511969992774096383, -79.41342506424436465, 7.689912663504889778 ) ) ;
#11091 = CARTESIAN_POINT ( 'NONE',  ( -6.277755163971999508, -79.30933998579799038, 7.588502419953999656 ) ) ;
#11092 = CARTESIAN_POINT ( 'NONE',  ( 0.000000000000000000, 4.040000000000000036, 0.000000000000000000 ) ) ;
#11093 = CARTESIAN_POINT ( 'NONE',  ( 2.932810412914000242, -77.51739520116099413, -10.54767017414000208 ) ) ;
#11094 = B_SPLINE_CURVE_WITH_KNOTS ( 'NONE', 3,
 ( #54445, #35828, #53556, #13981, #54146, #35230, #44123, #3672, #22554, #13686, #21673, #31683, #3953, #39678, #53260, #44701, #57685, #26966 ),
 .UNSPECIFIED., .F., .F.,
 ( 4, 2, 2, 2, 2, 2, 2, 2, 4 ),
 ( 0.000000000000000000, 0.1250000000000000000, 0.2499999999999999722, 0.3750000000000000000, 0.5000000000000000000, 0.6250000000000000000, 0.7500000000000000000, 0.8750000000000000000, 1.000000000000000000 ),
 .UNSPECIFIED. ) ;
#11095 = CARTESIAN_POINT ( 'NONE',  ( 1.602797262804000145, -82.15484732184999928, -0.06469291290319000021 ) ) ;
#11096 = CARTESIAN_POINT ( 'NONE',  ( -9.601739433208001273, -79.16259514476064396, -1.533141744029000053 ) ) ;
#11097 = CARTESIAN_POINT ( 'NONE',  ( 7.993200843029001135, -78.22653256295699009, -4.971914600080000746 ) ) ;
#11099 = CARTESIAN_POINT ( 'NONE',  ( 7.850068286652203575, -54.48530314306970013, 9.837745659570314771 ) ) ;
#11098 = CARTESIAN_POINT ( 'NONE',  ( -3.696851366990000276, -82.98328762115399115, -1.428033570587000201 ) ) ;
#11100 = CARTESIAN_POINT ( 'NONE',  ( 2.769824414688999870, -79.33935584965399812, -8.825563591736999669 ) ) ;
#11101 = CARTESIAN_POINT ( 'NONE',  ( 1.250000000000000000, -82.74999999999998579, 0.000000000000000000 ) ) ;
#11102 = CARTESIAN_POINT ( 'NONE',  ( 8.658023998471257698, -80.29953180223905918, -6.377467274757659510 ) ) ;
#11103 = CARTESIAN_POINT ( 'NONE',  ( -6.959349728372989041, -77.16901490944738384, -8.193258774412282008 ) ) ;
#11104 = CARTESIAN_POINT ( 'NONE',  ( -4.784380313523575623, -77.31666666666666288, 8.300970689365433586 ) ) ;
#11105 = EDGE_CURVE ( 'NONE', #26696, #6154, #38213, .T. ) ;
#11106 = ORIENTED_EDGE ( 'NONE', *, *, #1459, .T. ) ;
#11107 = CARTESIAN_POINT ( 'NONE',  ( 7.520016693046000178, -79.74484475749498813, -9.389162645085001202 ) ) ;
#11108 = CARTESIAN_POINT ( 'NONE',  ( 8.838834764832000701, -55.54999999966999980, 8.838834764832000701 ) ) ;
#11109 = DIRECTION ( 'NONE',  ( 0.000000000000000000, 0.000000000000000000, -1.000000000000000000 ) ) ;
#11110 = CIRCLE ( 'NONE', #38438, 10.50000000000000000 ) ;
#11111 = ORIENTED_EDGE ( 'NONE', *, *, #55225, .F. ) ;
#11112 = DIRECTION ( 'NONE',  ( 0.000000000000000000, 1.000000000000000000, 0.000000000000000000 ) ) ;
#11113 = VERTEX_POINT ( 'NONE', #29347 ) ;
#11114 = ORIENTED_EDGE ( 'NONE', *, *, #53159, .F. ) ;
#11115 = CIRCLE ( 'NONE', #4479, 0.5000000000000000000 ) ;
#11116 = B_SPLINE_CURVE_WITH_KNOTS ( 'NONE', 3,
 ( #21395, #39979, #30819, #57992, #49741, #36142 ),
 .UNSPECIFIED., .F., .F.,
 ( 4, 2, 4 ),
 ( 0.000000000000000000, 0.5000000000000000000, 1.000000000000000000 ),
 .UNSPECIFIED. ) ;
#11117 = CARTESIAN_POINT ( 'NONE',  ( -10.26699006316252749, -77.34166666666665435, -5.917523019358070790 ) ) ;
#11118 = EDGE_CURVE ( 'NONE', #52418, #7381, #47392, .T. ) ;
#11119 = CARTESIAN_POINT ( 'NONE',  ( -1.757514242320000086, -79.92992088582298038, 3.081509990535999943 ) ) ;
#11120 = CARTESIAN_POINT ( 'NONE',  ( 9.040019095898385260, -79.17444713763063646, 2.919477139292010914 ) ) ;
#11121 = ORIENTED_EDGE ( 'NONE', *, *, #51244, .F. ) ;
#11122 = CARTESIAN_POINT ( 'NONE',  ( -10.42531124908000173, -60.06485148440999922, -7.624341765471999821 ) ) ;
#11123 = ORIENTED_EDGE ( 'NONE', *, *, #51904, .T. ) ;
#11124 = DIRECTION ( 'NONE',  ( 1.000000000000000000, 0.000000000000000000, 0.000000000000000000 ) ) ;
#11125 = ORIENTED_EDGE ( 'NONE', *, *, #43215, .F. ) ;
#11126 = CARTESIAN_POINT ( 'NONE',  ( 1.733997378023100833, -18.47616783230471071, 12.54437956612015981 ) ) ;
#11127 = CARTESIAN_POINT ( 'NONE',  ( -0.06629182480466444538, -78.37178464163872604, -1.530081213047539634 ) ) ;
#11128 = CARTESIAN_POINT ( 'NONE',  ( 11.66152884693005731, -79.80000000000001137, 1.849687133078396606 ) ) ;
#11129 = CARTESIAN_POINT ( 'NONE',  ( -12.50385602495247639, -17.21562718850158902, 0.8579628946858919303 ) ) ;
#11130 = CARTESIAN_POINT ( 'NONE',  ( 10.75000000000000000, -78.35000000000000853, 1.923335087985999915E-14 ) ) ;
#11131 = CARTESIAN_POINT ( 'NONE',  ( 8.444976262095000408, -78.04099091448563286, 4.780490068936999570 ) ) ;
#11133 = EDGE_CURVE ( 'NONE', #56405, #27707, #47985, .T. ) ;
#11132 = CARTESIAN_POINT ( 'NONE',  ( -10.67244467921999984, -76.81272073173599324, 2.904229794498999873 ) ) ;
#11134 = CARTESIAN_POINT ( 'NONE',  ( -6.551127804292855572, -76.52735550355730254, 8.658837545241746980 ) ) ;
#11135 = CYLINDRICAL_SURFACE ( 'NONE', #12749, 9.199999999999999289 ) ;
#11136 = EDGE_CURVE ( 'NONE', #3351, #56911, #53532, .T. ) ;
#11137 = CARTESIAN_POINT ( 'NONE',  ( -5.246643863826999876, -76.47701249839499837, -9.797568585289999632 ) ) ;
#11138 = CARTESIAN_POINT ( 'NONE',  ( -2.993561518543238709, -78.69892983886539639, -8.753304730231880271 ) ) ;
#11139 = CARTESIAN_POINT ( 'NONE',  ( 8.595597484336256144, -76.50923340009842377, 8.012250707705186770 ) ) ;
#11140 = CARTESIAN_POINT ( 'NONE',  ( -4.802278608554999551, -77.58981167140099444, -8.220090885098999323 ) ) ;
#11141 = CARTESIAN_POINT ( 'NONE',  ( 0.5173218454072999739, -79.52141276759999755, 1.229208833401000067 ) ) ;
#11142 = CARTESIAN_POINT ( 'NONE',  ( -10.89273321435514497, -80.11128739981552371, -1.531847966823179918 ) ) ;
#11143 = CARTESIAN_POINT ( 'NONE',  ( -12.60354432329999952, -59.55100837068999908, -1.750000000001000089 ) ) ;
#11144 = CARTESIAN_POINT ( 'NONE',  ( -2.147119888857000003, -80.12503455456798918, -3.082407869100999953 ) ) ;
#11145 = CARTESIAN_POINT ( 'NONE',  ( 10.89405075708000048, -79.72170167379699990, -5.492612443427000279 ) ) ;
#11146 = CARTESIAN_POINT ( 'NONE',  ( -10.54835816730423304, -78.08464500269199959, 2.072073882157521307 ) ) ;
#11147 = CARTESIAN_POINT ( 'NONE',  ( 0.1634127036930090315, -82.96491418332730916, 1.239110987847197531 ) ) ;
#11148 = FACE_OUTER_BOUND ( 'NONE', #48847, .T. ) ;
#11149 = CARTESIAN_POINT ( 'NONE',  ( -3.992904449609000483, -78.77851881763731967, -1.675407828963362518E-14 ) ) ;
#11150 = CARTESIAN_POINT ( 'NONE',  ( -1.250000000000000000, -80.49999999999998579, 0.000000000000000000 ) ) ;
#11151 = CARTESIAN_POINT ( 'NONE',  ( 12.00000000000000000, -79.16041666666664867, 1.570796326794922093 ) ) ;
#11152 = CARTESIAN_POINT ( 'NONE',  ( -10.31444895690999886, -61.10075144983999706, -7.758883253367000243 ) ) ;
#11153 = CARTESIAN_POINT ( 'NONE',  ( -1.310615285706999922, -81.64914511185500601, -0.2467057407436999972 ) ) ;
#11154 = CARTESIAN_POINT ( 'NONE',  ( 0.1963495408493637351, -80.53541666666667709, -1.499999999999999778 ) ) ;
#11155 = CARTESIAN_POINT ( 'NONE',  ( 12.66316452095000145, -25.17866137669000182, -0.04044945982121000289 ) ) ;
#11156 = ADVANCED_FACE ( 'NONE', ( #35803 ), #36697, .T. ) ;
#11157 = CARTESIAN_POINT ( 'NONE',  ( -2.444356268457450909, -77.55728255341558963, -10.55741984921857046 ) ) ;
#11158 = CARTESIAN_POINT ( 'NONE',  ( -1.538085309883418406, -78.31279427438737173, -11.67755942590387797 ) ) ;
#11159 = CONICAL_SURFACE ( 'NONE', #40373, 10.59999999997999787, 0.7853981633972997312 ) ;
#11160 = CARTESIAN_POINT ( 'NONE',  ( 6.612939829087000732, -79.67354116428806776, 8.759739992124000452 ) ) ;
#11161 = FACE_OUTER_BOUND ( 'NONE', #52999, .T. ) ;
#11162 = EDGE_LOOP ( 'NONE', ( #7867, #9496, #47853 ) ) ;
#11163 = CARTESIAN_POINT ( 'NONE',  ( 3.962534114458999834, -82.75096544543198718, -0.06234403170014000267 ) ) ;
#11164 = DIRECTION ( 'NONE',  ( 0.000000000000000000, -1.000000000000000000, 0.000000000000000000 ) ) ;
#11165 = CARTESIAN_POINT ( 'NONE',  ( 9.152874836537630898, -78.33854092996706697, -1.339099148577004739 ) ) ;
#11166 = CARTESIAN_POINT ( 'NONE',  ( 0.000000000000000000, -76.75499999999999545, 0.000000000000000000 ) ) ;
#11167 = CARTESIAN_POINT ( 'NONE',  ( -10.58728162385000005, -77.87489427226098826, 3.705074683290000337 ) ) ;
#11168 = CARTESIAN_POINT ( 'NONE',  ( 12.66761570926000147, -54.57632520071999949, -1.696752301450999978 ) ) ;
#11169 = CARTESIAN_POINT ( 'NONE',  ( 8.475813183550998886, -78.12017682799398699, 4.797946079729999092 ) ) ;
#11170 = CARTESIAN_POINT ( 'NONE',  ( 0.6062141276560999437, -82.54346268355999428, -1.551696954864999922 ) ) ;
#11171 = LINE ( 'NONE', #20305, #40666 ) ;
#11172 = CARTESIAN_POINT ( 'NONE',  ( 1.602460118848999970, -79.73214323184600971, -0.1983317763271000012 ) ) ;
#11173 = ORIENTED_EDGE ( 'NONE', *, *, #17233, .T. ) ;
#11174 = DIRECTION ( 'NONE',  ( 4.762495317921000031E-11, -1.000000000000000000, -4.762531464717999529E-11 ) ) ;
#11175 = DIRECTION ( 'NONE',  ( 0.000000000000000000, -1.000000000000000000, 0.000000000000000000 ) ) ;
#11176 = ORIENTED_EDGE ( 'NONE', *, *, #9161, .F. ) ;
#11177 = CARTESIAN_POINT ( 'NONE',  ( -1.210921577777000158, -78.14370837986389517, 0.5587889421650999999 ) ) ;
#11178 = CARTESIAN_POINT ( 'NONE',  ( 12.71798269388000158, -60.09778754156999980, 1.931086388578000079 ) ) ;
#11179 = CARTESIAN_POINT ( 'NONE',  ( 0.07163746727446854146, -80.73022344930195970, -1.248029480940866520 ) ) ;
#11180 = ORIENTED_EDGE ( 'NONE', *, *, #48851, .F. ) ;
#11181 = CARTESIAN_POINT ( 'NONE',  ( -3.634457760627999523, -77.72550115664098769, 11.72972702006000034 ) ) ;
#11182 = CARTESIAN_POINT ( 'NONE',  ( 11.32642973867000080, -77.38166194916898633, 1.553704360265000028 ) ) ;
#11183 = VERTEX_POINT ( 'NONE', #35207 ) ;
#11184 = ORIENTED_EDGE ( 'NONE', *, *, #28599, .T. ) ;
#11185 = AXIS2_PLACEMENT_3D ( 'NONE', #51219, #32879, #18459 ) ;
#11186 = CARTESIAN_POINT ( 'NONE',  ( 0.9073035717151847201, -80.41100119561156134, 0.8599128470893483422 ) ) ;
#11187 = EDGE_CURVE ( 'NONE', #47194, #28878, #13073, .T. ) ;
#11188 = CARTESIAN_POINT ( 'NONE',  ( -6.301614265331000553, -77.06173998579799900, 7.165911196006999440 ) ) ;
#11189 = CARTESIAN_POINT ( 'NONE',  ( -7.479908383216000267, -79.56589192459449578, -6.281056869080000382 ) ) ;
#11190 = VERTEX_POINT ( 'NONE', #39942 ) ;
#11191 = CARTESIAN_POINT ( 'NONE',  ( -12.71536556657220451, -24.12544729046540581, -1.781281568994087072 ) ) ;
#11192 = CARTESIAN_POINT ( 'NONE',  ( 7.599690325503999588, -78.75968566096200618, -7.837095951096998192 ) ) ;
#11193 = EDGE_CURVE ( 'NONE', #425, #47713, #905, .T. ) ;
#11194 = ORIENTED_EDGE ( 'NONE', *, *, #45937, .F. ) ;
#11195 = CARTESIAN_POINT ( 'NONE',  ( -12.49837680049000177, -23.20957148803000081, -1.667051419334999895 ) ) ;
#11196 = CARTESIAN_POINT ( 'NONE',  ( -9.454379850511999805, -77.50246915034600192, 0.8787206290761000460 ) ) ;
#11197 = DIRECTION ( 'NONE',  ( 0.7071067811865475727, 0.000000000000000000, -0.7071067811865475727 ) ) ;
#11198 = CARTESIAN_POINT ( 'NONE',  ( 0.000000000000000000, -80.99999999999998579, 7.000000000000000000 ) ) ;
#11199 = CARTESIAN_POINT ( 'NONE',  ( 3.938458446976999205, -79.21000000000000796, -8.369650235310999165 ) ) ;
#11200 = CARTESIAN_POINT ( 'NONE',  ( 7.135985293347999914, -76.86160783604827884, -6.061232200253999558 ) ) ;
#11201 = EDGE_CURVE ( 'NONE', #17327, #5962, #44231, .T. ) ;
#11202 = CARTESIAN_POINT ( 'NONE',  ( -0.8490343226412601085, -78.42778975272105413, -1.282990012170490690 ) ) ;
#11203 = CARTESIAN_POINT ( 'NONE',  ( -2.879226727952072018, -79.70416666666665151, -10.71369944335147295 ) ) ;
#11204 = CARTESIAN_POINT ( 'NONE',  ( -6.282410744257000523, -75.86562114363999854, 10.58616248715999930 ) ) ;
#11205 = CARTESIAN_POINT ( 'NONE',  ( 6.582919013437252609, -77.16874999997368434, -6.583307234616106562 ) ) ;
#11206 = DIRECTION ( 'NONE',  ( 0.000000000000000000, 1.000000000000000000, 0.000000000000000000 ) ) ;
#11207 = CARTESIAN_POINT ( 'NONE',  ( -3.911342194028000208, -78.54716864382999120, -11.62327352135999980 ) ) ;
#11208 = CARTESIAN_POINT ( 'NONE',  ( 12.07535958108000074, -76.80152308111600234, -2.237927141218000404 ) ) ;
#11209 = CARTESIAN_POINT ( 'NONE',  ( 7.596835002782696300, -78.70208333333332007, 5.838193839761711246 ) ) ;
#11210 = CARTESIAN_POINT ( 'NONE',  ( -11.56310788679330237, -77.52280291465159223, 4.163831652655801463 ) ) ;
#11211 = CARTESIAN_POINT ( 'NONE',  ( 0.9578316561261159823, -78.88180395574651982, -11.17589679220000143 ) ) ;
#11212 = ORIENTED_EDGE ( 'NONE', *, *, #23827, .F. ) ;
#11213 = CARTESIAN_POINT ( 'NONE',  ( -0.9485035383083301186, -80.67909605160095055, 1.175018830168555128 ) ) ;
#11214 = CARTESIAN_POINT ( 'NONE',  ( 9.396085398178630754, -77.99791666666665435, -7.220923959705230821 ) ) ;
#11215 = CARTESIAN_POINT ( 'NONE',  ( 3.600000000000000089, -0.2000000000000000111, 0.000000000000000000 ) ) ;
#11216 = CARTESIAN_POINT ( 'NONE',  ( -13.89999999999999858, -72.79999999999999716, 0.000000000000000000 ) ) ;
#11217 = CARTESIAN_POINT ( 'NONE',  ( -0.4524135602540000356, -2.766177049815000011, 3.686430941907999692 ) ) ;
#11218 = CARTESIAN_POINT ( 'NONE',  ( 12.13705548371000020, -78.69651279900399743, 0.8212409526314999875 ) ) ;
#11219 = CARTESIAN_POINT ( 'NONE',  ( -8.102939992022999860, -78.31761851250499262, -5.403892966383000207 ) ) ;
#11220 = CIRCLE ( 'NONE', #15962, 1.250000000000000000 ) ;
#11222 = PLANE ( 'NONE',  #36232 ) ;
#11221 = CARTESIAN_POINT ( 'NONE',  ( -5.657080530349652747, -76.11476686863957752, 10.31273069280180366 ) ) ;
#11223 = CARTESIAN_POINT ( 'NONE',  ( 1.204186364734999959, -81.79254865883000036, -0.6131120777826000179 ) ) ;
#11224 = DIRECTION ( 'NONE',  ( 0.000000000000000000, -1.000000000000000000, 0.000000000000000000 ) ) ;
#11225 = VERTEX_POINT ( 'NONE', #40242 ) ;
#11226 = CARTESIAN_POINT ( 'NONE',  ( 12.70451681027663859, -25.17641660208789389, 0.5206746370197306018 ) ) ;
#11227 = CARTESIAN_POINT ( 'NONE',  ( -0.2199206942898871697, -79.42994573680664416, -1.482330506908097201 ) ) ;
#11228 = CARTESIAN_POINT ( 'NONE',  ( 8.596418555780418913, -77.30208333333331439, 6.606377239730356621 ) ) ;
#11229 = CARTESIAN_POINT ( 'NONE',  ( -7.624757096145000190, -60.60351363786999457, 10.47516529250999895 ) ) ;
#11230 = CARTESIAN_POINT ( 'NONE',  ( -9.888820909766963041, -80.06422814540057686, 4.845029618406575089 ) ) ;
#11231 = CARTESIAN_POINT ( 'NONE',  ( 7.549855238205000596, -78.88173981539898705, 5.864427966874999676 ) ) ;
#11232 = CARTESIAN_POINT ( 'NONE',  ( 12.00000000000000711, -78.13958333333333428, -1.570796326794872355 ) ) ;
#11233 = CARTESIAN_POINT ( 'NONE',  ( -1.480597980168999888E-14, -80.60000000000000853, 0.000000000000000000 ) ) ;
#11234 = ORIENTED_EDGE ( 'NONE', *, *, #12558, .T. ) ;
#11235 = EDGE_CURVE ( 'NONE', #25256, #28446, #40541, .T. ) ;
#11236 = CARTESIAN_POINT ( 'NONE',  ( -9.845147265217999433, -79.31693931322499225, -5.468732932272000191 ) ) ;
#11237 = CYLINDRICAL_SURFACE ( 'NONE', #7857, 12.80000000000000071 ) ;
#11238 = AXIS2_PLACEMENT_3D ( 'NONE', #14585, #49461, #45908 ) ;
#11239 = CARTESIAN_POINT ( 'NONE',  ( 10.96304720905350472, -79.33042955265048590, 4.455755102610416074 ) ) ;
#11240 = CARTESIAN_POINT ( 'NONE',  ( 0.000000000000000000, -18.84999999999999787, -12.00000000000000000 ) ) ;
#11241 = CARTESIAN_POINT ( 'NONE',  ( -0.01395791329646856385, -81.47639348663375358, 1.249632885952940864 ) ) ;
#11242 = CARTESIAN_POINT ( 'NONE',  ( -1.000309426110861599, -79.09703484861441325, 0.7891363950083513101 ) ) ;
#11243 = CARTESIAN_POINT ( 'NONE',  ( 0.3664097462935664851, -53.82809982434488916, -12.50575740041013439 ) ) ;
#11244 = CARTESIAN_POINT ( 'NONE',  ( 2.062670899148999926, -55.49360374314999689, -12.83044039271999992 ) ) ;
#11245 = CARTESIAN_POINT ( 'NONE',  ( -0.5100614604570999910, -79.17313804860999937, -1.204325901401000154 ) ) ;
#11246 = DIRECTION ( 'NONE',  ( 1.000000000000000000, 0.000000000000000000, 0.000000000000000000 ) ) ;
#11247 = CARTESIAN_POINT ( 'NONE',  ( 1.249999999999999778, -78.26041666666665719, 0.1636246173744711763 ) ) ;
#11248 = DIRECTION ( 'NONE',  ( 0.000000000000000000, -1.000000000000000000, 0.000000000000000000 ) ) ;
#11249 = ORIENTED_EDGE ( 'NONE', *, *, #47769, .F. ) ;
#11250 = ORIENTED_EDGE ( 'NONE', *, *, #38896, .T. ) ;
#11251 = CARTESIAN_POINT ( 'NONE',  ( -12.09770333016000166, -77.34888712250798903, -3.481192270638000075 ) ) ;
#11252 = CARTESIAN_POINT ( 'NONE',  ( 2.115012927989350811, -78.74089074757185358, -10.53979812572510255 ) ) ;
#11253 = EDGE_CURVE ( 'NONE', #35254, #54663, #3648, .T. ) ;
#11254 = VERTEX_POINT ( 'NONE', #17816 ) ;
#11255 = CARTESIAN_POINT ( 'NONE',  ( 7.986982684666001475, -17.27364722735000058, 10.07612755993999976 ) ) ;
#11256 = AXIS2_PLACEMENT_3D ( 'NONE', #35576, #17290, #18185 ) ;
#11257 = CARTESIAN_POINT ( 'NONE',  ( -1.779623408300066600, -54.66369130952792688, 12.71471627654026548 ) ) ;
#11258 = CARTESIAN_POINT ( 'NONE',  ( 2.581611620594999934, -78.68929468166000163, 11.78230914923999961 ) ) ;
#11259 = FACE_OUTER_BOUND ( 'NONE', #22332, .T. ) ;
#11260 = LINE ( 'NONE', #51995, #29604 ) ;
#11261 = FACE_OUTER_BOUND ( 'NONE', #18195, .T. ) ;
#11262 = CARTESIAN_POINT ( 'NONE',  ( 3.371435477143000181, -79.48318836525099584, -10.69820234502000034 ) ) ;
#11263 = EDGE_CURVE ( 'NONE', #3715, #30430, #55707, .T. ) ;
#11264 = VERTEX_POINT ( 'NONE', #39658 ) ;
#11265 = LINE ( 'NONE', #47292, #42575 ) ;
#11266 = ORIENTED_EDGE ( 'NONE', *, *, #28555, .T. ) ;
#11267 = CARTESIAN_POINT ( 'NONE',  ( 7.356220924712871145, -77.29817559292861517, -5.612009723571459219 ) ) ;
#11268 = CARTESIAN_POINT ( 'NONE',  ( 10.07768261906999996, -78.20698015179898732, -4.508174471003999706 ) ) ;
#11269 = AXIS2_PLACEMENT_3D ( 'NONE', #44390, #13675, #31672 ) ;
#11270 = CARTESIAN_POINT ( 'NONE',  ( 3.113304451009999863, -78.49783470746899638, -10.55022916317000181 ) ) ;
#11271 = UNCERTAINTY_MEASURE_WITH_UNIT (LENGTH_MEASURE( 1.000000000000000082E-05 ), #20137, 'distance_accuracy_value', 'NONE');
#11272 = CARTESIAN_POINT ( 'NONE',  ( -1.092853437769999880, -78.60826102536199755, -1.051005954092999906 ) ) ;
#11273 = CYLINDRICAL_SURFACE ( 'NONE', #29446, 10.75000000000000000 ) ;
#11274 = AXIS2_PLACEMENT_3D ( 'NONE', #37466, #28900, #1195 ) ;
#11275 = PLANE ( 'NONE',  #52103 ) ;
#11276 = CARTESIAN_POINT ( 'NONE',  ( 1.314530797355000225, -78.02943199921000428, -0.9595159925157999981 ) ) ;
#11277 = CARTESIAN_POINT ( 'NONE',  ( -7.682331425195999763, -19.23513569609999863, 10.04115011120000034 ) ) ;
#11278 = CARTESIAN_POINT ( 'NONE',  ( -9.501885680564001291, -79.53568019887099183, -5.638445012646999821 ) ) ;
#11279 = CARTESIAN_POINT ( 'NONE',  ( 6.536979956083999177, -79.32071718295554774, -10.09826910480999906 ) ) ;
#11280 = CARTESIAN_POINT ( 'NONE',  ( -3.302091768083000201, -84.62331260133198896, 1.295283620051000062 ) ) ;
#11281 = ORIENTED_EDGE ( 'NONE', *, *, #40043, .T. ) ;
#11282 = CARTESIAN_POINT ( 'NONE',  ( -0.4777645602529999591, -78.99535082056300439, -12.42424180296999836 ) ) ;
#11283 = DIRECTION ( 'NONE',  ( 0.7071067811865475727, 0.000000000000000000, -0.7071067811865475727 ) ) ;
#11284 = CARTESIAN_POINT ( 'NONE',  ( -1.249999986291000065, -76.30000000051599329, 0.6999999994844999796 ) ) ;
#11285 = CARTESIAN_POINT ( 'NONE',  ( 6.035966914210000311, -77.96687388343998748, 10.34809972146999968 ) ) ;
#11286 = CARTESIAN_POINT ( 'NONE',  ( -9.643342484277001248, -17.05965044154000054, 8.260141428683001052 ) ) ;
#11287 = CARTESIAN_POINT ( 'NONE',  ( 0.01020701576794861079, -78.62478094170407417, 1.275250707744829848 ) ) ;
#11288 = CARTESIAN_POINT ( 'NONE',  ( 0.6479767009551614665, -1.889685945776059972, -3.462595171283828321 ) ) ;
#11289 = CARTESIAN_POINT ( 'NONE',  ( 9.577959642148309527, -80.88765258768701472, 4.880894207245643379 ) ) ;
#11290 = CARTESIAN_POINT ( 'NONE',  ( 8.731705537153999330, -78.36041000571199788, -3.798380529179000042 ) ) ;
#11291 = CARTESIAN_POINT ( 'NONE',  ( 1.801750019967000016, -55.40992573246000319, -12.59656967650999881 ) ) ;
#11292 = CARTESIAN_POINT ( 'NONE',  ( 10.58169901997000117, -78.23167474757299544, 3.119195446298999919 ) ) ;
#11293 = CARTESIAN_POINT ( 'NONE',  ( 0.000000000000000000, -81.90000000002299885, 0.000000000000000000 ) ) ;
#11294 = CARTESIAN_POINT ( 'NONE',  ( -8.105251711770002032, -80.46822472744669597, 7.304004154415999039 ) ) ;
#11295 = CARTESIAN_POINT ( 'NONE',  ( -0.4908969598308604021, -81.24373489875783605, -1.175594168089061586 ) ) ;
#11296 = ORIENTED_EDGE ( 'NONE', *, *, #44540, .T. ) ;
#11297 = DIRECTION ( 'NONE',  ( -1.000000000000000000, 0.000000000000000000, 0.000000000000000000 ) ) ;
#11298 = CARTESIAN_POINT ( 'NONE',  ( 2.061649843245999758, -60.00561307554999502, -12.83797346717000210 ) ) ;
#11299 = CARTESIAN_POINT ( 'NONE',  ( -7.648026766733999615, -18.74999999413999774, -10.12290050089000104 ) ) ;
#11300 = CARTESIAN_POINT ( 'NONE',  ( -5.859445663532000914, -77.68484447970500639, 9.564779511708000115 ) ) ;
#11301 = CARTESIAN_POINT ( 'NONE',  ( 10.94409238582999855, -78.62588068511199424, 0.8311789410725000105 ) ) ;
#11302 = CARTESIAN_POINT ( 'NONE',  ( -0.9813197044111214851, -79.41829332103382910, -1.146063690337610685 ) ) ;
#11303 = CARTESIAN_POINT ( 'NONE',  ( -2.222528567983302228, -85.96510418484399452, 3.340687842950042619 ) ) ;
#11304 = CARTESIAN_POINT ( 'NONE',  ( -12.50000000000000000, -54.11762331445000029, -1.005384021965999963 ) ) ;
#11305 = CARTESIAN_POINT ( 'NONE',  ( 11.08108919492889655, -78.47635570878233580, 3.913470582576941137 ) ) ;
#11306 = CARTESIAN_POINT ( 'NONE',  ( -10.69999999999999929, -77.19999999999998863, 0.000000000000000000 ) ) ;
#11307 = ORIENTED_EDGE ( 'NONE', *, *, #45794, .F. ) ;
#11308 = EDGE_CURVE ( 'NONE', #38037, #17469, #43406, .T. ) ;
#11309 = CARTESIAN_POINT ( 'NONE',  ( -1.249631684896997275, -80.09712312601374151, 0.05486053264030937848 ) ) ;
#11310 = DIRECTION ( 'NONE',  ( 0.000000000000000000, 1.000000000000000000, 0.000000000000000000 ) ) ;
#11311 = EDGE_CURVE ( 'NONE', #48925, #37657, #42363, .T. ) ;
#11312 = CARTESIAN_POINT ( 'NONE',  ( -5.068180973607000261, -78.33054015155998684, -9.940077528656999561 ) ) ;
#11313 = CARTESIAN_POINT ( 'NONE',  ( -7.374560639698971798, -76.87291666666666856, -9.596002108778163731 ) ) ;
#11314 = CARTESIAN_POINT ( 'NONE',  ( 9.596002108778172612, -79.49791666666665435, -7.374560639698962028 ) ) ;
#11315 = CARTESIAN_POINT ( 'NONE',  ( 1.249716928680867145, -78.86070762237109477, 0.1637401775088879741 ) ) ;
#11316 = AXIS2_PLACEMENT_3D ( 'NONE', #28119, #18703, #50297 ) ;
#11317 = CARTESIAN_POINT ( 'NONE',  ( -0.5178498375169425794, -82.75219414049253430, 1.421764397643496602 ) ) ;
#11318 = CARTESIAN_POINT ( 'NONE',  ( -1.250000000000000000, -79.59999999999999432, 0.000000000000000000 ) ) ;
#11319 = AXIS2_PLACEMENT_3D ( 'NONE', #44925, #57616, #49654 ) ;
#11320 = CARTESIAN_POINT ( 'NONE',  ( -0.1963495408493606265, -78.01458333333334849, -1.500000000000000222 ) ) ;
#11321 = ORIENTED_EDGE ( 'NONE', *, *, #76, .T. ) ;
#11322 = CARTESIAN_POINT ( 'NONE',  ( 2.062670899148999926, -23.30639625649999758, 12.83044039274999903 ) ) ;
#11323 = B_SPLINE_CURVE_WITH_KNOTS ( 'NONE', 3,
 ( #25800, #8086, #26084, #52964, #48265, #4538, #43827, #21659, #39952, #23413, #32249, #37273, #28409, #10140, #28116, #46456, #46166, #13966 ),
 .UNSPECIFIED., .F., .F.,
 ( 4, 2, 2, 2, 2, 2, 2, 2, 4 ),
 ( 0.000000000000000000, 0.1250000000000000000, 0.2500000000000000000, 0.3750000000000000000, 0.5000000000000000000, 0.6250000000000000000, 0.7500000000000000000, 0.8750000000000000000, 1.000000000000000000 ),
 .UNSPECIFIED. ) ;
#11324 = CARTESIAN_POINT ( 'NONE',  ( -12.61112459819999998, -23.21565178569999688, 1.798929298655999931 ) ) ;
#11325 = VERTEX_POINT ( 'NONE', #52272 ) ;
#11326 = ORIENTED_EDGE ( 'NONE', *, *, #22856, .T. ) ;
#11327 = CARTESIAN_POINT ( 'NONE',  ( -12.78015286808999917, -54.49674784847999831, -1.806262579044999983 ) ) ;
#11328 = EDGE_CURVE ( 'NONE', #17190, #43667, #35098, .T. ) ;
#11329 = ORIENTED_EDGE ( 'NONE', *, *, #57711, .F. ) ;
#11330 = CARTESIAN_POINT ( 'NONE',  ( 2.074043784921811628, -79.89245142283287748, -9.331470595881391716 ) ) ;
#11331 = ORIENTED_EDGE ( 'NONE', *, *, #22017, .F. ) ;
#11332 = CARTESIAN_POINT ( 'NONE',  ( 0.006333666751159999601, -16.66737355700000123, 12.77652491955999992 ) ) ;
#11333 = CARTESIAN_POINT ( 'NONE',  ( 1.589707373765000042, -77.71003890373799550, -10.80037945888999928 ) ) ;
#11334 = CARTESIAN_POINT ( 'NONE',  ( 0.000000000000000000, 0.000000000000000000, 0.000000000000000000 ) ) ;
#11335 = CARTESIAN_POINT ( 'NONE',  ( 7.601397897754999633, -55.54999999966999980, -9.369164850722000892 ) ) ;
#11336 = CARTESIAN_POINT ( 'NONE',  ( -8.940852521590000990, -78.72666332859900251, -4.009928423322000057 ) ) ;
#11337 = CARTESIAN_POINT ( 'NONE',  ( -1.799561319299137985, -78.20949348124068479, -9.073216031666641257 ) ) ;
#11338 = LINE ( 'NONE', #1908, #23766 ) ;
#11339 = EDGE_CURVE ( 'NONE', #23790, #8940, #52718, .T. ) ;
#11340 = EDGE_LOOP ( 'NONE', ( #43171, #39987 ) ) ;
#11341 = COLOUR_RGB ( '', 0.09019608, 0.27058824, 0.51372549) ;
#11342 = ORIENTED_EDGE ( 'NONE', *, *, #44045, .T. ) ;
#11343 = PLANE ( 'NONE',  #57444 ) ;
#11344 = DIRECTION ( 'NONE',  ( 0.000000000000000000, 0.000000000000000000, -1.000000000000000000 ) ) ;
#11345 = ADVANCED_FACE ( 'NONE', ( #26255 ), #17113, .T. ) ;
#11346 = CARTESIAN_POINT ( 'NONE',  ( -12.66232158689999920, -61.93482640547999551, -0.5080765942054000783 ) ) ;
#11347 = CARTESIAN_POINT ( 'NONE',  ( 8.240135455977000589, -78.03587041461697993, -5.125512367919999868 ) ) ;
#11348 = CARTESIAN_POINT ( 'NONE',  ( 7.613962745608000127, -23.30639784948999704, 10.53101990620000095 ) ) ;
#11349 = DIRECTION ( 'NONE',  ( -0.9936845293270585300, -0.1122098755727947705, 0.000000000000000000 ) ) ;
#11350 = CARTESIAN_POINT ( 'NONE',  ( -0.7681833999686477066, -79.92708333333332860, 0.9995835529977223910 ) ) ;
#11351 = DIRECTION ( 'NONE',  ( 0.000000000000000000, -1.000000000000000000, 0.000000000000000000 ) ) ;
#11352 = CARTESIAN_POINT ( 'NONE',  ( -0.8211341099608999716, -80.35493433575999234, -1.491829658087999944 ) ) ;
#11353 = CARTESIAN_POINT ( 'NONE',  ( -12.05000000000000071, -79.29999999999999716, 0.000000000000000000 ) ) ;
#11354 = CARTESIAN_POINT ( 'NONE',  ( 3.837977427657000007, -82.34119486992599946, -1.636929820955000059 ) ) ;
#11355 = CARTESIAN_POINT ( 'NONE',  ( -0.2985019281634834210, -79.85924085546105289, -1.480232390986309321 ) ) ;
#11356 = CARTESIAN_POINT ( 'NONE',  ( 4.686931394918000038, -78.60731332859899112, -8.732305124302000010 ) ) ;
#11357 = CARTESIAN_POINT ( 'NONE',  ( 10.74995922344125532, -76.84496094653090381, -0.7036252426051674558 ) ) ;
#11358 = CARTESIAN_POINT ( 'NONE',  ( -7.646966891758999907, -18.80358255734000039, -10.19019756605999838 ) ) ;
#11359 = AXIS2_PLACEMENT_3D ( 'NONE', #31427, #26707, #36451 ) ;
#11360 = AXIS2_PLACEMENT_3D ( 'NONE', #31219, #17968, #35960 ) ;
#11362 = CARTESIAN_POINT ( 'NONE',  ( -1.320128238786999919, -78.77699527221300002, -0.1893081677438999966 ) ) ;
#11361 = CARTESIAN_POINT ( 'NONE',  ( 0.000000000000000000, -76.00000000000000000, 0.000000000000000000 ) ) ;
#11363 = AXIS2_PLACEMENT_3D ( 'NONE', #4551, #32554, #50602 ) ;
#11364 = ADVANCED_FACE ( 'NONE', ( #56701 ), #7965, .T. ) ;
#11365 = CARTESIAN_POINT ( 'NONE',  ( -0.8510563811109643773, -1.205768424899396285, -3.162557679667391319 ) ) ;
#11366 = CARTESIAN_POINT ( 'NONE',  ( -8.752258451002999706, -79.98164082875798897, -6.780921793939000075 ) ) ;
#11367 = DIRECTION ( 'NONE',  ( -1.000000000000000000, 0.000000000000000000, 0.000000000000000000 ) ) ;
#11368 = CARTESIAN_POINT ( 'NONE',  ( 0.07079953276963653341, -0.8766290037971383731, -3.580880310080847728 ) ) ;
#11369 = VERTEX_POINT ( 'NONE', #56981 ) ;
#11370 = DIRECTION ( 'NONE',  ( 0.000000000000000000, -1.000000000000000000, 0.000000000000000000 ) ) ;
#11371 = CARTESIAN_POINT ( 'NONE',  ( -2.062312494845999655, -55.57284340075000273, 12.83634740207000036 ) ) ;
#11372 = CARTESIAN_POINT ( 'NONE',  ( -0.007261404845503787592, -78.47568757210336798, 1.249841100264606375 ) ) ;
#11373 = CARTESIAN_POINT ( 'NONE',  ( 3.815187358399000139, -80.11518015861798858, -8.581477306024998697 ) ) ;
#11374 = CARTESIAN_POINT ( 'NONE',  ( -6.606527024733162001, -77.02724138212725791, 8.596707079130210261 ) ) ;
#11375 = DIRECTION ( 'NONE',  ( -1.000000000000000000, 0.000000000000000000, 0.000000000000000000 ) ) ;
#11376 = CARTESIAN_POINT ( 'NONE',  ( -3.250000000000001332, -3.010416666666667407, -0.4254240051736181139 ) ) ;
#11377 = ADVANCED_FACE ( 'NONE', ( #16543 ), #44269, .T. ) ;
#11378 = CARTESIAN_POINT ( 'NONE',  ( -1.417334032777999964, -79.02654225787900089, -0.4910847579886000736 ) ) ;
#11379 = EDGE_CURVE ( 'NONE', #11369, #3961, #39481, .T. ) ;
#11380 = MECHANICAL_DESIGN_GEOMETRIC_PRESENTATION_REPRESENTATION (  '', ( #5834 ), #36932 ) ;
#11381 = CARTESIAN_POINT ( 'NONE',  ( 3.992904449609000483, -78.62148118236265759, -4.889897653514886385E-16 ) ) ;
#11382 = CARTESIAN_POINT ( 'NONE',  ( 10.16239288306999988, -78.02471363368498203, -4.355854389664999715 ) ) ;
#11383 = CIRCLE ( 'NONE', #4791, 12.50000000000000000 ) ;
#11384 = CARTESIAN_POINT ( 'NONE',  ( 9.758188809318015799, -76.40248920481857908, -6.544674992857547835 ) ) ;
#11385 = CARTESIAN_POINT ( 'NONE',  ( -7.585478157043000103, -77.20580276511299189, -8.010134550088000793 ) ) ;
#11386 = CARTESIAN_POINT ( 'NONE',  ( -3.230363664242999810, -78.24804514476065265, -9.171071524558000121 ) ) ;
#11387 = CARTESIAN_POINT ( 'NONE',  ( 3.250000000000000444, -2.760416666666666963, 0.4254240051736248862 ) ) ;
#11388 = CARTESIAN_POINT ( 'NONE',  ( 1.210822168571061175, -78.36458333333334281, 9.250000000000001776 ) ) ;
#11389 = CARTESIAN_POINT ( 'NONE',  ( 3.165411199172027512, -2.729166666666666963, -0.8506806241676553304 ) ) ;
#11390 = CARTESIAN_POINT ( 'NONE',  ( 10.75315169796065895, -80.34831015543626620, -0.2582170068313175415 ) ) ;
#11391 = DIRECTION ( 'NONE',  ( 0.000000000000000000, 1.000000000000000000, 0.000000000000000000 ) ) ;
#11392 = DIRECTION ( 'NONE',  ( -0.7071067811865475727, 0.000000000000000000, -0.7071067811865475727 ) ) ;
#11393 = CARTESIAN_POINT ( 'NONE',  ( -9.625846388754000671, -79.25286561624899662, -7.214584339064000318 ) ) ;
#11394 = CARTESIAN_POINT ( 'NONE',  ( 9.549999999999998934, -76.39999999999999147, 0.000000000000000000 ) ) ;
#11395 = FACE_OUTER_BOUND ( 'NONE', #42401, .T. ) ;
#11396 = ORIENTED_EDGE ( 'NONE', *, *, #9775, .F. ) ;
#11397 = CARTESIAN_POINT ( 'NONE',  ( -0.5999999999999999778, -5.000000000000000000, -4.000000000000000000 ) ) ;
#11398 = ORIENTED_EDGE ( 'NONE', *, *, #57125, .T. ) ;
#11399 = EDGE_LOOP ( 'NONE', ( #27641, #45226, #12220, #14278, #15571 ) ) ;
#11400 = CIRCLE ( 'NONE', #45369, 12.90000000000000036 ) ;
#11401 =( LENGTH_UNIT ( ) NAMED_UNIT ( * ) SI_UNIT ( .MILLI., .METRE. ) );
#11402 = CARTESIAN_POINT ( 'NONE',  ( -1.538071403319991814, -77.41458333333332575, -11.75000000000000355 ) ) ;
#11403 = CARTESIAN_POINT ( 'NONE',  ( -3.459349611910000011, -81.80899506498398921, -0.7732216137953999979 ) ) ;
#11404 = CARTESIAN_POINT ( 'NONE',  ( 8.925046886613115404, -79.17747656854896832, 3.256041339590551420 ) ) ;
#11405 = ORIENTED_EDGE ( 'NONE', *, *, #20004, .T. ) ;
#11406 = CARTESIAN_POINT ( 'NONE',  ( 0.5370760595369525880, -82.76026336597686850, -1.130548436120011102 ) ) ;
#11407 = ORIENTED_EDGE ( 'NONE', *, *, #11911, .F. ) ;
#11408 = DIRECTION ( 'NONE',  ( 0.000000000000000000, 1.000000000000000000, 0.000000000000000000 ) ) ;
#11409 = VERTEX_POINT ( 'NONE', #57269 ) ;
#11410 = CARTESIAN_POINT ( 'NONE',  ( 7.919595949288999570, -55.64999999964999233, -9.050966799188000067 ) ) ;
#11411 = CARTESIAN_POINT ( 'NONE',  ( 1.465732314324990737, -78.97676429292373257, -0.4454333615512816591 ) ) ;
#11412 = CARTESIAN_POINT ( 'NONE',  ( -8.014512096362414795, -79.79999999999998295, -8.788959260803750340 ) ) ;
#11413 = CARTESIAN_POINT ( 'NONE',  ( -6.960157075943352645, -80.03140959141880728, 8.192335473613402641 ) ) ;
#11414 = CARTESIAN_POINT ( 'NONE',  ( 2.294679948690146798, -86.17851879815597727, -3.222726853798347779 ) ) ;
#11415 = CARTESIAN_POINT ( 'NONE',  ( -4.800187936532999800, -76.31198526659200354, 10.10109298474000106 ) ) ;
#11416 = CARTESIAN_POINT ( 'NONE',  ( -1.250000000000000000, -81.49999999999998579, 0.000000000000000000 ) ) ;
#11417 = CARTESIAN_POINT ( 'NONE',  ( 9.611650271896829523, -78.49166666666667425, 5.539808784079915505 ) ) ;
#11418 = CARTESIAN_POINT ( 'NONE',  ( -10.93116861664999995, -76.37668473043899553, 2.007280421741000076 ) ) ;
#11419 = CARTESIAN_POINT ( 'NONE',  ( -4.412537506371384310, -78.68548379871316456, -8.131199301624301157 ) ) ;
#11420 = VECTOR ( 'NONE', #1376, 1000.000000000000000 ) ;
#11421 = CARTESIAN_POINT ( 'NONE',  ( 2.167121982807000080, -77.36361167140100292, 9.270132485773999065 ) ) ;
#11422 = CARTESIAN_POINT ( 'NONE',  ( 0.9788970803261000109, -79.86870113126700232, -0.9057243817226000582 ) ) ;
#11423 = CARTESIAN_POINT ( 'NONE',  ( -10.28968504916697313, -80.12913738177938683, -3.888065173257339247 ) ) ;
#11424 = CARTESIAN_POINT ( 'NONE',  ( -3.110324816758189836, -3.077988516191772828, 0.9426514480803485085 ) ) ;
#11425 = CARTESIAN_POINT ( 'NONE',  ( -3.752701485998999775, -79.88453455456799190, 0.1690965569945000191 ) ) ;
#11426 = CARTESIAN_POINT ( 'NONE',  ( -12.18267985468999903, -79.51314988871099843, -0.6568425513276999750 ) ) ;
#11427 = CARTESIAN_POINT ( 'NONE',  ( -8.955948465137943515, -78.05351281406913699, 5.945725506398519045 ) ) ;
#11428 = EDGE_CURVE ( 'NONE', #45010, #29062, #52873, .T. ) ;
#11429 = CARTESIAN_POINT ( 'NONE',  ( -0.5585027192942962904, -83.01198894187744770, 1.119379558410208420 ) ) ;
#11430 = CARTESIAN_POINT ( 'NONE',  ( -13.13047446164998711, -59.58578169018999660, -0.8260994316375004365 ) ) ;
#11431 = CARTESIAN_POINT ( 'NONE',  ( -2.902028414455999794, -86.04119503318798934, 2.039475191455999870 ) ) ;
#11432 = FACE_OUTER_BOUND ( 'NONE', #812, .T. ) ;
#11433 = CARTESIAN_POINT ( 'NONE',  ( -7.646092217304000904, -60.50851177880000620, -10.13691708059000085 ) ) ;
#11434 = ADVANCED_FACE ( 'NONE', ( #37086 ), #53414, .T. ) ;
#11435 = CYLINDRICAL_SURFACE ( 'NONE', #26997, 9.500000000000000000 ) ;
#11436 = CARTESIAN_POINT ( 'NONE',  ( -0.1963495408493605987, -77.61458333333330017, -1.500000000000000444 ) ) ;
#11437 = VECTOR ( 'NONE', #37382, 1000.000000000000000 ) ;
#11438 = CARTESIAN_POINT ( 'NONE',  ( -12.83675912440999944, -18.77244614031999959, -2.062833085520999976 ) ) ;
#11439 = CARTESIAN_POINT ( 'NONE',  ( 5.647598101448999763, -77.89127586458999986, 11.72364604052000203 ) ) ;
#11440 = AXIS2_PLACEMENT_3D ( 'NONE', #22698, #21602, #23568 ) ;
#11441 = CARTESIAN_POINT ( 'NONE',  ( -8.316360841097289125, -78.00592770181216906, -6.948075690853510622 ) ) ;
#11442 = CARTESIAN_POINT ( 'NONE',  ( -0.7700304397887851593, -78.31794389177034077, -11.75310685588702064 ) ) ;
#11443 = CARTESIAN_POINT ( 'NONE',  ( -14.00000000000000000, -32.88214388149999934, 0.000000000000000000 ) ) ;
#11444 = CARTESIAN_POINT ( 'NONE',  ( 12.45128148039999871, -75.75224522809000405, 1.234877051265000025 ) ) ;
#11445 = VERTEX_POINT ( 'NONE', #23803 ) ;
#11446 = EDGE_CURVE ( 'NONE', #38752, #48919, #29647, .T. ) ;
#11447 = CARTESIAN_POINT ( 'NONE',  ( 10.07210119001000059, -80.53695791176038199, 5.045985883512999592 ) ) ;
#11448 = CARTESIAN_POINT ( 'NONE',  ( 3.106054555984999688, -86.07390000031799104, -1.382904586457999851 ) ) ;
#11449 = CARTESIAN_POINT ( 'NONE',  ( 12.48409101790999998, -60.16970703802000031, 1.669510252625000080 ) ) ;
#11450 = CARTESIAN_POINT ( 'NONE',  ( 10.72212007569999948, -79.38422702059999381, -4.932905528729000011 ) ) ;
#11451 = CARTESIAN_POINT ( 'NONE',  ( 12.77302454164000167, -54.07764858523999862, -1.481891240072999993 ) ) ;
#11452 = CARTESIAN_POINT ( 'NONE',  ( 9.062046460520999602, -77.61557598619799592, -3.260755114102000363 ) ) ;
#11453 = CARTESIAN_POINT ( 'NONE',  ( 0.3958579896396000608, -81.47369891792999397, -1.618315812554999900 ) ) ;
#11454 = DIRECTION ( 'NONE',  ( 0.000000000000000000, 1.000000000000000000, 0.000000000000000000 ) ) ;
#11455 = CARTESIAN_POINT ( 'NONE',  ( -1.500000000000000000, -77.50000000000000000, 0.000000000000000000 ) ) ;
#11456 = ORIENTED_EDGE ( 'NONE', *, *, #190, .F. ) ;
#11457 = LINE ( 'NONE', #25592, #22065 ) ;
#11458 = DIRECTION ( 'NONE',  ( 1.000000000000000000, 0.000000000000000000, 0.000000000000000000 ) ) ;
#11459 = CARTESIAN_POINT ( 'NONE',  ( 0.6796913841968065251, -78.91095482288170615, -3.420124432299513462 ) ) ;
#11460 = EDGE_CURVE ( 'NONE', #44860, #37493, #8125, .T. ) ;
#11461 = ORIENTED_EDGE ( 'NONE', *, *, #19575, .T. ) ;
#11462 = CARTESIAN_POINT ( 'NONE',  ( 0.9384621721472999889, -78.49099674353139733, 0.9475573338641000154 ) ) ;
#11463 = B_SPLINE_CURVE_WITH_KNOTS ( 'NONE', 3,
 ( #28196, #51548, #24952, #55375, #46835, #5776, #11104, #6362, #24378, #6069, #42677, #2246, #55083, #24077, #20243, #1370, #38236, #15808 ),
 .UNSPECIFIED., .F., .F.,
 ( 4, 2, 2, 2, 2, 2, 2, 2, 4 ),
 ( 0.000000000000000000, 0.1249999999999998335, 0.2499999999999997224, 0.3749999999999997224, 0.4999999999999997780, 0.6249999999999997780, 0.7499999999999998890, 0.8749999999999998890, 1.000000000000000000 ),
 .UNSPECIFIED. ) ;
#11464 = CARTESIAN_POINT ( 'NONE',  ( 2.567527713034000403, -78.45060060100799149, -10.74642708485000142 ) ) ;
#11465 = EDGE_CURVE ( 'NONE', #43629, #43983, #57428, .T. ) ;
#11466 = CARTESIAN_POINT ( 'NONE',  ( 5.729309059712077712, -77.67757408254945517, -7.360974123654262513 ) ) ;
#11467 = CARTESIAN_POINT ( 'NONE',  ( -9.709765936195999814, -79.63777772118899634, 5.586663845304999931 ) ) ;
#11468 = ORIENTED_EDGE ( 'NONE', *, *, #4758, .F. ) ;
#11469 = CIRCLE ( 'NONE', #6735, 0.5000000000000006661 ) ;
#11470 = CARTESIAN_POINT ( 'NONE',  ( 9.940990682305997694, -78.95998123256899248, -7.011364793726000855 ) ) ;
#11471 = CARTESIAN_POINT ( 'NONE',  ( -10.46158978484000102, -78.08816509035798958, -4.329824488994000298 ) ) ;
#11472 = ORIENTED_EDGE ( 'NONE', *, *, #52390, .T. ) ;
#11473 = ORIENTED_EDGE ( 'NONE', *, *, #32253, .F. ) ;
#11474 = ORIENTED_EDGE ( 'NONE', *, *, #22117, .T. ) ;
#11475 = CARTESIAN_POINT ( 'NONE',  ( -0.5581268078707392055, -80.51203588205464712, 1.118380629099624546 ) ) ;
#11476 = CARTESIAN_POINT ( 'NONE',  ( -8.818477034137000459, -77.09813998579799943, 3.646243024668999855 ) ) ;
#11477 = CARTESIAN_POINT ( 'NONE',  ( -9.387315177295000979, -80.22774216884852194, 2.697965643110000311 ) ) ;
#11478 = ORIENTED_EDGE ( 'NONE', *, *, #35451, .F. ) ;
#11479 = CARTESIAN_POINT ( 'NONE',  ( -1.433413778493000112, -78.18772245792399644, -10.60928646434000200 ) ) ;
#11480 = EDGE_LOOP ( 'NONE', ( #41927, #20880, #46655, #15639 ) ) ;
#11481 = AXIS2_PLACEMENT_3D ( 'NONE', #5580, #9730, #37172 ) ;
#11482 = CARTESIAN_POINT ( 'NONE',  ( -9.356096982537000173, -78.99405786821630215, 7.928589704419000128 ) ) ;
#11483 = CARTESIAN_POINT ( 'NONE',  ( -7.264520526674999701, -77.56551915034600597, -6.114261184555999762 ) ) ;
#11484 = AXIS2_PLACEMENT_3D ( 'NONE', #13759, #9351, #44778 ) ;
#11485 = CARTESIAN_POINT ( 'NONE',  ( 9.213130513665999999, -53.79475660653999824, 8.533779407502999348 ) ) ;
#11486 = CARTESIAN_POINT ( 'NONE',  ( 10.10712711932128549, -17.53345760874380588, -7.860996423953121592 ) ) ;
#11487 = CARTESIAN_POINT ( 'NONE',  ( -1.500000000000000444, -81.38958333333330586, 0.1963495408493560745 ) ) ;
#11488 = CARTESIAN_POINT ( 'NONE',  ( -11.67560174948319052, -77.20966691730704667, -1.536251511391871771 ) ) ;
#11489 = CARTESIAN_POINT ( 'NONE',  ( 2.914566591598000134, -77.01848277179368552, 9.303650809983000869 ) ) ;
#11490 = CARTESIAN_POINT ( 'NONE',  ( -1.495765920156680862, -77.83884168506972401, 0.2048668414424503481 ) ) ;
#11491 = CARTESIAN_POINT ( 'NONE',  ( -3.140159956018519161, -81.86041668085154299, -2.498940541498651413 ) ) ;
#11492 = CARTESIAN_POINT ( 'NONE',  ( -7.631896413330000684, -23.22122715205999555, 10.36221694966999962 ) ) ;
#11493 = CARTESIAN_POINT ( 'NONE',  ( -8.706831144604571193, -79.33395239776687902, -3.878314185012179838 ) ) ;
#11494 = CARTESIAN_POINT ( 'NONE',  ( 9.249999999999998224, -77.76041666666667140, 1.210822168571084934 ) ) ;
#11495 = CYLINDRICAL_SURFACE ( 'NONE', #34158, 1.750000000000001332 ) ;
#11496 = CARTESIAN_POINT ( 'NONE',  ( 10.42531125068999920, -23.26485145404000221, -7.624341767093000044 ) ) ;
#11497 = LINE ( 'NONE', #30332, #26272 ) ;
#11498 = DIRECTION ( 'NONE',  ( 0.000000000000000000, 0.000000000000000000, -1.000000000000000000 ) ) ;
#11499 = CARTESIAN_POINT ( 'NONE',  ( -8.501675986534307228, -77.48722301659734057, 8.566518206373759270 ) ) ;
#11500 = CARTESIAN_POINT ( 'NONE',  ( 0.6295237254636258939, -78.66666666666665719, -1.092232985442821658 ) ) ;
#11501 = MECHANICAL_DESIGN_GEOMETRIC_PRESENTATION_REPRESENTATION (  '', ( #20917 ), #51915 ) ;
#11502 = ORIENTED_EDGE ( 'NONE', *, *, #27994, .F. ) ;
#11503 = CARTESIAN_POINT ( 'NONE',  ( -1.463514287764630550, -80.77019107339425830, -0.3791178640163613833 ) ) ;
#11504 = CARTESIAN_POINT ( 'NONE',  ( 2.061613410425999771, -23.20570014476000154, 12.83797036855999885 ) ) ;
#11505 = DIRECTION ( 'NONE',  ( 0.000000000000000000, 0.000000000000000000, 1.000000000000000000 ) ) ;
#11506 = CARTESIAN_POINT ( 'NONE',  ( -2.528906407072000206, -2.906459358523000081, 2.502418873083000150 ) ) ;
#11507 = CARTESIAN_POINT ( 'NONE',  ( 11.16396169635999946, -78.72364211442699400, 4.832020119862000307 ) ) ;
#11508 = DIRECTION ( 'NONE',  ( -2.582622310454000054E-11, 0.000000000000000000, 1.000000000000000000 ) ) ;
#11510 = FACE_OUTER_BOUND ( 'NONE', #49584, .T. ) ;
#11509 = CARTESIAN_POINT ( 'NONE',  ( -9.578632711364354790, -76.15034707418256232, 6.805328245342409765 ) ) ;
#11511 = CARTESIAN_POINT ( 'NONE',  ( 4.528616239255999432, -79.18563051119899399, -9.933126443765001312 ) ) ;
#11512 = CARTESIAN_POINT ( 'NONE',  ( 0.000000000000000000, -75.09999999979599750, 0.000000000000000000 ) ) ;
#11513 = VERTEX_POINT ( 'NONE', #53885 ) ;
#11514 = EDGE_CURVE ( 'NONE', #12818, #6738, #13121, .T. ) ;
#11515 = CARTESIAN_POINT ( 'NONE',  ( -2.935661446561999899, -77.00000000000000000, -9.035036904803998681 ) ) ;
#11516 = CARTESIAN_POINT ( 'NONE',  ( -7.052869246477441401, -79.30872110581411505, -6.415029687693263760 ) ) ;
#11517 = CARTESIAN_POINT ( 'NONE',  ( 9.050966799188000067, -59.94999999967000548, -7.919595949288999570 ) ) ;
#11518 = CARTESIAN_POINT ( 'NONE',  ( -7.646788277353000041, -60.17228598344999568, 10.00831419132999933 ) ) ;
#11519 = AXIS2_PLACEMENT_3D ( 'NONE', #20480, #11629, #56780 ) ;
#11520 = CARTESIAN_POINT ( 'NONE',  ( -10.19950126981313687, -80.06978458045568914, 4.126879458600376971 ) ) ;
#11521 = CARTESIAN_POINT ( 'NONE',  ( -5.286327514246000447, -80.06604530392098695, 7.677899541690999641 ) ) ;
#11522 = DIRECTION ( 'NONE',  ( 1.000000000000000000, 0.000000000000000000, 0.000000000000000000 ) ) ;
#11523 = CARTESIAN_POINT ( 'NONE',  ( -1.439896632895311335, -78.71458333333333712, -11.00000000000000178 ) ) ;
#11524 = ORIENTED_EDGE ( 'NONE', *, *, #55298, .T. ) ;
#11525 = CIRCLE ( 'NONE', #34115, 0.5000000000000006661 ) ;
#11526 = CARTESIAN_POINT ( 'NONE',  ( 9.160466309606078994, -76.05310292770596448, -6.106013103578413315 ) ) ;
#11527 = CARTESIAN_POINT ( 'NONE',  ( -6.394497296648475881, -79.12919937753510169, -9.959691579247014204 ) ) ;
#11528 = CARTESIAN_POINT ( 'NONE',  ( 9.473958333266658371, -79.52604166666334606, -0.9915651818467657863 ) ) ;
#11529 = CARTESIAN_POINT ( 'NONE',  ( 0.4168712897526509753, -81.44826334302578630, 1.178261328541365893 ) ) ;
#11530 = ADVANCED_FACE ( 'NONE', ( #21121 ), #17870, .F. ) ;
#11531 = CARTESIAN_POINT ( 'NONE',  ( -1.160672508370670153, -78.68359632043879515, -0.5250652338630038551 ) ) ;
#11532 = CARTESIAN_POINT ( 'NONE',  ( 1.247385798810000113, -54.32277743478999810, -12.50301438874000048 ) ) ;
#11533 = DIRECTION ( 'NONE',  ( 0.7071067811865475727, 0.000000000000000000, 0.7071067811865475727 ) ) ;
#11534 = AXIS2_PLACEMENT_3D ( 'NONE', #38230, #1655, #55958 ) ;
#11535 = CARTESIAN_POINT ( 'NONE',  ( 1.980532758766000212, -19.23743349341999931, 12.80088938805999987 ) ) ;
#11536 = LINE ( 'NONE', #30082, #51859 ) ;
#11537 = DIRECTION ( 'NONE',  ( 0.000000000000000000, -0.7071067811866525998, -0.7071067811864425456 ) ) ;
#11538 = ORIENTED_EDGE ( 'NONE', *, *, #37347, .F. ) ;
#11539 = EDGE_LOOP ( 'NONE', ( #5316, #28565, #50787, #19435 ) ) ;
#11540 = B_SPLINE_CURVE_WITH_KNOTS ( 'NONE', 3,
 ( #21710, #40893, #49167, #484, #40308, #57723 ),
 .UNSPECIFIED., .F., .F.,
 ( 4, 1, 1, 4 ),
 ( 0.000000000000000000, 0.3333333333333000081, 0.6666666666667000474, 1.000000000000000000 ),
 .UNSPECIFIED. ) ;
#11541 = CARTESIAN_POINT ( 'NONE',  ( 10.32668202803999868, -76.46150529199699974, -6.991146065296999446 ) ) ;
#11542 = CARTESIAN_POINT ( 'NONE',  ( 4.892781134374668106, -78.76262618940380378, -9.574018988073637715 ) ) ;
#11543 = EDGE_LOOP ( 'NONE', ( #53831, #28729, #34018, #45007 ) ) ;
#11544 = ADVANCED_FACE ( 'NONE', ( #29964 ), #3981, .F. ) ;
#11545 = CARTESIAN_POINT ( 'NONE',  ( 7.633088938756000807, -18.60992532424000245, 10.18115029113000070 ) ) ;
#11546 = CARTESIAN_POINT ( 'NONE',  ( 9.253998064331378615, -79.07669581907259726, -2.773690070707886424 ) ) ;
#11547 = CARTESIAN_POINT ( 'NONE',  ( -1.980584515756000030, -55.53514849873000259, 12.76303204337999908 ) ) ;
#11548 = CARTESIAN_POINT ( 'NONE',  ( -10.46686097783000058, -77.11974203406001038, 7.365735401690999495 ) ) ;
#11549 = CARTESIAN_POINT ( 'NONE',  ( -10.75000000000000000, -79.59999999999999432, 0.000000000000000000 ) ) ;
#11550 = DIRECTION ( 'NONE',  ( 1.000000000000000000, 0.000000000000000000, 0.000000000000000000 ) ) ;
#11551 = CARTESIAN_POINT ( 'NONE',  ( -8.768124086712999699, -55.64999999965999677, -7.919595949288999570 ) ) ;
#11552 = CARTESIAN_POINT ( 'NONE',  ( 2.179295889402999897, -78.69333441819799191, 11.00312592022000047 ) ) ;
#11553 = ORIENTED_EDGE ( 'NONE', *, *, #53021, .T. ) ;
#11554 = CARTESIAN_POINT ( 'NONE',  ( 9.949999999959999286, -86.19999999995999929, 1.488367914068999967E-09 ) ) ;
#11555 = ORIENTED_EDGE ( 'NONE', *, *, #10939, .F. ) ;
#11556 = CARTESIAN_POINT ( 'NONE',  ( 5.442070907333274477, -77.27518984243994282, -7.479617580235857766 ) ) ;
#11557 = CARTESIAN_POINT ( 'NONE',  ( 12.54238283049872393, -60.32853599783607024, -1.749799162368461891 ) ) ;
#11558 = CYLINDRICAL_SURFACE ( 'NONE', #9746, 1.500000000000000000 ) ;
#11559 = CIRCLE ( 'NONE', #1203, 1.750000000000000000 ) ;
#11560 = CARTESIAN_POINT ( 'NONE',  ( -8.650006198296225080, -77.90482871549633614, -7.141358535548220310 ) ) ;
#11561 = CARTESIAN_POINT ( 'NONE',  ( -1.021885754039999927, -78.66363271308999572, -0.9827557610011000699 ) ) ;
#11562 = DIRECTION ( 'NONE',  ( -0.7071067811865475727, 0.000000000000000000, 0.7071067811865475727 ) ) ;
#11563 = CARTESIAN_POINT ( 'NONE',  ( 1.170845731893568331, -81.71777325584498897, -0.5056521153163634485 ) ) ;
#11564 = CARTESIAN_POINT ( 'NONE',  ( -0.1732310466989999687, -77.77311942765999220, 1.530487294790999986 ) ) ;
#11565 = CARTESIAN_POINT ( 'NONE',  ( 0.000000000000000000, -51.86282895648000135, 0.000000000000000000 ) ) ;
#11566 = CARTESIAN_POINT ( 'NONE',  ( 9.295311691678000088, -79.78851138786500030, 5.972861453165999812 ) ) ;
#11567 = CARTESIAN_POINT ( 'NONE',  ( -12.85140862679999962, -57.04439829966000275, 1.980464483675000054 ) ) ;
#11568 = DIRECTION ( 'NONE',  ( -0.9999999930530777403, 0.000000000000000000, -0.0001178721535689973885 ) ) ;
#11569 = CARTESIAN_POINT ( 'NONE',  ( -3.309164444370999991, -83.30682352787700040, -1.278276416343999911 ) ) ;
#11570 = ORIENTED_EDGE ( 'NONE', *, *, #48227, .T. ) ;
#11571 = CARTESIAN_POINT ( 'NONE',  ( -2.508516875516433320, -77.19999999999998863, 10.53783702169892678 ) ) ;
#11572 = CARTESIAN_POINT ( 'NONE',  ( -1.456085397364999867, -81.42568918487999952, -0.6271128268704999620 ) ) ;
#11573 = DIRECTION ( 'NONE',  ( 0.7071067811704841999, -1.939412262328955489E-07, -0.7071067812025843002 ) ) ;
#11574 = CARTESIAN_POINT ( 'NONE',  ( -11.06076315227999984, -78.03473190728298903, 4.601693484369000053 ) ) ;
#11575 = CARTESIAN_POINT ( 'NONE',  ( -9.830798712624998714, -17.90910918523000106, 7.765013391413999599 ) ) ;
#11576 = AXIS2_PLACEMENT_3D ( 'NONE', #53397, #57538, #21525 ) ;
#11577 = CARTESIAN_POINT ( 'NONE',  ( 10.20083256551678019, -78.87618565247994695, 3.463754871957966941 ) ) ;
#11578 = CARTESIAN_POINT ( 'NONE',  ( 3.487123655132066347, -1.989199735643871092, -0.4781024640137967463 ) ) ;
#11579 = CARTESIAN_POINT ( 'NONE',  ( 6.669449228234999971, -78.37530584965399783, -7.075468016816000016 ) ) ;
#11580 = CARTESIAN_POINT ( 'NONE',  ( 0.8456326333846000409, -78.27513851832499370, -9.484475825334998333 ) ) ;
#11581 = CARTESIAN_POINT ( 'NONE',  ( 0.5470778622144214509, -81.26141029258948834, -1.124504696060896425 ) ) ;
#11582 = CARTESIAN_POINT ( 'NONE',  ( 10.17013595917000046, -78.17720206157000007, -4.274350120612000481 ) ) ;
#11583 = DIRECTION ( 'NONE',  ( -0.7071067811864980568, -0.7071067811865969777, 1.459343291646993799E-08 ) ) ;
#11584 = DIRECTION ( 'NONE',  ( 0.7071067811865474617, 0.000000000000000000, -0.7071067811865474617 ) ) ;
#11585 = CARTESIAN_POINT ( 'NONE',  ( 0.8399831259196580691, -81.83208972731527808, -0.9577039101323847614 ) ) ;
#11586 = VERTEX_POINT ( 'NONE', #48014 ) ;
#11587 = AXIS2_PLACEMENT_3D ( 'NONE', #42512, #56379, #11793 ) ;
#11588 = CARTESIAN_POINT ( 'NONE',  ( -7.396918292183192634, -78.94791666666665719, 5.684557159767932077 ) ) ;
#11589 = EDGE_CURVE ( 'NONE', #10884, #4309, #107, .T. ) ;
#11590 = CARTESIAN_POINT ( 'NONE',  ( 11.75000000000000000, -76.95000000000000284, 0.000000000000000000 ) ) ;
#11591 = FACE_OUTER_BOUND ( 'NONE', #24891, .T. ) ;
#11592 = ADVANCED_FACE ( 'NONE', ( #26126, #44146, #39993, #34969 ), #39703, .F. ) ;
#11593 = CARTESIAN_POINT ( 'NONE',  ( -8.729704736441000534, -77.71208082270700856, 7.043462628994999974 ) ) ;
#11594 = CARTESIAN_POINT ( 'NONE',  ( 0.9090372547675998893, -78.73825010244298994, 10.93790052299999971 ) ) ;
#11595 = CYLINDRICAL_SURFACE ( 'NONE', #26234, 1.750000000000000000 ) ;
#11596 = CARTESIAN_POINT ( 'NONE',  ( 3.814358451465653221, -85.36770834507991879, -1.363609372161643796 ) ) ;
#11597 = DIRECTION ( 'NONE',  ( -3.655298286142000429E-11, 1.000000000000000000, 1.590757531940000291E-09 ) ) ;
#11598 = CYLINDRICAL_SURFACE ( 'NONE', #35891, 9.250000000000000000 ) ;
#11599 = CARTESIAN_POINT ( 'NONE',  ( -7.624341764943999955, -60.06485149430999826, 10.42531124854999902 ) ) ;
#11600 = ORIENTED_EDGE ( 'NONE', *, *, #6507, .T. ) ;
#11601 = CARTESIAN_POINT ( 'NONE',  ( -0.2126258756077037404, -79.98878773083430360, 1.232946059365898073 ) ) ;
#11602 = CARTESIAN_POINT ( 'NONE',  ( 4.658475568430802127, -78.16666666666665719, -8.082524092276894834 ) ) ;
#11603 = ADVANCED_FACE ( 'NONE', ( #44728 ), #48956, .F. ) ;
#11604 = CARTESIAN_POINT ( 'NONE',  ( -6.574673376928999780, -78.60377266276799446, 9.148912741538998361 ) ) ;
#11605 = CARTESIAN_POINT ( 'NONE',  ( 2.273403379124000026E-14, -92.33215535459000023, 0.000000000000000000 ) ) ;
#11606 = DIRECTION ( 'NONE',  ( 0.000000000000000000, 0.000000000000000000, -1.000000000000000000 ) ) ;
#11607 = CARTESIAN_POINT ( 'NONE',  ( -9.050966799188000067, -55.64999999964999233, -7.919595949288999570 ) ) ;
#11608 = VECTOR ( 'NONE', #10927, 1000.000000000000000 ) ;
#11609 = CARTESIAN_POINT ( 'NONE',  ( -1.036575664049323109, -82.91414466568171804, -1.099456454985895171 ) ) ;
#11610 = PRODUCT_DEFINITION_SHAPE ( 'NONE', 'NONE',  #49537 ) ;
#11611 = CARTESIAN_POINT ( 'NONE',  ( 0.004531456056113089548, -79.72569806758036748, -1.249755132514873690 ) ) ;
#11612 = ORIENTED_EDGE ( 'NONE', *, *, #24179, .T. ) ;
#11613 = CARTESIAN_POINT ( 'NONE',  ( 1.931086388578000079, -18.70221245812999911, 12.71798269385000069 ) ) ;
#11614 = CARTESIAN_POINT ( 'NONE',  ( 8.414570695956999913, -55.64999999967000122, -8.414570695956999913 ) ) ;
#11615 = VERTEX_POINT ( 'NONE', #39422 ) ;
#11616 = ORIENTED_EDGE ( 'NONE', *, *, #24294, .T. ) ;
#11617 = CARTESIAN_POINT ( 'NONE',  ( -12.48375942314000042, -55.42730665069999674, -1.669542353228000042 ) ) ;
#11618 = VERTEX_POINT ( 'NONE', #39127 ) ;
#11619 = ORIENTED_EDGE ( 'NONE', *, *, #43573, .T. ) ;
#11620 = CARTESIAN_POINT ( 'NONE',  ( 10.01676216527999941, -23.20941515021999635, 7.658899892521000119 ) ) ;
#11621 = TOROIDAL_SURFACE ( 'NONE', #10657, 1.250000000000000000, 0.5000000000000000000 ) ;
#11622 = CARTESIAN_POINT ( 'NONE',  ( 3.906270390259000358, -78.22752942077299565, -10.19392449069000151 ) ) ;
#11623 = ITEM_DEFINED_TRANSFORMATION ( 'NONE', 'NONE', #15026,  #43526 ) ;
#11624 = CARTESIAN_POINT ( 'NONE',  ( -12.99510751537000353, -63.10294702886003648, -6.911973076623003642 ) ) ;
#11625 = B_SPLINE_SURFACE_WITH_KNOTS ( 'NONE', 3, 3, ( 
 ( #30231, #26094, #48274, #29935, #56829, #57402, #7231, #43839, #47988, #21097, #25235, #21381, #16960, #34942, #16676, #57110, #3386, #25521, #20525 ),
 ( #30521, #16099, #11957, #43255, #48552, #8098, #34657, #17238, #47412, #52685, #35225, #53256, #7524, #29364, #34079, #24946, #2523, #20805, #38523 ),
 ( #52115, #11675, #29650, #47701, #38812, #16385, #39963, #21951, #18423, #731, #49725, #8675, #8977, #444, #18711, #36705, #41140, #18130, #4843 ),
 ( #12805, #49125, #23132, #22839, #50015, #17836, #31088, #40852, #36413, #22249, #13385, #26377, #30804, #44396, #48837, #9268, #36125, #3948, #54441 ) ),
 .UNSPECIFIED., .F., .F., .F.,
 ( 4, 4 ),
 ( 4, 1, 1, 1, 1, 1, 1, 1, 1, 1, 1, 1, 1, 1, 1, 1, 4 ),
 ( -0.4045438850609999748, 1.404543885061000141 ),
 ( -0.004592865874913999551, 0.01033394821856000075, 0.02526076231202999817, 0.04018757640548999838, 0.05511439049895999753, 0.07004120459242998975, 0.08496801868589999585, 0.09989483277937000194, 0.1148216468727999984, 0.1297484609662999944, 0.1446752750597999904, 0.1596020891533000141, 0.1745289032467000068, 0.1894557173402000028, 0.2043825314336999988, 0.2193093455270999914, 0.2342361596205999874 ),
 .UNSPECIFIED. ) ;
#11626 = CIRCLE ( 'NONE', #21046, 1.250000000000000000 ) ;
#11627 = CARTESIAN_POINT ( 'NONE',  ( 8.377812017747999107, -79.05173667140100235, 5.294595800518999695 ) ) ;
#11628 = CARTESIAN_POINT ( 'NONE',  ( -2.632720150768073974, -78.20209331882408321, -8.868811374433354544 ) ) ;
#11629 = DIRECTION ( 'NONE',  ( 0.000000000000000000, -1.000000000000000000, 0.000000000000000000 ) ) ;
#11630 = ORIENTED_EDGE ( 'NONE', *, *, #39977, .F. ) ;
#11631 = ORIENTED_EDGE ( 'NONE', *, *, #56709, .F. ) ;
#11632 = CARTESIAN_POINT ( 'NONE',  ( -4.216522652542374239, -77.51279216956007190, 8.232977916204301749 ) ) ;
#11633 = CARTESIAN_POINT ( 'NONE',  ( -12.70228545255361752, -24.82820680358864252, 1.205254117556738169 ) ) ;
#11634 = EDGE_CURVE ( 'NONE', #55458, #36570, #8708, .T. ) ;
#11635 = DIRECTION ( 'NONE',  ( -1.000000000000000000, 0.000000000000000000, 0.000000000000000000 ) ) ;
#11636 = CARTESIAN_POINT ( 'NONE',  ( -7.843978203195000276, -77.78005595245699055, 5.713380375430999969 ) ) ;
#11637 = CARTESIAN_POINT ( 'NONE',  ( 7.655542440070999710, -22.77819125662999866, 10.38645071867999903 ) ) ;
#11638 = CARTESIAN_POINT ( 'NONE',  ( 7.770369683913386893, -61.03583903303879765, 10.20674856006229980 ) ) ;
#11639 = CARTESIAN_POINT ( 'NONE',  ( 2.813789756862274505, -76.64583333333334281, -10.47020627418438821 ) ) ;
#11640 = CARTESIAN_POINT ( 'NONE',  ( -8.838834764832000701, -60.04999999966999980, 8.838834764832000701 ) ) ;
#11641 = CARTESIAN_POINT ( 'NONE',  ( 1.386886761648000066, -79.47070532422000610, -0.9883168548346998872 ) ) ;
#11642 = CARTESIAN_POINT ( 'NONE',  ( -0.6204398466918998878, -82.19746881207100841, -1.165230367032999981 ) ) ;
#11644 = CIRCLE ( 'NONE', #42402, 11.19999999999999929 ) ;
#11643 = CARTESIAN_POINT ( 'NONE',  ( 0.5323558113646862378, -79.40376574649415886, -1.414199531720756298 ) ) ;
#11645 = CARTESIAN_POINT ( 'NONE',  ( -7.675809325333999844, -77.99761332859900165, -6.269164879585000349 ) ) ;
#11646 = CARTESIAN_POINT ( 'NONE',  ( 6.917788961650999546, -78.87567121485298571, -9.780606322222999083 ) ) ;
#11647 = CARTESIAN_POINT ( 'NONE',  ( 1.931087888240000217, -23.31584731985000047, -12.71658872084999992 ) ) ;
#11649 = CARTESIAN_POINT ( 'NONE',  ( 0.2086861075963999945, -78.62815740206998782, 1.317203954600000060 ) ) ;
#11648 = CARTESIAN_POINT ( 'NONE',  ( -0.7554284705563540925, -78.81666666666669130, 1.310679582531384391 ) ) ;
#11650 = CARTESIAN_POINT ( 'NONE',  ( 2.398181734629726503, -79.45434264457517770, 8.953979686625713086 ) ) ;
#11651 = CARTESIAN_POINT ( 'NONE',  ( 0.7222841580580000587, -80.29899131680598146, 11.04814689212999923 ) ) ;
#11652 = CARTESIAN_POINT ( 'NONE',  ( 12.85144117169000033, -20.24527983099999773, 1.980464439859999981 ) ) ;
#11653 = CARTESIAN_POINT ( 'NONE',  ( 0.000000000000000000, -75.20000000000000284, -7.200000000000000178 ) ) ;
#11654 = CARTESIAN_POINT ( 'NONE',  ( 1.657628819186623526, -1.087677343702487587, 3.213874994219929171 ) ) ;
#11655 = ORIENTED_EDGE ( 'NONE', *, *, #54684, .T. ) ;
#11656 = CARTESIAN_POINT ( 'NONE',  ( -2.599125635968795311, -1.549700445914265368, 1.994837577964314601 ) ) ;
#11657 = VECTOR ( 'NONE', #29249, 1000.000000000000000 ) ;
#11658 = DIRECTION ( 'NONE',  ( 1.000000000000000000, 0.000000000000000000, 0.000000000000000000 ) ) ;
#11659 = CARTESIAN_POINT ( 'NONE',  ( 1.242692993603842222, -78.35873442546773049, 0.1364330655704606987 ) ) ;
#11660 = EDGE_CURVE ( 'NONE', #11586, #49814, #56515, .T. ) ;
#11661 = CARTESIAN_POINT ( 'NONE',  ( 3.338062356706000156, -79.80347180386698369, 8.930159145143999666 ) ) ;
#11662 = CARTESIAN_POINT ( 'NONE',  ( 1.407118610985540252, -76.96474581824523398, 10.75041648542711314 ) ) ;
#11663 = FACE_OUTER_BOUND ( 'NONE', #1876, .T. ) ;
#11664 = CARTESIAN_POINT ( 'NONE',  ( 2.839805762151339952, -3.208333333333332149, -1.636761686205418176 ) ) ;
#11665 = VECTOR ( 'NONE', #48965, 1000.000000000000000 ) ;
#11666 = CARTESIAN_POINT ( 'NONE',  ( 9.722718241315000398, -18.75000000000000000, -7.247844507162001015 ) ) ;
#11667 = CIRCLE ( 'NONE', #9761, 2.299999999999999822 ) ;
#11668 = CARTESIAN_POINT ( 'NONE',  ( -4.036611699677500553, -78.62148118236264338, 2.280827005624593617 ) ) ;
#11669 = CARTESIAN_POINT ( 'NONE',  ( 6.514771768986000744, -77.48207916904298997, -8.933413800474999888 ) ) ;
#11670 = ADVANCED_FACE ( 'NONE', ( #12550 ), #5584, .T. ) ;
#11671 = CARTESIAN_POINT ( 'NONE',  ( 11.12972475151000040, -77.95443840457200224, -0.6195381557079999713 ) ) ;
#11672 = CARTESIAN_POINT ( 'NONE',  ( -0.9331672942107464008, -82.04272704394496429, 0.8318759801249889785 ) ) ;
#11673 = DIRECTION ( 'NONE',  ( 0.000000000000000000, 1.000000000000000000, 0.000000000000000000 ) ) ;
#11674 = EDGE_CURVE ( 'NONE', #13177, #56405, #15549, .T. ) ;
#11675 = CARTESIAN_POINT ( 'NONE',  ( -9.555818165766000405, -77.33116456062899147, -0.1257991660602000017 ) ) ;
#11676 = CARTESIAN_POINT ( 'NONE',  ( 1.460959015002472494, -78.77083333333337123, 0.3926218265389233020 ) ) ;
#11677 = CARTESIAN_POINT ( 'NONE',  ( -1.439896632895359962, -77.48541666666666572, 10.99999999999999645 ) ) ;
#11678 = CARTESIAN_POINT ( 'NONE',  ( 0.7554284705563453217, -81.33333333333332860, 1.310679582531389276 ) ) ;
#11679 = CARTESIAN_POINT ( 'NONE',  ( -1.500000000000000000, -80.90000000000000568, 0.000000000000000000 ) ) ;
#11680 = CARTESIAN_POINT ( 'NONE',  ( 8.962230876647016231, -80.15077933492216289, 6.668113489195105714 ) ) ;
#11681 = CARTESIAN_POINT ( 'NONE',  ( 9.785129497364000173, -79.19891811065798493, -6.997026981537000090 ) ) ;
#11682 = CARTESIAN_POINT ( 'NONE',  ( 0.1636246173744642929, -81.86458333333334281, 1.250000000000000888 ) ) ;
#11683 = CARTESIAN_POINT ( 'NONE',  ( -11.25198206936999945, -79.82677595101669965, -0.4763024974861999605 ) ) ;
#11684 = VERTEX_POINT ( 'NONE', #22277 ) ;
#11685 = CARTESIAN_POINT ( 'NONE',  ( 12.50659830422946683, -17.02653389314800947, 0.3508388550761127322 ) ) ;
#11686 = ORIENTED_EDGE ( 'NONE', *, *, #7745, .T. ) ;
#11687 = EDGE_LOOP ( 'NONE', ( #2353, #9119, #45671, #48474, #24208, #16971 ) ) ;
#11688 = CARTESIAN_POINT ( 'NONE',  ( 3.500000000000000000, -3.500000000000000000, 1.049058100190999900E-13 ) ) ;
#11689 = EDGE_CURVE ( 'NONE', #45142, #20811, #24016, .T. ) ;
#11690 = ORIENTED_EDGE ( 'NONE', *, *, #41232, .F. ) ;
#11691 = AXIS2_PLACEMENT_3D ( 'NONE', #39900, #13619, #30744 ) ;
#11692 = CARTESIAN_POINT ( 'NONE',  ( -3.178381252491000009, -80.36598997120898957, -1.569351427020000189 ) ) ;
#11693 = CARTESIAN_POINT ( 'NONE',  ( 3.575328375144039228, -79.24388340919793450, 8.805561371781996272 ) ) ;
#11694 = ORIENTED_EDGE ( 'NONE', *, *, #9288, .F. ) ;
#11695 = CARTESIAN_POINT ( 'NONE',  ( 0.6122205248558478807, -82.76563067023366216, -1.094235436730285116 ) ) ;
#11696 = EDGE_LOOP ( 'NONE', ( #9135, #10962, #34295, #21801 ) ) ;
#11697 = CARTESIAN_POINT ( 'NONE',  ( -9.009247259181922374, -79.52083333333332860, -2.421167930323344653 ) ) ;
#11698 = ORIENTED_EDGE ( 'NONE', *, *, #9568, .F. ) ;
#11699 = CARTESIAN_POINT ( 'NONE',  ( -1.124031593430794063, -79.56385312167009261, 0.5524272544800838958 ) ) ;
#11700 = CARTESIAN_POINT ( 'NONE',  ( -1.455667963173603141, -78.27095469975617448, -0.3934943062302369565 ) ) ;
#11701 = CARTESIAN_POINT ( 'NONE',  ( 0.000000000000000000, -87.70000000000000284, 0.000000000000000000 ) ) ;
#11702 = EDGE_CURVE ( 'NONE', #40725, #54085, #32903, .T. ) ;
#11703 = AXIS2_PLACEMENT_3D ( 'NONE', #37329, #10190, #15188 ) ;
#11704 = CARTESIAN_POINT ( 'NONE',  ( -8.693530819781495111, -80.05018064888071194, 6.323148125732028113 ) ) ;
#11705 = CARTESIAN_POINT ( 'NONE',  ( -9.497876546326999403, -77.25168256874098915, -0.2008509664869000122 ) ) ;
#11706 = CARTESIAN_POINT ( 'NONE',  ( 10.02574878253000001, -76.68821439642898952, 4.955627619753999902 ) ) ;
#11707 = CARTESIAN_POINT ( 'NONE',  ( -7.342331066867000544, -55.64999999967000122, 8.190859204290999784 ) ) ;
#11708 = EDGE_CURVE ( 'NONE', #32124, #33417, #27861, .T. ) ;
#11709 = CARTESIAN_POINT ( 'NONE',  ( -2.251478210889264364, -76.95593248568935962, -9.257098554661395085 ) ) ;
#11710 = CARTESIAN_POINT ( 'NONE',  ( -10.60592548576000027, -76.86996292289100552, 2.886128316406999961 ) ) ;
#11711 = CARTESIAN_POINT ( 'NONE',  ( -3.481545117580455262, -78.69439501636868783, -8.569750538382592708 ) ) ;
#11712 = CARTESIAN_POINT ( 'NONE',  ( -0.2340539085346999837, -80.06715162479200387, 1.312933706406000267 ) ) ;
#11713 = CARTESIAN_POINT ( 'NONE',  ( -10.93151875640478643, -80.10922970060033776, -1.237410007773367404 ) ) ;
#11714 = CARTESIAN_POINT ( 'NONE',  ( -9.252740428349008894, -77.27916666666671119, 2.486604901413127955 ) ) ;
#11715 = CARTESIAN_POINT ( 'NONE',  ( -3.429377950856999924, -78.32128455456849281, 1.098412442743999851 ) ) ;
#11716 = CARTESIAN_POINT ( 'NONE',  ( -9.008069698304732142, -78.05420658299554759, 5.866654319817532937 ) ) ;
#11717 = DIRECTION ( 'NONE',  ( 0.000000000000000000, 1.000000000000000000, 0.000000000000000000 ) ) ;
#11718 = DIRECTION ( 'NONE',  ( -1.000000000000000000, 0.000000000000000000, 0.000000000000000000 ) ) ;
#11719 = CARTESIAN_POINT ( 'NONE',  ( -0.6678581783745000111, -84.42674735065199343, 3.481225250072000232 ) ) ;
#11720 = LINE ( 'NONE', #29696, #45915 ) ;
#11721 = CARTESIAN_POINT ( 'NONE',  ( 10.18589234708000113, -23.28917565320000094, 7.641012386039999882 ) ) ;
#11722 = CARTESIAN_POINT ( 'NONE',  ( -7.634438871678000282, -60.54781730666999806, -10.30764054783999839 ) ) ;
#11723 = CARTESIAN_POINT ( 'NONE',  ( -4.882675258918448336, -79.20818948587456987, 11.01334000465016416 ) ) ;
#11724 = AXIS2_PLACEMENT_3D ( 'NONE', #12270, #53003, #56567 ) ;
#11725 = FACE_OUTER_BOUND ( 'NONE', #32792, .T. ) ;
#11726 = CARTESIAN_POINT ( 'NONE',  ( 1.500000000000000888, -79.23137852148992977, -0.3510066005171250114 ) ) ;
#11727 = CARTESIAN_POINT ( 'NONE',  ( 6.891227191158999510, -76.69101173772000379, -9.824000600561999974 ) ) ;
#11728 = CARTESIAN_POINT ( 'NONE',  ( 10.12290050124000018, -23.24999999991999644, 7.648026767085999822 ) ) ;
#11729 = DIRECTION ( 'NONE',  ( 0.009503199022040095811, 0.000000000000000000, -0.9999548435846228323 ) ) ;
#11730 = CARTESIAN_POINT ( 'NONE',  ( -5.241082234444999877, -75.58422357026000782, -11.04946354059000058 ) ) ;
#11731 = VERTEX_POINT ( 'NONE', #54467 ) ;
#11732 = AXIS2_PLACEMENT_3D ( 'NONE', #37654, #42093, #1663 ) ;
#11733 = CARTESIAN_POINT ( 'NONE',  ( 9.621742410812267110, -54.17938299883542896, -8.060146970871130634 ) ) ;
#11734 = CARTESIAN_POINT ( 'NONE',  ( 12.66761950495000022, -61.02355206165999846, 1.696827901577000031 ) ) ;
#11735 = CARTESIAN_POINT ( 'NONE',  ( 5.973326116064999525, -79.42032643418001214, -10.95954443647000076 ) ) ;
#11736 = CARTESIAN_POINT ( 'NONE',  ( 12.49837451343999994, -55.59042109264999709, -1.667049596277000001 ) ) ;
#11737 = CARTESIAN_POINT ( 'NONE',  ( 2.845884614340000063, -78.04193342313199366, -9.200769029100998253 ) ) ;
#11738 = EDGE_CURVE ( 'NONE', #45641, #24608, #4873, .T. ) ;
#11739 = CARTESIAN_POINT ( 'NONE',  ( -2.666231078231000140, -84.50932768054498467, 3.209013417975999705 ) ) ;
#11740 = CARTESIAN_POINT ( 'NONE',  ( -1.495312310314963478, -79.98653854018940024, 10.64535603553911614 ) ) ;
#11741 = DIRECTION ( 'NONE',  ( 0.000000000000000000, 1.000000000000000000, 0.000000000000000000 ) ) ;
#11742 = ORIENTED_EDGE ( 'NONE', *, *, #49273, .F. ) ;
#11743 = CARTESIAN_POINT ( 'NONE',  ( 10.74995494553095021, -77.34974026310845829, -0.04523175681011006727 ) ) ;
#11744 = CARTESIAN_POINT ( 'NONE',  ( 0.8474260888054412355, -78.91675431682378417, -3.388359286580899354 ) ) ;
#11745 = VERTEX_POINT ( 'NONE', #22579 ) ;
#11746 = CARTESIAN_POINT ( 'NONE',  ( 10.24785796630000156, -78.14927573546698625, 3.830033060943999867 ) ) ;
#11747 = SURFACE_STYLE_FILL_AREA ( #52192 ) ;
#11748 = CARTESIAN_POINT ( 'NONE',  ( -4.043962765326000408, -80.21098163303398110, 10.58371677765999941 ) ) ;
#11749 = ORIENTED_EDGE ( 'NONE', *, *, #44691, .F. ) ;
#11750 = EDGE_LOOP ( 'NONE', ( #46632, #10159, #41888, #4562 ) ) ;
#11751 = ORIENTED_EDGE ( 'NONE', *, *, #50035, .F. ) ;
#11752 = EDGE_CURVE ( 'NONE', #50911, #22487, #31735, .T. ) ;
#11753 = CARTESIAN_POINT ( 'NONE',  ( 0.3984351131076449004, -80.44939689437285324, 1.184687104124929613 ) ) ;
#11754 = ADVANCED_FACE ( 'NONE', ( #5158 ), #40591, .T. ) ;
#11755 = CARTESIAN_POINT ( 'NONE',  ( -3.647699726329999947, -86.17851881790099355, 1.624060543896000075 ) ) ;
#11756 = CARTESIAN_POINT ( 'NONE',  ( -0.5483576180056000116, -79.63083724111049833, -9.751923335751000010 ) ) ;
#11757 = CIRCLE ( 'NONE', #23077, 1.750000000000001332 ) ;
#11758 = ORIENTED_EDGE ( 'NONE', *, *, #49558, .T. ) ;
#11759 = CARTESIAN_POINT ( 'NONE',  ( -12.70249480706781497, -24.96498603299993846, -0.9989402950542592974 ) ) ;
#11760 = ORIENTED_EDGE ( 'NONE', *, *, #39005, .F. ) ;
#11761 = CARTESIAN_POINT ( 'NONE',  ( 0.4532606190057231199, -79.30375411270249231, -1.190852882372544386 ) ) ;
#11762 = CARTESIAN_POINT ( 'NONE',  ( 0.000000000000000000, -74.70999999999999375, 0.000000000000000000 ) ) ;
#11763 = CARTESIAN_POINT ( 'NONE',  ( 10.08162962779999994, -54.08146287347000225, 7.981572332307999673 ) ) ;
#11764 = CARTESIAN_POINT ( 'NONE',  ( 1.460959015002472494, -80.67083333333334849, 0.3926218265389232465 ) ) ;
#11765 = CARTESIAN_POINT ( 'NONE',  ( -0.7554284705563540925, -81.31666666666669130, 1.310679582531384391 ) ) ;
#11766 = CARTESIAN_POINT ( 'NONE',  ( -0.8482561879233938562, -78.93107913613843607, 9.687824124670456172 ) ) ;
#11767 = EDGE_CURVE ( 'NONE', #19797, #9151, #7808, .T. ) ;
#11768 = AXIS2_PLACEMENT_3D ( 'NONE', #10742, #50893, #5138 ) ;
#11769 = CARTESIAN_POINT ( 'NONE',  ( -12.70556836347999941, -16.77227722772000007, 1.774192816106000118E-09 ) ) ;
#11770 = DIRECTION ( 'NONE',  ( -0.7071067811865475727, 0.000000000000000000, 0.7071067811865475727 ) ) ;
#11771 = CARTESIAN_POINT ( 'NONE',  ( -3.646991572042142860, -81.80260418020685620, -1.672477627614840090 ) ) ;
#11772 = B_SPLINE_CURVE_WITH_KNOTS ( 'NONE', 3,
 ( #20794, #29924, #51820, #48538, #30216, #6930, #2510, #34356, #20514, #11374, #38511, #56527, #52104, #11662, #29638, #47691, #43241, #52393, #4829, #39663, #36114, #22236, #3937, #27533 ),
 .UNSPECIFIED., .F., .F.,
 ( 4, 2, 2, 2, 2, 2, 2, 2, 2, 2, 2, 4 ),
 ( 0.000000000000000000, 0.06249999999999995837, 0.1249999999999999167, 0.1874999999999999167, 0.2499999999999999445, 0.3749999999999999445, 0.5000000000000000000, 0.6250000000000000000, 0.7500000000000000000, 0.8750000000000000000, 0.9374999999999998890, 1.000000000000000000 ),
 .UNSPECIFIED. ) ;
#11773 = CARTESIAN_POINT ( 'NONE',  ( -9.662446363796000526, -76.39482503998999618, 7.627099640079999965 ) ) ;
#11774 = CARTESIAN_POINT ( 'NONE',  ( -3.559593837270000005, -80.08782046129100252, 2.176197791817000127 ) ) ;
#11775 = CARTESIAN_POINT ( 'NONE',  ( -9.009247259181927703, -77.97916666666667140, 2.421167930323307793 ) ) ;
#11776 = DIRECTION ( 'NONE',  ( -1.000000000000000000, 0.000000000000000000, 0.000000000000000000 ) ) ;
#11777 = CARTESIAN_POINT ( 'NONE',  ( -9.356096982537000173, -78.92672392741998522, 7.928589704419000128 ) ) ;
#11778 = DIRECTION ( 'NONE',  ( 0.000000000000000000, 1.000000000000000000, 0.000000000000000000 ) ) ;
#11779 = CARTESIAN_POINT ( 'NONE',  ( 9.500000000000001776, -78.66041666666667709, 1.243547092045981239 ) ) ;
#11780 = CARTESIAN_POINT ( 'NONE',  ( 12.56594317823000040, -23.25000001387000026, -1.750000000000000000 ) ) ;
#11781 = LINE ( 'NONE', #7915, #21078 ) ;
#11782 = ADVANCED_FACE ( 'NONE', ( #187 ), #9590, .T. ) ;
#11783 = CARTESIAN_POINT ( 'NONE',  ( 0.3915780857578022855, -81.10420615330434657, 1.460265237947602879 ) ) ;
#11784 = CARTESIAN_POINT ( 'NONE',  ( -8.500000000000000000, -3.500000000000000000, 0.000000000000000000 ) ) ;
#11785 = CARTESIAN_POINT ( 'NONE',  ( 9.250000000000000000, -79.24999999999998579, 0.000000000000000000 ) ) ;
#11786 = CARTESIAN_POINT ( 'NONE',  ( 1.500000000000000000, -78.75000000000000000, 0.000000000000000000 ) ) ;
#11787 = CARTESIAN_POINT ( 'NONE',  ( -3.382079042057999807, -1.966566916551000022, 0.09601839907216000447 ) ) ;
#11788 = CARTESIAN_POINT ( 'NONE',  ( 0.9776138843420000279, -78.07253854425700013, -12.12546088519999898 ) ) ;
#11789 = CARTESIAN_POINT ( 'NONE',  ( -5.702118101738999911, -78.34604234163299452, -7.895919506952999711 ) ) ;
#11791 = LINE ( 'NONE', #48671, #41048 ) ;
#11790 = CARTESIAN_POINT ( 'NONE',  ( 6.586108526242999694, -80.17391735373439587, 8.810401493720998900 ) ) ;
#11792 = CARTESIAN_POINT ( 'NONE',  ( -0.7107282322889000303, -81.16095650773000614, -1.148979047684000054 ) ) ;
#11793 = DIRECTION ( 'NONE',  ( 1.000000000000000000, 0.000000000000000000, 0.000000000000000000 ) ) ;
#11794 = ORIENTED_EDGE ( 'NONE', *, *, #8705, .F. ) ;
#11795 = CARTESIAN_POINT ( 'NONE',  ( -1.500000000000000000, -83.24999999999998579, 0.000000000000000000 ) ) ;
#11796 = CARTESIAN_POINT ( 'NONE',  ( 5.817551787861000356, -79.78979933005598468, -10.15771087481999935 ) ) ;
#11797 = VECTOR ( 'NONE', #37641, 1000.000000000000000 ) ;
#11798 = CARTESIAN_POINT ( 'NONE',  ( 2.308268922230239273, -79.39449714348630494, -9.238196189940964587 ) ) ;
#11799 = CARTESIAN_POINT ( 'NONE',  ( -4.419147127517656592, -79.99999999999998579, -8.303618670951507852 ) ) ;
#11800 = CARTESIAN_POINT ( 'NONE',  ( 0.000000000000000000, -23.25000000000000000, 12.50000000000000000 ) ) ;
#11801 = VECTOR ( 'NONE', #49398, 1000.000000000000000 ) ;
#11802 = CARTESIAN_POINT ( 'NONE',  ( -10.49130490104844604, -80.07586413098869116, 3.306199282034132825 ) ) ;
#11803 = CARTESIAN_POINT ( 'NONE',  ( 9.065614955752000270, -78.93479598044999079, -2.589622044563999914 ) ) ;
#11804 = CARTESIAN_POINT ( 'NONE',  ( -6.043427764450784778, -77.98333333333330586, -10.48543666025109822 ) ) ;
#11805 = CARTESIAN_POINT ( 'NONE',  ( 9.250000000000000000, -79.24999999999998579, 0.000000000000000000 ) ) ;
#11806 = VERTEX_POINT ( 'NONE', #41166 ) ;
#11807 = LINE ( 'NONE', #29781, #20133 ) ;
#11808 = CARTESIAN_POINT ( 'NONE',  ( 3.005800864929102367, -78.90401322919130678, 11.38072746178960237 ) ) ;
#11809 = CARTESIAN_POINT ( 'NONE',  ( 9.546819346421999697, -24.68527546640000025, -8.130850183241999929 ) ) ;
#11811 = CARTESIAN_POINT ( 'NONE',  ( 1.195514927944278050, -81.37427934806251528, 0.3747885264647531356 ) ) ;
#11810 = AXIS2_PLACEMENT_3D ( 'NONE', #23624, #37487, #15643 ) ;
#11812 = CARTESIAN_POINT ( 'NONE',  ( -0.5432945554243000519, -81.48433123016999957, -1.398152719143000100 ) ) ;
#11813 = VERTEX_POINT ( 'NONE', #37023 ) ;
#11814 = CARTESIAN_POINT ( 'NONE',  ( -1.266763334644595895, -78.15884741929295387, -0.1447707219529647815 ) ) ;
#11815 = CARTESIAN_POINT ( 'NONE',  ( -9.051338284747782126, -77.00000000000000000, 2.171493758094802828 ) ) ;
#11816 = CARTESIAN_POINT ( 'NONE',  ( 0.000000000000000000, -74.64999999999999147, 0.000000000000000000 ) ) ;
#11817 = ADVANCED_FACE ( 'NONE', ( #36731 ), #31930, .F. ) ;
#11818 = CARTESIAN_POINT ( 'NONE',  ( 10.71573898357587851, -79.71745869582807131, 2.375027775440368139 ) ) ;
#11819 = CYLINDRICAL_SURFACE ( 'NONE', #42243, 11.00000000000000000 ) ;
#11820 = ORIENTED_EDGE ( 'NONE', *, *, #11589, .F. ) ;
#11821 = ORIENTED_EDGE ( 'NONE', *, *, #32253, .T. ) ;
#11822 = CARTESIAN_POINT ( 'NONE',  ( 8.300816029147002340, -77.44509101131500017, -8.570629797104999170 ) ) ;
#11823 = CARTESIAN_POINT ( 'NONE',  ( 0.06764921458087505557, -78.72558927515626692, -10.74974898025365988 ) ) ;
#11824 = EDGE_LOOP ( 'NONE', ( #22276, #35072, #46194, #20974 ) ) ;
#11825 = CARTESIAN_POINT ( 'NONE',  ( 7.948094694409999050, -17.55965255610999876, 9.636752590488001147 ) ) ;
#11826 = CARTESIAN_POINT ( 'NONE',  ( -7.456940411035866134, -78.79464413336293660, 6.210303333646408852 ) ) ;
#11827 = CARTESIAN_POINT ( 'NONE',  ( 11.44417895085271475, -76.02916666666666856, -3.075537641221520069 ) ) ;
#11828 = CARTESIAN_POINT ( 'NONE',  ( 7.289493654314999738, -77.34176059790999602, -10.52009694070999934 ) ) ;
#11829 = DIRECTION ( 'NONE',  ( -0.7071067811865475727, 0.000000000000000000, 0.7071067811865475727 ) ) ;
#11831 = EDGE_CURVE ( 'NONE', #57912, #44932, #14292, .T. ) ;
#11830 = CYLINDRICAL_SURFACE ( 'NONE', #30572, 11.75000000000000000 ) ;
#11832 = CARTESIAN_POINT ( 'NONE',  ( -2.350111744378833301, -86.12609999968211127, 3.172282531658822791 ) ) ;
#11833 = CARTESIAN_POINT ( 'NONE',  ( -0.2291600886666000092, -78.45728611218200399, -11.06898422383999936 ) ) ;
#11834 = VECTOR ( 'NONE', #48955, 1000.000000000000000 ) ;
#11835 = CARTESIAN_POINT ( 'NONE',  ( -11.05000000000000071, -81.00000000000000000, 0.000000000000000000 ) ) ;
#11836 = ORIENTED_EDGE ( 'NONE', *, *, #21054, .F. ) ;
#11837 = DIRECTION ( 'NONE',  ( 0.000000000000000000, 1.000000000000000000, 0.000000000000000000 ) ) ;
#11838 = ORIENTED_EDGE ( 'NONE', *, *, #55187, .F. ) ;
#11839 = CARTESIAN_POINT ( 'NONE',  ( -3.642272407944000090, -79.71961638910200065, -10.66127506782999923 ) ) ;
#11840 = CARTESIAN_POINT ( 'NONE',  ( 4.552121687394530269, -77.26596116455657182, -8.053328680974594533 ) ) ;
#11841 = CARTESIAN_POINT ( 'NONE',  ( 1.209428572278999914, -79.59100130914399074, 0.7398254253092000354 ) ) ;
#11842 = CARTESIAN_POINT ( 'NONE',  ( 0.1636246173744697330, -83.13541666666665719, -1.249999999999999778 ) ) ;
#11843 = B_SPLINE_CURVE_WITH_KNOTS ( 'NONE', 3,
 ( #17160, #52894, #44036, #30147, #44316, #21872, #34291, #7729, #43754, #47912, #35436, #16883, #53465, #48197, #25443, #44613, #21016, #22166 ),
 .UNSPECIFIED., .F., .F.,
 ( 4, 2, 2, 2, 2, 2, 2, 2, 4 ),
 ( 0.000000000000000000, 0.1250000000000000000, 0.2500000000000000000, 0.3750000000000000000, 0.5000000000000000000, 0.6250000000000000000, 0.7500000000000000000, 0.8750000000000000000, 1.000000000000000000 ),
 .UNSPECIFIED. ) ;
#11844 = FACE_OUTER_BOUND ( 'NONE', #10307, .T. ) ;
#11845 = UNCERTAINTY_MEASURE_WITH_UNIT (LENGTH_MEASURE( 1.000000000000000082E-05 ), #2180, 'distance_accuracy_value', 'NONE');
#11846 = CARTESIAN_POINT ( 'NONE',  ( -0.1190996060027000036, -77.72099286884960634, -1.412746526842000083 ) ) ;
#11847 = DIRECTION ( 'NONE',  ( 0.000000000000000000, 1.000000000000000000, 0.000000000000000000 ) ) ;
#11848 = LINE ( 'NONE', #38118, #2173 ) ;
#11849 = CARTESIAN_POINT ( 'NONE',  ( -1.573065832928000063, -78.80897397612000077, 0.4172852021023999991 ) ) ;
#11850 = EDGE_CURVE ( 'NONE', #39177, #22144, #44210, .T. ) ;
#11851 = DIRECTION ( 'NONE',  ( 0.000000000000000000, 0.000000000000000000, 1.000000000000000000 ) ) ;
#11852 = CARTESIAN_POINT ( 'NONE',  ( -7.624341764943999955, -60.06485149430999826, 10.42531124854999902 ) ) ;
#11853 = CARTESIAN_POINT ( 'NONE',  ( -5.018808260229000062, -78.58054015155998684, -9.843244246394000641 ) ) ;
#11854 = FACE_OUTER_BOUND ( 'NONE', #7175, .T. ) ;
#11855 = EDGE_CURVE ( 'NONE', #56550, #4324, #50072, .T. ) ;
#11856 = LINE ( 'NONE', #54041, #22468 ) ;
#11857 = CARTESIAN_POINT ( 'NONE',  ( 3.433252676588999908, -83.90807560421097833, -0.8929367438167998827 ) ) ;
#11858 = ORIENTED_EDGE ( 'NONE', *, *, #11036, .T. ) ;
#11859 = CARTESIAN_POINT ( 'NONE',  ( -8.599335516584035943, -77.20000000000000284, 6.732869530217218568 ) ) ;
#11860 = CARTESIAN_POINT ( 'NONE',  ( -1.384313526018999818, -80.98373215275999826, -0.4900246725272000003 ) ) ;
#11861 = CARTESIAN_POINT ( 'NONE',  ( -9.369164850722000892, -55.54999999966999980, -7.601397897754999633 ) ) ;
#11862 = CARTESIAN_POINT ( 'NONE',  ( -8.557169117579000783, -77.62779217592600389, -8.383968101560000719 ) ) ;
#11863 = CARTESIAN_POINT ( 'NONE',  ( 10.07627163191000008, -23.24999999688999708, -7.601397897754999633 ) ) ;
#11864 = CARTESIAN_POINT ( 'NONE',  ( 1.496210884224999926, -82.99740586305399859, 0.7325374182646999799 ) ) ;
#11865 = CARTESIAN_POINT ( 'NONE',  ( 1.898611045869317726, -2.079666817341920382, 2.965229623691935767 ) ) ;
#11866 = CARTESIAN_POINT ( 'NONE',  ( 6.669449228234999971, -78.31520194988499384, -7.075468016816000016 ) ) ;
#11867 = CARTESIAN_POINT ( 'NONE',  ( -9.487842642213001554, -77.64981427748799092, -0.8069809344748999358 ) ) ;
#11868 = DIRECTION ( 'NONE',  ( 0.7071067811865475727, 0.000000000000000000, -0.7071067811865475727 ) ) ;
#11869 = CARTESIAN_POINT ( 'NONE',  ( -10.26277353288999983, -78.05427472496999997, -3.721672393288999903 ) ) ;
#11870 = CARTESIAN_POINT ( 'NONE',  ( 9.517603932039000014, -80.81724464549388642, 5.334679179331001109 ) ) ;
#11871 = CARTESIAN_POINT ( 'NONE',  ( -1.051406088259749128, -82.10241491881451736, 0.7198062334868400303 ) ) ;
#11872 = ORIENTED_EDGE ( 'NONE', *, *, #23252, .T. ) ;
#11873 = CARTESIAN_POINT ( 'NONE',  ( 10.99609774599710654, -18.31447404871020268, -0.3135602106693130553 ) ) ;
#11874 = CARTESIAN_POINT ( 'NONE',  ( 1.341570204796000088, -79.46030790634399921, -12.19772931051000064 ) ) ;
#11875 = CARTESIAN_POINT ( 'NONE',  ( 3.992904449609001372, -78.62148118236265759, -1.477225460011499791E-15 ) ) ;
#11876 = CARTESIAN_POINT ( 'NONE',  ( 9.070694317316998934, -78.13394183500699341, 6.598531290616000078 ) ) ;
#11877 = CARTESIAN_POINT ( 'NONE',  ( -7.604423127187000198, -79.80575956708399588, 7.914351627518998455 ) ) ;
#11878 = CARTESIAN_POINT ( 'NONE',  ( -1.481817198881961950, -79.36475258761093698, -0.2847931209667339814 ) ) ;
#11879 = CARTESIAN_POINT ( 'NONE',  ( -0.9935076046995571231, -17.03183812246616213, 12.70250268217020917 ) ) ;
#11880 = EDGE_CURVE ( 'NONE', #43451, #17562, #47369, .T. ) ;
#11881 = CARTESIAN_POINT ( 'NONE',  ( -7.624585833192999651, -77.14761986081299483, -9.463128976555999827 ) ) ;
#11882 = CARTESIAN_POINT ( 'NONE',  ( 11.73235549862695670, -78.45166484604632728, 0.7720932834806667477 ) ) ;
#11883 = CARTESIAN_POINT ( 'NONE',  ( -10.27340958486083089, -60.86161210392388909, 7.712164009451874414 ) ) ;
#11884 = ORIENTED_EDGE ( 'NONE', *, *, #37094, .F. ) ;
#11885 = CARTESIAN_POINT ( 'NONE',  ( -6.167563198928999846, -79.63052105083700383, 9.285244464097999639 ) ) ;
#11886 = CARTESIAN_POINT ( 'NONE',  ( -1.138858729362214106, -80.06622006278557535, 0.5167690694360175252 ) ) ;
#11887 = CARTESIAN_POINT ( 'NONE',  ( -6.760013919724102038, -78.12708333333334565, 8.796335266379953666 ) ) ;
#11888 = AXIS2_PLACEMENT_3D ( 'NONE', #45420, #37119, #14677 ) ;
#11889 = CARTESIAN_POINT ( 'NONE',  ( 1.712298698931000063, -78.10580131689799543, 11.02540857285000087 ) ) ;
#11890 = CARTESIAN_POINT ( 'NONE',  ( -12.60413652834999887, -60.10716934574000447, -1.799502287743000029 ) ) ;
#11891 = LINE ( 'NONE', #16604, #34491 ) ;
#11892 = DIRECTION ( 'NONE',  ( -1.000000000000000000, 0.000000000000000000, 0.000000000000000000 ) ) ;
#11893 = CARTESIAN_POINT ( 'NONE',  ( -1.274260011682852189, -82.39792736663919470, -0.8801008395726741540 ) ) ;
#11894 = CARTESIAN_POINT ( 'NONE',  ( 0.5499219767868982478, -79.76170476781604179, -1.122585114487897773 ) ) ;
#11895 = CIRCLE ( 'NONE', #43946, 3.600000000000000089 ) ;
#11896 = CARTESIAN_POINT ( 'NONE',  ( 1.931087888240000217, -18.68415268018999953, 12.71658872085999903 ) ) ;
#11897 = CARTESIAN_POINT ( 'NONE',  ( -12.77297283014999962, -24.72822696531000020, 1.476112654659999857 ) ) ;
#11898 = ORIENTED_EDGE ( 'NONE', *, *, #48016, .F. ) ;
#11899 = ORIENTED_EDGE ( 'NONE', *, *, #10634, .T. ) ;
#11900 = DIRECTION ( 'NONE',  ( 0.000000000000000000, 1.000000000000000000, 0.000000000000000000 ) ) ;
#11901 = VERTEX_POINT ( 'NONE', #55923 ) ;
#11902 = ORIENTED_EDGE ( 'NONE', *, *, #20588, .F. ) ;
#11903 = CARTESIAN_POINT ( 'NONE',  ( -5.029463238270672321, -80.99999999999998579, -9.703467947973461349 ) ) ;
#11904 = CARTESIAN_POINT ( 'NONE',  ( -9.269928330473998557, -77.02913032869298604, 5.765743207788000646 ) ) ;
#11905 = CARTESIAN_POINT ( 'NONE',  ( -1.199500263597270022, -78.05208333333332860, -0.9218200799623730290 ) ) ;
#11907 = ADVANCED_FACE ( 'NONE', ( #16053 ), #42633, .T. ) ;
#11906 = CARTESIAN_POINT ( 'NONE',  ( -3.098141882180000195, -79.35658667140100420, -9.414028956051998520 ) ) ;
#11908 = CARTESIAN_POINT ( 'NONE',  ( -3.364651265678953340, -78.19549771079697109, -8.616567145014089490 ) ) ;
#11909 = CARTESIAN_POINT ( 'NONE',  ( 9.236725725698626377, -79.26122289752220240, 1.304468322093308652 ) ) ;
#11910 = ORIENTED_EDGE ( 'NONE', *, *, #43490, .F. ) ;
#11912 = EDGE_LOOP ( 'NONE', ( #26826, #37311, #37009 ) ) ;
#11911 = EDGE_CURVE ( 'NONE', #37664, #45201, #5565, .T. ) ;
#11913 = CARTESIAN_POINT ( 'NONE',  ( -6.861508235578342330, -77.54162168376055320, 6.204469612445603133 ) ) ;
#11914 = CARTESIAN_POINT ( 'NONE',  ( -1.821913034590999979E-14, -80.69999999923000189, 0.000000000000000000 ) ) ;
#11915 = FACE_OUTER_BOUND ( 'NONE', #56043, .T. ) ;
#11916 = CARTESIAN_POINT ( 'NONE',  ( -5.351292223237999579, -77.75163212332799390, 8.095330809056001442 ) ) ;
#11917 = CARTESIAN_POINT ( 'NONE',  ( 7.626500777234999973, -23.31584731985000047, 10.35747145892000098 ) ) ;
#11918 = CYLINDRICAL_SURFACE ( 'NONE', #20037, 11.75000000000000000 ) ;
#11919 = CARTESIAN_POINT ( 'NONE',  ( 0.5999999999999999778, -18.84999999999999787, 10.98362417419999915 ) ) ;
#11920 = CARTESIAN_POINT ( 'NONE',  ( 8.693423296916000353, -80.00478354744298315, -7.148151291522000683 ) ) ;
#11921 = CARTESIAN_POINT ( 'NONE',  ( -12.00000000000000000, -23.25000000000000000, 0.000000000000000000 ) ) ;
#11922 = CARTESIAN_POINT ( 'NONE',  ( -0.5837186552087999525, -82.24414371479799968, -1.096265345431000071 ) ) ;
#11923 = EDGE_CURVE ( 'NONE', #1594, #41674, #36657, .T. ) ;
#11924 = B_SPLINE_CURVE_WITH_KNOTS ( 'NONE', 3,
 ( #47053, #6582, #50305, #46766, #10148, #37285 ),
 .UNSPECIFIED., .F., .F.,
 ( 4, 2, 4 ),
 ( 0.000000000000000000, 0.5000000000000000000, 1.000000000000000000 ),
 .UNSPECIFIED. ) ;
#11925 = APPLICATION_CONTEXT ( 'automotive_design' ) ;
#11926 = CARTESIAN_POINT ( 'NONE',  ( -7.618386520025000053, -55.57287536619999457, 10.53495200518000097 ) ) ;
#11927 = CARTESIAN_POINT ( 'NONE',  ( -0.5414817640998000892, -78.56376332859900913, -9.895821147420001296 ) ) ;
#11928 = CARTESIAN_POINT ( 'NONE',  ( -11.06076315227999984, -78.17030901383499497, 4.601693484369000053 ) ) ;
#11929 = CARTESIAN_POINT ( 'NONE',  ( -12.71106812367899330, -61.05135172933366761, 1.717582538852624907 ) ) ;
#11930 = CIRCLE ( 'NONE', #47768, 12.90000000000000036 ) ;
#11932 = CARTESIAN_POINT ( 'NONE',  ( -1.801614160558000055, -18.61347738095000182, -12.59687422887999908 ) ) ;
#11931 = CARTESIAN_POINT ( 'NONE',  ( 2.398305471015380608, -78.45419662550813200, 8.954209520413279222 ) ) ;
#11933 = CARTESIAN_POINT ( 'NONE',  ( 9.500000000000005329, -79.03958333333333997, -1.243547092045939939 ) ) ;
#11934 = CARTESIAN_POINT ( 'NONE',  ( -4.084322113587999681, -80.33425248214398096, 10.29083287403000035 ) ) ;
#11935 = CARTESIAN_POINT ( 'NONE',  ( 8.229676506584999274, -77.63320278771699634, 7.688067972860000765 ) ) ;
#11936 = CARTESIAN_POINT ( 'NONE',  ( -0.7994329013177036147, -3.500000000000000444, 3.166868224362918927 ) ) ;
#11937 = DIRECTION ( 'NONE',  ( 0.000000000000000000, 1.000000000000000000, 0.000000000000000000 ) ) ;
#11938 = AXIS2_PLACEMENT_3D ( 'NONE', #7699, #26275, #25983 ) ;
#11939 = ORIENTED_EDGE ( 'NONE', *, *, #37633, .T. ) ;
#11940 = CARTESIAN_POINT ( 'NONE',  ( 6.436424241555000592, -80.32391735373440156, 8.610165096135999008 ) ) ;
#11941 = CARTESIAN_POINT ( 'NONE',  ( 11.79999999999999893, -18.84999999999999787, 0.000000000000000000 ) ) ;
#11942 = CARTESIAN_POINT ( 'NONE',  ( -12.50745077490000057, -24.99994448286999926, -2.662114616045000020E-09 ) ) ;
#11943 = CARTESIAN_POINT ( 'NONE',  ( 0.4506131419724269116, -78.44581188727093490, 1.166324524794932982 ) ) ;
#11944 = VECTOR ( 'NONE', #22743, 1000.000000000000114 ) ;
#11945 = CARTESIAN_POINT ( 'NONE',  ( -3.316243310697999824, -2.097363918999999743, 1.514716574117999981 ) ) ;
#11946 = CARTESIAN_POINT ( 'NONE',  ( -1.840794636227000014, -80.06647572818799574, -9.354253787032998702 ) ) ;
#11947 = CARTESIAN_POINT ( 'NONE',  ( -12.54901566175999861, -53.79264670667999582, 0.4731578885121000555 ) ) ;
#11948 = FACE_OUTER_BOUND ( 'NONE', #39406, .T. ) ;
#11949 = DIRECTION ( 'NONE',  ( 0.7071067811865475727, 0.000000000000000000, 0.7071067811865475727 ) ) ;
#11950 = LINE ( 'NONE', #7516, #46177 ) ;
#11951 = CARTESIAN_POINT ( 'NONE',  ( 2.322889965704379112, -78.69999999999998863, 4.022071092610017828 ) ) ;
#11952 = CARTESIAN_POINT ( 'NONE',  ( 10.95453373411999998, -77.56775829503899899, 1.498774166161999988 ) ) ;
#11953 = CARTESIAN_POINT ( 'NONE',  ( -0.07779856576520610689, -76.32427321278245813, -11.74963840653824576 ) ) ;
#11954 = CARTESIAN_POINT ( 'NONE',  ( -6.841895596235000099, -78.28127452059300140, -8.800175226803998996 ) ) ;
#11955 = CARTESIAN_POINT ( 'NONE',  ( 0.4123449529901261346, -81.94846309541368612, 1.180275517497846316 ) ) ;
#11956 = CARTESIAN_POINT ( 'NONE',  ( 7.710095619821999868, -21.75064714351000106, 10.18496935396999881 ) ) ;
#11957 = CARTESIAN_POINT ( 'NONE',  ( -9.467475792354999697, -77.25345539031198427, 1.978357023055999919 ) ) ;
#11958 = CARTESIAN_POINT ( 'NONE',  ( -8.082524092276896610, -78.45833333333331439, 4.658475568430797686 ) ) ;
#11959 = B_SPLINE_CURVE_WITH_KNOTS ( 'NONE', 3,
 ( #8901, #44918, #48770, #8314, #82, #19510, #1518, #14773, #18931, #32772 ),
 .UNSPECIFIED., .F., .F.,
 ( 4, 2, 2, 2, 4 ),
 ( 0.000000000000000000, 0.5000000000000091038, 0.6250000000000093259, 0.7500000000000096589, 1.000000000000000000 ),
 .UNSPECIFIED. ) ;
#11960 = CARTESIAN_POINT ( 'NONE',  ( 2.839805762151339952, -2.708333333333331705, -1.636761686205418176 ) ) ;
#11961 = CARTESIAN_POINT ( 'NONE',  ( 6.867301783449541119, -80.28033772753711617, -8.270490925764946155 ) ) ;
#11962 = ADVANCED_FACE ( 'NONE', ( #11059 ), #49881, .T. ) ;
#11963 = CARTESIAN_POINT ( 'NONE',  ( -9.500000000000000000, -77.29999999999999716, 0.000000000000000000 ) ) ;
#11964 = CARTESIAN_POINT ( 'NONE',  ( 10.63577493293750464, -80.12563822179964745, 3.563963872659641652 ) ) ;
#11965 = B_SPLINE_CURVE_WITH_KNOTS ( 'NONE', 3,
 ( #54931, #21946, #26956, #35518, #44987, #4542, #23350, #13380, #40255, #21664, #53846, #3381, #35818, #14483, #30516, #41361, #943, #8374, #44692, #22244, #53546, #16955, #43833, #58267, #39958, #44112, #32474, #50519, #21374, #17232, #34936, #3662, #17831, #52969, #39669, #57676, #35221, #13085, #31082, #53250, #12801, #30800, #44391, #49119, #3943, #57971, #8670, #26658, #51108, #37210, #24513, #46689, #41650, #24223, #20096, #32767, #33361, #1514, #46101, #42240, #1807, #42529, #14769, #37796, #19503, #19802, #6504, #38084, #55817, #2098, #55519, #41942, #55222, #56108, #10357, #28054, #15369, #15066, #10951, #51395, #5625, #37498, #33061, #23636, #28932, #46976, #1227, #19218, #50814, #28340, #46392, #5917, #23924, #10661, #28639, #6209, #5237, #50710, #40962, #37101, #27067, #54545, #23528, #41540, #9963, #50413, #18819, #259, #32371, #39568, #14371, #55118, #49534, #27944, #1122, #27367, #23242, #41249, #32084, #54830, #57569, #837, #18531, #22659, #45992, #5519, #21560, #54255, #19110 ),
 .UNSPECIFIED., .F., .F.,
 ( 4, 2, 2, 2, 2, 2, 1, 2, 2, 2, 2, 2, 2, 2, 2, 2, 2, 1, 2, 2, 1, 1, 2, 2, 1, 2, 2, 1, 2, 2, 2, 2, 2, 2, 2, 1, 2, 2, 2, 2, 2, 2, 2, 1, 2, 2, 1, 2, 2, 1, 1, 2, 2, 1, 2, 2, 2, 2, 2, 2, 2, 2, 2, 2, 1, 2, 2, 2, 2, 2, 4 ),
 ( 0.000000000000000000, 0.01562499999999993755, 0.03124999999999987510, 0.04687499999999981265, 0.06249999999999975020, 0.07812499999999969469, 0.09374999999999963918, 0.1093749999999995837, 0.1249999999999995282, 0.1406249999999994726, 0.1562499999999993894, 0.1718749999999993339, 0.1874999999999992784, 0.2031249999999992228, 0.2187499999999991396, 0.2343749999999990841, 0.2421874999999990563, 0.2499999999999990563, 0.2656249999999990008, 0.2734374999999989453, 0.2812499999999989453, 0.2968749999999989453, 0.3046874999999988898, 0.3124999999999988343, 0.3281249999999988343, 0.3359374999999988343, 0.3437499999999987788, 0.3593749999999987788, 0.3671874999999988343, 0.3749999999999988343, 0.3906249999999988343, 0.4062499999999988343, 0.4218749999999988343, 0.4374999999999987788, 0.4687499999999987788, 0.4999999999999987788, 0.5312499999999987788, 0.5624999999999987788, 0.5781249999999987788, 0.5937499999999988898, 0.6093749999999988898, 0.6249999999999988898, 0.6328124999999988898, 0.6406249999999988898, 0.6562499999999988898, 0.6640624999999988898, 0.6718749999999988898, 0.6874999999999988898, 0.6953124999999988898, 0.7031249999999988898, 0.7187499999999988898, 0.7265624999999990008, 0.7343749999999991118, 0.7499999999999991118, 0.7578124999999992228, 0.7656249999999992228, 0.7812499999999993339, 0.7968749999999993339, 0.8124999999999994449, 0.8281249999999994449, 0.8437499999999995559, 0.8593749999999995559, 0.8749999999999995559, 0.8906249999999996669, 0.9062499999999996669, 0.9218749999999997780, 0.9374999999999997780, 0.9531249999999998890, 0.9687499999999998890, 0.9843750000000000000, 1.000000000000000000 ),
 .UNSPECIFIED. ) ;
#11966 = CARTESIAN_POINT ( 'NONE',  ( 10.52307592342000042, -79.35635755647699341, 5.828552047478999576 ) ) ;
#11967 = CARTESIAN_POINT ( 'NONE',  ( -0.6292628992211932726, -78.18342697397770280, -1.092251993020334044 ) ) ;
#11968 = CARTESIAN_POINT ( 'NONE',  ( 10.67847671903000162, -80.09913938103490239, 3.578272902691999491 ) ) ;
#11969 = CARTESIAN_POINT ( 'NONE',  ( -11.00000000000000000, -23.75000000000000000, 0.000000000000000000 ) ) ;
#11970 = ORIENTED_EDGE ( 'NONE', *, *, #32409, .T. ) ;
#11971 = CARTESIAN_POINT ( 'NONE',  ( 12.50386430100449076, -17.21495444376988360, 0.8574445000318078325 ) ) ;
#11972 = VERTEX_POINT ( 'NONE', #15473 ) ;
#11973 = CIRCLE ( 'NONE', #15725, 11.19999999999999929 ) ;
#11974 = VERTEX_POINT ( 'NONE', #51502 ) ;
#11975 = FACE_OUTER_BOUND ( 'NONE', #104, .T. ) ;
#11976 = ORIENTED_EDGE ( 'NONE', *, *, #29217, .T. ) ;
#11977 = CARTESIAN_POINT ( 'NONE',  ( -3.410021335790000219, -78.72256750329937347, 0.4933396517058999398 ) ) ;
#11978 = CARTESIAN_POINT ( 'NONE',  ( 3.065954117407362123, -79.24853233248634865, 8.991551369834709817 ) ) ;
#11979 = ORIENTED_EDGE ( 'NONE', *, *, #39787, .T. ) ;
#11980 = CARTESIAN_POINT ( 'NONE',  ( 0.3746329102212312967, -82.74941308002549079, -1.192428859071045899 ) ) ;
#11981 = CIRCLE ( 'NONE', #43121, 0.5000000000000006661 ) ;
#11982 = LINE ( 'NONE', #18364, #5185 ) ;
#11984 = EDGE_CURVE ( 'NONE', #22563, #10870, #48034, .T. ) ;
#11983 = ORIENTED_EDGE ( 'NONE', *, *, #57105, .T. ) ;
#11985 = CARTESIAN_POINT ( 'NONE',  ( 0.8142187701153039692, -79.41871938336271342, 0.9486283461955962171 ) ) ;
#11986 = CARTESIAN_POINT ( 'NONE',  ( -1.133755312681792971, -78.69107945759728295, 1.029799983678180819 ) ) ;
#11987 = AXIS2_PLACEMENT_3D ( 'NONE', #57683, #4254, #8979 ) ;
#11988 = CARTESIAN_POINT ( 'NONE',  ( -12.50000000000000000, -60.04999999725999515, 1.750000000000000000 ) ) ;
#11989 = CARTESIAN_POINT ( 'NONE',  ( -10.51332871484163789, -80.08341230348659678, 2.247839838564814396 ) ) ;
#11990 = CARTESIAN_POINT ( 'NONE',  ( -7.000000000000000000, -81.19999999999998863, 0.000000000000000000 ) ) ;
#11991 = CARTESIAN_POINT ( 'NONE',  ( 0.4177402061725503657, -86.25171435493597016, -3.969220662749826545 ) ) ;
#11992 = CARTESIAN_POINT ( 'NONE',  ( -10.85772169724999969, -76.88886993234198997, 1.763485056683000041 ) ) ;
#11993 = CARTESIAN_POINT ( 'NONE',  ( -11.66766085128260677, -79.11458333336996418, 2.485230469016839194 ) ) ;
#11994 = CARTESIAN_POINT ( 'NONE',  ( -0.9882926363948538739, -79.54166666776707473, -9.458333340432636405 ) ) ;
#11995 = CARTESIAN_POINT ( 'NONE',  ( -10.79004770952999870, -76.87832357022099927, 1.752493610282999992 ) ) ;
#11996 = EDGE_CURVE ( 'NONE', #41515, #18786, #2480, .T. ) ;
#11997 = CARTESIAN_POINT ( 'NONE',  ( -4.000000000000000000, -76.79999999999999716, 0.000000000000000000 ) ) ;
#11998 = CARTESIAN_POINT ( 'NONE',  ( 10.69999999999999929, -76.39999999999999147, 0.000000000000000000 ) ) ;
#11999 = CARTESIAN_POINT ( 'NONE',  ( -2.304930700997001924, -3.038123778412107789, 2.290893979963799953 ) ) ;
#12000 = CARTESIAN_POINT ( 'NONE',  ( -1.861195093537999945, -79.64403455456849201, 3.263022358706999970 ) ) ;
#12001 = CARTESIAN_POINT ( 'NONE',  ( -4.122653348105549398, -78.00633941627575041, 9.928033855777968597 ) ) ;
#12002 = CARTESIAN_POINT ( 'NONE',  ( 0.000000000000000000, -87.20000000000000284, 0.000000000000000000 ) ) ;
#12003 = CARTESIAN_POINT ( 'NONE',  ( 3.235133317747000081, -82.35352836652198505, -1.192150282569000019 ) ) ;
#12004 = CARTESIAN_POINT ( 'NONE',  ( -8.358306106603231811, -76.26144349183930160, -8.257935116388701147 ) ) ;
#12005 = CARTESIAN_POINT ( 'NONE',  ( 12.00000000000000000, -55.54999999966999980, -1.250000000000000000 ) ) ;
#12006 = CARTESIAN_POINT ( 'NONE',  ( -9.101516360845000264, -61.68066799025999813, -8.485522730771000610 ) ) ;
#12007 = CARTESIAN_POINT ( 'NONE',  ( 5.462882135474436573, -79.13756601347041908, 10.73736906863111251 ) ) ;
#12008 = CARTESIAN_POINT ( 'NONE',  ( -1.460959015002473382, -77.52083333333332860, -0.3926218265389205819 ) ) ;
#12009 = CARTESIAN_POINT ( 'NONE',  ( 12.50412681318975139, -54.28010473027887173, 1.235016000149061322 ) ) ;
#12010 = CARTESIAN_POINT ( 'NONE',  ( 12.56884868898000107, -76.78118304535000505, -3.366471670097000324 ) ) ;
#12011 = AXIS2_PLACEMENT_3D ( 'NONE', #12565, #17279, #35269 ) ;
#12012 = CARTESIAN_POINT ( 'NONE',  ( -1.066991882994506646, -79.46378521489916125, -1.111185832896742998 ) ) ;
#12013 = CARTESIAN_POINT ( 'NONE',  ( 1.750000000001000089, -23.24999998674999802, -12.56594318051000059 ) ) ;
#12014 = CARTESIAN_POINT ( 'NONE',  ( 11.57190666824999958, -76.81145138379000059, -2.972430358477000212 ) ) ;
#12015 = ORIENTED_EDGE ( 'NONE', *, *, #38636, .T. ) ;
#12016 = DIRECTION ( 'NONE',  ( 0.000000000000000000, 0.8191944459061824002, -0.5735158758015881375 ) ) ;
#12017 = CARTESIAN_POINT ( 'NONE',  ( 3.140027144888999810, -85.94828564506399005, -1.398030157551999997 ) ) ;
#12018 = CARTESIAN_POINT ( 'NONE',  ( 12.77657007944999989, -62.11210281297999813, 0.1589025507403999948 ) ) ;
#12019 = CARTESIAN_POINT ( 'NONE',  ( 2.583815929080000018, -78.94027611781000076, 12.52952761449999919 ) ) ;
#12020 = CARTESIAN_POINT ( 'NONE',  ( 12.82229880955999946, -55.37735182805000278, -2.065917129154000165 ) ) ;
#12021 = CARTESIAN_POINT ( 'NONE',  ( -1.535759092668000036, -78.84482872126899622, 9.397436897434999992 ) ) ;
#12022 = AXIS2_PLACEMENT_3D ( 'NONE', #42957, #47112, #2511 ) ;
#12023 = CARTESIAN_POINT ( 'NONE',  ( -0.7861846466844000236, -84.38907726527799014, 4.097373424592999136 ) ) ;
#12024 = CARTESIAN_POINT ( 'NONE',  ( 4.982545483063324454, -79.93680840925433984, 9.528384401333727993 ) ) ;
#12025 = CARTESIAN_POINT ( 'NONE',  ( -0.7332490996008999007, -80.07943159551300027, -1.438596428395999993 ) ) ;
#12026 = ORIENTED_EDGE ( 'NONE', *, *, #9639, .T. ) ;
#12027 = EDGE_CURVE ( 'NONE', #10154, #9880, #36035, .T. ) ;
#12028 = CARTESIAN_POINT ( 'NONE',  ( 1.356641013456250544, -82.10677083333045800, 0.3654621275246989209 ) ) ;
#12029 = CONICAL_SURFACE ( 'NONE', #43185, 12.84999999993999964, 0.7853981633972997312 ) ;
#12030 = CARTESIAN_POINT ( 'NONE',  ( 3.399999999999725020, -78.69999999999998863, -4.163799117100664307E-16 ) ) ;
#12031 = ORIENTED_EDGE ( 'NONE', *, *, #24078, .T. ) ;
#12032 = EDGE_CURVE ( 'NONE', #30887, #456, #38127, .T. ) ;
#12033 = CARTESIAN_POINT ( 'NONE',  ( 0.1286847231337999997, -79.24487755444098980, 10.93943584368999922 ) ) ;
#12034 = CARTESIAN_POINT ( 'NONE',  ( -10.12290050126000196, -60.04999999958999979, -7.648026767103999646 ) ) ;
#12035 = CARTESIAN_POINT ( 'NONE',  ( -8.309722314488999118, -79.75160881430899451, 6.932476156777000575 ) ) ;
#12036 = ORIENTED_EDGE ( 'NONE', *, *, #21142, .T. ) ;
#12037 = CARTESIAN_POINT ( 'NONE',  ( 9.846943056836000352, -78.89225416815600056, -6.945033154232000072 ) ) ;
#12038 = ORIENTED_EDGE ( 'NONE', *, *, #55014, .T. ) ;
#12039 = ORIENTED_EDGE ( 'NONE', *, *, #18169, .F. ) ;
#12040 = CARTESIAN_POINT ( 'NONE',  ( 0.5488453404877545738, -80.43885426786198423, 1.123841912394225817 ) ) ;
#12041 = CARTESIAN_POINT ( 'NONE',  ( -5.913030101731338917, -78.11524859537807686, 10.26283145188432044 ) ) ;
#12042 = CARTESIAN_POINT ( 'NONE',  ( -9.387315177295000979, -80.10788932539801976, 2.697965643110000311 ) ) ;
#12043 = ORIENTED_EDGE ( 'NONE', *, *, #27695, .F. ) ;
#12045 = EDGE_CURVE ( 'NONE', #45320, #11731, #29121, .T. ) ;
#12044 = ORIENTED_EDGE ( 'NONE', *, *, #21142, .F. ) ;
#12046 = CARTESIAN_POINT ( 'NONE',  ( -1.099193429257143029, -79.19244373973189965, -0.6451977031882378810 ) ) ;
#12047 = CARTESIAN_POINT ( 'NONE',  ( -0.03561181053916687156, -78.99318692756679638, -3.778384671869483125 ) ) ;
#12048 = CARTESIAN_POINT ( 'NONE',  ( 9.996785040876998707, -54.64937852858999889, 7.758588586516999008 ) ) ;
#12049 = CYLINDRICAL_SURFACE ( 'NONE', #53431, 1.750000000000001332 ) ;
#12050 = CARTESIAN_POINT ( 'NONE',  ( -1.500000000000000000, -78.39999999999999147, 0.000000000000000000 ) ) ;
#12051 = CARTESIAN_POINT ( 'NONE',  ( -0.6472720423598817829, -77.92942913613843814, 9.703421317447949335 ) ) ;
#12052 = CARTESIAN_POINT ( 'NONE',  ( 12.70619440583160475, -61.26151788282474087, -1.571771935831642653 ) ) ;
#12053 = CARTESIAN_POINT ( 'NONE',  ( -1.105309719138173108, -77.91022932963348069, -1.053953978756914101 ) ) ;
#12054 = ADVANCED_FACE ( 'NONE', ( #26047 ), #15943, .F. ) ;
#12055 = CARTESIAN_POINT ( 'NONE',  ( 11.00000000000000355, -79.83958333333332291, -1.439896632895299566 ) ) ;
#12056 = CARTESIAN_POINT ( 'NONE',  ( 5.894077591580000330, -76.61273252672999945, -10.80721126921000064 ) ) ;
#12057 = EDGE_CURVE ( 'NONE', #37150, #50613, #53648, .T. ) ;
#12058 = CARTESIAN_POINT ( 'NONE',  ( -3.197906501122000034, -78.88532046129088826, -2.679581358368999577 ) ) ;
#12059 = CARTESIAN_POINT ( 'NONE',  ( 4.248461405734000884, -77.98106001420198652, -8.911888886500999973 ) ) ;
#12060 = CARTESIAN_POINT ( 'NONE',  ( 0.7681833999686413783, -83.32291666666667140, 0.9995835529977274980 ) ) ;
#12061 = CARTESIAN_POINT ( 'NONE',  ( 8.438902753042999194, -78.63339079806000598, -8.898539530003999332 ) ) ;
#12062 = CARTESIAN_POINT ( 'NONE',  ( 8.174587033571999228, -77.18454464919399527, -8.440297792765999674 ) ) ;
#12063 = DIRECTION ( 'NONE',  ( 0.000000000000000000, 0.000000000000000000, -1.000000000000000000 ) ) ;
#12064 = CARTESIAN_POINT ( 'NONE',  ( 12.50240681834000078, -24.68234730741999883, -1.005418943851999813 ) ) ;
#12065 = DIRECTION ( 'NONE',  ( 0.000000000000000000, 1.000000000000000000, 0.000000000000000000 ) ) ;
#12066 = CARTESIAN_POINT ( 'NONE',  ( 0.7537979459027094320, -80.41593265530910628, -1.352198804742777760 ) ) ;
#12067 = CARTESIAN_POINT ( 'NONE',  ( 9.035852695838000770, -77.23166978779399017, 2.902309323059000246 ) ) ;
#12068 = FACE_OUTER_BOUND ( 'NONE', #8123, .T. ) ;
#12069 = LINE ( 'NONE', #43658, #7775 ) ;
#12070 = CARTESIAN_POINT ( 'NONE',  ( -3.389826679555999700, -1.914953706142999978, -1.517104093797000175 ) ) ;
#12071 = CARTESIAN_POINT ( 'NONE',  ( 0.4872551020249000220, -77.38064477680499920, 12.03986520427999984 ) ) ;
#12072 = CARTESIAN_POINT ( 'NONE',  ( 5.949632932387999951, -77.94810873382799343, -7.711132450962999485 ) ) ;
#12073 = EDGE_CURVE ( 'NONE', #39893, #53803, #34326, .T. ) ;
#12075 = CARTESIAN_POINT ( 'NONE',  ( 0.2064441143900000164, -78.60443884411000681, 1.303052737963999785 ) ) ;
#12074 = CARTESIAN_POINT ( 'NONE',  ( -11.74961884786346467, -76.19396137550481285, 0.7978361957832171836 ) ) ;
#12076 = CARTESIAN_POINT ( 'NONE',  ( 0.6445170026176001432, -81.98218377781998356, 1.319487011787000119 ) ) ;
#12077 = DIRECTION ( 'NONE',  ( 0.000000000000000000, -1.000000000000000000, 0.000000000000000000 ) ) ;
#12078 = ORIENTED_EDGE ( 'NONE', *, *, #58361, .F. ) ;
#12079 = CARTESIAN_POINT ( 'NONE',  ( -10.01332844637000008, -18.71943307332999851, -7.654537085030999499 ) ) ;
#12080 = CARTESIAN_POINT ( 'NONE',  ( 8.185807787635999588, -79.00525020734799853, 8.524724615276998207 ) ) ;
#12081 = CARTESIAN_POINT ( 'NONE',  ( 7.875215672226593355, -79.45217620423241556, -5.395709537963816693 ) ) ;
#12082 = CARTESIAN_POINT ( 'NONE',  ( 5.462937134022767260, -79.73749999999996874, 10.72588375220489887 ) ) ;
#12083 = CARTESIAN_POINT ( 'NONE',  ( -7.762981007074000850, -60.96089459184000248, 9.992000916374999875 ) ) ;
#12084 = CARTESIAN_POINT ( 'NONE',  ( -1.626826133776999786E-14, -74.80000000000001137, 0.000000000000000000 ) ) ;
#12085 = CARTESIAN_POINT ( 'NONE',  ( 4.175433224444000224, -79.04683895522299508, 8.844688580446998571 ) ) ;
#12086 = DIRECTION ( 'NONE',  ( 0.7071067811865475727, 0.000000000000000000, -0.7071067811865475727 ) ) ;
#12087 = CARTESIAN_POINT ( 'NONE',  ( -12.71466563513548209, -54.66210710670594608, -1.778810201849397643 ) ) ;
#12088 = ORIENTED_EDGE ( 'NONE', *, *, #10305, .F. ) ;
#12089 = LINE ( 'NONE', #50745, #42766 ) ;
#12090 = CARTESIAN_POINT ( 'NONE',  ( -9.991034349598352904, -79.00462831674920494, 6.345779858256005213 ) ) ;
#12091 = CARTESIAN_POINT ( 'NONE',  ( 9.612200201122000465, -79.55766001420199984, -1.584397442130999867 ) ) ;
#12092 = CONICAL_SURFACE ( 'NONE', #14905, 1.099999997148999986, 0.7853981633972997312 ) ;
#12093 = EDGE_CURVE ( 'NONE', #6883, #54081, #26289, .T. ) ;
#12094 = CARTESIAN_POINT ( 'NONE',  ( -10.01235002625000092, -60.09848884406000025, -7.653559626114000203 ) ) ;
#12095 = CARTESIAN_POINT ( 'NONE',  ( -0.3164372427141999844, -79.71981609832999993, 1.635583079321000000 ) ) ;
#12096 = ORIENTED_EDGE ( 'NONE', *, *, #41105, .T. ) ;
#12097 = DIRECTION ( 'NONE',  ( 0.000000000000000000, -1.000000000000000000, -1.983598470663000190E-13 ) ) ;
#12098 = CARTESIAN_POINT ( 'NONE',  ( 0.000000000000000000, -74.99999999999998579, 0.000000000000000000 ) ) ;
#12099 = CARTESIAN_POINT ( 'NONE',  ( 1.931086388455000025, -55.50221404479999876, -12.71798280852999952 ) ) ;
#12100 = AXIS2_PLACEMENT_3D ( 'NONE', #17730, #3285, #57297 ) ;
#12101 = CARTESIAN_POINT ( 'NONE',  ( -0.3271848554491046945, -78.39583333333328596, 1.217465845835393301 ) ) ;
#12102 = CARTESIAN_POINT ( 'NONE',  ( 12.70610308055456805, -54.34479009114169656, -1.580620443402273256 ) ) ;
#12103 = ORIENTED_EDGE ( 'NONE', *, *, #53036, .F. ) ;
#12104 = ORIENTED_EDGE ( 'NONE', *, *, #56073, .F. ) ;
#12105 = CARTESIAN_POINT ( 'NONE',  ( -12.47961470992000166, -76.81611152454399871, 1.652929733484999941 ) ) ;
#12106 = CARTESIAN_POINT ( 'NONE',  ( 0.3551920607923636508, -78.72769057884195831, -10.74440567796370694 ) ) ;
#12107 = CARTESIAN_POINT ( 'NONE',  ( 0.8706374436944001038, -77.82080235332999507, -1.123568498160000040 ) ) ;
#12108 = ORIENTED_EDGE ( 'NONE', *, *, #50852, .F. ) ;
#12109 = FACE_OUTER_BOUND ( 'NONE', #52758, .T. ) ;
#12110 = DIRECTION ( 'NONE',  ( 0.000000000000000000, -1.000000000000000000, 0.000000000000000000 ) ) ;
#12111 = CARTESIAN_POINT ( 'NONE',  ( 0.8898229089104329192, -53.77675468782315704, 12.70296869040592824 ) ) ;
#12112 = CARTESIAN_POINT ( 'NONE',  ( -12.91020013338000005, -77.08816582529999550, -1.090565897604000023 ) ) ;
#12113 = DIRECTION ( 'NONE',  ( 1.000000000000000000, 0.000000000000000000, 0.000000000000000000 ) ) ;
#12114 = FACE_OUTER_BOUND ( 'NONE', #53515, .T. ) ;
#12115 = CARTESIAN_POINT ( 'NONE',  ( 0.3926218265389159190, -79.85416666666668561, 1.460959015002474715 ) ) ;
#12116 = CARTESIAN_POINT ( 'NONE',  ( 8.645668071321999548, -78.70665028547099951, 7.146365085715999044 ) ) ;
#12117 = CARTESIAN_POINT ( 'NONE',  ( 0.9519614230518689268, -79.96731120637714696, 9.201533066724445931 ) ) ;
#12118 = ORIENTED_EDGE ( 'NONE', *, *, #4638, .T. ) ;
#12119 = DIRECTION ( 'NONE',  ( -1.000000000000000000, 0.000000000000000000, 0.000000000000000000 ) ) ;
#12120 = ORIENTED_EDGE ( 'NONE', *, *, #44213, .T. ) ;
#12121 = CARTESIAN_POINT ( 'NONE',  ( -5.117553686986000550, -78.70829163312599519, -10.03691081092000026 ) ) ;
#12122 = CARTESIAN_POINT ( 'NONE',  ( 6.565127467646830972, -77.28787814322510030, -6.516269025712384533 ) ) ;
#12123 = CARTESIAN_POINT ( 'NONE',  ( -0.7681833999686432657, -83.07291666666667140, -0.9995835529977258327 ) ) ;
#12124 = CARTESIAN_POINT ( 'NONE',  ( 11.01657791821742371, -77.11497476844333221, 2.111070802985992589 ) ) ;
#12125 = CARTESIAN_POINT ( 'NONE',  ( -1.287313221243000072, -78.06828123251710849, 0.5940404451740000091 ) ) ;
#12126 = CARTESIAN_POINT ( 'NONE',  ( -7.970414252720478210, -61.32292089011284730, -9.713036876910228656 ) ) ;
#12127 = AXIS2_PLACEMENT_3D ( 'NONE', #41843, #24423, #46294 ) ;
#12128 = CARTESIAN_POINT ( 'NONE',  ( 1.250000000000000000, -81.74999999999998579, 0.000000000000000000 ) ) ;
#12129 = CARTESIAN_POINT ( 'NONE',  ( 0.000000000000000000, -0.2000000000000000111, 0.000000000000000000 ) ) ;
#12130 = DIRECTION ( 'NONE',  ( 0.000000000000000000, 1.000000000000000000, 0.000000000000000000 ) ) ;
#12131 = CARTESIAN_POINT ( 'NONE',  ( -7.653559626096999580, -23.29848884437999956, 10.01235002622999914 ) ) ;
#12132 = CARTESIAN_POINT ( 'NONE',  ( -7.138937464960999790, -79.48718652232298609, 8.574798629027000629 ) ) ;
#12133 = CARTESIAN_POINT ( 'NONE',  ( 10.18491068059999805, -23.30716934606000024, -7.640030139755999983 ) ) ;
#12134 = CARTESIAN_POINT ( 'NONE',  ( 2.121761250100177243, -79.78927564072810696, -11.65386660924905549 ) ) ;
#12135 = CARTESIAN_POINT ( 'NONE',  ( 0.000000000000000000, -87.20000000000000284, 0.000000000000000000 ) ) ;
#12136 = CARTESIAN_POINT ( 'NONE',  ( 0.000000000000000000, -79.99999999999998579, 0.000000000000000000 ) ) ;
#12137 = ORIENTED_EDGE ( 'NONE', *, *, #23673, .T. ) ;
#12138 = CARTESIAN_POINT ( 'NONE',  ( -1.512180334517000180, -83.36904964980398347, 0.4761993468540999808 ) ) ;
#12139 = CARTESIAN_POINT ( 'NONE',  ( -1.348464306027999937, -81.48900587363999648, -0.5807621341562000383 ) ) ;
#12140 = CARTESIAN_POINT ( 'NONE',  ( 10.74972511287136534, -79.34491661344335967, -0.7035994354972746612 ) ) ;
#12141 = CARTESIAN_POINT ( 'NONE',  ( -1.835125225091999823, -77.95334396101199559, 11.83842809849000055 ) ) ;
#12142 = CARTESIAN_POINT ( 'NONE',  ( 1.250000000000000000, -81.34999999999999432, 0.000000000000000000 ) ) ;
#12143 = CARTESIAN_POINT ( 'NONE',  ( 0.3958579896396000608, -81.35526627018998624, -1.618315812554999900 ) ) ;
#12144 = AXIS2_PLACEMENT_3D ( 'NONE', #7040, #44145, #39421 ) ;
#12145 = CARTESIAN_POINT ( 'NONE',  ( -3.506641315871922071, -2.242507564398121822, 0.3302723819864074595 ) ) ;
#12146 = CARTESIAN_POINT ( 'NONE',  ( 4.495978696100999983, -77.96680194988499579, 8.621246072682998474 ) ) ;
#12147 = CARTESIAN_POINT ( 'NONE',  ( 8.085542028362999289, -77.84878108138998698, -5.029352477166999513 ) ) ;
#12149 = ADVANCED_FACE ( 'NONE', ( #16347 ), #27638, .F. ) ;
#12148 = CARTESIAN_POINT ( 'NONE',  ( 0.4436071767293376378, -81.25405316505460007, -1.168520871849203946 ) ) ;
#12150 = CARTESIAN_POINT ( 'NONE',  ( 7.624341766647000362, -18.73514853758999976, -10.42531125024999916 ) ) ;
#12151 = CARTESIAN_POINT ( 'NONE',  ( 9.879208005528543168, -75.99548624166914124, 6.361455101744899032 ) ) ;
#12152 = CARTESIAN_POINT ( 'NONE',  ( -0.8056434147970419346, -81.72077935434506912, -0.9882239605117585368 ) ) ;
#12153 = ORIENTED_EDGE ( 'NONE', *, *, #30745, .F. ) ;
#12154 = CARTESIAN_POINT ( 'NONE',  ( -9.250000000000000000, -78.99999999999998579, 0.000000000000000000 ) ) ;
#12155 = DIRECTION ( 'NONE',  ( 0.000000000000000000, 0.000000000000000000, 1.000000000000000000 ) ) ;
#12156 = CARTESIAN_POINT ( 'NONE',  ( 3.992904449609000483, -78.62148118236265759, -2.356505974700060513 ) ) ;
#12157 = CARTESIAN_POINT ( 'NONE',  ( -1.458706046781999888, -81.78949499347999108, 0.8046341008317999810 ) ) ;
#12158 = CARTESIAN_POINT ( 'NONE',  ( 10.75916580684000046, -78.10670549200499124, 3.171507801093999657 ) ) ;
#12159 = CARTESIAN_POINT ( 'NONE',  ( -1.297526016723000053, -78.48541891344798671, -10.89864408161000142 ) ) ;
#12160 = CARTESIAN_POINT ( 'NONE',  ( 9.788011744275999959, -24.52881292764999799, -7.956359616222000497 ) ) ;
#12161 = LINE ( 'NONE', #12444, #10040 ) ;
#12162 = CARTESIAN_POINT ( 'NONE',  ( -1.144883253578000248, -76.82350204046299780, 12.33394807668000048 ) ) ;
#12163 = CARTESIAN_POINT ( 'NONE',  ( -8.768124086549999419, -59.94999999446000771, -7.919595949288999570 ) ) ;
#12164 = CARTESIAN_POINT ( 'NONE',  ( 9.708203932494999577, -79.25000000000000000, 7.053423027515000499 ) ) ;
#12165 = ORIENTED_EDGE ( 'NONE', *, *, #6351, .T. ) ;
#12166 = CARTESIAN_POINT ( 'NONE',  ( 10.42771306556999988, -79.93012082385709505, -3.939212573787000515 ) ) ;
#12167 = CARTESIAN_POINT ( 'NONE',  ( 8.266242728491365099, -77.28744835287174908, 4.213564929189619335 ) ) ;
#12168 = CARTESIAN_POINT ( 'NONE',  ( -1.439896632895359962, -78.08541666666666003, 10.99999999999999645 ) ) ;
#12169 = EDGE_CURVE ( 'NONE', #50392, #56632, #27211, .T. ) ;
#12170 = CARTESIAN_POINT ( 'NONE',  ( 0.2682802194768000303, -79.30608152108499098, -11.26307951182000089 ) ) ;
#12171 = FACE_OUTER_BOUND ( 'NONE', #4932, .T. ) ;
#12172 = CARTESIAN_POINT ( 'NONE',  ( 7.220923959705223716, -77.62291666666665435, 9.396085398178630754 ) ) ;
#12173 = CARTESIAN_POINT ( 'NONE',  ( -10.12290050255000118, -60.04999997790999799, 7.648026768390999486 ) ) ;
#12174 = CARTESIAN_POINT ( 'NONE',  ( -0.5534603023178866765, -82.94451038915471486, -1.408692892589827217 ) ) ;
#12175 = CARTESIAN_POINT ( 'NONE',  ( 0.4887196984038748582, -79.75730190472970094, -1.150295180735885658 ) ) ;
#12176 = CIRCLE ( 'NONE', #45180, 12.05000000000000071 ) ;
#12177 = EDGE_CURVE ( 'NONE', #38384, #30828, #37238, .T. ) ;
#12178 = CARTESIAN_POINT ( 'NONE',  ( 8.666925696778452703, -17.00708316157502864, -9.019429295394159496 ) ) ;
#12179 = CARTESIAN_POINT ( 'NONE',  ( 12.76303204522000101, -23.26485147686999966, 1.980584515753000208 ) ) ;
#12180 = FILL_AREA_STYLE ('',( #3040 ) ) ;
#12181 = EDGE_CURVE ( 'NONE', #35471, #35553, #41969, .T. ) ;
#12182 = CARTESIAN_POINT ( 'NONE',  ( -12.70926857199000004, -23.40841990708999987, 1.933876778424000076 ) ) ;
#12183 = VERTEX_POINT ( 'NONE', #24833 ) ;
#12184 = ORIENTED_EDGE ( 'NONE', *, *, #20894, .T. ) ;
#12185 = CARTESIAN_POINT ( 'NONE',  ( -12.61271781517999990, -55.60306329017999616, -1.798333084008999938 ) ) ;
#12186 = CIRCLE ( 'NONE', #45191, 1.250000000000000000 ) ;
#12187 = ORIENTED_EDGE ( 'NONE', *, *, #7468, .T. ) ;
#12188 = B_SPLINE_CURVE_WITH_KNOTS ( 'NONE', 3,
 ( #11270, #47298, #7120, #24255, #20126, #42271, #1838, #6825, #52286, #19832, #20982, #24835, #47006, #51719, #33391, #56996, #43423, #2410, #38405, #55847, #37826, #42851, #52005, #11560, #29537, #47593, #15397, #38115, #38696, #38985, #51137, #29824, #25120, #43143, #10690, #2702, #51428, #10984, #28669, #7404, #56716, #6534, #15685, #46721, #24545, #16274, #2126, #34252, #56137, #33681, #47874, #25407, #12124, #17128, #50119, #36517, #54250, #12412, #12694, #548, #40664, #7692, #21267, #44283, #35112 ),
 .UNSPECIFIED., .F., .F.,
 ( 4, 1, 1, 1, 1, 1, 1, 1, 1, 1, 1, 1, 1, 1, 1, 1, 1, 1, 1, 1, 1, 1, 1, 1, 1, 1, 1, 1, 1, 1, 1, 1, 1, 1, 1, 1, 1, 1, 1, 1, 1, 1, 1, 1, 1, 1, 1, 1, 1, 1, 1, 1, 1, 1, 1, 1, 1, 1, 1, 1, 1, 1, 4 ),
 ( 0.000000000000000000, 0.01249977918653473984, 0.02874978664248292043, 0.04499979409843109929, 0.06124980155437927815, 0.07749980901032745007, 0.09374981646627562892, 0.1099998239222238078, 0.1262498313781720005, 0.1424998388341201516, 0.1587498462900683582, 0.1749998537460165093, 0.1912498612019647160, 0.2074998686579128671, 0.2237498761138610737, 0.2399998835698092525, 0.2562498910257574036, 0.2724998984817056380, 0.2887499059376538169, 0.3049999133936019402, 0.3212499208495501191, 0.3374999283054983534, 0.3537499357614465323, 0.3699999432173946556, 0.3862499506733428345, 0.4024999581292910689, 0.4187499655852392477, 0.4349999730411874266, 0.4512499804971355499, 0.4674999879530837843, 0.4837499954090319632, 0.5000000028649801420, 0.5162500103209283209, 0.5325000177768764997, 0.5487500252328246786, 0.5650000326887728574, 0.5812500401447211473, 0.5975000476006693262, 0.6137500550566175050, 0.6300000625125655729, 0.6462500699685137517, 0.6625000774244619306, 0.6787500848804101095, 0.6950000923363582883, 0.7112500997923065782, 0.7275001072482547571, 0.7437501147042029359, 0.7600001221601511148, 0.7762501296160991826, 0.7925001370720473615, 0.8087501445279955403, 0.8250001519839437192, 0.8412501594398920091, 0.8575001668958401879, 0.8737501743517883668, 0.8900001818077365456, 0.9062501892636847245, 0.9225001967196327923, 0.9387502041755809712, 0.9550002116315291500, 0.9712502190874773289, 0.9875002265434256188, 1.000000000000000000 ),
 .UNSPECIFIED. ) ;
#12189 = ORIENTED_EDGE ( 'NONE', *, *, #50366, .F. ) ;
#12190 = CARTESIAN_POINT ( 'NONE',  ( 10.36289662401999934, -23.20106470441999846, 7.633500902327000404 ) ) ;
#12191 = CARTESIAN_POINT ( 'NONE',  ( -9.786314039287999478, -78.03687501975998941, 4.837708502169000724 ) ) ;
#12192 = VECTOR ( 'NONE', #7539, 1000.000000000000000 ) ;
#12193 = CARTESIAN_POINT ( 'NONE',  ( 2.253288347564000205, -79.40013667140100040, -9.650850687256999905 ) ) ;
#12194 = CARTESIAN_POINT ( 'NONE',  ( 9.249483092228999226, -79.25084128437099196, 0.09778817195952001218 ) ) ;
#12195 = ORIENTED_EDGE ( 'NONE', *, *, #39281, .T. ) ;
#12196 = ORIENTED_EDGE ( 'NONE', *, *, #25391, .F. ) ;
#12197 = CARTESIAN_POINT ( 'NONE',  ( -6.557430175411668394, -77.53787113409947551, 6.523852457878298594 ) ) ;
#12198 = CARTESIAN_POINT ( 'NONE',  ( 10.77519778174000109, -77.11087656805389656, -1.228540277667999892 ) ) ;
#12199 = CARTESIAN_POINT ( 'NONE',  ( -12.46165725309000116, -60.47155322489999918, -1.631637378451999965 ) ) ;
#12200 = CARTESIAN_POINT ( 'NONE',  ( 9.051070938631999852, -77.60951297768299639, 3.499832029064999794 ) ) ;
#12201 = CARTESIAN_POINT ( 'NONE',  ( 7.640030264154999529, -18.69283319134000010, 10.18491080493000212 ) ) ;
#12202 = FACE_OUTER_BOUND ( 'NONE', #18693, .T. ) ;
#12203 = CARTESIAN_POINT ( 'NONE',  ( 8.792808668394924254, -53.57303577587560994, -9.175550543417134719 ) ) ;
#12204 = CARTESIAN_POINT ( 'NONE',  ( -9.459258931978000717, -79.94904572086998940, 5.442530770145999952 ) ) ;
#12205 = CARTESIAN_POINT ( 'NONE',  ( 12.43645963092999907, -17.08248289540999920, 0.05235777564064000161 ) ) ;
#12206 = CARTESIAN_POINT ( 'NONE',  ( -0.3904991445228000457, -82.21237762652100400, -1.255013400307000149 ) ) ;
#12207 = CARTESIAN_POINT ( 'NONE',  ( -9.767984832581378285, -76.65268247146492797, 6.530121237128238221 ) ) ;
#12208 = VERTEX_POINT ( 'NONE', #28963 ) ;
#12209 = CARTESIAN_POINT ( 'NONE',  ( -7.657744736598999680, -55.13080421771999795, 9.966195456739999514 ) ) ;
#12210 = CARTESIAN_POINT ( 'NONE',  ( 11.36821324764999908, -77.92614517502100568, -3.778861202892000115 ) ) ;
#12211 = CARTESIAN_POINT ( 'NONE',  ( -8.541162059891000524, -16.99199348450000002, -9.205819316576999256 ) ) ;
#12213 = CARTESIAN_POINT ( 'NONE',  ( -0.9887300587125997797, -17.06589942230999668, -12.65963207090000076 ) ) ;
#12212 = CARTESIAN_POINT ( 'NONE',  ( 7.612971540256999958, -55.47547726255000100, 10.53003236230999917 ) ) ;
#12214 = AXIS2_PLACEMENT_3D ( 'NONE', #52312, #11868, #1860 ) ;
#12215 = DIRECTION ( 'NONE',  ( 0.000000000000000000, 1.000000000000000000, 0.000000000000000000 ) ) ;
#12216 = CARTESIAN_POINT ( 'NONE',  ( -0.2842604123649000170, -80.11603890021898167, -11.17811493562000003 ) ) ;
#12217 = CARTESIAN_POINT ( 'NONE',  ( 6.163257195008000622, -78.56341404718699550, -9.114053931137998887 ) ) ;
#12218 = CARTESIAN_POINT ( 'NONE',  ( 1.679092372047056303, -3.500000000000000444, 2.912269088518365301 ) ) ;
#12219 = CARTESIAN_POINT ( 'NONE',  ( -6.603701251060000388, -80.74830188227322481, 9.115088936944999887 ) ) ;
#12220 = ORIENTED_EDGE ( 'NONE', *, *, #27751, .T. ) ;
#12221 = DIRECTION ( 'NONE',  ( -1.000000000000000000, 0.000000000000000000, 0.000000000000000000 ) ) ;
#12222 = CARTESIAN_POINT ( 'NONE',  ( 10.10912542009492476, -18.52413588830737012, -7.634643956514229224 ) ) ;
#12223 = CARTESIAN_POINT ( 'NONE',  ( -12.64502302235000109, -22.77129148951999937, 1.799490220168999954 ) ) ;
#12224 = CARTESIAN_POINT ( 'NONE',  ( 3.399769613747000374, -1.852058083081000062, -1.316590098206999793 ) ) ;
#12225 = CARTESIAN_POINT ( 'NONE',  ( 5.169261753999999875, -79.69201159510198806, -7.880669826094999664 ) ) ;
#12226 = DIRECTION ( 'NONE',  ( 0.000000000000000000, 1.000000000000000000, 0.000000000000000000 ) ) ;
#12227 = CARTESIAN_POINT ( 'NONE',  ( -1.724324800276255454, -77.21249999999999147, -10.89830687840934864 ) ) ;
#12228 = CARTESIAN_POINT ( 'NONE',  ( -1.500000000000000000, -79.90000000000000568, 0.000000000000000000 ) ) ;
#12229 = CARTESIAN_POINT ( 'NONE',  ( 4.044903269867999640, -79.05999999999998806, -8.595856998426999240 ) ) ;
#12230 = AXIS2_PLACEMENT_3D ( 'NONE', #40569, #162, #22558 ) ;
#12231 = CARTESIAN_POINT ( 'NONE',  ( 3.490710543544000455, -85.63696544543098810, -1.876411688659999966 ) ) ;
#12232 = DIRECTION ( 'NONE',  ( -1.000000000000000000, 0.000000000000000000, 0.000000000000000000 ) ) ;
#12233 = EDGE_CURVE ( 'NONE', #54663, #25767, #5717, .T. ) ;
#12234 = CARTESIAN_POINT ( 'NONE',  ( 3.999999999999885425, -78.69999999999998863, 2.360693471584177860 ) ) ;
#12235 = CARTESIAN_POINT ( 'NONE',  ( 4.790019567428999814, -77.96759421635398724, -9.965127559477000574 ) ) ;
#12236 = CARTESIAN_POINT ( 'NONE',  ( 8.150535938090355259, -76.38592193059849933, -8.463838335192644280 ) ) ;
#12237 = CARTESIAN_POINT ( 'NONE',  ( -10.86494198988000015, -78.22680183458999181, -2.491513063939999828 ) ) ;
#12238 = CARTESIAN_POINT ( 'NONE',  ( 0.3833199769307082949, -81.95046860891231688, 1.189846988800133287 ) ) ;
#12239 = CARTESIAN_POINT ( 'NONE',  ( 1.178978867320999990, -78.64234607169998981, 1.173689911365999983 ) ) ;
#12240 = CARTESIAN_POINT ( 'NONE',  ( 10.14950121161999874, -59.55077027461999961, 7.674627477469999626 ) ) ;
#12241 = CARTESIAN_POINT ( 'NONE',  ( -9.250000000000000000, -78.49999999999998579, 0.000000000000000000 ) ) ;
#12242 = CARTESIAN_POINT ( 'NONE',  ( -11.00000000000000888, -77.58958333333332291, 1.439896632895276252 ) ) ;
#12243 = CARTESIAN_POINT ( 'NONE',  ( -4.098243062044448770, -80.19425443582535706, -9.937901660273714910 ) ) ;
#12244 = CYLINDRICAL_SURFACE ( 'NONE', #25869, 1.250000000000000000 ) ;
#12245 = CARTESIAN_POINT ( 'NONE',  ( -9.697390092196839007, -17.02767731347392299, -8.266602378574265941 ) ) ;
#12246 = CARTESIAN_POINT ( 'NONE',  ( 7.313768098873999257, -78.88818067319900251, 9.313141831727000053 ) ) ;
#12247 = CARTESIAN_POINT ( 'NONE',  ( -9.050966798898000931, -55.65000000893999754, 7.919595949288999570 ) ) ;
#12248 = ADVANCED_FACE ( 'NONE', ( #29535 ), #14453, .F. ) ;
#12249 = CARTESIAN_POINT ( 'NONE',  ( -10.80063122475000092, -78.84626760295098791, -3.190662894339999944 ) ) ;
#12250 = CARTESIAN_POINT ( 'NONE',  ( -0.9465222407332000154, -81.15663953506998496, -0.8164530897714000757 ) ) ;
#12251 = ORIENTED_EDGE ( 'NONE', *, *, #19969, .F. ) ;
#12252 = CARTESIAN_POINT ( 'NONE',  ( -2.353768593183752866, -0.7500000000000000000, 2.616124937882430945 ) ) ;
#12253 = VERTEX_POINT ( 'NONE', #55779 ) ;
#12254 = ORIENTED_EDGE ( 'NONE', *, *, #31389, .T. ) ;
#12255 = CYLINDRICAL_SURFACE ( 'NONE', #13137, 10.50000000000000000 ) ;
#12256 = ORIENTED_EDGE ( 'NONE', *, *, #42729, .T. ) ;
#12257 = CARTESIAN_POINT ( 'NONE',  ( 3.263538630792000017, -79.53581372688118734, -1.494342973906999994 ) ) ;
#12258 = CARTESIAN_POINT ( 'NONE',  ( 0.1752985264899695750, -79.27328162838476544, 9.505737417831570113 ) ) ;
#12259 = ORIENTED_EDGE ( 'NONE', *, *, #42011, .F. ) ;
#12260 = CARTESIAN_POINT ( 'NONE',  ( -11.50369798034000013, -78.89133840368999984, 4.092992355904999435 ) ) ;
#12261 = B_SPLINE_CURVE_WITH_KNOTS ( 'NONE', 3,
 ( #21754, #35315, #4340, #12892, #8767, #17328, #26759, #30893, #48926, #44486 ),
 .UNSPECIFIED., .F., .F.,
 ( 4, 2, 2, 2, 4 ),
 ( 0.1666666058611807055, 0.3749999543958855153, 0.5833333029305902695, 0.7916666514652952458, 1.000000000000000000 ),
 .UNSPECIFIED. ) ;
#12262 = ORIENTED_EDGE ( 'NONE', *, *, #50295, .T. ) ;
#12263 = CARTESIAN_POINT ( 'NONE',  ( -7.653559626114000203, -60.09848884406000025, 10.01235002625000092 ) ) ;
#12264 = ORIENTED_EDGE ( 'NONE', *, *, #3920, .T. ) ;
#12265 = CARTESIAN_POINT ( 'NONE',  ( -3.234167002596432638, -1.610214578096402116, -0.3547048605170013413 ) ) ;
#12266 = VECTOR ( 'NONE', #1588, 1000.000000000000000 ) ;
#12267 = CYLINDRICAL_SURFACE ( 'NONE', #5768, 10.69999999999999929 ) ;
#12268 = EDGE_CURVE ( 'NONE', #18435, #19319, #54958, .T. ) ;
#12269 = CARTESIAN_POINT ( 'NONE',  ( -9.936142110726182253, -80.06889634899292219, 4.117545299896771205 ) ) ;
#12270 = CARTESIAN_POINT ( 'NONE',  ( 1.750000000000000000, -76.29999999999999716, -0.5000000000000000000 ) ) ;
#12271 = CARTESIAN_POINT ( 'NONE',  ( -3.079437091258010017, -86.12609999968208285, 1.441203386403802078 ) ) ;
#12272 = CARTESIAN_POINT ( 'NONE',  ( 1.546553306619000256, -76.46993419121800173, -11.07619323537999989 ) ) ;
#12273 = CARTESIAN_POINT ( 'NONE',  ( 7.406580528771000260, -77.67838321630000564, -10.82165712228000132 ) ) ;
#12274 = DIRECTION ( 'NONE',  ( -0.6489586469979856664, 0.04890178911501888437, -0.7592504787669837052 ) ) ;
#12275 = CARTESIAN_POINT ( 'NONE',  ( 10.06256222744999995, -76.17602919452599508, 4.718524714222000149 ) ) ;
#12276 = DIRECTION ( 'NONE',  ( 0.7071067811865474617, 0.000000000000000000, -0.7071067811865474617 ) ) ;
#12277 = CARTESIAN_POINT ( 'NONE',  ( -2.360807543337999803, -80.61806754721197876, -3.388967605774999559 ) ) ;
#12278 = FACE_OUTER_BOUND ( 'NONE', #24088, .T. ) ;
#12279 = CARTESIAN_POINT ( 'NONE',  ( -0.02783871057799041163, -2.976126516332163963, 3.249638514261254940 ) ) ;
#12280 = CARTESIAN_POINT ( 'NONE',  ( -0.9782436348499000678, -81.33525264934799281, 3.407051980398000168 ) ) ;
#12281 = EDGE_CURVE ( 'NONE', #53816, #41078, #41584, .T. ) ;
#12282 = CARTESIAN_POINT ( 'NONE',  ( 8.343860018000999190, -60.54999999966955926, -8.343860018000999190 ) ) ;
#12283 = CARTESIAN_POINT ( 'NONE',  ( -0.8442961504774461057, -80.98138397070125905, 10.71670580309706544 ) ) ;
#12284 = CARTESIAN_POINT ( 'NONE',  ( -2.266693762821000213, -84.47794503318799286, 2.728307486420999961 ) ) ;
#12285 = CARTESIAN_POINT ( 'NONE',  ( -3.796701970596999764, -2.777085600324999959, 0.2667143827384000354 ) ) ;
#12286 = CARTESIAN_POINT ( 'NONE',  ( -1.237049208466255878, -79.76968421440388113, -0.3056626403079319432 ) ) ;
#12287 = DIRECTION ( 'NONE',  ( -0.9957542217969272969, 0.04890179605515140859, 0.07798810240143222439 ) ) ;
#12288 = CARTESIAN_POINT ( 'NONE',  ( -11.29698467241381543, -79.27175061103834253, 4.184771565250528624 ) ) ;
#12289 = CARTESIAN_POINT ( 'NONE',  ( -1.127489577578000057, -80.76097822051700348, -0.5989559841152000130 ) ) ;
#12290 = AXIS2_PLACEMENT_3D ( 'NONE', #31989, #27561, #41154 ) ;
#12291 = CARTESIAN_POINT ( 'NONE',  ( -9.399464885765262068, -78.91333333333335531, -1.591687513073350990 ) ) ;
#12292 = CARTESIAN_POINT ( 'NONE',  ( -12.96685733093999993, -77.05870625016000020, -1.095351912296000041 ) ) ;
#12293 = B_SPLINE_CURVE_WITH_KNOTS ( 'NONE', 3,
 ( #41889, #55468, #55175, #2333, #47218, #55769, #6747, #19166, #1467, #24756, #51057, #42772, #10021, #38324, #7320, #34747, #25323, #43631, #51924, #21183, #48644, #52775, #56344 ),
 .UNSPECIFIED., .F., .F.,
 ( 4, 2, 2, 2, 2, 2, 1, 2, 2, 2, 2, 4 ),
 ( 0.000000000000000000, 0.1250000000000000555, 0.2500000000000000555, 0.3125000000000000000, 0.3749999999999999445, 0.4374999999999998890, 0.4999999999999998890, 0.5624999999999998890, 0.6249999999999998890, 0.7499999999999998890, 0.8749999999999998890, 1.000000000000000000 ),
 .UNSPECIFIED. ) ;
#12294 = CARTESIAN_POINT ( 'NONE',  ( -10.71369944335147117, -79.72083333333331723, -2.879226727952084453 ) ) ;
#12295 = DIRECTION ( 'NONE',  ( -0.9999999999995751176, 0.000000000000000000, -9.217549100139771309E-07 ) ) ;
#12296 = CARTESIAN_POINT ( 'NONE',  ( 6.720944364705999874, -75.82425451000999317, 10.55406361522000047 ) ) ;
#12297 = ORIENTED_EDGE ( 'NONE', *, *, #22440, .F. ) ;
#12298 = ADVANCED_FACE ( 'NONE', ( #52216 ), #53413, .F. ) ;
#12299 = CARTESIAN_POINT ( 'NONE',  ( -7.624341764906000130, -55.53514850498000044, -10.42531124851000079 ) ) ;
#12300 = DIRECTION ( 'NONE',  ( 0.000000000000000000, -1.000000000000000000, 0.000000000000000000 ) ) ;
#12301 = ADVANCED_FACE ( 'NONE', ( #15317, #45758 ), #5867, .F. ) ;
#12302 = CARTESIAN_POINT ( 'NONE',  ( 12.49837680052000088, -60.00957148770000060, 1.667051419334000029 ) ) ;
#12303 = CARTESIAN_POINT ( 'NONE',  ( 7.642147947538999730, -19.21514526754999963, -10.55910102244999926 ) ) ;
#12304 = CARTESIAN_POINT ( 'NONE',  ( -0.5506691749702000704, -78.01350959400299701, -9.615090921292999582 ) ) ;
#12305 = CARTESIAN_POINT ( 'NONE',  ( -0.8075256636061000082, -83.54105886393099922, -4.093650542163000061 ) ) ;
#12306 = CARTESIAN_POINT ( 'NONE',  ( 4.250518816003403089, -79.94278005840584456, 9.873894375703258675 ) ) ;
#12307 = CARTESIAN_POINT ( 'NONE',  ( -0.9624967649451999785, -80.61439197592500250, -1.086495216026000188 ) ) ;
#12308 = ORIENTED_EDGE ( 'NONE', *, *, #2312, .T. ) ;
#12309 = CARTESIAN_POINT ( 'NONE',  ( -0.3450130740848871280, -82.18489583333146697, 1.280549398083555390 ) ) ;
#12310 = CIRCLE ( 'NONE', #45324, 13.89999999999999858 ) ;
#12311 = VECTOR ( 'NONE', #7652, 1000.000000000000000 ) ;
#12312 = CARTESIAN_POINT ( 'NONE',  ( 0.1735539215762753051, -78.89307393851466088, -3.951712425000363460 ) ) ;
#12313 = ORIENTED_EDGE ( 'NONE', *, *, #45487, .F. ) ;
#12314 = CARTESIAN_POINT ( 'NONE',  ( -10.93134324956000114, -78.37401457012799710, -0.4399444258272000030 ) ) ;
#12315 = CARTESIAN_POINT ( 'NONE',  ( -7.342377162853141570, -55.56980390652893931, -8.190817883596540838 ) ) ;
#12316 = B_SPLINE_CURVE_WITH_KNOTS ( 'NONE', 3,
 ( #47585, #6526, #38398, #2119, #3265, #51420 ),
 .UNSPECIFIED., .F., .F.,
 ( 4, 1, 1, 4 ),
 ( 0.000000000000000000, 0.3333333333333000081, 0.6666666666667000474, 1.000000000000000000 ),
 .UNSPECIFIED. ) ;
#12317 = EDGE_CURVE ( 'NONE', #35080, #38899, #33312, .T. ) ;
#12318 = CARTESIAN_POINT ( 'NONE',  ( -8.227975111406001574, -79.81548455509199869, 6.864277664119000200 ) ) ;
#12319 = EDGE_LOOP ( 'NONE', ( #37886, #6897, #5383, #55102 ) ) ;
#12320 = ORIENTED_EDGE ( 'NONE', *, *, #32009, .F. ) ;
#12321 = EDGE_LOOP ( 'NONE', ( #27916, #49290, #5609, #12926 ) ) ;
#12322 = B_SPLINE_CURVE_WITH_KNOTS ( 'NONE', 3,
 ( #15542, #43288, #2841, #11134, #50989, #42706, #6096, #42421, #24106, #20558, #10540, #37971, #28523, #34107, #1691, #47447, #24406, #1990, #19984, #55996, #47157, #2273, #6687 ),
 .UNSPECIFIED., .F., .F.,
 ( 4, 2, 2, 2, 2, 1, 2, 2, 2, 2, 2, 4 ),
 ( 0.000000000000000000, 0.1249999999999998890, 0.2499999999999997780, 0.3749999999999997224, 0.4374999999999997224, 0.4999999999999996669, 0.5624999999999996669, 0.6249999999999997780, 0.7499999999999998890, 0.8749999999999998890, 0.9374999999999998890, 1.000000000000000000 ),
 .UNSPECIFIED. ) ;
#12323 = CARTESIAN_POINT ( 'NONE',  ( -1.250000000000000000, -60.04999999966999980, -12.50000000000000000 ) ) ;
#12324 = FACE_OUTER_BOUND ( 'NONE', #6662, .T. ) ;
#12325 = CARTESIAN_POINT ( 'NONE',  ( -3.303475362236280688, -1.803380025278898957, 2.022687598699045797 ) ) ;
#12326 = ORIENTED_EDGE ( 'NONE', *, *, #37396, .F. ) ;
#12327 = CARTESIAN_POINT ( 'NONE',  ( -12.70556836328846728, -25.22772277325712409, -0.2642470010205509867 ) ) ;
#12328 = AXIS2_PLACEMENT_3D ( 'NONE', #24426, #20288, #38576 ) ;
#12329 = VERTEX_POINT ( 'NONE', #610 ) ;
#12330 = DIRECTION ( 'NONE',  ( 0.000000000000000000, 1.000000000000000000, 0.000000000000000000 ) ) ;
#12331 = CARTESIAN_POINT ( 'NONE',  ( -3.850965819624345254, -78.96264283715740362, 0.07259824540930022441 ) ) ;
#12332 = CARTESIAN_POINT ( 'NONE',  ( 9.038965287750000854, -53.46737759073999996, 9.029769469428000406 ) ) ;
#12333 = CARTESIAN_POINT ( 'NONE',  ( 1.310679582531385501, -81.19166666666669130, 0.7554284705563518720 ) ) ;
#12334 = CARTESIAN_POINT ( 'NONE',  ( -17.50000000000000000, -57.79999999999999716, 0.000000000000000000 ) ) ;
#12335 = CARTESIAN_POINT ( 'NONE',  ( 4.767018142753490118, -80.18960264150359762, 10.03241642955576829 ) ) ;
#12336 = CARTESIAN_POINT ( 'NONE',  ( -4.085659785884999451, -78.55269560739655788, 11.26159174134999930 ) ) ;
#12337 = CARTESIAN_POINT ( 'NONE',  ( 9.099688436573039496, -78.83571894269113045, -1.661325781669990453 ) ) ;
#12338 = CARTESIAN_POINT ( 'NONE',  ( -7.646788277333999240, -23.37228598377000210, 10.00831419131999844 ) ) ;
#12339 = CIRCLE ( 'NONE', #3870, 2.899999999999999911 ) ;
#12340 = CARTESIAN_POINT ( 'NONE',  ( 0.9272595967461000344, -81.28405496681197917, 4.068200085201000071 ) ) ;
#12341 = EDGE_CURVE ( 'NONE', #7317, #39806, #8385, .T. ) ;
#12342 = CARTESIAN_POINT ( 'NONE',  ( -3.662222950988999859, -77.66248667140099826, 9.049764572265999618 ) ) ;
#12343 = CARTESIAN_POINT ( 'NONE',  ( -12.54673671099000032, -17.17796527435999820, 0.9173654211231000444 ) ) ;
#12344 = CARTESIAN_POINT ( 'NONE',  ( 12.76303204517000012, -18.73514852243999940, -1.980584515753000208 ) ) ;
#12345 = DIRECTION ( 'NONE',  ( 0.000000000000000000, 1.000000000000000000, 0.000000000000000000 ) ) ;
#12346 = CARTESIAN_POINT ( 'NONE',  ( -10.50000000000000000, -7.000000000000000000, 0.000000000000000000 ) ) ;
#12347 = CARTESIAN_POINT ( 'NONE',  ( 0.000000000000000000, -26.93717104351999936, 0.000000000000000000 ) ) ;
#12348 = CARTESIAN_POINT ( 'NONE',  ( -0.1636246173744673738, -78.61458333333330017, -1.249999999999999778 ) ) ;
#12349 = CARTESIAN_POINT ( 'NONE',  ( -0.7972742194625092038, -80.33495930260389173, -1.448481206412859157 ) ) ;
#12350 = CARTESIAN_POINT ( 'NONE',  ( 9.489101650983998937, -77.20556042082598935, -0.1642684238307999811 ) ) ;
#12351 = CARTESIAN_POINT ( 'NONE',  ( 0.6906586288378000482, -79.06822964757999728, -1.459522026167999975 ) ) ;
#12352 = CARTESIAN_POINT ( 'NONE',  ( -10.75000000000000000, -80.50000000000000000, -1.711887504597999906E-14 ) ) ;
#12353 = CARTESIAN_POINT ( 'NONE',  ( 1.080502472816999848, -3.206346044169000375, -3.225196509442000092 ) ) ;
#12354 = CARTESIAN_POINT ( 'NONE',  ( 8.480197680338001476, -78.05907011069199086, -8.881555409017000358 ) ) ;
#12355 = CARTESIAN_POINT ( 'NONE',  ( 17.50000000000000000, -63.73717104351998586, 4.519614127395999927E-10 ) ) ;
#12357 = CARTESIAN_POINT ( 'NONE',  ( -1.242864761025999965, -77.72794916437750601, 0.2245736866142999943 ) ) ;
#12356 = CARTESIAN_POINT ( 'NONE',  ( 6.585791278903703194, -80.10725068706773300, 8.809977328666299456 ) ) ;
#12358 = CARTESIAN_POINT ( 'NONE',  ( -1.407332420019999919, -81.66638770227000066, -0.4193609517060999936 ) ) ;
#12359 = CARTESIAN_POINT ( 'NONE',  ( -6.210567785792292739, -79.52403206663427682, 8.774603838976910097 ) ) ;
#12360 = ORIENTED_EDGE ( 'NONE', *, *, #15660, .T. ) ;
#12361 = CARTESIAN_POINT ( 'NONE',  ( -10.21381326472000062, -22.77129148951999937, -7.668949790003000366 ) ) ;
#12362 = CARTESIAN_POINT ( 'NONE',  ( 10.28508546004999857, -79.48465556260299536, 6.261730588902000072 ) ) ;
#12363 = CARTESIAN_POINT ( 'NONE',  ( -8.340505669901505215, -79.20899701435310192, 4.714710602094070779 ) ) ;
#12364 = B_SPLINE_CURVE_WITH_KNOTS ( 'NONE', 3,
 ( #6166, #32427, #5293, #9727, #1470, #38042, #51061, #2054, #55474, #1181, #23587, #895, #10611, #36871, #10025, #19459, #37455, #33014, #50473, #28593, #28294, #46638, #6457, #45760, #54882, #24176, #27715, #42192, #37165, #46346 ),
 .UNSPECIFIED., .F., .F.,
 ( 4, 2, 2, 2, 2, 2, 2, 2, 2, 2, 2, 2, 2, 2, 4 ),
 ( 0.000000000000000000, 0.1250000000000000000, 0.1875000000000000000, 0.2500000000000000000, 0.3125000000000000000, 0.3750000000000000000, 0.4999999999999999445, 0.5624999999999998890, 0.6249999999999998890, 0.6874999999999998890, 0.7499999999999998890, 0.8124999999999998890, 0.8437499999999998890, 0.8749999999999998890, 1.000000000000000000 ),
 .UNSPECIFIED. ) ;
#12365 = STYLED_ITEM ( 'NONE', ( #41218 ), #57583 ) ;
#12366 = ADVANCED_FACE ( 'NONE', ( #15018 ), #33012, .F. ) ;
#12367 = CARTESIAN_POINT ( 'NONE',  ( -2.811854283077139804, -79.79375000000001705, 11.70391985135060864 ) ) ;
#12368 = CARTESIAN_POINT ( 'NONE',  ( 10.99999999999999645, -78.86041666666666572, 1.439896632895345974 ) ) ;
#12369 = CARTESIAN_POINT ( 'NONE',  ( 3.743655618246999772, -1.488444768727999801, 0.9564365499490000699 ) ) ;
#12370 = CARTESIAN_POINT ( 'NONE',  ( 9.470739325998000169, -78.94724519986900191, -1.171383596386999848 ) ) ;
#12371 = CARTESIAN_POINT ( 'NONE',  ( -3.251382512355739163, -3.110731818665983361, -0.4248859449704894820 ) ) ;
#12372 = CARTESIAN_POINT ( 'NONE',  ( 3.325701842495000005, -82.39999999999999147, -0.7068997487804000723 ) ) ;
#12373 = ORIENTED_EDGE ( 'NONE', *, *, #23830, .F. ) ;
#12374 = CARTESIAN_POINT ( 'NONE',  ( 7.000000000000000000, -81.10000000285099020, 0.000000000000000000 ) ) ;
#12375 = CARTESIAN_POINT ( 'NONE',  ( -7.764665820177000022, -79.87226001420199850, -5.883443353344000037 ) ) ;
#12376 = CARTESIAN_POINT ( 'NONE',  ( -12.54435570283313162, -18.47582218226908424, 1.733918077769268873 ) ) ;
#12377 = CARTESIAN_POINT ( 'NONE',  ( -0.9218200799623714747, -78.47291666666666288, -1.199500263597270466 ) ) ;
#12378 = CARTESIAN_POINT ( 'NONE',  ( 0.9441861370063999725, -79.59744055935000517, 1.372505234203999835 ) ) ;
#12379 = ADVANCED_FACE ( 'NONE', ( #5003 ), #5574, .T. ) ;
#12380 = ORIENTED_EDGE ( 'NONE', *, *, #54345, .T. ) ;
#12381 = DIRECTION ( 'NONE',  ( 0.9999999999995751176, 0.000000000000000000, 9.217549097710770925E-07 ) ) ;
#12382 = CARTESIAN_POINT ( 'NONE',  ( -0.6454797251710800987, -53.91193487831872488, -12.50471521364922545 ) ) ;
#12383 = LINE ( 'NONE', #48413, #14829 ) ;
#12384 = EDGE_CURVE ( 'NONE', #34267, #46987, #41393, .T. ) ;
#12385 = CONICAL_SURFACE ( 'NONE', #7665, 0.5999999993581000002, 0.7853981633972997312 ) ;
#12386 = CARTESIAN_POINT ( 'NONE',  ( -12.92177931909999877, -57.04263462147999775, 2.062503053667999797 ) ) ;
#12387 = CARTESIAN_POINT ( 'NONE',  ( 1.092232985442820992, -78.29166666666667140, 0.6295237254636267821 ) ) ;
#12388 = DIRECTION ( 'NONE',  ( 0.000000000000000000, -1.000000000000000000, 0.000000000000000000 ) ) ;
#12389 = ORIENTED_EDGE ( 'NONE', *, *, #7536, .F. ) ;
#12390 = ORIENTED_EDGE ( 'NONE', *, *, #57484, .T. ) ;
#12391 = CARTESIAN_POINT ( 'NONE',  ( -11.67502321291000023, -76.85709426284898882, -4.708162379318000745 ) ) ;
#12392 = CARTESIAN_POINT ( 'NONE',  ( -9.600681700141771913, -78.63729878341381152, -4.836084120192285063 ) ) ;
#12393 = CARTESIAN_POINT ( 'NONE',  ( 1.305753739922999923, -77.92566549289000477, 0.5616213463899000224 ) ) ;
#12394 = VERTEX_POINT ( 'NONE', #41018 ) ;
#12395 = DIRECTION ( 'NONE',  ( 0.000000000000000000, -1.000000000000000000, 0.000000000000000000 ) ) ;
#12396 = CARTESIAN_POINT ( 'NONE',  ( -6.760013919724102038, -77.62708333333333144, 8.796335266379953666 ) ) ;
#12397 = ADVANCED_FACE ( 'NONE', ( #37163 ), #10303, .F. ) ;
#12398 = FACE_OUTER_BOUND ( 'NONE', #23143, .T. ) ;
#12399 = CARTESIAN_POINT ( 'NONE',  ( -7.915529793650001089, -78.59986579304998600, 9.174504061492999796 ) ) ;
#12400 = CARTESIAN_POINT ( 'NONE',  ( 0.1392748842281999744, -77.12401228047586699, 11.21600254538999941 ) ) ;
#12401 = CARTESIAN_POINT ( 'NONE',  ( 0.000000000000000000, -19.21421830981000767, 13.15643568216998638 ) ) ;
#12402 = CARTESIAN_POINT ( 'NONE',  ( 4.020839152127012817, -86.31452042059399332, 0.4615274515354030882 ) ) ;
#12403 = CARTESIAN_POINT ( 'NONE',  ( -8.982117338527000783, -79.85057669154679161, 6.718606902359000266 ) ) ;
#12404 = FACE_OUTER_BOUND ( 'NONE', #53194, .T. ) ;
#12405 = CARTESIAN_POINT ( 'NONE',  ( 2.000000000000000000, -76.29999999999999716, 0.000000000000000000 ) ) ;
#12406 = COLOUR_RGB ( '', 0.72549020, 0.75294118, 0.79215686) ;
#12407 = EDGE_LOOP ( 'NONE', ( #25503, #56189, #1674, #55264 ) ) ;
#12408 = CARTESIAN_POINT ( 'NONE',  ( 11.14483649738000004, -79.38250813710999410, 1.649713251514000056 ) ) ;
#12409 = CARTESIAN_POINT ( 'NONE',  ( 7.840108872306949195, -77.30560672394517496, -4.911361524887249530 ) ) ;
#12410 = CARTESIAN_POINT ( 'NONE',  ( 1.396889377938999921, -80.53364115338500540, -0.2424037069397000088 ) ) ;
#12411 = CARTESIAN_POINT ( 'NONE',  ( -0.9995835529977249445, -83.05208333333330017, -0.7681833999686439318 ) ) ;
#12412 = CARTESIAN_POINT ( 'NONE',  ( 0.5473746484684922642, -76.97879305343433032, -11.20365965675252795 ) ) ;
#12414 = EDGE_CURVE ( 'NONE', #16042, #35254, #45781, .T. ) ;
#12413 = CARTESIAN_POINT ( 'NONE',  ( -0.1877060973040000080, -78.21711910266039069, -1.405284953735000064 ) ) ;
#12415 = CYLINDRICAL_SURFACE ( 'NONE', #53022, 9.250000000000000000 ) ;
#12416 = CARTESIAN_POINT ( 'NONE',  ( 9.342458652602138258, -77.03333333333333144, -1.989514594393971603 ) ) ;
#12417 = CARTESIAN_POINT ( 'NONE',  ( 0.9999999970759999579, -75.20000000292399989, -7.199999982805000087 ) ) ;
#12418 = CARTESIAN_POINT ( 'NONE',  ( 0.000000000000000000, -80.69999999999998863, 0.000000000000000000 ) ) ;
#12419 = CARTESIAN_POINT ( 'NONE',  ( -7.718346056127999510, -20.25111654322000021, 10.07719973196000041 ) ) ;
#12420 = ADVANCED_FACE ( 'NONE', ( #39992 ), #50845, .F. ) ;
#12421 = CARTESIAN_POINT ( 'NONE',  ( -3.607132791900000246, -79.65574064831898227, -10.55841809546000043 ) ) ;
#12422 = CARTESIAN_POINT ( 'NONE',  ( 10.55911395187000146, -19.21538333566000034, -7.642160924884000117 ) ) ;
#12423 = CARTESIAN_POINT ( 'NONE',  ( -0.8973488778757167106, -83.03941064879536782, 0.8696509586403449177 ) ) ;
#12424 = CARTESIAN_POINT ( 'NONE',  ( -4.013587779334000238, -78.64724969135635035, 0.5806597091830999480 ) ) ;
#12425 = ORIENTED_EDGE ( 'NONE', *, *, #54062, .F. ) ;
#12426 = CARTESIAN_POINT ( 'NONE',  ( 1.565347158977999920, -82.54782237971299708, -0.6704515100525999527 ) ) ;
#12427 = CARTESIAN_POINT ( 'NONE',  ( 1.399788002916999785, -80.73109529231999204, 0.4438937798904999954 ) ) ;
#12428 = DIRECTION ( 'NONE',  ( 1.000000000000000000, 0.000000000000000000, 0.000000000000000000 ) ) ;
#12429 = CARTESIAN_POINT ( 'NONE',  ( -11.86109855473999986, -78.50952966248199516, -1.682380905046999997 ) ) ;
#12430 = CARTESIAN_POINT ( 'NONE',  ( -12.70451796517048315, -16.82354927383735799, 0.5205401191410179429 ) ) ;
#12431 = CONICAL_SURFACE ( 'NONE', #2093, 5.199999999809000073, 0.7853981633972997312 ) ;
#12432 = CARTESIAN_POINT ( 'NONE',  ( 1.571434226476000173, -82.93424664794399348, -0.5530452149683998675 ) ) ;
#12433 = CARTESIAN_POINT ( 'NONE',  ( -3.386904097422250182, -1.772078739568806682, -0.9629521321246109489 ) ) ;
#12434 = CARTESIAN_POINT ( 'NONE',  ( 6.482950081930999531, -79.25674805011499302, -6.598019266050999754 ) ) ;
#12435 = CARTESIAN_POINT ( 'NONE',  ( -0.005523896504025000050, -53.73036543741000060, -12.55021156877000088 ) ) ;
#12436 = CARTESIAN_POINT ( 'NONE',  ( 9.655637611919594576, -75.99817351014564792, 6.698623033092742318 ) ) ;
#12437 = CARTESIAN_POINT ( 'NONE',  ( -3.547560735670601595, -85.83735716284299144, 1.500007025275386097 ) ) ;
#12438 = EDGE_LOOP ( 'NONE', ( #39330, #32679, #8462, #22484 ) ) ;
#12439 = CARTESIAN_POINT ( 'NONE',  ( -5.747123378374999980, -78.61567021304000491, 10.24856442990000005 ) ) ;
#12440 = CARTESIAN_POINT ( 'NONE',  ( 1.500000000000000000, -79.14999999999999147, 0.000000000000000000 ) ) ;
#12441 = CARTESIAN_POINT ( 'NONE',  ( -10.04834954474590170, -78.74359739231434219, -6.156343130738470393 ) ) ;
#12442 = FACE_OUTER_BOUND ( 'NONE', #10902, .T. ) ;
#12443 = CARTESIAN_POINT ( 'NONE',  ( 3.303001513109999898, -79.01917364576898706, -10.46681410869999951 ) ) ;
#12444 = CARTESIAN_POINT ( 'NONE',  ( 9.050966799188000067, -59.94999999969999749, -7.919595949288999570 ) ) ;
#12445 = CARTESIAN_POINT ( 'NONE',  ( 10.30382210470000182, -76.14431275097399521, -6.875193506978999558 ) ) ;
#12446 = CARTESIAN_POINT ( 'NONE',  ( 0.7004007752496766992, -78.56662277740376510, 11.72745275690763833 ) ) ;
#12447 = CARTESIAN_POINT ( 'NONE',  ( -10.36746145409134812, -55.03400544978683229, -7.635225828739184983 ) ) ;
#12448 = VERTEX_POINT ( 'NONE', #10906 ) ;
#12449 = CARTESIAN_POINT ( 'NONE',  ( 10.83083824887000013, -79.43986664982399759, -2.635819302916999618 ) ) ;
#12450 = CARTESIAN_POINT ( 'NONE',  ( -0.01192727606575066587, -77.37492492956100421, 9.363670505352606810 ) ) ;
#12451 = CARTESIAN_POINT ( 'NONE',  ( -11.00000000000000000, -77.59999999999999432, 0.000000000000000000 ) ) ;
#12452 = CARTESIAN_POINT ( 'NONE',  ( 3.229284361504000334, -79.59469609652998656, 10.68004289648999894 ) ) ;
#12453 = DIRECTION ( 'NONE',  ( 0.000000000000000000, -1.000000000000000000, 4.329869796038000067E-14 ) ) ;
#12454 = CARTESIAN_POINT ( 'NONE',  ( -7.624341766656999475, -60.06485146221000093, -10.42531125026000005 ) ) ;
#12455 = CARTESIAN_POINT ( 'NONE',  ( 1.365918550425730738, -82.06390440843598810, -0.6514700801450835632 ) ) ;
#12456 = FACE_OUTER_BOUND ( 'NONE', #48156, .T. ) ;
#12457 = DIRECTION ( 'NONE',  ( -0.9999999999998321343, 0.000000000000000000, -5.794542750377190787E-07 ) ) ;
#12458 = FACE_OUTER_BOUND ( 'NONE', #13760, .T. ) ;
#12459 = CARTESIAN_POINT ( 'NONE',  ( 0.9999999970759999579, -75.20000000292399989, 7.200000017194999380 ) ) ;
#12460 = EDGE_LOOP ( 'NONE', ( #42151, #11983, #15823, #56782 ) ) ;
#12461 = EDGE_LOOP ( 'NONE', ( #3122, #8607, #10005, #21969, #47 ) ) ;
#12462 = FACE_BOUND ( 'NONE', #45528, .T. ) ;
#12463 = TOROIDAL_SURFACE ( 'NONE', #13387, 17.50000000000000000, 5.000000000000000000 ) ;
#12464 = EDGE_LOOP ( 'NONE', ( #8626, #20039, #15240, #17105, #23362, #24319, #39159 ) ) ;
#12465 = CARTESIAN_POINT ( 'NONE',  ( -9.551084006840532936, -79.74233320338822750, 0.9337316140615163906 ) ) ;
#12466 = ORIENTED_EDGE ( 'NONE', *, *, #19715, .T. ) ;
#12467 = CARTESIAN_POINT ( 'NONE',  ( 1.310679582531385279, -81.79166666666901619, 0.7554284705563519831 ) ) ;
#12468 = CARTESIAN_POINT ( 'NONE',  ( -0.8033103333046999195, -77.19254838670400432, -10.88715107357000100 ) ) ;
#12469 = ADVANCED_FACE ( 'NONE', ( #26125 ), #2335, .F. ) ;
#12470 = CARTESIAN_POINT ( 'NONE',  ( -9.816946295765999864, -78.26783667140099965, -1.359421753724999959 ) ) ;
#12471 = EDGE_CURVE ( 'NONE', #30828, #45319, #39486, .T. ) ;
#12472 = CARTESIAN_POINT ( 'NONE',  ( 0.06516443285433551336, -78.22564617984212987, -9.249726598108379605 ) ) ;
#12473 = AXIS2_PLACEMENT_3D ( 'NONE', #4385, #45133, #36839 ) ;
#12474 = CARTESIAN_POINT ( 'NONE',  ( 8.554126827399000987, -79.96012667201070201, -7.255689219360999864 ) ) ;
#12475 = ORIENTED_EDGE ( 'NONE', *, *, #10515, .F. ) ;
#12476 = ORIENTED_EDGE ( 'NONE', *, *, #13739, .T. ) ;
#12477 = CARTESIAN_POINT ( 'NONE',  ( -6.545454099276200033, -77.53772617611215878, 6.535861892516707350 ) ) ;
#12478 = CARTESIAN_POINT ( 'NONE',  ( 10.42639159904000046, -77.10027333183208498, -2.617796444239999687 ) ) ;
#12479 = CARTESIAN_POINT ( 'NONE',  ( -1.243547092045951263, -77.51458333333332007, -9.500000000000003553 ) ) ;
#12480 = CARTESIAN_POINT ( 'NONE',  ( -1.182190922889000184, -78.94543294674498668, -9.631881180458998770 ) ) ;
#12481 = CIRCLE ( 'NONE', #7771, 0.5000000000000006661 ) ;
#12482 = CARTESIAN_POINT ( 'NONE',  ( 3.673449851479000383, -75.85705099976999577, 11.86240085298999958 ) ) ;
#12483 = CARTESIAN_POINT ( 'NONE',  ( -6.722882011319116558, -79.46222606496974095, -6.711992429377692915 ) ) ;
#12484 = CARTESIAN_POINT ( 'NONE',  ( -9.497876546326999403, -77.35168256874098347, -0.2008509664869000122 ) ) ;
#12485 = CARTESIAN_POINT ( 'NONE',  ( -9.459258931978000717, -79.88874279519899346, 5.442530770145999952 ) ) ;
#12486 = ADVANCED_FACE ( 'NONE', ( #3693 ), #29173, .T. ) ;
#12487 = AXIS2_PLACEMENT_3D ( 'NONE', #52885, #26873, #9177 ) ;
#12488 = CARTESIAN_POINT ( 'NONE',  ( 12.66761570929000058, -17.77632520104999969, -1.696752301450999978 ) ) ;
#12489 = CARTESIAN_POINT ( 'NONE',  ( -0.6804402928152999408, -82.23668930757399664, -1.032525207220000185 ) ) ;
#12490 = CARTESIAN_POINT ( 'NONE',  ( -11.75000000000000000, -76.70000000000000284, 1.487410190129999909E-14 ) ) ;
#12491 = ORIENTED_EDGE ( 'NONE', *, *, #39130, .T. ) ;
#12492 = CARTESIAN_POINT ( 'NONE',  ( -5.528827828690000779, -79.16377338295399113, -10.74483463111999981 ) ) ;
#12493 = DIRECTION ( 'NONE',  ( 1.000000000000000000, 0.000000000000000000, 0.000000000000000000 ) ) ;
#12494 = CARTESIAN_POINT ( 'NONE',  ( -10.26943924278000075, -78.65863669146300197, 6.168847710360999770 ) ) ;
#12495 = CARTESIAN_POINT ( 'NONE',  ( -10.18127254044999930, -18.61355771719999908, -7.633407132383000615 ) ) ;
#12497 = PLANE ( 'NONE',  #55336 ) ;
#12496 = CARTESIAN_POINT ( 'NONE',  ( 7.718368845804999268, -57.05199022587000002, 10.07722254368999870 ) ) ;
#12498 = CARTESIAN_POINT ( 'NONE',  ( 9.007844276740291534, -79.37087089868364842, 2.420897759216547040 ) ) ;
#12499 = CARTESIAN_POINT ( 'NONE',  ( -8.397876581538000096, -79.87585733274299571, 6.655340051815000102 ) ) ;
#12500 = CARTESIAN_POINT ( 'NONE',  ( -0.5900578684300998855, -82.27212043593699775, -1.108170840844000082 ) ) ;
#12501 = CARTESIAN_POINT ( 'NONE',  ( -8.764875654205999567, -77.76938450272599823, 7.071839882566000490 ) ) ;
#12502 = CARTESIAN_POINT ( 'NONE',  ( 0.6457562008196999770, -80.45297733623330316, -11.23729128717999970 ) ) ;
#12503 = ORIENTED_EDGE ( 'NONE', *, *, #31416, .F. ) ;
#12504 = CARTESIAN_POINT ( 'NONE',  ( 9.238576773750208915, -80.29311845634506994, 5.559101997765116820 ) ) ;
#12505 = ADVANCED_FACE ( 'NONE', ( #36155 ), #1803, .T. ) ;
#12506 = CARTESIAN_POINT ( 'NONE',  ( -1.886823409076999969, -55.03680315604999151, 12.68610076202999792 ) ) ;
#12507 = CARTESIAN_POINT ( 'NONE',  ( -12.00000000000000000, -23.25000000000000000, 0.000000000000000000 ) ) ;
#12508 = CARTESIAN_POINT ( 'NONE',  ( -3.254128868261999763, -1.540113550428000133, 0.1923296600005000023 ) ) ;
#12509 = CARTESIAN_POINT ( 'NONE',  ( -3.827647950032363244, -78.04671362439400184, -10.14077206697919387 ) ) ;
#12510 = CARTESIAN_POINT ( 'NONE',  ( -4.647088938219000376, -78.10731010046200140, 10.20895072913000057 ) ) ;
#12511 = CARTESIAN_POINT ( 'NONE',  ( -12.43421868114999995, -54.36340276600000010, 1.197355605038999959 ) ) ;
#12512 = DIRECTION ( 'NONE',  ( 0.000000000000000000, 1.000000000000000000, 0.000000000000000000 ) ) ;
#12513 = CARTESIAN_POINT ( 'NONE',  ( 0.9113424693931000409, -61.62535793526999583, 12.54674099561999867 ) ) ;
#12514 = DIRECTION ( 'NONE',  ( 1.000000000000000000, 0.000000000000000000, 0.000000000000000000 ) ) ;
#12515 = CARTESIAN_POINT ( 'NONE',  ( -1.832761557483999937, -85.98999735065198990, 3.751106806215999789 ) ) ;
#12516 = DIRECTION ( 'NONE',  ( 0.000000000000000000, 1.000000000000000000, 0.000000000000000000 ) ) ;
#12517 = TOROIDAL_SURFACE ( 'NONE', #57768, 17.50000000000000000, 5.000000000000000000 ) ;
#12518 = CARTESIAN_POINT ( 'NONE',  ( 9.498848458907630743, -79.03416273108655332, 0.1004247326035953569 ) ) ;
#12519 = B_SPLINE_SURFACE_WITH_KNOTS ( 'NONE', 3, 3, ( 
 ( #39203, #57218, #57794, #34766, #43938, #3489, #21493, #39499, #40970, #58088, #53967, #17648, #35637, #4667, #27664, #45115, #36530, #18828, #27075 ),
 ( #8790, #32379, #36820, #36239, #54262, #31199, #53665, #40677, #13504, #35939, #9089, #26486, #31496, #22960, #49543, #18248, #269, #22666, #18539 ),
 ( #40378, #54554, #54837, #27374, #9385, #41258, #14094, #32093, #50133, #14380, #13795, #49239, #9676, #4955, #45708, #13205, #31796, #26781, #5245 ),
 ( #561, #49838, #44811, #45412, #4363, #23249, #844, #8490, #40071, #22364, #44510, #4060, #22064, #58385, #17948, #37700, #38280, #37988, #55125 ) ),
 .UNSPECIFIED., .F., .F., .F.,
 ( 4, 4 ),
 ( 4, 1, 1, 1, 1, 1, 1, 1, 1, 1, 1, 1, 1, 1, 1, 1, 4 ),
 ( -0.3708084972812999980, 1.370808497280999960 ),
 ( -0.01116670151518999940, 0.02512507840917000204, 0.06141685833353999896, 0.09770863825790000734, 0.1340004181822999907, 0.1702921981065999846, 0.2065839780310000096, 0.2428757579554000068, 0.2791675378797000007, 0.3154593178041000257, 0.3517510977284000195, 0.3880428776527999890, 0.4243346575772000140, 0.4606264375015000079, 0.4969182174258999773, 0.5332099973503000578, 0.5695017772746000517 ),
 .UNSPECIFIED. ) ;
#12520 = CARTESIAN_POINT ( 'NONE',  ( 8.308415499261105452, -76.38746760283510184, -8.308548603794546850 ) ) ;
#12521 = CARTESIAN_POINT ( 'NONE',  ( -10.68734765800000019, -76.66107590507699854, -2.735374635455000369 ) ) ;
#12522 = CARTESIAN_POINT ( 'NONE',  ( 1.081160367018396462, -81.89214477630333988, 0.6272441749643766773 ) ) ;
#12523 = FACE_OUTER_BOUND ( 'NONE', #22399, .T. ) ;
#12524 = CARTESIAN_POINT ( 'NONE',  ( 0.000000000000000000, -3.500000000000000000, 0.000000000000000000 ) ) ;
#12525 = DIRECTION ( 'NONE',  ( 0.000000000000000000, -1.000000000000000000, 0.000000000000000000 ) ) ;
#12526 = CARTESIAN_POINT ( 'NONE',  ( -5.827680902778979544, -80.17946448389406555, -9.033442447713206036 ) ) ;
#12527 = CARTESIAN_POINT ( 'NONE',  ( -11.75935053634283989, -76.25833333328885999, 2.506420011343689414 ) ) ;
#12528 = CARTESIAN_POINT ( 'NONE',  ( 11.21501439771859054, -80.09840187879784423, -0.2123206566945571028 ) ) ;
#12529 = AXIS2_PLACEMENT_3D ( 'NONE', #48392, #17080, #21215 ) ;
#12530 = AXIS2_PLACEMENT_3D ( 'NONE', #23484, #794, #27900 ) ;
#12531 = CARTESIAN_POINT ( 'NONE',  ( -9.625846388754000671, -79.11728850969700488, -7.214584339064000318 ) ) ;
#12532 = CARTESIAN_POINT ( 'NONE',  ( 9.500000000000000000, -78.54999999999999716, 0.000000000000000000 ) ) ;
#12533 = CARTESIAN_POINT ( 'NONE',  ( -0.2732061834123999944, -79.20034006197499821, 11.25874428786999992 ) ) ;
#12534 = CARTESIAN_POINT ( 'NONE',  ( -10.75000000000000000, -77.60000000000000853, 2.252154972635999871E-14 ) ) ;
#12535 = ORIENTED_EDGE ( 'NONE', *, *, #12904, .F. ) ;
#12536 = ORIENTED_EDGE ( 'NONE', *, *, #209, .T. ) ;
#12537 = CARTESIAN_POINT ( 'NONE',  ( -1.318114156682550941, -24.73572477192366037, 12.70261578162813265 ) ) ;
#12538 = ORIENTED_EDGE ( 'NONE', *, *, #47199, .F. ) ;
#12539 = ORIENTED_EDGE ( 'NONE', *, *, #33081, .T. ) ;
#12540 = CARTESIAN_POINT ( 'NONE',  ( 3.169069393497101483, -3.500000000000000444, -1.511488537269458643 ) ) ;
#12541 = CARTESIAN_POINT ( 'NONE',  ( -1.199500263597274685, -78.44791666666668561, 0.9218200799623673669 ) ) ;
#12542 = CARTESIAN_POINT ( 'NONE',  ( 9.125560752801000319, -79.27717617799699212, -5.991619725684000031 ) ) ;
#12543 = CARTESIAN_POINT ( 'NONE',  ( 3.579488350411999864, -79.65606415136248586, 0.2664741063475999927 ) ) ;
#12544 = CARTESIAN_POINT ( 'NONE',  ( -1.627038676344989110, -79.28854989600672809, 9.360266054361467525 ) ) ;
#12545 = VERTEX_POINT ( 'NONE', #27285 ) ;
#12546 = DIRECTION ( 'NONE',  ( 2.706894537570999990E-12, 1.000000000000000000, 1.232851854724000084E-11 ) ) ;
#12547 = CARTESIAN_POINT ( 'NONE',  ( -1.317308456444000075, -79.12212284379999971, -12.28806242769000079 ) ) ;
#12548 = ORIENTED_EDGE ( 'NONE', *, *, #14195, .T. ) ;
#12549 = VERTEX_POINT ( 'NONE', #32001 ) ;
#12550 = FACE_OUTER_BOUND ( 'NONE', #50622, .T. ) ;
#12551 = VECTOR ( 'NONE', #13287, 1000.000000000000000 ) ;
#12552 = CARTESIAN_POINT ( 'NONE',  ( 5.392351874751835084, -79.79999999999999716, 10.61425309677364837 ) ) ;
#12553 = CARTESIAN_POINT ( 'NONE',  ( -10.27037232371433895, -80.07614521482391012, 3.176628361632590991 ) ) ;
#12554 = CARTESIAN_POINT ( 'NONE',  ( 0.000000000000000000, 4.040000000000000036, 0.000000000000000000 ) ) ;
#12555 = CARTESIAN_POINT ( 'NONE',  ( 3.140027144888942967, -86.25171435493598437, -1.398030157552127895 ) ) ;
#12556 = CARTESIAN_POINT ( 'NONE',  ( -2.014760465083978325, -86.03700509404642105, 2.765359799179270883 ) ) ;
#12557 = CARTESIAN_POINT ( 'NONE',  ( 5.921937764992279973, -79.02083333333980875, 10.24701051719076439 ) ) ;
#12558 = EDGE_CURVE ( 'NONE', #52926, #39245, #16867, .T. ) ;
#12559 = CARTESIAN_POINT ( 'NONE',  ( -3.078285613438000112, -78.22578184934000944, 12.42192206172999924 ) ) ;
#12560 = AXIS2_PLACEMENT_3D ( 'NONE', #41259, #18829, #47873 ) ;
#12561 = CARTESIAN_POINT ( 'NONE',  ( 7.781700644545999523, -76.83820410512299759, 7.610227757096000190 ) ) ;
#12562 = CARTESIAN_POINT ( 'NONE',  ( -8.724187533938204453, -78.62698228320140004, -3.074223295207495266 ) ) ;
#12563 = CARTESIAN_POINT ( 'NONE',  ( 3.843843749258000209, -82.73863223182399906, -0.2533585598290000185 ) ) ;
#12564 = B_SPLINE_CURVE_WITH_KNOTS ( 'NONE', 3,
 ( #17724, #35711, #48444, #44009 ),
 .UNSPECIFIED., .F., .F.,
 ( 4, 4 ),
 ( 0.000000000000000000, 1.000000000000000000 ),
 .UNSPECIFIED. ) ;
#12565 = CARTESIAN_POINT ( 'NONE',  ( -8.485281374238999419, -55.64999999967000122, 8.485281374238999419 ) ) ;
#12566 = CARTESIAN_POINT ( 'NONE',  ( -2.299428515032341025, -3.037945768799499291, 2.296401124946453542 ) ) ;
#12567 = CARTESIAN_POINT ( 'NONE',  ( 2.358048202871999788, -81.09475264934799554, 2.646615284092999509 ) ) ;
#12568 = CARTESIAN_POINT ( 'NONE',  ( 12.00000000000000000, -23.25000000000000000, 1.250000000000000000 ) ) ;
#12569 = CARTESIAN_POINT ( 'NONE',  ( 0.1745084697671999974, -85.80069503318799207, 3.542747450414000188 ) ) ;
#12570 = CARTESIAN_POINT ( 'NONE',  ( -3.448863046786000197, -1.817410797673999934, -1.608907009436000068 ) ) ;
#12571 = CARTESIAN_POINT ( 'NONE',  ( 0.7034081407617550630, -79.57886472181323256, 1.062556203884562844 ) ) ;
#12572 = ORIENTED_EDGE ( 'NONE', *, *, #43359, .T. ) ;
#12573 = CARTESIAN_POINT ( 'NONE',  ( -7.606021324617000090, -60.22158946241999899, -10.52692925329000140 ) ) ;
#12574 = EDGE_CURVE ( 'NONE', #28211, #25253, #40503, .T. ) ;
#12575 = LINE ( 'NONE', #3434, #14733 ) ;
#12576 = CARTESIAN_POINT ( 'NONE',  ( -1.179157772963000061, -82.13943273986299687, 0.6230118014947999550 ) ) ;
#12577 = CARTESIAN_POINT ( 'NONE',  ( -12.43569863939999998, -17.11799904157000185, -0.4278707626186999957 ) ) ;
#12578 = FACE_OUTER_BOUND ( 'NONE', #6821, .T. ) ;
#12579 = CARTESIAN_POINT ( 'NONE',  ( 8.212410987726999068, -78.00373067278798089, -6.936771999183999782 ) ) ;
#12580 = CARTESIAN_POINT ( 'NONE',  ( 0.8898229089128317781, -25.02324531182464185, -12.70296869045280275 ) ) ;
#12581 = CARTESIAN_POINT ( 'NONE',  ( -4.687723163076999100, -76.48740961512999093, 11.43893144258999861 ) ) ;
#12582 = ORIENTED_EDGE ( 'NONE', *, *, #52968, .F. ) ;
#12583 = CARTESIAN_POINT ( 'NONE',  ( -0.9849936891751999157, -80.86803245780032512, -11.22225356808999841 ) ) ;
#12584 = DIRECTION ( 'NONE',  ( 1.000000000000000000, 0.000000000000000000, 0.000000000000000000 ) ) ;
#12585 = CARTESIAN_POINT ( 'NONE',  ( -10.98362417419999915, -18.84999999999999787, -0.5999999999999999778 ) ) ;
#12586 = CARTESIAN_POINT ( 'NONE',  ( 7.919595949288999570, -55.65000000893999754, 9.050966798898000931 ) ) ;
#12587 = CARTESIAN_POINT ( 'NONE',  ( 1.846868607710999921, -78.81640489213999956, 9.341276817324001058 ) ) ;
#12588 = CARTESIAN_POINT ( 'NONE',  ( -3.975720615853999274, -86.19283349427999497, 0.4344903803919999974 ) ) ;
#12589 = CARTESIAN_POINT ( 'NONE',  ( 4.592783297679469356, -79.93999167834631692, 9.722085715425176744 ) ) ;
#12590 = CARTESIAN_POINT ( 'NONE',  ( 1.293420685949000060, -79.34100130914399074, 0.7912046490545000532 ) ) ;
#12591 = EDGE_CURVE ( 'NONE', #47034, #3351, #54174, .T. ) ;
#12592 = ORIENTED_EDGE ( 'NONE', *, *, #50508, .T. ) ;
#12593 = CARTESIAN_POINT ( 'NONE',  ( 0.000000000000000000, -45.69638659094999866, 0.000000000000000000 ) ) ;
#12594 = CARTESIAN_POINT ( 'NONE',  ( 1.439896632895302009, -78.83541666666664582, -11.00000000000000000 ) ) ;
#12595 = CARTESIAN_POINT ( 'NONE',  ( 3.399999999999690381, -78.72609999968184979, 6.799999999999410072 ) ) ;
#12596 = VERTEX_POINT ( 'NONE', #13120 ) ;
#12597 = VERTEX_POINT ( 'NONE', #9589 ) ;
#12598 = CARTESIAN_POINT ( 'NONE',  ( 10.94008345411999983, -78.12118338113400284, 0.05084573220516999670 ) ) ;
#12599 = VECTOR ( 'NONE', #24874, 1000.000000000000000 ) ;
#12600 = CARTESIAN_POINT ( 'NONE',  ( -8.111636311582410386, -55.28385402668900639, -7.429974109819841743 ) ) ;
#12601 = CARTESIAN_POINT ( 'NONE',  ( 11.28909814340999951, -79.98006123089598418, -1.860932571041999939 ) ) ;
#12602 = ORIENTED_EDGE ( 'NONE', *, *, #21468, .F. ) ;
#12603 = B_SPLINE_CURVE_WITH_KNOTS ( 'NONE', 3,
 ( #8318, #22480, #17767, #40490, #31612, #22771, #40781, #45519, #18355, #44332, #36345, #48773, #39895, #31024, #50821, #10960, #32776, #10365 ),
 .UNSPECIFIED., .F., .F.,
 ( 4, 2, 2, 2, 2, 2, 2, 2, 4 ),
 ( 0.000000000000000000, 0.1249999999999999445, 0.2500000000000000000, 0.3750000000000000555, 0.5000000000000001110, 0.6250000000000000000, 0.7500000000000000000, 0.8749999999999998890, 1.000000000000000000 ),
 .UNSPECIFIED. ) ;
#12604 = CARTESIAN_POINT ( 'NONE',  ( 0.3923696854197999961, -77.38648093799099570, -11.92498586577000097 ) ) ;
#12605 = VERTEX_POINT ( 'NONE', #49755 ) ;
#12606 = B_SPLINE_CURVE_WITH_KNOTS ( 'NONE', 3,
 ( #30421, #48453, #25993, #12991, #44017, #39861 ),
 .UNSPECIFIED., .F., .F.,
 ( 4, 2, 4 ),
 ( 0.000000000000000000, 0.5000000000000000000, 1.000000000000000000 ),
 .UNSPECIFIED. ) ;
#12607 = EDGE_LOOP ( 'NONE', ( #19375, #27047, #19191, #35608, #49345, #57470, #33009, #38594, #21394 ) ) ;
#12608 = CARTESIAN_POINT ( 'NONE',  ( -9.344374848299676017, -78.14684388159851380, 7.168986247577478821 ) ) ;
#12609 = CARTESIAN_POINT ( 'NONE',  ( 3.366547962069000199, -79.90301558626953238, -9.168809063548000182 ) ) ;
#12610 = ORIENTED_EDGE ( 'NONE', *, *, #19106, .T. ) ;
#12611 = CARTESIAN_POINT ( 'NONE',  ( -9.250000000000000000, -79.09999999999999432, 1.813240672189999963E-14 ) ) ;
#12612 = ORIENTED_EDGE ( 'NONE', *, *, #39116, .T. ) ;
#12613 = CARTESIAN_POINT ( 'NONE',  ( -0.2776637860332794583, -79.54227634049593121, 1.244172164868827757 ) ) ;
#12614 = CARTESIAN_POINT ( 'NONE',  ( 2.194290298650410698, -78.99318692756679638, -3.799401814995372995 ) ) ;
#12615 = CARTESIAN_POINT ( 'NONE',  ( 12.60354432324999863, -56.04899162853999428, -1.750000000000000000 ) ) ;
#12616 = CARTESIAN_POINT ( 'NONE',  ( 0.3135214471491306609, -18.31418618813953358, 10.99610567419586182 ) ) ;
#12617 = CARTESIAN_POINT ( 'NONE',  ( 8.838834764832000701, -55.54999999966999980, -8.838834764832000701 ) ) ;
#12618 = EDGE_CURVE ( 'NONE', #23838, #38250, #45321, .T. ) ;
#12619 = CARTESIAN_POINT ( 'NONE',  ( 12.70457892003493150, -61.97873330296430794, -0.5105076820992421327 ) ) ;
#12620 = AXIS2_PLACEMENT_3D ( 'NONE', #13861, #31857, #49898 ) ;
#12621 = CARTESIAN_POINT ( 'NONE',  ( -1.158060974166144508, -77.79422440721735654, 0.9671104533053733743 ) ) ;
#12622 = CARTESIAN_POINT ( 'NONE',  ( 8.564407298655666523, -78.81931219690746104, -3.494578516088384657 ) ) ;
#12623 = EDGE_CURVE ( 'NONE', #30461, #47356, #58305, .T. ) ;
#12624 = DIRECTION ( 'NONE',  ( 0.000000000000000000, 0.7071067811866525998, -0.7071067811864425456 ) ) ;
#12625 = CARTESIAN_POINT ( 'NONE',  ( 0.6660448984561999630, -82.05675264934798463, -4.121397237571000183 ) ) ;
#12626 = CARTESIAN_POINT ( 'NONE',  ( 7.000738396026999766, -77.01039334753599519, -6.633884475650999590 ) ) ;
#12627 = CARTESIAN_POINT ( 'NONE',  ( -0.9995835529977281642, -83.44791666666662877, 0.7681833999686391579 ) ) ;
#12628 = LINE ( 'NONE', #30331, #8480 ) ;
#12629 = CARTESIAN_POINT ( 'NONE',  ( 9.500000000000000000, -77.64999999999999147, 0.000000000000000000 ) ) ;
#12630 = CARTESIAN_POINT ( 'NONE',  ( -0.1131650557487513253, -80.86835801496910392, -1.320356500459302307 ) ) ;
#12631 = CARTESIAN_POINT ( 'NONE',  ( 6.874986978319857833, -78.37672046791054470, 9.923497271207523340 ) ) ;
#12632 = CARTESIAN_POINT ( 'NONE',  ( -12.00000000000000000, -77.79999999999999716, 0.000000000000000000 ) ) ;
#12633 = AXIS2_PLACEMENT_3D ( 'NONE', #40425, #35987, #44558 ) ;
#12634 = B_SPLINE_SURFACE_WITH_KNOTS ( 'NONE', 3, 3, ( 
 ( #16409, #29961, #23944, #1533 ),
 ( #14502, #46710, #6230, #50539 ),
 ( #41668, #5077, #41380, #23072 ),
 ( #49962, #36939, #28661, #15087 ),
 ( #19526, #24246, #42262, #51127 ),
 ( #54950, #18661, #19824, #36649 ),
 ( #31917, #1828, #54668, #28363 ),
 ( #50833, #33083, #54385, #46410 ),
 ( #41086, #963, #678, #41960 ),
 ( #32493, #13922, #10680, #32786 ),
 ( #10093, #37519, #5361, #9503 ),
 ( #23655, #28072, #46122, #18946 ),
 ( #1248, #27490, #55537, #14209 ),
 ( #45531, #37228, #32206, #5646 ),
 ( #50247, #9798, #27781, #45826 ),
 ( #23369, #19236, #55245, #14791 ),
 ( #10379, #5939, #20686, #33672 ) ),
 .UNSPECIFIED., .F., .F., .F.,
 ( 4, 1, 1, 1, 1, 1, 1, 1, 1, 1, 1, 1, 1, 1, 4 ),
 ( 4, 4 ),
 ( -0.01011400514355999952, 0.000000000000000000, 0.08333333333333001192, 0.1666666666667000196, 0.2500000000000000000, 0.3333333333333000081, 0.4166666666666999919, 0.5000000000000000000, 0.5833333333333000637, 0.6666666666667000474, 0.7500000000000000000, 0.8333333333333000637, 0.9166666666667000474, 1.000000000000000000, 1.010365328128000062 ),
 ( -0.3559705546945999832, 1.357612395641000003 ),
 .UNSPECIFIED. ) ;
#12635 = ADVANCED_FACE ( 'NONE', ( #49155 ), #8707, .F. ) ;
#12636 = B_SPLINE_CURVE_WITH_KNOTS ( 'NONE', 3,
 ( #3668, #39674, #39394, #34370, #12240, #2811 ),
 .UNSPECIFIED., .F., .F.,
 ( 4, 1, 1, 4 ),
 ( 0.000000000000000000, 0.3333333333333000081, 0.6666666666667000474, 1.000000000000000000 ),
 .UNSPECIFIED. ) ;
#12637 = CARTESIAN_POINT ( 'NONE',  ( 0.9655213319334129407, -80.02944677308721566, -1.162632870702606791 ) ) ;
#12638 = CARTESIAN_POINT ( 'NONE',  ( -3.759408710945999488, -77.04890421901679076, -8.530078903752000841 ) ) ;
#12639 = CARTESIAN_POINT ( 'NONE',  ( 1.980532734072999901, -56.03767313155999830, -12.80090744964999949 ) ) ;
#12640 = CARTESIAN_POINT ( 'NONE',  ( 0.000000000000000000, -22.78578169018998878, -13.15643568216998638 ) ) ;
#12641 = CARTESIAN_POINT ( 'NONE',  ( -3.600395895414000069, -77.34004702781498963, 11.61979689923000159 ) ) ;
#12642 = CARTESIAN_POINT ( 'NONE',  ( -1.980532758766000212, -59.56256650660999696, 12.80088938804999898 ) ) ;
#12644 = DIRECTION ( 'NONE',  ( 1.000000000000000000, 0.000000000000000000, 0.000000000000000000 ) ) ;
#12643 = CARTESIAN_POINT ( 'NONE',  ( -10.06032152983862638, -75.80000000000001137, 6.218695677770802455 ) ) ;
#12645 = CARTESIAN_POINT ( 'NONE',  ( -0.5793938177159999592, -82.55061671381200483, 1.349352049262000142 ) ) ;
#12646 = CARTESIAN_POINT ( 'NONE',  ( -8.988913058593215766, -79.55386370958336784, 5.895957875921411961 ) ) ;
#12647 = ORIENTED_EDGE ( 'NONE', *, *, #13563, .F. ) ;
#12648 = CARTESIAN_POINT ( 'NONE',  ( -0.7446082967701634914, -78.77994009691290955, 12.02413132939186369 ) ) ;
#12649 = CARTESIAN_POINT ( 'NONE',  ( -11.66126045851000015, -79.67109097853600019, 3.001209278140000158 ) ) ;
#12650 = CARTESIAN_POINT ( 'NONE',  ( 5.649609181776704681, -79.42525939925479861, -7.715451315860589965 ) ) ;
#12651 = CARTESIAN_POINT ( 'NONE',  ( 10.26420232462597149, -79.69374999999999432, 6.287639862081866760 ) ) ;
#12652 = CARTESIAN_POINT ( 'NONE',  ( -10.30767511324000019, -60.54763733864000130, 7.634418707071000121 ) ) ;
#12653 = CARTESIAN_POINT ( 'NONE',  ( 0.6116024548114998849, -1.269669754918000049, -3.650360381117999431 ) ) ;
#12654 = CARTESIAN_POINT ( 'NONE',  ( -8.050862028188001673, -79.15888192999699413, 5.553975462107000105 ) ) ;
#12655 = CARTESIAN_POINT ( 'NONE',  ( 12.54673349184999864, -24.82806887810999896, -0.9076721992841999542 ) ) ;
#12656 = FACE_OUTER_BOUND ( 'NONE', #6363, .T. ) ;
#12657 = EDGE_LOOP ( 'NONE', ( #21849, #57626 ) ) ;
#12658 = CARTESIAN_POINT ( 'NONE',  ( 0.000000000000000000, -77.74999999981000087, 0.000000000000000000 ) ) ;
#12659 = CARTESIAN_POINT ( 'NONE',  ( 8.277425028854000999, -79.61486001420199443, 5.137022432363000490 ) ) ;
#12660 = CARTESIAN_POINT ( 'NONE',  ( -3.140976149987326327, -1.624123246795792008, -0.9279992776312928626 ) ) ;
#12661 = CARTESIAN_POINT ( 'NONE',  ( -10.18589234709999936, -60.08917565288000162, -7.641012386057000505 ) ) ;
#12662 = CARTESIAN_POINT ( 'NONE',  ( -2.859007450852999899, -84.83242953870899328, -2.100149760972999768 ) ) ;
#12663 = CIRCLE ( 'NONE', #9863, 0.5999999999999999778 ) ;
#12664 = ORIENTED_EDGE ( 'NONE', *, *, #43490, .T. ) ;
#12665 = CARTESIAN_POINT ( 'NONE',  ( 12.50000000000000000, -55.35321828636000419, -1.250000000000000000 ) ) ;
#12666 = CYLINDRICAL_SURFACE ( 'NONE', #50538, 9.549999999999998934 ) ;
#12667 = CARTESIAN_POINT ( 'NONE',  ( -2.839805762151337731, -1.041666666666666741, -1.636761686205423949 ) ) ;
#12668 = ORIENTED_EDGE ( 'NONE', *, *, #3364, .F. ) ;
#12669 = EDGE_CURVE ( 'NONE', #38673, #4989, #26990, .T. ) ;
#12670 = CARTESIAN_POINT ( 'NONE',  ( 1.618935784558559021, -54.87248831271503491, 12.52134385796530047 ) ) ;
#12671 = CARTESIAN_POINT ( 'NONE',  ( -7.633502222218000455, -55.59895684611999656, -10.36289759015999934 ) ) ;
#12672 = AXIS2_PLACEMENT_3D ( 'NONE', #25170, #43193, #48485 ) ;
#12673 = CARTESIAN_POINT ( 'NONE',  ( -5.726462542197000793, -79.84499576192899895, -7.912542777261000637 ) ) ;
#12674 = VERTEX_POINT ( 'NONE', #19606 ) ;
#12675 = VERTEX_POINT ( 'NONE', #46791 ) ;
#12676 = CARTESIAN_POINT ( 'NONE',  ( 0.03300762091332999637, -76.13364338555700783, 11.93139356344000035 ) ) ;
#12677 = CARTESIAN_POINT ( 'NONE',  ( -0.2201363562291999698, -79.36327907013999550, -1.483758735329000045 ) ) ;
#12678 = CARTESIAN_POINT ( 'NONE',  ( 0.3645270829314000149, -79.35220299592999993, -1.380445500850000062 ) ) ;
#12679 = EDGE_LOOP ( 'NONE', ( #25171, #48980, #39361, #42980, #22567, #41808, #41449, #10273, #9926, #11180, #48692, #48819 ) ) ;
#12680 = CARTESIAN_POINT ( 'NONE',  ( 7.092659876394000307, -77.93792694988499647, 6.312768414564000174 ) ) ;
#12681 = CARTESIAN_POINT ( 'NONE',  ( -4.475319841928504516, -78.93676327900720935, -8.610768833002914846 ) ) ;
#12682 = CARTESIAN_POINT ( 'NONE',  ( 0.9951994886139982066, -80.29861577946837770, -0.7569065563915547967 ) ) ;
#12683 = CARTESIAN_POINT ( 'NONE',  ( 12.32442898454999813, -77.89680700753000053, -3.452188809138999837 ) ) ;
#12684 = CARTESIAN_POINT ( 'NONE',  ( -9.524774638983998898, -77.20572130948103506, 5.924253427061998423 ) ) ;
#12685 = CARTESIAN_POINT ( 'NONE',  ( 1.412628807274971088, -86.36264282632899381, 3.255037163431034219 ) ) ;
#12686 = DIRECTION ( 'NONE',  ( -0.7026410690473252618, 0.1122098755728027641, -0.7026410690473252618 ) ) ;
#12687 = CARTESIAN_POINT ( 'NONE',  ( 3.538064976920356042, -79.94385801930759783, 8.546548758931297840 ) ) ;
#12688 = CARTESIAN_POINT ( 'NONE',  ( 10.93619165073445210, -80.21437323052235513, 1.947132623917049887 ) ) ;
#12689 = ORIENTED_EDGE ( 'NONE', *, *, #27360, .T. ) ;
#12690 = CARTESIAN_POINT ( 'NONE',  ( -4.391024480082000636, -79.21395401111398371, -10.37534762698999913 ) ) ;
#12691 = EDGE_CURVE ( 'NONE', #46623, #2183, #35916, .T. ) ;
#12692 = CARTESIAN_POINT ( 'NONE',  ( -2.463318457235554426, -77.20365170611822236, -8.921952837938405878 ) ) ;
#12693 = CARTESIAN_POINT ( 'NONE',  ( 1.086271320152000008, -79.49177606238200156, -0.9110860045855999623 ) ) ;
#12694 = CARTESIAN_POINT ( 'NONE',  ( -3.244532303892139424, -76.95155671043232815, -10.73753325156647520 ) ) ;
#12695 = CARTESIAN_POINT ( 'NONE',  ( 1.301001062148999798, -78.42132866053150053, 0.2190019327816999928 ) ) ;
#12696 = CARTESIAN_POINT ( 'NONE',  ( 12.92177931904999966, -21.75736537952000305, 2.062503053667999797 ) ) ;
#12697 = CARTESIAN_POINT ( 'NONE',  ( 1.538071403319964281, -76.66458333333332575, 11.75000000000000711 ) ) ;
#12698 = DIRECTION ( 'NONE',  ( 1.000000000000000000, 0.000000000000000000, 0.000000000000000000 ) ) ;
#12699 = FACE_OUTER_BOUND ( 'NONE', #15304, .T. ) ;
#12700 = CARTESIAN_POINT ( 'NONE',  ( 7.917622607290999426, -78.86915472700400187, 7.861478989701000231 ) ) ;
#12701 = CARTESIAN_POINT ( 'NONE',  ( -10.12290050124000018, -23.24999999991999644, -7.648026767085999822 ) ) ;
#12702 = CARTESIAN_POINT ( 'NONE',  ( -1.249764222956683657, -83.09108160190875481, 0.1462821142628205062 ) ) ;
#12703 = CARTESIAN_POINT ( 'NONE',  ( 3.934294415302999948, -81.01217470615398497, 1.388482249934000157 ) ) ;
#12704 = CARTESIAN_POINT ( 'NONE',  ( -0.5999999999999999778, -18.84999999999999787, 12.00000000000000000 ) ) ;
#12705 = ADVANCED_FACE ( 'NONE', ( #6609, #37312 ), #11343, .F. ) ;
#12706 = ORIENTED_EDGE ( 'NONE', *, *, #41494, .T. ) ;
#12707 = CARTESIAN_POINT ( 'NONE',  ( 0.4426188121580000301, -82.10602282125999807, -1.400191678299000042 ) ) ;
#12708 = CIRCLE ( 'NONE', #35319, 4.000000000000000000 ) ;
#12709 = CARTESIAN_POINT ( 'NONE',  ( 1.426111243542000029, -80.22582157143999382, 0.3502211593775000353 ) ) ;
#12710 = CARTESIAN_POINT ( 'NONE',  ( 7.648026768008000076, -55.55000001556999933, -10.12290050216000026 ) ) ;
#12711 = CARTESIAN_POINT ( 'NONE',  ( 6.035966914210000311, -77.89908533016399872, 10.34809972146999968 ) ) ;
#12712 = CARTESIAN_POINT ( 'NONE',  ( -12.90000000000000036, -5.899999999999999467, 0.000000000000000000 ) ) ;
#12713 = CARTESIAN_POINT ( 'NONE',  ( -0.5544740949720999845, -82.11317685150999068, 1.570928860995999932 ) ) ;
#12714 = CARTESIAN_POINT ( 'NONE',  ( 11.83900414546000057, -78.31650993477799716, -1.507807444711000144 ) ) ;
#12715 = CARTESIAN_POINT ( 'NONE',  ( -5.505695391233000002, -78.70715194988498808, -8.014431902511001127 ) ) ;
#12716 = CARTESIAN_POINT ( 'NONE',  ( -10.41144098943260055, -23.52546312060280798, -7.610433527965647649 ) ) ;
#12717 = CARTESIAN_POINT ( 'NONE',  ( 9.776257737944273885, -75.99675307336229935, 6.518143555704688730 ) ) ;
#12718 = CARTESIAN_POINT ( 'NONE',  ( 4.515731304085703890, -85.88547955769999476, 0.5183330846481556398 ) ) ;
#12719 = ORIENTED_EDGE ( 'NONE', *, *, #24622, .F. ) ;
#12720 = CARTESIAN_POINT ( 'NONE',  ( -9.500000000000000000, -78.29999999999999716, 0.000000000000000000 ) ) ;
#12721 = CARTESIAN_POINT ( 'NONE',  ( 2.842273781882246109, -2.309665338011450242, -1.638569763671750668 ) ) ;
#12722 = VECTOR ( 'NONE', #27010, 1000.000000000000114 ) ;
#12723 = CARTESIAN_POINT ( 'NONE',  ( -11.88401260600999976, -79.80654510736209772, 3.058538056121000270 ) ) ;
#12724 = CARTESIAN_POINT ( 'NONE',  ( 3.962812355710999768, -78.54828561723799396, -2.338746421483398841 ) ) ;
#12725 = CARTESIAN_POINT ( 'NONE',  ( -0.4492251327744000156, -81.66711945450001053, 1.604198796042999753 ) ) ;
#12726 = CARTESIAN_POINT ( 'NONE',  ( 4.038786804788999873, -79.58513894942799993, -10.20549938643999965 ) ) ;
#12727 = CARTESIAN_POINT ( 'NONE',  ( 1.782734487935019541, -17.87754631442412645, 12.71547286926183062 ) ) ;
#12728 = CARTESIAN_POINT ( 'NONE',  ( -6.508777536021999488, -76.58936719843599406, -10.40112358611999888 ) ) ;
#12729 = CARTESIAN_POINT ( 'NONE',  ( 3.275141186877373656, -78.55044160814078680, 11.28318025823995541 ) ) ;
#12730 = CARTESIAN_POINT ( 'NONE',  ( -7.391903123959864708, -76.93479338433584758, 7.904442030565260069 ) ) ;
#12731 = VERTEX_POINT ( 'NONE', #37605 ) ;
#12732 = CARTESIAN_POINT ( 'NONE',  ( 3.609690327934000020, -80.05722375786560008, 10.39335624559999971 ) ) ;
#12733 = CARTESIAN_POINT ( 'NONE',  ( 0.4768038028798605721, -79.94409901709930466, 1.155327188750691292 ) ) ;
#12734 = CARTESIAN_POINT ( 'NONE',  ( 8.907139034666096578, -75.80000000000001137, -7.900904588343065527 ) ) ;
#12735 = CARTESIAN_POINT ( 'NONE',  ( -10.83342013959000028, -78.72383311221699387, 2.669945268378000058 ) ) ;
#12736 = FACE_OUTER_BOUND ( 'NONE', #36853, .T. ) ;
#12737 = CARTESIAN_POINT ( 'NONE',  ( -9.000000000000000000, -80.79999999999999716, 0.000000000000000000 ) ) ;
#12738 = CARTESIAN_POINT ( 'NONE',  ( 11.75000000000000000, -76.95000000000000284, 0.000000000000000000 ) ) ;
#12739 = ADVANCED_FACE ( 'NONE', ( #1912 ), #29319, .T. ) ;
#12740 = DIRECTION ( 'NONE',  ( 0.000000000000000000, -1.000000000000000000, 0.000000000000000000 ) ) ;
#12741 = EDGE_CURVE ( 'NONE', #35302, #34134, #33165, .T. ) ;
#12742 = DIRECTION ( 'NONE',  ( 0.000000000000000000, 1.000000000000000000, 0.000000000000000000 ) ) ;
#12743 = AXIS2_PLACEMENT_3D ( 'NONE', #10205, #32905, #18772 ) ;
#12744 = CARTESIAN_POINT ( 'NONE',  ( 0.000000000000000000, -26.93717104351999936, 0.000000000000000000 ) ) ;
#12745 = ORIENTED_EDGE ( 'NONE', *, *, #19701, .F. ) ;
#12746 = ORIENTED_EDGE ( 'NONE', *, *, #16607, .F. ) ;
#12747 = B_SPLINE_CURVE_WITH_KNOTS ( 'NONE', 3,
 ( #27566, #45610, #5151, #45900, #52354, #33746 ),
 .UNSPECIFIED., .F., .F.,
 ( 4, 1, 1, 4 ),
 ( 0.000000000000000000, 0.3333333333333000081, 0.6666666666667000474, 1.000000000000000000 ),
 .UNSPECIFIED. ) ;
#12748 = FACE_OUTER_BOUND ( 'NONE', #56465, .T. ) ;
#12749 = AXIS2_PLACEMENT_3D ( 'NONE', #47450, #1992, #43001 ) ;
#12750 = ORIENTED_EDGE ( 'NONE', *, *, #57349, .F. ) ;
#12751 = CARTESIAN_POINT ( 'NONE',  ( -11.89999999977000122, -23.15000000000000213, 0.000000000000000000 ) ) ;
#12752 = ORIENTED_EDGE ( 'NONE', *, *, #15032, .T. ) ;
#12753 = FACE_OUTER_BOUND ( 'NONE', #38141, .T. ) ;
#12754 = CARTESIAN_POINT ( 'NONE',  ( -7.639223145873000220, -76.51163981165899486, 7.500260266847000423 ) ) ;
#12755 = CARTESIAN_POINT ( 'NONE',  ( 7.890654042133999901, -77.92253998579799656, 4.760698198672999482 ) ) ;
#12756 = CARTESIAN_POINT ( 'NONE',  ( -6.041084908348863358, -78.16847799058953683, -7.008332470365363775 ) ) ;
#12757 = CARTESIAN_POINT ( 'NONE',  ( 5.865103843792000227, -78.36710291063299394, -9.561319920857000554 ) ) ;
#12758 = ORIENTED_EDGE ( 'NONE', *, *, #22057, .F. ) ;
#12759 = ORIENTED_EDGE ( 'NONE', *, *, #14422, .T. ) ;
#12760 = CARTESIAN_POINT ( 'NONE',  ( -7.162195376558232240, -77.54552129972844909, 5.853735638857269663 ) ) ;
#12761 = CARTESIAN_POINT ( 'NONE',  ( -10.47078769031000078, -77.83521312279499682, -3.499536356729999742 ) ) ;
#12762 = CARTESIAN_POINT ( 'NONE',  ( -0.3926218265389255779, -77.89583333333338544, 1.460959015002472494 ) ) ;
#12763 = LINE ( 'NONE', #44654, #50299 ) ;
#12764 = CARTESIAN_POINT ( 'NONE',  ( -1.959694873104000257, -77.43897000290898802, -9.504225410855001499 ) ) ;
#12765 = CARTESIAN_POINT ( 'NONE',  ( 6.505968525872999564, -75.99885856455000521, -11.03293300994000070 ) ) ;
#12766 = CARTESIAN_POINT ( 'NONE',  ( -6.899571484722149428, -79.46005502588960212, -6.530559442748636201 ) ) ;
#12767 = CARTESIAN_POINT ( 'NONE',  ( 0.1198033158700999995, -79.08031231683999351, 1.623056241665000066 ) ) ;
#12768 = CARTESIAN_POINT ( 'NONE',  ( -10.55592303174000079, -80.01864766310099242, -3.904632140253000205 ) ) ;
#12769 = CARTESIAN_POINT ( 'NONE',  ( 12.48408657659000021, -18.63026141570000149, -1.669508654504000100 ) ) ;
#12770 = CARTESIAN_POINT ( 'NONE',  ( -9.770427757044000572, -25.05529868456000386, -8.292768371742001321 ) ) ;
#12771 = CARTESIAN_POINT ( 'NONE',  ( -11.52337632743963347, -76.68415288553248388, 2.295937825998684012 ) ) ;
#12772 = EDGE_CURVE ( 'NONE', #32566, #41582, #35167, .T. ) ;
#12773 = ORIENTED_EDGE ( 'NONE', *, *, #4266, .T. ) ;
#12774 = CARTESIAN_POINT ( 'NONE',  ( -2.478361877531000346, -79.68515284566699108, -11.82696626457999933 ) ) ;
#12775 = DIRECTION ( 'NONE',  ( 1.000000000000000000, 0.000000000000000000, 0.000000000000000000 ) ) ;
#12776 = ADVANCED_FACE ( 'NONE', ( #30685 ), #13973, .F. ) ;
#12777 = DIRECTION ( 'NONE',  ( 3.944178317128000824E-11, 1.000000000000000000, -1.496715540702999877E-09 ) ) ;
#12778 = CARTESIAN_POINT ( 'NONE',  ( -10.36222501930000028, -18.77880030165999869, -7.631889976314999657 ) ) ;
#12779 = CARTESIAN_POINT ( 'NONE',  ( 7.612971414731999786, -60.12452529330000317, 10.53003223724999948 ) ) ;
#12780 = DIRECTION ( 'NONE',  ( 0.000000000000000000, 1.000000000000000000, 0.000000000000000000 ) ) ;
#12781 = CARTESIAN_POINT ( 'NONE',  ( -11.10900444195999981, -80.10274572043100250, 2.566683358663000014 ) ) ;
#12782 = CARTESIAN_POINT ( 'NONE',  ( -0.3713770062794000126, -82.28702925038599858, -1.193557338046999927 ) ) ;
#12783 = CARTESIAN_POINT ( 'NONE',  ( -11.00476719864000152, -77.30636667169498821, 2.393546210564999832 ) ) ;
#12784 = CARTESIAN_POINT ( 'NONE',  ( 7.601397897754999633, -23.24999999688999708, 10.07627163191000008 ) ) ;
#12785 = CARTESIAN_POINT ( 'NONE',  ( -5.300832050426999231, -80.90938799829500283, -9.929493364645999520 ) ) ;
#12786 = VERTEX_POINT ( 'NONE', #2629 ) ;
#12787 = CARTESIAN_POINT ( 'NONE',  ( 0.000000000000000000, -76.19999999999998863, 0.000000000000000000 ) ) ;
#12788 = CARTESIAN_POINT ( 'NONE',  ( 1.295048492664000017, -54.27106480841000291, 12.54716442233000073 ) ) ;
#12789 = VECTOR ( 'NONE', #46517, 1000.000000000000114 ) ;
#12790 = CARTESIAN_POINT ( 'NONE',  ( -12.60552522436000089, -23.28917565320000094, 1.799501877760999902 ) ) ;
#12791 = CARTESIAN_POINT ( 'NONE',  ( -3.114903485943000039, -2.587975590836000261, 1.894521665057000037 ) ) ;
#12792 = CARTESIAN_POINT ( 'NONE',  ( 2.854969924326999919, -78.05283741445799706, 10.84745395576000071 ) ) ;
#12793 = CARTESIAN_POINT ( 'NONE',  ( 9.500000000000000000, -77.54999999999999716, 0.000000000000000000 ) ) ;
#12794 = DIRECTION ( 'NONE',  ( 0.000000000000000000, -1.000000000000000000, 0.000000000000000000 ) ) ;
#12795 = CARTESIAN_POINT ( 'NONE',  ( -0.4450739772378000114, -61.67813214767999597, 12.43586747599000120 ) ) ;
#12796 = DIRECTION ( 'NONE',  ( -0.7071067811864970576, -3.534300182982984496E-08, -0.7071067811865970887 ) ) ;
#12797 = VECTOR ( 'NONE', #14377, 1000.000000000000000 ) ;
#12798 = CARTESIAN_POINT ( 'NONE',  ( -0.8080452641954999349, -83.58499735065198877, -4.095932448746999910 ) ) ;
#12799 = ADVANCED_FACE ( 'NONE', ( #7050 ), #26185, .F. ) ;
#12800 = DIRECTION ( 'NONE',  ( 0.000000000000000000, 1.000000000000000000, 0.000000000000000000 ) ) ;
#12801 = CARTESIAN_POINT ( 'NONE',  ( 11.37518297042895909, -77.17675121447568642, -3.894839749335730517 ) ) ;
#12802 = CARTESIAN_POINT ( 'NONE',  ( -6.912545260079999920, -78.34900158500600753, -8.891046157644998615 ) ) ;
#12803 = CARTESIAN_POINT ( 'NONE',  ( 1.007676913700946697, -81.90086700953483501, 0.7397467089371103643 ) ) ;
#12804 = CARTESIAN_POINT ( 'NONE',  ( -1.410540931501999884, -78.42725491157000306, -0.6403706075564999933 ) ) ;
#12805 = CARTESIAN_POINT ( 'NONE',  ( -9.429275737370000243, -77.40017060862199116, -1.157047565421999824 ) ) ;
#12806 = CARTESIAN_POINT ( 'NONE',  ( -0.7280429309147493644, -82.83501156738459770, -1.324360742052439477 ) ) ;
#12807 = CARTESIAN_POINT ( 'NONE',  ( -12.77297283019000140, -61.52822696498000710, 1.476112654660999723 ) ) ;
#12808 = CARTESIAN_POINT ( 'NONE',  ( 3.232567627276669242, -80.24941509227865311, -10.25408852723510478 ) ) ;
#12809 = FACE_OUTER_BOUND ( 'NONE', #6597, .T. ) ;
#12810 = CARTESIAN_POINT ( 'NONE',  ( 11.99999999999998757, -75.80000000000001137, 1.262728147666866585 ) ) ;
#12811 = ORIENTED_EDGE ( 'NONE', *, *, #52089, .T. ) ;
#12812 = EDGE_CURVE ( 'NONE', #13297, #16896, #33874, .T. ) ;
#12813 = CARTESIAN_POINT ( 'NONE',  ( 1.041624132644355161, -81.80353841734945775, -0.6908730350728758962 ) ) ;
#12814 = CARTESIAN_POINT ( 'NONE',  ( -9.252740428349008894, -78.77916666666668277, 2.486604901413127955 ) ) ;
#12815 = CARTESIAN_POINT ( 'NONE',  ( 0.000000000000000000, -79.79999999999999716, 0.000000000000000000 ) ) ;
#12816 = CARTESIAN_POINT ( 'NONE',  ( 10.75000000000000000, -78.75000000000000000, 0.000000000000000000 ) ) ;
#12817 = ORIENTED_EDGE ( 'NONE', *, *, #23827, .T. ) ;
#12818 = VERTEX_POINT ( 'NONE', #27365 ) ;
#12819 = CARTESIAN_POINT ( 'NONE',  ( -1.494228022679999768, -80.96100974943900042, 0.6119612316942000252 ) ) ;
#12820 = ORIENTED_EDGE ( 'NONE', *, *, #1310, .T. ) ;
#12821 = EDGE_LOOP ( 'NONE', ( #32412, #48577, #21332, #17018 ) ) ;
#12822 = DIRECTION ( 'NONE',  ( 0.000000000000000000, -1.000000000000000000, 0.000000000000000000 ) ) ;
#12823 = CARTESIAN_POINT ( 'NONE',  ( -1.310679582531389498, -78.45833333333332860, 0.7554284705563444335 ) ) ;
#12824 = CARTESIAN_POINT ( 'NONE',  ( 10.84306248592000088, -78.81415834696599632, -1.266239280945999912 ) ) ;
#12825 = CARTESIAN_POINT ( 'NONE',  ( 0.5506765233278000382, -25.25954292244000143, -12.77514798311000099 ) ) ;
#12826 = CARTESIAN_POINT ( 'NONE',  ( -3.204937774633000114, -80.37370721702599496, 1.959526568264000179 ) ) ;
#12827 = CARTESIAN_POINT ( 'NONE',  ( -3.727509208301453381, -79.30673376728708490, 8.737982862341825196 ) ) ;
#12828 = ORIENTED_EDGE ( 'NONE', *, *, #14062, .T. ) ;
#12829 = CARTESIAN_POINT ( 'NONE',  ( 4.099999999699000419, -75.20000000030088927, -8.298664203784000017E-10 ) ) ;
#12830 = CARTESIAN_POINT ( 'NONE',  ( -11.64344076419000018, -78.97841925342000025, 4.142712554322000251 ) ) ;
#12831 = ORIENTED_EDGE ( 'NONE', *, *, #6505, .F. ) ;
#12832 = ORIENTED_EDGE ( 'NONE', *, *, #36248, .F. ) ;
#12833 = CARTESIAN_POINT ( 'NONE',  ( -1.498805164377271737, -77.75840249518691394, -0.1584492094687433572 ) ) ;
#12834 = CARTESIAN_POINT ( 'NONE',  ( 4.110498728239191379, -79.79999999999998295, 11.18969932762453112 ) ) ;
#12835 = AXIS2_PLACEMENT_3D ( 'NONE', #27089, #27962, #58098 ) ;
#12836 = CARTESIAN_POINT ( 'NONE',  ( -0.6056189234361001317, -80.30937613589500756, -1.188192690176999911 ) ) ;
#12837 = CARTESIAN_POINT ( 'NONE',  ( -3.616440607051700340, -86.17851881763697008, 1.692525710106622894 ) ) ;
#12838 = CARTESIAN_POINT ( 'NONE',  ( 7.486068761172999686, -76.08624778869000238, -8.059700645992000645 ) ) ;
#12839 = VECTOR ( 'NONE', #9258, 1000.000000000000227 ) ;
#12840 = CARTESIAN_POINT ( 'NONE',  ( 6.944463141141999252, -76.67929967898000143, -9.899892744310998083 ) ) ;
#12841 = CARTESIAN_POINT ( 'NONE',  ( 12.19230762942000013, -76.97310353941999495, -3.339585897562999950 ) ) ;
#12842 = CARTESIAN_POINT ( 'NONE',  ( -7.489130957889000406, -76.46197497528599740, 7.898313055298999963 ) ) ;
#12843 = STYLED_ITEM ( 'NONE', ( #15407 ), #17895 ) ;
#12844 = CARTESIAN_POINT ( 'NONE',  ( -8.867285139540818761, -78.62306678270786620, -2.634614563402982501 ) ) ;
#12845 = DIRECTION ( 'NONE',  ( -1.000000000000000000, 0.000000000000000000, 0.000000000000000000 ) ) ;
#12846 = CARTESIAN_POINT ( 'NONE',  ( -0.003892519155869273318, -2.975579981115140438, 3.249707649575004798 ) ) ;
#12847 = CARTESIAN_POINT ( 'NONE',  ( -2.027398468737999782, -80.44230496681200293, -2.910535655822000134 ) ) ;
#12848 = CARTESIAN_POINT ( 'NONE',  ( -13.89999999999999858, -6.000000000000000000, 0.000000000000000000 ) ) ;
#12849 = CARTESIAN_POINT ( 'NONE',  ( -4.000000000000000000, -78.69999999915415856, 2.834003763004000336E-08 ) ) ;
#12850 = CARTESIAN_POINT ( 'NONE',  ( 1.781953555039999859, -2.946439977264000198, -3.363141973650999983 ) ) ;
#12851 = CARTESIAN_POINT ( 'NONE',  ( 1.062425010523426527, -80.45345406285113654, -0.7035154447333287209 ) ) ;
#12852 = ORIENTED_EDGE ( 'NONE', *, *, #22643, .F. ) ;
#12853 = DIRECTION ( 'NONE',  ( 1.000000000000000000, 0.000000000000000000, 0.000000000000000000 ) ) ;
#12854 = CARTESIAN_POINT ( 'NONE',  ( 0.000000000000000000, -77.40000000000736691, 0.000000000000000000 ) ) ;
#12855 = CARTESIAN_POINT ( 'NONE',  ( -1.234140985588999984, -81.14718027224098762, 0.5054425604136000283 ) ) ;
#12856 = CARTESIAN_POINT ( 'NONE',  ( -12.44180763926000033, -17.90743932638000047, -1.459474665415000150 ) ) ;
#12857 = CARTESIAN_POINT ( 'NONE',  ( -9.339950055924999717, -78.07862776177000796, -9.061158367717998985 ) ) ;
#12858 = EDGE_CURVE ( 'NONE', #34312, #11183, #48938, .T. ) ;
#12859 = CARTESIAN_POINT ( 'NONE',  ( 1.854164892466000136, -79.71126001420199714, -9.336963670056000808 ) ) ;
#12860 = CARTESIAN_POINT ( 'NONE',  ( -12.32022177036999899, -76.50834268828999996, -2.184374125126999910 ) ) ;
#12861 = ORIENTED_EDGE ( 'NONE', *, *, #45866, .F. ) ;
#12862 = CARTESIAN_POINT ( 'NONE',  ( -14.00000000000000000, -69.46217755556000384, -5.544640309915999038E-06 ) ) ;
#12863 = DIRECTION ( 'NONE',  ( 0.8320502943378438321, -0.5547001962252288143, 2.960700184868154238E-12 ) ) ;
#12864 = B_SPLINE_CURVE_WITH_KNOTS ( 'NONE', 3,
 ( #57134, #18074, #22785, #39125, #21119, #7545, #13627, #30254, #25258, #53797, #48294, #43862, #48011, #4495, #22493, #11697, #43562, #34681 ),
 .UNSPECIFIED., .F., .F.,
 ( 4, 2, 2, 2, 2, 2, 2, 2, 4 ),
 ( 0.000000000000000000, 0.1250000000000000278, 0.2500000000000000555, 0.3750000000000001665, 0.5000000000000001110, 0.6250000000000001110, 0.7500000000000002220, 0.8750000000000001110, 1.000000000000000000 ),
 .UNSPECIFIED. ) ;
#12865 = CARTESIAN_POINT ( 'NONE',  ( 1.330850115287000035, -81.57385641401499754, 0.4611193915267000065 ) ) ;
#12866 = CARTESIAN_POINT ( 'NONE',  ( -1.799475304559999822, -20.24828923609000242, -12.69616050747999836 ) ) ;
#12867 = CARTESIAN_POINT ( 'NONE',  ( -5.062255795481000575, -77.53733258133598838, -8.064983548927001422 ) ) ;
#12868 = CARTESIAN_POINT ( 'NONE',  ( -3.883990342729000123, -84.62957809581099866, 1.523540054217000117 ) ) ;
#12869 = CARTESIAN_POINT ( 'NONE',  ( -3.342781753851123305, -80.00035736669231312, 10.21718976228000031 ) ) ;
#12870 = CARTESIAN_POINT ( 'NONE',  ( 0.5881506857339000582, -79.39061393252499954, 1.397505295191999952 ) ) ;
#12871 = EDGE_LOOP ( 'NONE', ( #27038, #9423, #20374 ) ) ;
#12872 = CIRCLE ( 'NONE', #28893, 1.199999999999999734 ) ;
#12873 = CARTESIAN_POINT ( 'NONE',  ( -4.661427456832804239, -77.18932811019587348, -9.686758570029148530 ) ) ;
#12874 = CARTESIAN_POINT ( 'NONE',  ( -0.1738511558967903159, -82.17838541666473873, 1.321614583343871274 ) ) ;
#12875 = CARTESIAN_POINT ( 'NONE',  ( 3.485499217012001161, -78.91452042059381711, 6.970998434024031631 ) ) ;
#12876 = VERTEX_POINT ( 'NONE', #18240 ) ;
#12877 = VECTOR ( 'NONE', #10556, 1000.000000000000227 ) ;
#12879 = EDGE_CURVE ( 'NONE', #23736, #35917, #17938, .T. ) ;
#12878 = ORIENTED_EDGE ( 'NONE', *, *, #43410, .F. ) ;
#12880 = CARTESIAN_POINT ( 'NONE',  ( 9.601044633201999190, -79.16060049144299171, 5.244783912358999878 ) ) ;
#12881 = CARTESIAN_POINT ( 'NONE',  ( -7.353725627631181538, -55.49344856148322691, -8.180687091746209560 ) ) ;
#12882 = CARTESIAN_POINT ( 'NONE',  ( 1.802966087674999995, -80.16922046769499843, 11.18561714559999842 ) ) ;
#12883 = VECTOR ( 'NONE', #40533, 1000.000000000000114 ) ;
#12884 = ORIENTED_EDGE ( 'NONE', *, *, #12858, .T. ) ;
#12885 = VERTEX_POINT ( 'NONE', #36228 ) ;
#12886 = ORIENTED_EDGE ( 'NONE', *, *, #26417, .T. ) ;
#12887 = EDGE_CURVE ( 'NONE', #21042, #18942, #53697, .T. ) ;
#12888 = CARTESIAN_POINT ( 'NONE',  ( -11.74632961396963182, -78.18897092989068653, 1.536354035319362099 ) ) ;
#12889 = CARTESIAN_POINT ( 'NONE',  ( -3.315446055502797140, -0.8053565017603924181, 2.002980581032114404 ) ) ;
#12890 = EDGE_CURVE ( 'NONE', #27720, #29378, #3710, .T. ) ;
#12891 = ORIENTED_EDGE ( 'NONE', *, *, #50634, .T. ) ;
#12892 = CARTESIAN_POINT ( 'NONE',  ( 0.7352315925313128719, -82.04166666286488407, -1.273945750275897071 ) ) ;
#12893 = ORIENTED_EDGE ( 'NONE', *, *, #52449, .T. ) ;
#12894 = CARTESIAN_POINT ( 'NONE',  ( -1.084778369707915413, -80.19423709646559928, -0.6700028332395955299 ) ) ;
#12895 = CARTESIAN_POINT ( 'NONE',  ( 3.621447497674998850, -78.99318692614359350, -2.137281964302801374 ) ) ;
#12896 = B_SPLINE_CURVE_WITH_KNOTS ( 'NONE', 3,
 ( #37876, #19299, #37583, #37290, #20177, #46182, #10744, #24886, #11320, #29019, #6000, #46772, #38164, #15450, #50604, #15736, #10153, #55306 ),
 .UNSPECIFIED., .F., .F.,
 ( 4, 2, 2, 2, 2, 2, 2, 2, 4 ),
 ( 0.000000000000000000, 0.1250000000000000000, 0.2500000000000000000, 0.3750000000000000000, 0.5000000000000000000, 0.6250000000000000000, 0.7500000000000000000, 0.8750000000000000000, 1.000000000000000000 ),
 .UNSPECIFIED. ) ;
#12897 = CARTESIAN_POINT ( 'NONE',  ( 10.36292447788999915, -55.59904187545999577, 7.633480004398999874 ) ) ;
#12898 = CARTESIAN_POINT ( 'NONE',  ( -7.641012386038000592, -18.71082434677000350, -10.18589234708000113 ) ) ;
#12899 = CARTESIAN_POINT ( 'NONE',  ( 1.535709645332969941, -77.33338449841629370, -11.74782911498686389 ) ) ;
#12900 = CARTESIAN_POINT ( 'NONE',  ( -9.149885487026406139, -80.39887705342988511, -6.477978945181864567 ) ) ;
#12901 = CARTESIAN_POINT ( 'NONE',  ( 7.668949790015999746, -59.57129148919000272, -10.21381326473999884 ) ) ;
#12902 = CARTESIAN_POINT ( 'NONE',  ( 9.079299172193310952, -78.83476146753204716, -1.768634379958562208 ) ) ;
#12903 = CARTESIAN_POINT ( 'NONE',  ( -10.53562597589000127, -23.20558297624999966, 7.620013358880999732 ) ) ;
#12904 = EDGE_CURVE ( 'NONE', #14353, #37723, #31979, .T. ) ;
#12905 = VECTOR ( 'NONE', #28821, 1000.000000000000000 ) ;
#12906 = CARTESIAN_POINT ( 'NONE',  ( -3.200023585962000094, -78.81000264934789357, -2.681355300499000283 ) ) ;
#12907 = CARTESIAN_POINT ( 'NONE',  ( 6.877190604583000244, -77.44408667140099567, -6.929239867807000408 ) ) ;
#12908 = DIRECTION ( 'NONE',  ( -0.7071067811864976127, -0.7071067811865975328, 4.006692910709986783E-09 ) ) ;
#12909 = CARTESIAN_POINT ( 'NONE',  ( 9.611650271896820641, -77.89166666666666572, 5.539808784079911952 ) ) ;
#12910 = CARTESIAN_POINT ( 'NONE',  ( -1.801614160558000055, -23.38652261905000174, 12.59687422887999908 ) ) ;
#12911 = CARTESIAN_POINT ( 'NONE',  ( 1.316195966539962292, -81.00943227468225416, 0.1540212709399112478 ) ) ;
#12912 = AXIS2_PLACEMENT_3D ( 'NONE', #16569, #31495, #34554 ) ;
#12913 = CARTESIAN_POINT ( 'NONE',  ( -8.650571159592999493, -79.61510095943374665, 4.057379972786000266 ) ) ;
#12914 = B_SPLINE_CURVE_WITH_KNOTS ( 'NONE', 3,
 ( #3773, #35638, #39781, #562, #8205, #45413, #13505, #31797, #27077, #4956, #26208, #44511, #44812, #36531, #53364, #22961 ),
 .UNSPECIFIED., .F., .F.,
 ( 4, 2, 2, 2, 2, 2, 2, 4 ),
 ( 0.000000000000000000, 0.1250000000000000278, 0.2500000000000000555, 0.3750000000000001110, 0.5000000000000001110, 0.7500000000000002220, 0.8750000000000002220, 1.000000000000000000 ),
 .UNSPECIFIED. ) ;
#12915 = CIRCLE ( 'NONE', #32721, 1.750000000000000000 ) ;
#12916 = CARTESIAN_POINT ( 'NONE',  ( 1.227268718659146218, -80.04969058873581389, -0.8848763678067933514 ) ) ;
#12917 = CARTESIAN_POINT ( 'NONE',  ( -0.6149910796752999786, -79.26092107675799525, 1.385894317580000035 ) ) ;
#12918 = TOROIDAL_SURFACE ( 'NONE', #56321, 17.50000000000000000, 5.000000000000000000 ) ;
#12919 = FACE_BOUND ( 'NONE', #53627, .T. ) ;
#12920 = CARTESIAN_POINT ( 'NONE',  ( -5.597547907814000467, -78.10874741097399010, -9.372450235129999641 ) ) ;
#12921 = CARTESIAN_POINT ( 'NONE',  ( -8.353021825866999706, -78.43888052662398991, -9.001266886329000627 ) ) ;
#12922 = DIRECTION ( 'NONE',  ( 0.000000000000000000, -1.000000000000000000, 0.000000000000000000 ) ) ;
#12923 = LINE ( 'NONE', #57230, #42064 ) ;
#12924 = CARTESIAN_POINT ( 'NONE',  ( 1.261625697157999992, -81.35059162671998934, -0.7514603626543999715 ) ) ;
#12925 = CARTESIAN_POINT ( 'NONE',  ( -3.691465036726909066, -79.50301741532913979, 10.09624330836405015 ) ) ;
#12926 = ORIENTED_EDGE ( 'NONE', *, *, #56821, .F. ) ;
#12927 = CARTESIAN_POINT ( 'NONE',  ( -10.04116292115999975, -22.76462890193000277, -7.682344222570999470 ) ) ;
#12928 = CARTESIAN_POINT ( 'NONE',  ( 10.90780079584000006, -79.47248173447398756, -5.366096107902000867 ) ) ;
#12929 = CARTESIAN_POINT ( 'NONE',  ( -2.510982762904000243, -80.68017688227318729, -10.76696539026999844 ) ) ;
#12930 = DIRECTION ( 'NONE',  ( -1.000000000000000000, 0.000000000000000000, 0.000000000000000000 ) ) ;
#12931 = CARTESIAN_POINT ( 'NONE',  ( -10.53495260694000102, -60.02711197453000125, 7.618387230260000642 ) ) ;
#12932 = CARTESIAN_POINT ( 'NONE',  ( 2.610509270830999817, -0.8533534949847000339, 2.388898296653999775 ) ) ;
#12933 = CARTESIAN_POINT ( 'NONE',  ( 9.634996601833998753, -79.94318275341397850, -1.682215218792999956 ) ) ;
#12934 = CARTESIAN_POINT ( 'NONE',  ( 12.68624828429000040, -23.76426636002999970, -1.886933512377000133 ) ) ;
#12935 = CARTESIAN_POINT ( 'NONE',  ( -7.958763982144999360, -54.32301960774000094, -9.723170657514000226 ) ) ;
#12936 = VERTEX_POINT ( 'NONE', #17638 ) ;
#12937 = CARTESIAN_POINT ( 'NONE',  ( -12.71005124793994945, -54.50500926678794400, 1.687536500513815874 ) ) ;
#12938 = CARTESIAN_POINT ( 'NONE',  ( 8.060180467146665251, -24.62064870852272236, -9.621709426102265539 ) ) ;
#12939 = DIRECTION ( 'NONE',  ( 0.000000000000000000, 0.000000000000000000, -1.000000000000000000 ) ) ;
#12940 = EDGE_CURVE ( 'NONE', #41885, #20895, #24647, .T. ) ;
#12941 = CARTESIAN_POINT ( 'NONE',  ( -10.53101998748999968, -60.10639625617000092, -7.613962827198000660 ) ) ;
#12942 = FACE_OUTER_BOUND ( 'NONE', #43615, .T. ) ;
#12943 = ORIENTED_EDGE ( 'NONE', *, *, #3683, .F. ) ;
#12944 = EDGE_CURVE ( 'NONE', #43269, #40118, #3509, .T. ) ;
#12945 = CARTESIAN_POINT ( 'NONE',  ( 10.99860714806000139, -77.19003472681939115, 1.508735257010000108 ) ) ;
#12946 = CARTESIAN_POINT ( 'NONE',  ( 0.000000000000000000, -0.5000000000000000000, 0.000000000000000000 ) ) ;
#12947 = FACE_OUTER_BOUND ( 'NONE', #45972, .T. ) ;
#12948 = VERTEX_POINT ( 'NONE', #41537 ) ;
#12949 = AXIS2_PLACEMENT_3D ( 'NONE', #10769, #11351, #52082 ) ;
#12950 = CARTESIAN_POINT ( 'NONE',  ( -9.108265402946999600, -53.92189187171000242, -8.478706101031999509 ) ) ;
#12951 = CARTESIAN_POINT ( 'NONE',  ( 8.985706068735000329, -79.48779652109199390, -3.828549499589000149 ) ) ;
#12952 = EDGE_LOOP ( 'NONE', ( #50094, #29300, #12390, #10594 ) ) ;
#12953 = ADVANCED_FACE ( 'NONE', ( #50120 ), #17234, .F. ) ;
#12954 = VECTOR ( 'NONE', #30740, 1000.000000000000000 ) ;
#12955 = VERTEX_POINT ( 'NONE', #51076 ) ;
#12956 = CARTESIAN_POINT ( 'NONE',  ( -3.152476705098000487, -77.22767140587998824, -11.82163513714000125 ) ) ;
#12957 = DIRECTION ( 'NONE',  ( 0.7071067811865475727, 0.000000000000000000, -0.7071067811865475727 ) ) ;
#12958 = CARTESIAN_POINT ( 'NONE',  ( 0.8068013270406000359, -79.03761357724998504, 1.305699365831000103 ) ) ;
#12959 = EDGE_LOOP ( 'NONE', ( #8119, #54866, #14494, #13323 ) ) ;
#12960 = CARTESIAN_POINT ( 'NONE',  ( 10.01676960212000012, -18.79061945240999876, 7.658895148207999881 ) ) ;
#12961 = CARTESIAN_POINT ( 'NONE',  ( -0.3767128267918133933, -79.35487657498305225, -1.459930215568542522 ) ) ;
#12962 = CARTESIAN_POINT ( 'NONE',  ( 0.0006957917016094362049, -80.22560324140505372, -1.249665624490517768 ) ) ;
#12963 = CARTESIAN_POINT ( 'NONE',  ( -1.349038754591999956, -78.11117779481000412, -13.04399231589999886 ) ) ;
#12964 = CARTESIAN_POINT ( 'NONE',  ( 8.196653188619999142, -77.55979376850486062, 7.657217973713000170 ) ) ;
#12965 = CARTESIAN_POINT ( 'NONE',  ( 3.618614839418587081, -86.36264283715698298, 2.628308734607720520 ) ) ;
#12966 = CARTESIAN_POINT ( 'NONE',  ( 10.89876807034000095, -79.63268594753199636, -2.652350870517000025 ) ) ;
#12967 = CARTESIAN_POINT ( 'NONE',  ( -2.858407197967999913, -79.99999999999998579, 8.797272775729998884 ) ) ;
#12968 = B_SPLINE_CURVE_WITH_KNOTS ( 'NONE', 3,
 ( #16475, #57198, #6450, #38321, #16188, #29168, #47214, #20047, #24465, #43338, #34166, #38898, #42477, #52203, #7035, #16766, #34744, #34456 ),
 .UNSPECIFIED., .F., .F.,
 ( 4, 2, 2, 2, 2, 2, 2, 2, 4 ),
 ( 0.000000000000000000, 0.1250000000000000000, 0.2499999999999999722, 0.3749999999999999445, 0.4999999999999999445, 0.6250000000000000000, 0.7500000000000000000, 0.8750000000000000000, 1.000000000000000000 ),
 .UNSPECIFIED. ) ;
#12969 = CARTESIAN_POINT ( 'NONE',  ( 10.18249594443127393, -17.70907903273885964, 7.792385963404970362 ) ) ;
#12970 = ORIENTED_EDGE ( 'NONE', *, *, #48133, .F. ) ;
#12971 = CARTESIAN_POINT ( 'NONE',  ( -7.707335466132000157, -79.18586165678098610, -8.217415310065000256 ) ) ;
#12972 = CARTESIAN_POINT ( 'NONE',  ( 7.331368884251999951, -75.87623222076001639, 9.888700222343000945 ) ) ;
#12973 = CARTESIAN_POINT ( 'NONE',  ( 1.243995776054000135, -80.08712754295498826, 0.6800984409344000836 ) ) ;
#12974 = EDGE_CURVE ( 'NONE', #50856, #45467, #56333, .T. ) ;
#12975 = CARTESIAN_POINT ( 'NONE',  ( -0.5931688960305999681, -78.57016653067499590, 1.178438064142999897 ) ) ;
#12976 = CARTESIAN_POINT ( 'NONE',  ( 0.2195004960192260823, -2.979185772309488556, -3.512406260861363982 ) ) ;
#12977 = CARTESIAN_POINT ( 'NONE',  ( 8.727615157005653046, -77.01666666666665151, -3.881808298730416773 ) ) ;
#12978 = DIRECTION ( 'NONE',  ( -1.000000000000000000, 0.000000000000000000, 0.000000000000000000 ) ) ;
#12979 = CARTESIAN_POINT ( 'NONE',  ( -10.57172952804012667, -80.44999999999998863, -2.251292830071324857 ) ) ;
#12980 = CARTESIAN_POINT ( 'NONE',  ( 3.357763675545999860, -79.20626297899599422, -10.64034880800999971 ) ) ;
#12981 = CARTESIAN_POINT ( 'NONE',  ( -9.207228400713001193, -77.40571498579799936, -3.168505599523000260 ) ) ;
#12982 = CARTESIAN_POINT ( 'NONE',  ( 10.55910102242999926, -22.78485473281999774, -7.642147947518999729 ) ) ;
#12983 = CARTESIAN_POINT ( 'NONE',  ( -0.8902956382338467201, -83.03876140007196227, 0.8768580129426997161 ) ) ;
#12984 = CARTESIAN_POINT ( 'NONE',  ( 1.099819419251000019, -79.61718521679551941, 11.16281809564999961 ) ) ;
#12985 = B_SPLINE_SURFACE_WITH_KNOTS ( 'NONE', 3, 3, ( 
 ( #58172, #57879, #26566, #8873, #17738, #44598, #27155, #40753, #4447, #22448, #18326, #40463, #8287, #39582, #49920, #35726, #13882, #26867, #36319, #31284, #45195, #54342, #21578, #31876, #12714, #44303, #53753, #13290, #49327, #26290, #44895, #4152, #22151, #55, #3859, #49031, #21857, #39866, #40159, #25998, #17436, #44021, #18030, #35421, #36022, #53451, #3573, #8579, #37189, #55203, #32166, #36610, #41626, #14462, #36897, #10052, #27450, #54910, #23903, #32453, #32745, #41049, #10339, #37775, #50793, #41338, #37476 ),
 ( #45488, #42219, #46370, #46662, #19780, #19198, #6189, #55796, #41921, #1784, #55497, #924, #14746, #15346, #5323, #24202, #1493, #28034, #54633, #28317, #23330, #15047, #18904, #50498, #33340, #1206, #9465, #637, #5894, #50205, #51085, #19483, #5031, #33039, #46078, #10635, #45787, #28617, #23033, #18619, #5602, #23613, #14169, #9755, #27740, #20925, #47243, #46955, #48104, #39214, #29198, #38926, #33912, #38352, #25636, #28911, #12071, #20075, #2077, #7065, #51671, #52515, #47819, #7636, #6481, #42506, #43090 ),
 ( #24493, #57228, #29482, #6774, #11507, #11218, #16793, #3220, #20641, #38643, #15633, #38066, #25066, #56374, #20357, #51951, #10930, #15924, #7350, #47541, #16216, #56087, #52231, #21207, #34194, #24783, #56943, #51373, #11788, #29763, #43661, #16502, #33629, #42798, #2648, #2359, #56661, #25349, #43366, #2924, #34485, #30052, #43947, #4373, #30342, #17361, #9097, #53974, #13212, #30634, #30918, #22374, #44229, #22675, #35347, #12641, #3497, #40386, #53372, #48667, #45125, #26790, #13513, #39788, #53088, #58393, #17956 ),
 ( #58096, #17072, #52801, #31207, #17658, #7923, #35947, #49247, #8211, #44818, #3781, #31506, #12921, #21783, #8797, #57801, #35645, #25923, #53672, #4676, #49552, #26213, #27086, #40686, #278, #34775, #12354, #48385, #21500, #57511, #48954, #39506, #35054, #8498, #26494, #22071, #44517, #4069, #40080, #46303, #13805, #852, #51016, #37409, #55131, #14104, #14388, #5826, #27671, #6123, #18836, #54564, #45419, #23833, #36829, #32100, #28549, #10268, #55429, #23259, #36541, #41850, #1429, #45717, #10566, #569, #41556 ) ),
 .UNSPECIFIED., .F., .F., .F.,
 ( 4, 4 ),
 ( 4, 1, 1, 1, 1, 1, 1, 1, 1, 1, 1, 1, 1, 1, 1, 1, 1, 1, 1, 1, 1, 1, 1, 1, 1, 1, 1, 1, 1, 1, 1, 1, 1, 1, 1, 1, 1, 1, 1, 1, 1, 1, 1, 1, 1, 1, 1, 1, 1, 1, 1, 1, 1, 1, 1, 1, 1, 1, 1, 1, 1, 1, 1, 1, 4 ),
 ( -0.1772706441294000235, 1.177270644128999955 ),
 ( -0.02000000000000000042, -0.003749999999999999861, 0.01250000000000000069, 0.02875000000000000125, 0.04499999999999999833, 0.06124999999999999889, 0.07749999999999999944, 0.09375000000000000000, 0.1100000000000000006, 0.1262500000000000011, 0.1424999999999999878, 0.1587500000000000022, 0.1749999999999999889, 0.1912500000000000033, 0.2074999999999999900, 0.2237500000000000044, 0.2399999999999999911, 0.2562499999999999778, 0.2725000000000000200, 0.2887500000000000067, 0.3049999999999999933, 0.3212499999999999800, 0.3375000000000000222, 0.3537500000000000089, 0.3699999999999999956, 0.3862499999999999822, 0.4025000000000000244, 0.4187500000000000111, 0.4349999999999999978, 0.4512499999999999845, 0.4675000000000000266, 0.4837500000000000133, 0.5000000000000000000, 0.5162499999999999867, 0.5324999999999999734, 0.5487499999999999600, 0.5649999999999999467, 0.5812500000000000444, 0.5975000000000000311, 0.6137500000000000178, 0.6300000000000000044, 0.6462499999999999911, 0.6624999999999999778, 0.6787499999999999645, 0.6949999999999999512, 0.7112500000000000488, 0.7275000000000000355, 0.7437500000000000222, 0.7600000000000000089, 0.7762499999999999956, 0.7924999999999999822, 0.8087499999999999689, 0.8249999999999999556, 0.8412500000000000533, 0.8575000000000000400, 0.8737500000000000266, 0.8900000000000000133, 0.9062500000000000000, 0.9224999999999999867, 0.9387499999999999734, 0.9549999999999999600, 0.9712499999999999467, 0.9875000000000000444, 1.003749999999999920, 1.020000000000000018 ),
 .UNSPECIFIED. ) ;
#12986 = DIRECTION ( 'NONE',  ( 6.203992508747998875E-09, -1.000000000000000000, 6.182590554452000020E-10 ) ) ;
#12987 = ORIENTED_EDGE ( 'NONE', *, *, #49558, .F. ) ;
#12988 = DIRECTION ( 'NONE',  ( 0.000000000000000000, 0.000000000000000000, -1.000000000000000000 ) ) ;
#12989 = CARTESIAN_POINT ( 'NONE',  ( -0.3959877895327999497, -81.85338596081999185, 1.414086365320999850 ) ) ;
#12990 = CARTESIAN_POINT ( 'NONE',  ( 1.249711497515000103, -80.16266235632998871, -0.7711480544179000196 ) ) ;
#12991 = CARTESIAN_POINT ( 'NONE',  ( -0.9768374075688754932, -77.83333333333224857, 1.065675943311487295 ) ) ;
#12992 = CYLINDRICAL_SURFACE ( 'NONE', #7889, 12.00000000000000000 ) ;
#12993 = DIRECTION ( 'NONE',  ( -0.3090169943748910519, 0.000000000000000000, 0.9510565162951719609 ) ) ;
#12994 = EDGE_CURVE ( 'NONE', #37470, #43983, #5595, .T. ) ;
#12995 = CARTESIAN_POINT ( 'NONE',  ( -0.6201509082777801884, -79.16543617070907146, 1.113615692535757429 ) ) ;
#12996 = CARTESIAN_POINT ( 'NONE',  ( -11.99938675919335651, -76.39122388691224330, 1.256423165442345447 ) ) ;
#12997 = CARTESIAN_POINT ( 'NONE',  ( 6.669449228234999971, -78.19499415034600531, -7.075468016816000016 ) ) ;
#12998 = CARTESIAN_POINT ( 'NONE',  ( -1.761265949711000145, -55.09141781180999686, -12.57448205041000122 ) ) ;
#12999 = CARTESIAN_POINT ( 'NONE',  ( 10.35033528849731077, -75.98912452525786421, 5.575283253277660833 ) ) ;
#13000 = CARTESIAN_POINT ( 'NONE',  ( -0.6747260877994001316, -82.22962677363800310, -1.052256958371999840 ) ) ;
#13001 = ORIENTED_EDGE ( 'NONE', *, *, #44045, .F. ) ;
#13002 = CARTESIAN_POINT ( 'NONE',  ( -1.500000000000000000, -79.39999999999999147, 0.000000000000000000 ) ) ;
#13003 = CARTESIAN_POINT ( 'NONE',  ( 10.58663230755379558, -78.98684970000721250, 5.411474183400683202 ) ) ;
#13004 = CARTESIAN_POINT ( 'NONE',  ( -3.547719542586254882, -78.43735717367049176, 0.06688145936885296627 ) ) ;
#13005 = CARTESIAN_POINT ( 'NONE',  ( 6.329984427697000093, -78.16117817800899559, 9.260097609460000712 ) ) ;
#13006 = CARTESIAN_POINT ( 'NONE',  ( 3.915498778898000687, -79.27612305176899099, 10.25343288338999947 ) ) ;
#13007 = CARTESIAN_POINT ( 'NONE',  ( -1.575772165385731283, -17.53845457198085711, 12.70597445617638144 ) ) ;
#13008 = CARTESIAN_POINT ( 'NONE',  ( -12.06623464587999983, -76.02337612386199339, -2.225025071791999931 ) ) ;
#13009 = CARTESIAN_POINT ( 'NONE',  ( -0.8690907654282591377, -78.57852448961540404, 11.75728093043408151 ) ) ;
#13010 = CARTESIAN_POINT ( 'NONE',  ( -1.247385803317999864, -61.27722255996999934, -12.50301438880000049 ) ) ;
#13011 = B_SPLINE_CURVE_WITH_KNOTS ( 'NONE', 3,
 ( #28258, #27971, #46896, #6719, #24438, #32687, #47187, #2020, #46021, #51316, #10574, #42157, #46312, #56027, #15576, #5542, #41860, #19428, #23552, #33571, #24138, #15867, #38295, #33853 ),
 .UNSPECIFIED., .F., .F.,
 ( 4, 2, 2, 2, 2, 2, 2, 2, 2, 2, 2, 4 ),
 ( 0.000000000000000000, 0.1249999999999965028, 0.2499999999999930056, 0.3749999999999895084, 0.4374999999999880096, 0.4999999999999865663, 0.6249999999999841238, 0.7499999999999817923, 0.8124999999999819034, 0.8437499999999832356, 0.8749999999999845679, 1.000000000000000000 ),
 .UNSPECIFIED. ) ;
#13012 = VERTEX_POINT ( 'NONE', #32444 ) ;
#13013 = CARTESIAN_POINT ( 'NONE',  ( 10.75129243007999946, -78.90912175438100462, 2.472133787718999720 ) ) ;
#13014 = CARTESIAN_POINT ( 'NONE',  ( 0.2973127429259597720, -79.95643973076548150, 1.214524578331088733 ) ) ;
#13015 = CIRCLE ( 'NONE', #15862, 1.250000000000000000 ) ;
#13016 = CARTESIAN_POINT ( 'NONE',  ( 1.439896632895333539, -77.73541666666666572, -10.99999999999999822 ) ) ;
#13017 = EDGE_CURVE ( 'NONE', #52316, #17327, #29162, .T. ) ;
#13018 = CARTESIAN_POINT ( 'NONE',  ( -10.97221500190000043, -79.25758784453798000, -2.025363574538999956 ) ) ;
#13019 = EDGE_CURVE ( 'NONE', #44485, #4989, #14077, .T. ) ;
#13020 = CARTESIAN_POINT ( 'NONE',  ( -12.50385602492088566, -54.01562718794550477, 0.8579628942656060131 ) ) ;
#13021 = CARTESIAN_POINT ( 'NONE',  ( -11.00000000000000000, -23.75000000000000000, 0.000000000000000000 ) ) ;
#13022 = CARTESIAN_POINT ( 'NONE',  ( 2.899999999999999911, -80.69999999999998863, 0.000000000000000000 ) ) ;
#13023 = CARTESIAN_POINT ( 'NONE',  ( 1.980584515756000030, -23.26485150094000076, 12.76303204340999997 ) ) ;
#13024 = CARTESIAN_POINT ( 'NONE',  ( 9.723199429438999175, -17.52306056078000296, -7.958735708418001487 ) ) ;
#13025 = CARTESIAN_POINT ( 'NONE',  ( 9.393203674808260573, -78.29166666666665719, 5.413904038987188194 ) ) ;
#13026 = CARTESIAN_POINT ( 'NONE',  ( -12.43641409351999982, -24.91801033895000117, -0.03481937293212000045 ) ) ;
#13027 = EDGE_LOOP ( 'NONE', ( #20539, #32778, #18496, #41457 ) ) ;
#13028 = EDGE_CURVE ( 'NONE', #4183, #51185, #14798, .T. ) ;
#13029 = VERTEX_POINT ( 'NONE', #35910 ) ;
#13030 = CARTESIAN_POINT ( 'NONE',  ( 7.596835002782719393, -78.59791666666667709, -5.838193839761677495 ) ) ;
#13031 = CARTESIAN_POINT ( 'NONE',  ( -9.378008371271000954, -77.64413998579800591, -1.764535237813999791 ) ) ;
#13032 = VERTEX_POINT ( 'NONE', #22639 ) ;
#13033 = CARTESIAN_POINT ( 'NONE',  ( -6.383854037583304830, -79.81686861624592666, -7.133078034627309272 ) ) ;
#13034 = ORIENTED_EDGE ( 'NONE', *, *, #52799, .T. ) ;
#13035 = CARTESIAN_POINT ( 'NONE',  ( 7.633403016703000254, -23.38650073851000144, 10.18126993294000115 ) ) ;
#13036 = CARTESIAN_POINT ( 'NONE',  ( -10.57583826563999985, -76.59334884066400662, -2.706834349011999930 ) ) ;
#13037 = VECTOR ( 'NONE', #21657, 1000.000000000000000 ) ;
#13038 = CARTESIAN_POINT ( 'NONE',  ( 4.479242302639000251, -77.96608998579800698, 8.589153267943999026 ) ) ;
#13039 = CARTESIAN_POINT ( 'NONE',  ( -3.536609267268810974, -78.19392279636586807, -8.547114838364091582 ) ) ;
#13040 = CARTESIAN_POINT ( 'NONE',  ( 10.63562707217000103, -80.04183570101619694, 3.563914325689000240 ) ) ;
#13041 = CARTESIAN_POINT ( 'NONE',  ( 1.065724622738618121, -79.39441019242424602, 0.6536201573516686736 ) ) ;
#13042 = ORIENTED_EDGE ( 'NONE', *, *, #6979, .F. ) ;
#13043 = ORIENTED_EDGE ( 'NONE', *, *, #19051, .F. ) ;
#13044 = CARTESIAN_POINT ( 'NONE',  ( 0.4664785593013082154, -77.47109208897903443, 9.249934602145987839 ) ) ;
#13045 = CARTESIAN_POINT ( 'NONE',  ( -1.996894868142000012, -77.25932187515898875, 10.85801781015000067 ) ) ;
#13046 = CARTESIAN_POINT ( 'NONE',  ( 7.596835002782719393, -77.59791666666664867, -5.838193839761677495 ) ) ;
#13047 = CARTESIAN_POINT ( 'NONE',  ( 1.487026788147999934, -77.46739383203798468, -9.589549613196998834 ) ) ;
#13048 = CARTESIAN_POINT ( 'NONE',  ( -9.584819989847998656, -76.38917353800999877, -8.495977810255999074 ) ) ;
#13049 = VECTOR ( 'NONE', #57648, 1000.000000000000000 ) ;
#13050 = CARTESIAN_POINT ( 'NONE',  ( -9.384480618050281109, -79.41205795043663329, -1.475605007748509223 ) ) ;
#13051 = CARTESIAN_POINT ( 'NONE',  ( 7.635226873531286707, -55.03391307102463514, -10.36745167320620808 ) ) ;
#13052 = CARTESIAN_POINT ( 'NONE',  ( -1.870137171474999915, -79.98156414243598533, -11.09839649295000008 ) ) ;
#13053 = CARTESIAN_POINT ( 'NONE',  ( 12.77302454167999990, -17.27764858556999883, -1.481891240072999993 ) ) ;
#13054 = CARTESIAN_POINT ( 'NONE',  ( -9.310177428684999867, -25.13531023636999961, -8.596745825432000387 ) ) ;
#13055 = CARTESIAN_POINT ( 'NONE',  ( -4.209390496675390558, -79.21181571460809323, 8.537567007200664193 ) ) ;
#13056 = EDGE_LOOP ( 'NONE', ( #36641, #22565, #8748, #41660 ) ) ;
#13057 = CARTESIAN_POINT ( 'NONE',  ( -9.793435742113999254, -78.88928473073799807, 7.469585195921999876 ) ) ;
#13058 = PLANE ( 'NONE',  #35313 ) ;
#13059 = CARTESIAN_POINT ( 'NONE',  ( -2.170310836754803852, -77.99131390061577918, 10.52858361609908577 ) ) ;
#13060 = CARTESIAN_POINT ( 'NONE',  ( 0.3864029911681999829, -77.32930023569899447, -11.74364478040999948 ) ) ;
#13061 = CARTESIAN_POINT ( 'NONE',  ( -12.72923908220886524, -60.57554307127314530, 1.930512971237506870 ) ) ;
#13062 = EDGE_CURVE ( 'NONE', #42403, #3300, #241, .T. ) ;
#13064 = DIRECTION ( 'NONE',  ( 1.000000000000000000, 0.000000000000000000, 0.000000000000000000 ) ) ;
#13063 = CARTESIAN_POINT ( 'NONE',  ( 7.640030264136999705, -55.49283319101999723, 10.18491080491000034 ) ) ;
#13065 = CARTESIAN_POINT ( 'NONE',  ( -1.250000000000000000, -23.44678171330999916, 12.50000000000000000 ) ) ;
#13066 = CARTESIAN_POINT ( 'NONE',  ( 5.496473448154000074, -80.39148163303399031, 9.863667302640999779 ) ) ;
#13067 = CARTESIAN_POINT ( 'NONE',  ( -0.5900578684300998855, -82.23765691653800047, -1.108170840844000082 ) ) ;
#13068 = CARTESIAN_POINT ( 'NONE',  ( 8.315675604772998497, -78.01451158974199984, -7.594965687514999786 ) ) ;
#13069 = CARTESIAN_POINT ( 'NONE',  ( 3.165411199172025292, -1.770833333333333481, 0.8506806241676674318 ) ) ;
#13070 = CARTESIAN_POINT ( 'NONE',  ( 1.957338178487000313, -80.18450047619698751, 11.08434491862000115 ) ) ;
#13071 = ADVANCED_FACE ( 'NONE', ( #36213 ), #24460, .F. ) ;
#13072 = VERTEX_POINT ( 'NONE', #54231 ) ;
#13073 = LINE ( 'NONE', #26359, #3698 ) ;
#13074 = CARTESIAN_POINT ( 'NONE',  ( 0.9887300587132999974, -53.86589942198000358, 12.65963207085999898 ) ) ;
#13075 = DIRECTION ( 'NONE',  ( 0.000000000000000000, 0.000000000000000000, 1.000000000000000000 ) ) ;
#13076 = CARTESIAN_POINT ( 'NONE',  ( 3.356323744093999917, -1.913384542061000060, 1.423708999316999790 ) ) ;
#13077 = CARTESIAN_POINT ( 'NONE',  ( -6.382469709265000013, -79.95501551942399487, 6.934717328048000340 ) ) ;
#13078 = DIRECTION ( 'NONE',  ( 0.000000000000000000, -1.000000000000000000, 0.000000000000000000 ) ) ;
#13079 = CARTESIAN_POINT ( 'NONE',  ( 11.00000000000000178, -77.34374999999998579, -0.8639379797371515846 ) ) ;
#13080 = CARTESIAN_POINT ( 'NONE',  ( -0.005523896503676999775, -61.86963456192999899, 12.55021156886000000 ) ) ;
#13081 = CARTESIAN_POINT ( 'NONE',  ( 12.43410192431999839, -17.55868879885999689, 1.192687910177000044 ) ) ;
#13082 = CARTESIAN_POINT ( 'NONE',  ( -1.732973334768000084, -82.91469503318799639, 3.795637342627999899 ) ) ;
#13083 = VECTOR ( 'NONE', #27141, 1000.000000000000000 ) ;
#13084 = CARTESIAN_POINT ( 'NONE',  ( 0.000000000000000000, -77.59999999938000315, 0.000000000000000000 ) ) ;
#13085 = CARTESIAN_POINT ( 'NONE',  ( 7.575978808960503130, -77.13227571528085491, -9.335878689481054593 ) ) ;
#13086 = CARTESIAN_POINT ( 'NONE',  ( 10.59026995113000069, -79.47130787033000843, -4.872245490990999350 ) ) ;
#13087 = CARTESIAN_POINT ( 'NONE',  ( -2.194598275924000141, -77.88598375397499751, -11.04616236372000060 ) ) ;
#13088 = EDGE_CURVE ( 'NONE', #26901, #29384, #26708, .T. ) ;
#13089 = CARTESIAN_POINT ( 'NONE',  ( 0.5348319831205907704, -81.93981601381945268, 1.130533534708823229 ) ) ;
#13090 = CARTESIAN_POINT ( 'NONE',  ( -1.491498510839000202, -78.37157334178999690, 0.4184882615579000320 ) ) ;
#13091 = CARTESIAN_POINT ( 'NONE',  ( 1.495357591765385630, -61.35876337328488717, 12.70444646763499108 ) ) ;
#13092 = CARTESIAN_POINT ( 'NONE',  ( 1.509093300816331418, -82.99695827279550997, -0.05655753630307266966 ) ) ;
#13093 = CARTESIAN_POINT ( 'NONE',  ( -5.052420809101000088E-14, -80.84999999994215614, 0.000000000000000000 ) ) ;
#13094 = CARTESIAN_POINT ( 'NONE',  ( 2.155490813879537448, -80.24142094974830286, -10.53147914176322075 ) ) ;
#13095 = CARTESIAN_POINT ( 'NONE',  ( 0.000000000000000000, -0.09999999995300053179, -13.89999999994999946 ) ) ;
#13096 = CARTESIAN_POINT ( 'NONE',  ( 0.03840800099673202100, -77.77721185482320720, -1.273617133072684426 ) ) ;
#13097 = AXIS2_PLACEMENT_3D ( 'NONE', #27575, #54747, #759 ) ;
#13098 = CARTESIAN_POINT ( 'NONE',  ( 1.140339328391035467, -81.81637019837238256, -0.5133320548427554586 ) ) ;
#13099 = CARTESIAN_POINT ( 'NONE',  ( 0.000000000000000000, -80.49999999999998579, 0.000000000000000000 ) ) ;
#13100 = CARTESIAN_POINT ( 'NONE',  ( -10.99597256337999873, -79.40424884139699202, -1.828438666275999935 ) ) ;
#13101 = CARTESIAN_POINT ( 'NONE',  ( -0.3271848554490991434, -80.10416666666667140, -1.217465845835395299 ) ) ;
#13102 = VERTEX_POINT ( 'NONE', #6670 ) ;
#13103 = EDGE_CURVE ( 'NONE', #38250, #22857, #48074, .T. ) ;
#13104 = ORIENTED_EDGE ( 'NONE', *, *, #1527, .T. ) ;
#13105 = CARTESIAN_POINT ( 'NONE',  ( -1.365100536947999821, -80.53103368013600516, -0.7251819899571000372 ) ) ;
#13106 = EDGE_CURVE ( 'NONE', #15092, #32066, #14070, .T. ) ;
#13107 = EDGE_LOOP ( 'NONE', ( #57482, #47424, #29167, #2198 ) ) ;
#13108 = VERTEX_POINT ( 'NONE', #47426 ) ;
#13109 = DIRECTION ( 'NONE',  ( 0.000000000000000000, 0.000000000000000000, -1.000000000000000000 ) ) ;
#13110 = CARTESIAN_POINT ( 'NONE',  ( 0.000000000000000000, -75.15999999999999659, 0.000000000000000000 ) ) ;
#13111 = CARTESIAN_POINT ( 'NONE',  ( -8.833962032441000645, -79.59003032942598566, 6.607787011616999884 ) ) ;
#13112 = CARTESIAN_POINT ( 'NONE',  ( -12.00000000000000178, -76.31041666661776901, -1.570796326794897890 ) ) ;
#13113 = CARTESIAN_POINT ( 'NONE',  ( -3.613773621817000237, -78.97078559807879117, 0.5228172038748000183 ) ) ;
#13114 = CARTESIAN_POINT ( 'NONE',  ( -1.479726591698317328, -79.28725347445197258, 9.383940043454046531 ) ) ;
#13115 = ORIENTED_EDGE ( 'NONE', *, *, #51849, .T. ) ;
#13116 = CARTESIAN_POINT ( 'NONE',  ( -8.283402485400999993, -77.90747789361365960, -7.298588567666998372 ) ) ;
#13117 = CARTESIAN_POINT ( 'NONE',  ( -11.97043380835999926, -78.40274619638999809, 2.407544143317999819 ) ) ;
#13118 = VERTEX_POINT ( 'NONE', #19967 ) ;
#13119 = ORIENTED_EDGE ( 'NONE', *, *, #57844, .T. ) ;
#13120 = CARTESIAN_POINT ( 'NONE',  ( 7.919595949288999570, -55.65000000488999632, 8.768124086549999419 ) ) ;
#13121 = LINE ( 'NONE', #7835, #43324 ) ;
#13122 = CARTESIAN_POINT ( 'NONE',  ( -0.1698911186725000078, -80.65082589376000044, 1.322768475116000042 ) ) ;
#13123 = CARTESIAN_POINT ( 'NONE',  ( -8.073459667400001649, -78.25635051282399957, -5.384232384047000330 ) ) ;
#13124 = EDGE_CURVE ( 'NONE', #36059, #38869, #2824, .T. ) ;
#13125 = CARTESIAN_POINT ( 'NONE',  ( -3.802013078733825324, -86.17851881763698429, -2.653507570502878998 ) ) ;
#13126 = CARTESIAN_POINT ( 'NONE',  ( 9.776276929627000456, -76.11132973067898888, -5.431214116490000521 ) ) ;
#13127 = CARTESIAN_POINT ( 'NONE',  ( -12.50000000000000000, -23.25000000000000000, 0.000000000000000000 ) ) ;
#13128 = CARTESIAN_POINT ( 'NONE',  ( -10.25367346088999909, -77.69466387191998535, 7.393739220494000008 ) ) ;
#13129 = CARTESIAN_POINT ( 'NONE',  ( 5.896171905175000560, -77.86999999999999034, 7.127247495676000355 ) ) ;
#13130 = CARTESIAN_POINT ( 'NONE',  ( -8.823800648792902379, -78.62434323315024187, -2.778829492415963553 ) ) ;
#13131 = CARTESIAN_POINT ( 'NONE',  ( -3.165913743354999532, -79.05481202895639115, -2.652492535831999731 ) ) ;
#13132 = CIRCLE ( 'NONE', #53690, 13.89999999999999858 ) ;
#13133 = CARTESIAN_POINT ( 'NONE',  ( -10.59551070214999946, -57.04351820043999766, 7.678690995233999672 ) ) ;
#13134 = CARTESIAN_POINT ( 'NONE',  ( 1.208728522240711367, -2.945855492842563095, 3.016110857596538963 ) ) ;
#13135 = CARTESIAN_POINT ( 'NONE',  ( 0.4740280817681999936, -79.11955496681159161, -3.515234240849999914 ) ) ;
#13136 = ADVANCED_FACE ( 'NONE', ( #11975 ), #47715, .F. ) ;
#13137 = AXIS2_PLACEMENT_3D ( 'NONE', #30247, #35245, #48855 ) ;
#13138 = DIRECTION ( 'NONE',  ( 0.000000000000000000, -1.000000000000000000, 0.000000000000000000 ) ) ;
#13139 = CARTESIAN_POINT ( 'NONE',  ( 9.250000000000000000, -78.74999999999998579, 0.000000000000000000 ) ) ;
#13140 = CARTESIAN_POINT ( 'NONE',  ( -3.593558748265999636, -1.779776491687000028, 0.1459214154804999997 ) ) ;
#13141 = CARTESIAN_POINT ( 'NONE',  ( -0.6452061973881114687, -80.16722482396566818, 1.099126683074162392 ) ) ;
#13142 = ADVANCED_FACE ( 'NONE', ( #25538 ), #923, .F. ) ;
#13143 = EDGE_LOOP ( 'NONE', ( #492, #52001, #40928, #3965 ) ) ;
#13144 = DIRECTION ( 'NONE',  ( -1.000000000000000000, 0.000000000000000000, 0.000000000000000000 ) ) ;
#13145 = CARTESIAN_POINT ( 'NONE',  ( -5.539808784079887083, -79.28333333333333144, -9.611650271896841957 ) ) ;
#13146 = CARTESIAN_POINT ( 'NONE',  ( -0.4870599102559999838, -82.27173306887900139, -1.180149847382000017 ) ) ;
#13147 = CARTESIAN_POINT ( 'NONE',  ( -12.54705919859000041, -17.46307476627999833, -1.287183453418999868 ) ) ;
#13148 = CARTESIAN_POINT ( 'NONE',  ( -3.274010471232999819, -77.41257207022999864, 12.59444704299999884 ) ) ;
#13149 = CARTESIAN_POINT ( 'NONE',  ( 1.875550138011000012, -79.64748667140099769, -9.444652722706999626 ) ) ;
#13150 = CARTESIAN_POINT ( 'NONE',  ( 12.87022657274000004, -19.21514526754999963, -2.062597299672999540 ) ) ;
#13151 = VERTEX_POINT ( 'NONE', #20821 ) ;
#13152 = CARTESIAN_POINT ( 'NONE',  ( -14.00000000000000000, -69.50420297070000686, 0.000000000000000000 ) ) ;
#13153 = CARTESIAN_POINT ( 'NONE',  ( -5.869402599192000025, -78.36567021304000491, 10.46661899222999992 ) ) ;
#13154 = CARTESIAN_POINT ( 'NONE',  ( -0.7187448651093000240, -81.71493067372900043, 1.211279877421999940 ) ) ;
#13155 = DIRECTION ( 'NONE',  ( 1.000000000000000000, 0.000000000000000000, 0.000000000000000000 ) ) ;
#13156 = CARTESIAN_POINT ( 'NONE',  ( -9.171168281578999881, -77.93526618914198423, 2.561259179188999813 ) ) ;
#13158 = CARTESIAN_POINT ( 'NONE',  ( -0.1204595238885999980, -0.6950726927052999216, 3.497926457646999943 ) ) ;
#13157 = CARTESIAN_POINT ( 'NONE',  ( -1.734896692008999874, -84.78318437814699848, -3.748152468934999870 ) ) ;
#13159 = CARTESIAN_POINT ( 'NONE',  ( 12.00000000000000000, -60.04999999966999980, 1.250000000000000000 ) ) ;
#13160 = CARTESIAN_POINT ( 'NONE',  ( -0.6438247211726000341, -80.19017497096899660, -1.263150469460000203 ) ) ;
#13161 = ORIENTED_EDGE ( 'NONE', *, *, #24328, .T. ) ;
#13162 = CARTESIAN_POINT ( 'NONE',  ( -4.665370423308930370, -77.18929613357201447, -9.684859775919129277 ) ) ;
#13163 = PLANE ( 'NONE',  #41741 ) ;
#13164 = CARTESIAN_POINT ( 'NONE',  ( -0.4969611113247792145, -78.87321456624501081, -3.919997644563975037 ) ) ;
#13165 = ORIENTED_EDGE ( 'NONE', *, *, #45440, .T. ) ;
#13166 = VERTEX_POINT ( 'NONE', #3402 ) ;
#13167 = CARTESIAN_POINT ( 'NONE',  ( -6.898009915208000109, -79.44152403476999780, -8.491482529321999095 ) ) ;
#13168 = CARTESIAN_POINT ( 'NONE',  ( 0.000000000000000000, -33.10361340872000113, 0.000000000000000000 ) ) ;
#13169 = CARTESIAN_POINT ( 'NONE',  ( 9.050966798898000931, -55.65000000893999754, -7.919595949288999570 ) ) ;
#13170 = ORIENTED_EDGE ( 'NONE', *, *, #125, .T. ) ;
#13171 = B_SPLINE_CURVE_WITH_KNOTS ( 'NONE', 3,
 ( #56238, #25216, #34062, #39085, #30212, #11942 ),
 .UNSPECIFIED., .F., .F.,
 ( 4, 2, 4 ),
 ( 0.000000000000000000, 0.5000000000000000000, 1.000000000000000000 ),
 .UNSPECIFIED. ) ;
#13172 = CARTESIAN_POINT ( 'NONE',  ( 5.516244905679999810, -78.96017368086199895, 10.58329673088999989 ) ) ;
#13173 = AXIS2_PLACEMENT_3D ( 'NONE', #20172, #10738, #28125 ) ;
#13174 = ADVANCED_FACE ( 'NONE', ( #21111 ), #6539, .F. ) ;
#13175 = ORIENTED_EDGE ( 'NONE', *, *, #52470, .T. ) ;
#13176 = B_SPLINE_SURFACE_WITH_KNOTS ( 'NONE', 3, 3, ( 
 ( #49795, #54790, #27032, #23203 ),
 ( #26737, #26443, #9631, #44768 ),
 ( #4317, #22317, #22912, #44465 ),
 ( #40334, #35895, #27619, #53927 ),
 ( #5202, #45364, #41208, #32329 ),
 ( #8448, #31455, #4016, #22022 ),
 ( #4913, #58044, #49497, #9046 ),
 ( #45069, #4621, #22620, #40632 ) ),
 .UNSPECIFIED., .F., .F., .F.,
 ( 4, 1, 1, 1, 1, 4 ),
 ( 4, 4 ),
 ( -0.01200407345746999990, 0.000000000000000000, 0.3333333333333000081, 0.6666666666667000474, 1.000000000000000000, 1.011997855551999947 ),
 ( -0.3559705542741999906, 1.355970554273999928 ),
 .UNSPECIFIED. ) ;
#13177 = VERTEX_POINT ( 'NONE', #56552 ) ;
#13178 = AXIS2_PLACEMENT_3D ( 'NONE', #46400, #5633, #37217 ) ;
#13179 = CARTESIAN_POINT ( 'NONE',  ( 7.345153731672220410, -60.02841244177673730, 8.188331488387616375 ) ) ;
#13180 = CARTESIAN_POINT ( 'NONE',  ( -10.48543666025111420, -78.75833333333331154, 6.043427764450754580 ) ) ;
#13181 = CARTESIAN_POINT ( 'NONE',  ( -9.250000000000000000, -79.59999999999999432, 0.000000000000000000 ) ) ;
#13182 = ORIENTED_EDGE ( 'NONE', *, *, #1611, .T. ) ;
#13183 = CARTESIAN_POINT ( 'NONE',  ( -12.00000000000000000, -23.25000000000000000, -1.250000000000000000 ) ) ;
#13184 = ORIENTED_EDGE ( 'NONE', *, *, #27381, .F. ) ;
#13185 = CARTESIAN_POINT ( 'NONE',  ( 7.395663543987498478, -79.29799491392495270, -5.683475073351669238 ) ) ;
#13186 = CARTESIAN_POINT ( 'NONE',  ( 3.548349909810999847, -78.96264282632948550, -2.094141712711119485 ) ) ;
#13187 = DIRECTION ( 'NONE',  ( 0.7071067811865474617, 0.7071067811865474617, 6.623688493237445538E-09 ) ) ;
#13188 = EDGE_CURVE ( 'NONE', #25114, #16112, #42953, .T. ) ;
#13189 = DIRECTION ( 'NONE',  ( 0.000000000000000000, -1.000000000000000000, 0.000000000000000000 ) ) ;
#13190 = CARTESIAN_POINT ( 'NONE',  ( 11.15465700714716135, -77.42101778503236176, -3.785658037966275202 ) ) ;
#13191 = ADVANCED_FACE ( 'NONE', ( #39119 ), #34961, .F. ) ;
#13192 = CARTESIAN_POINT ( 'NONE',  ( -1.532229593853648764, -54.67701036647127211, 12.51228690871742977 ) ) ;
#13193 = CARTESIAN_POINT ( 'NONE',  ( 7.613962827198000660, -60.10639625617000092, -10.53101998748999968 ) ) ;
#13194 = CARTESIAN_POINT ( 'NONE',  ( 11.00000000000000000, -79.84999999999999432, 0.000000000000000000 ) ) ;
#13195 = CARTESIAN_POINT ( 'NONE',  ( 0.5962167095188528609, -23.22841244210244938, -10.98383273456533260 ) ) ;
#13196 = CARTESIAN_POINT ( 'NONE',  ( 1.500000000000000000, -80.15000000000000568, 0.000000000000000000 ) ) ;
#13197 = CARTESIAN_POINT ( 'NONE',  ( 3.934662594658999257, -81.04355496681199611, 1.388701755431000162 ) ) ;
#13198 = CARTESIAN_POINT ( 'NONE',  ( 3.712903092914000336, -78.03551332859899503, 8.550517029640001709 ) ) ;
#13199 = CARTESIAN_POINT ( 'NONE',  ( 0.000000000000000000, -33.10361340872000113, 0.000000000000000000 ) ) ;
#13200 = CARTESIAN_POINT ( 'NONE',  ( 6.760013919724039866, -77.92291666666667993, 8.796335266379998075 ) ) ;
#13201 = CARTESIAN_POINT ( 'NONE',  ( 0.9113424693944999211, -24.82535793559999959, 12.54674099557999867 ) ) ;
#13202 = CARTESIAN_POINT ( 'NONE',  ( -1.321889952614464736, -81.24455604087124527, 0.09328200148542904746 ) ) ;
#13203 = FACE_BOUND ( 'NONE', #53792, .T. ) ;
#13204 = ADVANCED_FACE ( 'NONE', ( #24961, #30822 ), #48288, .F. ) ;
#13205 = CARTESIAN_POINT ( 'NONE',  ( -3.640412412913000217, -0.9909739483179998976, -1.054207720119999969 ) ) ;
#13206 = CARTESIAN_POINT ( 'NONE',  ( 4.789894294226004767, -79.31810081118388212, -7.967628558423081486 ) ) ;
#13207 = CARTESIAN_POINT ( 'NONE',  ( -1.057528278039415515, -80.41407927041096571, -1.131349316642257019 ) ) ;
#13208 = CARTESIAN_POINT ( 'NONE',  ( 1.980584515752000119, -60.06485146591000301, -12.76303204605000197 ) ) ;
#13209 = CARTESIAN_POINT ( 'NONE',  ( -9.250000000000000000, -78.59999999999999432, 0.000000000000000000 ) ) ;
#13210 = CARTESIAN_POINT ( 'NONE',  ( -6.797161730763000342, -77.45507517892998806, 8.542479639784000156 ) ) ;
#13211 = AXIS2_PLACEMENT_3D ( 'NONE', #40306, #58314, #45038 ) ;
#13212 = CARTESIAN_POINT ( 'NONE',  ( -5.342744711435999605, -77.52995223578199102, -10.92875150845999954 ) ) ;
#13213 = CARTESIAN_POINT ( 'NONE',  ( 1.199500263597268246, -80.80208333333334281, 0.9218200799623752495 ) ) ;
#13214 = AXIS2_PLACEMENT_3D ( 'NONE', #53030, #39732, #7001 ) ;
#13215 = ADVANCED_FACE ( 'NONE', ( #52702 ), #12255, .T. ) ;
#13217 = CARTESIAN_POINT ( 'NONE',  ( -1.403409243600000300, -78.80864840198100296, -0.2012507760191999950 ) ) ;
#13216 = CARTESIAN_POINT ( 'NONE',  ( -0.7554284705563540925, -79.81666666666667709, 1.310679582531384391 ) ) ;
#13218 = CARTESIAN_POINT ( 'NONE',  ( 1.575652246471999973, -82.55093166112899894, 0.6458614041720999177 ) ) ;
#13219 = ORIENTED_EDGE ( 'NONE', *, *, #57288, .T. ) ;
#13220 = CARTESIAN_POINT ( 'NONE',  ( 1.885058010937000095, -85.88132450217399594, 3.054554980983000156 ) ) ;
#13221 = CARTESIAN_POINT ( 'NONE',  ( -6.472232015619999501, -79.04405766632500274, 10.01728928138000008 ) ) ;
#13222 = EDGE_CURVE ( 'NONE', #17310, #18079, #40091, .T. ) ;
#13223 = CARTESIAN_POINT ( 'NONE',  ( -10.11188841328999999, -80.54028613825869343, 4.470155568018000736 ) ) ;
#13224 = CARTESIAN_POINT ( 'NONE',  ( -9.723174505940001211, -24.47697504200000296, -7.958760297012999807 ) ) ;
#13225 = FACE_OUTER_BOUND ( 'NONE', #21824, .T. ) ;
#13226 = CARTESIAN_POINT ( 'NONE',  ( 9.668944085725000193, -77.12619714393999004, 5.685915129398999568 ) ) ;
#13227 = CARTESIAN_POINT ( 'NONE',  ( -12.85140862673999784, -58.55560170131000319, -1.980464483675000054 ) ) ;
#13228 = CARTESIAN_POINT ( 'NONE',  ( -4.299999999999999822, -74.99999999999998579, 0.000000000000000000 ) ) ;
#13229 = CARTESIAN_POINT ( 'NONE',  ( -3.688842081945000295, -1.137975590836000084, -0.3027291113864000183 ) ) ;
#13230 = DIRECTION ( 'NONE',  ( -0.7071067811865475727, 0.000000000000000000, -0.7071067811865475727 ) ) ;
#13231 = CARTESIAN_POINT ( 'NONE',  ( 12.43410103865999972, -24.44137177768999791, -1.192638008239000014 ) ) ;
#13232 = DIRECTION ( 'NONE',  ( 0.000000000000000000, 0.000000000000000000, 1.000000000000000000 ) ) ;
#13233 = VERTEX_POINT ( 'NONE', #54459 ) ;
#13234 = CARTESIAN_POINT ( 'NONE',  ( -12.76303204513999923, -55.53514852210999919, 1.980584515753000208 ) ) ;
#13235 = CARTESIAN_POINT ( 'NONE',  ( 8.092873224492999285, -79.48731332859900078, 5.022488412950999681 ) ) ;
#13236 = CARTESIAN_POINT ( 'NONE',  ( -3.003066045103267800, -1.634010044345757695, -1.313579205990373699 ) ) ;
#13237 = CARTESIAN_POINT ( 'NONE',  ( -10.21380041493999968, -56.02847221959000024, -7.668936932630000314 ) ) ;
#13238 = CARTESIAN_POINT ( 'NONE',  ( -2.847971885115999857, -83.02867953870898532, 2.115090749172999995 ) ) ;
#13239 = DIRECTION ( 'NONE',  ( 0.000000000000000000, -1.000000000000000000, 0.000000000000000000 ) ) ;
#13240 = ORIENTED_EDGE ( 'NONE', *, *, #34746, .T. ) ;
#13241 = AXIS2_PLACEMENT_3D ( 'NONE', #38283, #48042, #29988 ) ;
#13242 = DIRECTION ( 'NONE',  ( 0.000000000000000000, -1.000000000000000000, 0.000000000000000000 ) ) ;
#13243 = CARTESIAN_POINT ( 'NONE',  ( 0.000000000000000000, -74.64999999999999147, 0.000000000000000000 ) ) ;
#13244 = DIRECTION ( 'NONE',  ( -0.7071067811865474617, 0.000000000000000000, -0.7071067811865474617 ) ) ;
#13245 = ORIENTED_EDGE ( 'NONE', *, *, #21693, .F. ) ;
#13246 = ORIENTED_EDGE ( 'NONE', *, *, #46423, .T. ) ;
#13247 = CARTESIAN_POINT ( 'NONE',  ( -8.485548443509001615, -53.91931586703000079, -9.101490738433000161 ) ) ;
#13248 = FILL_AREA_STYLE ('',( #40719 ) ) ;
#13249 = CARTESIAN_POINT ( 'NONE',  ( 8.193575559979001000, -79.06565196373898630, 5.316613930189999948 ) ) ;
#13250 = ORIENTED_EDGE ( 'NONE', *, *, #24826, .F. ) ;
#13251 = ORIENTED_EDGE ( 'NONE', *, *, #23281, .T. ) ;
#13252 = CARTESIAN_POINT ( 'NONE',  ( -11.34677089036000019, -76.65391306960999884, -4.575788746496000314 ) ) ;
#13253 = CARTESIAN_POINT ( 'NONE',  ( -12.50000000000000000, -23.25000000000000000, 0.000000000000000000 ) ) ;
#13254 = CIRCLE ( 'NONE', #43496, 12.05000000000000071 ) ;
#13255 = CARTESIAN_POINT ( 'NONE',  ( 1.574466862065000194, -78.99606712646000517, -0.4877912776778999815 ) ) ;
#13256 = ORIENTED_EDGE ( 'NONE', *, *, #19101, .F. ) ;
#13257 = DIRECTION ( 'NONE',  ( 1.000000000000000000, 0.000000000000000000, 0.000000000000000000 ) ) ;
#13258 = CIRCLE ( 'NONE', #20820, 14.00000000000000000 ) ;
#13259 = CARTESIAN_POINT ( 'NONE',  ( -7.844108077142347035, -77.79981011384823830, 5.713474972744468694 ) ) ;
#13260 = CARTESIAN_POINT ( 'NONE',  ( 0.4850963087208033375, -80.25687247894693144, -1.151929813589695373 ) ) ;
#13261 = CARTESIAN_POINT ( 'NONE',  ( -10.72428337452000058, -76.94558033460998558, 7.546888592172999566 ) ) ;
#13262 = UNCERTAINTY_MEASURE_WITH_UNIT (LENGTH_MEASURE( 1.000000000000000082E-05 ), #3121, 'distance_accuracy_value', 'NONE');
#13263 = CARTESIAN_POINT ( 'NONE',  ( -0.9512330062464997571, -78.13175697154288457, 11.17646036812999633 ) ) ;
#13264 = DIRECTION ( 'NONE',  ( -1.000000000000000000, 0.000000000000000000, 0.000000000000000000 ) ) ;
#13265 = CARTESIAN_POINT ( 'NONE',  ( -3.605449341530932106, -86.31452044229999387, 1.524483932634073335 ) ) ;
#13266 = CARTESIAN_POINT ( 'NONE',  ( -10.34326456654000026, -78.87006834348099460, 4.339929572939999147 ) ) ;
#13267 = CARTESIAN_POINT ( 'NONE',  ( 8.240432763520827208, -79.88799569061337991, 4.201471099154182376 ) ) ;
#13268 = CARTESIAN_POINT ( 'NONE',  ( -8.838834764832000701, -23.25000000000000000, 8.838834764832000701 ) ) ;
#13269 = ORIENTED_EDGE ( 'NONE', *, *, #22775, .T. ) ;
#13270 = DIRECTION ( 'NONE',  ( -1.206135027324979392E-11, 1.868136817095964273E-07, 0.9999999999999824585 ) ) ;
#13271 = CARTESIAN_POINT ( 'NONE',  ( 12.17088485526999975, -75.81397293882999122, 1.845041276493999849 ) ) ;
#13272 = CARTESIAN_POINT ( 'NONE',  ( 2.969846905577856688, -2.646672701395195837, 1.998772415440041472 ) ) ;
#13273 = CARTESIAN_POINT ( 'NONE',  ( -7.864797288620628990, -17.54877151179043793, 10.10445166986456123 ) ) ;
#13274 = CARTESIAN_POINT ( 'NONE',  ( -1.250000000000000000, -81.49999999999998579, 0.000000000000000000 ) ) ;
#13275 = CARTESIAN_POINT ( 'NONE',  ( 0.000000000000000000, -77.50000000000000000, 0.000000000000000000 ) ) ;
#13276 = CARTESIAN_POINT ( 'NONE',  ( 11.03731426084000056, -79.31863239632698992, 1.633797283747999929 ) ) ;
#13277 = ADVANCED_FACE ( 'NONE', ( #53873, #18149 ), #18729, .T. ) ;
#13278 = CARTESIAN_POINT ( 'NONE',  ( 4.339214180343000216, -77.71673998579798592, 8.489796212882000148 ) ) ;
#13279 = CARTESIAN_POINT ( 'NONE',  ( -7.393247292513355440, -77.12252906155467258, -9.541960917511291385 ) ) ;
#13280 = FACE_OUTER_BOUND ( 'NONE', #9511, .T. ) ;
#13281 = CARTESIAN_POINT ( 'NONE',  ( 5.622824352109999424, -79.91678498981538326, -9.705769245306999693 ) ) ;
#13282 = CARTESIAN_POINT ( 'NONE',  ( -10.75000000000000000, -78.00000000000000000, 2.252154972635999871E-14 ) ) ;
#13283 = AXIS2_PLACEMENT_3D ( 'NONE', #18215, #32052, #36206 ) ;
#13284 = ORIENTED_EDGE ( 'NONE', *, *, #34756, .F. ) ;
#13285 = CARTESIAN_POINT ( 'NONE',  ( -1.446479059201000172, -82.92693514403299559, -0.6496884318727998986 ) ) ;
#13286 = CARTESIAN_POINT ( 'NONE',  ( 1.250000000000000000, -78.85000000000000853, 0.000000000000000000 ) ) ;
#13287 = DIRECTION ( 'NONE',  ( 0.000000000000000000, 0.7071067811866525998, -0.7071067811864425456 ) ) ;
#13288 = CARTESIAN_POINT ( 'NONE',  ( -9.690626710582000314, -78.04833130027799371, -7.043281791253000357 ) ) ;
#13289 = CARTESIAN_POINT ( 'NONE',  ( 6.134715390259300349, -76.99999999999998579, 6.994583833444441012 ) ) ;
#13290 = CARTESIAN_POINT ( 'NONE',  ( 4.881373948557000020, -78.23512198850700372, -10.89071580847000220 ) ) ;
#13291 = CARTESIAN_POINT ( 'NONE',  ( -8.871933854994999535, -78.54339415034600336, -3.979018739998999354 ) ) ;
#13292 = CARTESIAN_POINT ( 'NONE',  ( 8.959721679174998954, -77.36557598619799592, -3.223936051704999972 ) ) ;
#13293 = CARTESIAN_POINT ( 'NONE',  ( 1.194090706002000069, -54.35968341064000242, -12.43436538485999954 ) ) ;
#13294 = CARTESIAN_POINT ( 'NONE',  ( 4.630631704076160204, -76.04223606416009318, 10.79891528241036092 ) ) ;
#13295 = CARTESIAN_POINT ( 'NONE',  ( -6.040190233171999878, -79.94824811525009522, 9.093484917090998820 ) ) ;
#13296 = PLANE ( 'NONE',  #41746 ) ;
#13297 = VERTEX_POINT ( 'NONE', #49447 ) ;
#13298 = CARTESIAN_POINT ( 'NONE',  ( -9.500000000000003553, -78.29250000000001819, 0.8953539062730667686 ) ) ;
#13299 = CARTESIAN_POINT ( 'NONE',  ( -9.344545319423653851, -77.14671203089999096, 7.168886721853569455 ) ) ;
#13300 = ADVANCED_FACE ( 'NONE', ( #750 ), #22595, .F. ) ;
#13301 = CARTESIAN_POINT ( 'NONE',  ( 3.437187628289000152, -78.54828564506388489, -2.028536691635913325 ) ) ;
#13302 = VECTOR ( 'NONE', #55991, 1000.000000000000000 ) ;
#13303 = CARTESIAN_POINT ( 'NONE',  ( -6.920341278396000106, -79.50086188642998763, -8.518972542050999408 ) ) ;
#13304 = DIRECTION ( 'NONE',  ( 0.7071067811865475727, 0.000000000000000000, -0.7071067811865475727 ) ) ;
#13305 = CARTESIAN_POINT ( 'NONE',  ( -10.64045665439999944, -76.48390739571800623, -6.341743875680000642 ) ) ;
#13306 = CARTESIAN_POINT ( 'NONE',  ( -12.76303204294000082, -18.73514849292999784, -1.980584515756000030 ) ) ;
#13307 = FACE_OUTER_BOUND ( 'NONE', #43789, .T. ) ;
#13308 = EDGE_LOOP ( 'NONE', ( #39232, #44263, #53500, #49879 ) ) ;
#13309 = CARTESIAN_POINT ( 'NONE',  ( 8.588590363140999884, -79.97061154526829796, -7.284921508032001114 ) ) ;
#13310 = CARTESIAN_POINT ( 'NONE',  ( 0.4375120388952565831, -79.94686972374893230, 1.170817719393832279 ) ) ;
#13311 = CARTESIAN_POINT ( 'NONE',  ( 11.07590168690624921, -75.80000000000001137, -4.579409602955339054 ) ) ;
#13312 = DIRECTION ( 'NONE',  ( -1.000000000000000000, 0.000000000000000000, 0.000000000000000000 ) ) ;
#13313 = CARTESIAN_POINT ( 'NONE',  ( 4.105747930350998942, -79.39804961620099277, -10.37470161445000016 ) ) ;
#13314 = CARTESIAN_POINT ( 'NONE',  ( -12.00000000000000000, -18.84999999999999787, 0.000000000000000000 ) ) ;
#13315 = CARTESIAN_POINT ( 'NONE',  ( -10.98449824368628569, -23.30634943317874885, 0.5845455749771404363 ) ) ;
#13316 = EDGE_CURVE ( 'NONE', #18942, #48890, #1, .T. ) ;
#13317 = CARTESIAN_POINT ( 'NONE',  ( -11.90546970521999981, -77.80688910291300431, 3.009247460619000059 ) ) ;
#13318 = DIRECTION ( 'NONE',  ( 0.000000000000000000, 1.000000000000000000, 0.000000000000000000 ) ) ;
#13319 = DIRECTION ( 'NONE',  ( 0.000000000000000000, -0.7071067811866525998, -0.7071067811864425456 ) ) ;
#13320 = CARTESIAN_POINT ( 'NONE',  ( -12.76303204525000012, -60.06485147653999945, -1.980584515753000208 ) ) ;
#13321 = CARTESIAN_POINT ( 'NONE',  ( 10.20000000000000107, -0.5000000000000000000, 0.000000000000000000 ) ) ;
#13322 = ORIENTED_EDGE ( 'NONE', *, *, #17478, .F. ) ;
#13323 = ORIENTED_EDGE ( 'NONE', *, *, #46847, .T. ) ;
#13324 =( GEOMETRIC_REPRESENTATION_CONTEXT ( 3 ) GLOBAL_UNCERTAINTY_ASSIGNED_CONTEXT ( ( #24256 ) ) GLOBAL_UNIT_ASSIGNED_CONTEXT ( ( #52057, #16036, #7462 ) ) REPRESENTATION_CONTEXT ( 'NONE', 'WORKASPACE' ) );
#13325 = DIRECTION ( 'NONE',  ( -1.000000000000000000, 0.000000000000000000, 0.000000000000000000 ) ) ;
#13326 = VERTEX_POINT ( 'NONE', #26980 ) ;
#13327 = DIRECTION ( 'NONE',  ( 0.000000000000000000, 0.000000000000000000, -1.000000000000000000 ) ) ;
#13328 = ORIENTED_EDGE ( 'NONE', *, *, #15451, .T. ) ;
#13329 = CARTESIAN_POINT ( 'NONE',  ( 7.622785526030999570, -23.78712283485999990, 10.47836401506999948 ) ) ;
#13330 = CARTESIAN_POINT ( 'NONE',  ( 7.037082147462999870, -78.32249282818800395, -8.217099986793998667 ) ) ;
#13331 = CARTESIAN_POINT ( 'NONE',  ( 7.995796640821898116, -55.11315380194076141, -7.555116226629998266 ) ) ;
#13332 = CARTESIAN_POINT ( 'NONE',  ( -0.3278092779548479330, -82.49649409683389933, 1.218271132180950511 ) ) ;
#13333 = CARTESIAN_POINT ( 'NONE',  ( -4.898542333728430620, -78.18064372240367277, -7.846565971572500686 ) ) ;
#13334 = CARTESIAN_POINT ( 'NONE',  ( -5.268979267983999293, -78.61222999764899555, 9.902321347348999936 ) ) ;
#13335 = CARTESIAN_POINT ( 'NONE',  ( -0.4565665923329550457, -81.00000000000000000, 10.78468286928460351 ) ) ;
#13336 = ORIENTED_EDGE ( 'NONE', *, *, #37501, .F. ) ;
#13337 = ORIENTED_EDGE ( 'NONE', *, *, #24078, .F. ) ;
#13338 = CARTESIAN_POINT ( 'NONE',  ( 1.272989083314503000, -77.46403964825013588, 9.162259919681792653 ) ) ;
#13339 = CIRCLE ( 'NONE', #33024, 10.14999999999999858 ) ;
#13340 = CARTESIAN_POINT ( 'NONE',  ( 10.74764839381999870, -78.11818400912298443, -0.2248421733643000131 ) ) ;
#13341 =( NAMED_UNIT ( * ) PLANE_ANGLE_UNIT ( ) SI_UNIT ( $, .RADIAN. ) );
#13342 = CIRCLE ( 'NONE', #46388, 0.5000000000000004441 ) ;
#13343 = CARTESIAN_POINT ( 'NONE',  ( 7.658860137760000519, -78.69307375199699095, 5.959242465009999989 ) ) ;
#13344 = CARTESIAN_POINT ( 'NONE',  ( -2.166618510580000212, -76.03018013234999728, -12.78353179556000008 ) ) ;
#13345 = CARTESIAN_POINT ( 'NONE',  ( -8.487831271174274050, -79.43705601822802009, -4.266955699134562074 ) ) ;
#13346 = CARTESIAN_POINT ( 'NONE',  ( 12.76303204525000012, -60.06485147653999945, 1.980584515753000208 ) ) ;
#13347 = CARTESIAN_POINT ( 'NONE',  ( 0.000000000000000000, -75.15999999999999659, 0.000000000000000000 ) ) ;
#13348 = ADVANCED_FACE ( 'NONE', ( #18442 ), #46181, .F. ) ;
#13349 = CARTESIAN_POINT ( 'NONE',  ( -0.9995835529977249445, -78.05208333333330017, -0.7681833999686439318 ) ) ;
#13350 = CARTESIAN_POINT ( 'NONE',  ( -11.03440961815829624, -76.67173248339075542, 4.064493473767709197 ) ) ;
#13351 = CARTESIAN_POINT ( 'NONE',  ( 3.544224594258000405, -82.38975280906599608, -0.05576024114378000385 ) ) ;
#13352 = EDGE_LOOP ( 'NONE', ( #28667, #43197, #9879, #1898 ) ) ;
#13353 = EDGE_CURVE ( 'NONE', #10113, #21051, #44716, .T. ) ;
#13354 = CARTESIAN_POINT ( 'NONE',  ( 12.31128233177999931, -79.68873324023100224, -0.3719124246491999908 ) ) ;
#13355 = CARTESIAN_POINT ( 'NONE',  ( 8.818917551212999584, -75.94225605456199446, 6.571393569026001025 ) ) ;
#13356 = CARTESIAN_POINT ( 'NONE',  ( -6.844313060652878811, -78.03000987509473418, 8.289561653482776293 ) ) ;
#13357 = CARTESIAN_POINT ( 'NONE',  ( 0.9627474882855999727, -78.26529635310198785, -11.94107121277999894 ) ) ;
#13358 = CARTESIAN_POINT ( 'NONE',  ( -10.36221646773000060, -18.77876216379999974, 7.631895822745999425 ) ) ;
#13359 = DIRECTION ( 'NONE',  ( 1.000000000000000000, 0.000000000000000000, 0.000000000000000000 ) ) ;
#13360 = CARTESIAN_POINT ( 'NONE',  ( -17.50000000000000000, -49.87071424677999687, -2.007252870860999804E-13 ) ) ;
#13361 = FACE_OUTER_BOUND ( 'NONE', #56048, .T. ) ;
#13362 = DIRECTION ( 'NONE',  ( 0.000000000000000000, 0.000000000000000000, -1.000000000000000000 ) ) ;
#13363 = CARTESIAN_POINT ( 'NONE',  ( -8.674044796698000326, -76.83844565707200047, 6.768505387188000988 ) ) ;
#13364 = CARTESIAN_POINT ( 'NONE',  ( 11.99999999999999822, -78.06041666666666856, 1.570796326794923203 ) ) ;
#13365 = CARTESIAN_POINT ( 'NONE',  ( 11.00000000000000000, -79.94999999999998863, 0.000000000000000000 ) ) ;
#13366 = VERTEX_POINT ( 'NONE', #17550 ) ;
#13367 = CARTESIAN_POINT ( 'NONE',  ( 3.250000000000000000, -1.350000000000000089, 0.000000000000000000 ) ) ;
#13368 = CARTESIAN_POINT ( 'NONE',  ( 2.019183793707000074, -55.01279722724000010, 12.79944116701999768 ) ) ;
#13369 = CARTESIAN_POINT ( 'NONE',  ( 0.000000000000000000, -82.50000000000000000, 0.000000000000000000 ) ) ;
#13370 = EDGE_CURVE ( 'NONE', #11254, #43096, #4567, .T. ) ;
#13371 = CARTESIAN_POINT ( 'NONE',  ( 1.478503027591000052, -2.061791850768999623, 3.507110283440000309 ) ) ;
#13372 = B_SPLINE_CURVE_WITH_KNOTS ( 'NONE', 3,
 ( #29356, #47403, #56822, #21373, #38803, #48268, #30515, #20798, #34360, #2514, #26087, #48544, #56245, #20231, #29928, #16669, #47977, #7224 ),
 .UNSPECIFIED., .F., .F.,
 ( 4, 2, 2, 2, 2, 2, 2, 2, 4 ),
 ( 0.000000000000000000, 0.1250000000000000000, 0.2500000000000000000, 0.3750000000000000000, 0.5000000000000000000, 0.6250000000000000000, 0.7500000000000000000, 0.8750000000000000000, 1.000000000000000000 ),
 .UNSPECIFIED. ) ;
#13373 = CARTESIAN_POINT ( 'NONE',  ( -10.17713110909000029, -76.66378392136499542, 4.716330562529999604 ) ) ;
#13374 = DIRECTION ( 'NONE',  ( 0.000000000000000000, 0.000000000000000000, -1.000000000000000000 ) ) ;
#13375 = CARTESIAN_POINT ( 'NONE',  ( -3.399186938124999724, -77.19999999999998863, -10.46162167925000119 ) ) ;
#13376 = CARTESIAN_POINT ( 'NONE',  ( -1.801614160555000010, -60.18652261871999798, 12.59687422890000086 ) ) ;
#13377 = DIRECTION ( 'NONE',  ( 0.9999999999995751176, 0.000000000000000000, 9.217549102787771002E-07 ) ) ;
#13378 = CARTESIAN_POINT ( 'NONE',  ( 4.171964897155000074, -82.43369503318800184, -0.06563908455728000024 ) ) ;
#13379 = FACE_OUTER_BOUND ( 'NONE', #27190, .T. ) ;
#13380 = CARTESIAN_POINT ( 'NONE',  ( 10.05509635955887582, -76.74978642219571157, 6.690173733955245616 ) ) ;
#13381 = CARTESIAN_POINT ( 'NONE',  ( 9.549799293660999666, -79.45431405828000493, -7.133803361836999812 ) ) ;
#13382 = CARTESIAN_POINT ( 'NONE',  ( -10.11369910513000114, -76.67433028348600033, 4.686934626122000402 ) ) ;
#13383 = CARTESIAN_POINT ( 'NONE',  ( -12.79999999971638225, -2.899999999995986233, -2.660989632711285603E-09 ) ) ;
#13384 = CARTESIAN_POINT ( 'NONE',  ( 1.002166123569000034, -79.27011357725000096, 1.026519443915999918 ) ) ;
#13385 = CARTESIAN_POINT ( 'NONE',  ( 9.208615812369000508, -77.16518630590849170, 2.957800710608999850 ) ) ;
#13386 = DIRECTION ( 'NONE',  ( 0.000000000000000000, 0.000000000000000000, 1.000000000000000000 ) ) ;
#13387 = AXIS2_PLACEMENT_3D ( 'NONE', #39131, #57433, #56284 ) ;
#13388 = FACE_OUTER_BOUND ( 'NONE', #4325, .T. ) ;
#13389 = CARTESIAN_POINT ( 'NONE',  ( 0.7641671376257024306, -80.23108036345902860, -10.72413782510657931 ) ) ;
#13390 = CARTESIAN_POINT ( 'NONE',  ( -12.52785920744742043, -23.79405666946010456, -1.668536824485600256 ) ) ;
#13391 = CARTESIAN_POINT ( 'NONE',  ( -0.2213420416186210049, -77.76131037297035675, -1.254942581273592817 ) ) ;
#13392 = CARTESIAN_POINT ( 'NONE',  ( 12.55432891850757748, -55.41272687720891099, -1.749897736046111651 ) ) ;
#13393 = LINE ( 'NONE', #31394, #17922 ) ;
#13394 = CARTESIAN_POINT ( 'NONE',  ( -0.6454797250855089930, -61.68806512111238760, 12.50471521371613726 ) ) ;
#13395 = CARTESIAN_POINT ( 'NONE',  ( 10.05750832943000006, -79.67661227141499580, 4.806363154649000435 ) ) ;
#13396 = LINE ( 'NONE', #57987, #47907 ) ;
#13397 = VERTEX_POINT ( 'NONE', #4863 ) ;
#13398 = ORIENTED_EDGE ( 'NONE', *, *, #8970, .T. ) ;
#13399 = CARTESIAN_POINT ( 'NONE',  ( -1.499999999985999866, -82.00000000001401190, -1.019196462549000076E-10 ) ) ;
#13400 = B_SPLINE_CURVE_WITH_KNOTS ( 'NONE', 3,
 ( #10907, #51347, #51060, #41600, #50768, #28881, #19169, #24470 ),
 .UNSPECIFIED., .F., .F.,
 ( 4, 1, 1, 1, 1, 4 ),
 ( 0.000000000000000000, 0.1999938512431460313, 0.3999979371066214595, 0.6000020229700968599, 0.8000061088335723714, 1.000000000000000000 ),
 .UNSPECIFIED. ) ;
#13401 = VERTEX_POINT ( 'NONE', #31405 ) ;
#13402 = FILL_AREA_STYLE ('',( #39409 ) ) ;
#13404 = ADVANCED_FACE ( 'NONE', ( #13703 ), #1842, .T. ) ;
#13403 = ORIENTED_EDGE ( 'NONE', *, *, #31084, .T. ) ;
#13405 = CARTESIAN_POINT ( 'NONE',  ( -1.576170184333999913, -17.83913032783999952, 12.55466896104999996 ) ) ;
#13406 = AXIS2_PLACEMENT_3D ( 'NONE', #47417, #42971, #1664 ) ;
#13407 = DIRECTION ( 'NONE',  ( 0.000000000000000000, 0.1122098755727947705, 0.9936845293270585300 ) ) ;
#13408 = FACE_OUTER_BOUND ( 'NONE', #5157, .T. ) ;
#13409 = CARTESIAN_POINT ( 'NONE',  ( 5.530078818784999406, -79.80792107344059616, -9.545677681241999224 ) ) ;
#13410 = CARTESIAN_POINT ( 'NONE',  ( -2.689975106962999796, -82.06107264098699261, -2.376505205460000436 ) ) ;
#13411 = CARTESIAN_POINT ( 'NONE',  ( -3.597607681491937992, -79.30558875575349020, 8.792251918324103244 ) ) ;
#13412 = ORIENTED_EDGE ( 'NONE', *, *, #24328, .F. ) ;
#13413 = LINE ( 'NONE', #8405, #46978 ) ;
#13414 = CARTESIAN_POINT ( 'NONE',  ( -1.769904851686999958, -78.80511624945999927, 12.08118746087999895 ) ) ;
#13415 = ORIENTED_EDGE ( 'NONE', *, *, #42011, .T. ) ;
#13416 = ORIENTED_EDGE ( 'NONE', *, *, #2631, .F. ) ;
#13417 = CARTESIAN_POINT ( 'NONE',  ( -2.653227710365042125, -77.00733822163999776, -11.74665041585868153 ) ) ;
#13418 = CARTESIAN_POINT ( 'NONE',  ( 0.5765222740522000233, -80.10508703656800833, 1.202579817323000233 ) ) ;
#13419 = CARTESIAN_POINT ( 'NONE',  ( 5.091895231007000255, -78.54058880411299981, 8.260951054388000259 ) ) ;
#13420 = CARTESIAN_POINT ( 'NONE',  ( -1.661313768260602286, -86.09999999999976694, -3.638686103992718746 ) ) ;
#13421 = CARTESIAN_POINT ( 'NONE',  ( 3.626474550257886342, -85.80798832763333905, 1.029710946748257916 ) ) ;
#13422 = CARTESIAN_POINT ( 'NONE',  ( -12.76493461869000079, -77.83724936260999527, -0.9303755367166000045 ) ) ;
#13423 = CARTESIAN_POINT ( 'NONE',  ( 0.5308835263170998964, -80.92289485077999700, 1.242631599581000001 ) ) ;
#13424 = DIRECTION ( 'NONE',  ( 0.000000000000000000, 0.000000000000000000, -1.000000000000000000 ) ) ;
#13425 = DIRECTION ( 'NONE',  ( 0.000000000000000000, 1.000000000000000000, 0.000000000000000000 ) ) ;
#13426 = CARTESIAN_POINT ( 'NONE',  ( 9.489539964980000519, -77.25051167140100006, -0.7618433214053000890 ) ) ;
#13427 = ADVANCED_FACE ( 'NONE', ( #27565 ), #31698, .T. ) ;
#13428 = CARTESIAN_POINT ( 'NONE',  ( -1.492427764749000074, -79.17506245343760440, -3.851117465929000172 ) ) ;
#13429 = AXIS2_PLACEMENT_3D ( 'NONE', #38410, #47302, #24840 ) ;
#13430 = CARTESIAN_POINT ( 'NONE',  ( 11.68767212001977995, -76.57083333333332575, 3.140974612311385972 ) ) ;
#13431 = CARTESIAN_POINT ( 'NONE',  ( 2.999869787185454495, -2.882451689260415506, 1.248622406629191106 ) ) ;
#13432 = CARTESIAN_POINT ( 'NONE',  ( 2.184293099093999935, -82.17700264934799748, -2.791770796765000284 ) ) ;
#13433 = CARTESIAN_POINT ( 'NONE',  ( 0.000000000000000000, -74.64999999999999147, 0.000000000000000000 ) ) ;
#13434 = CARTESIAN_POINT ( 'NONE',  ( 1.328862289696999932, -80.26727390273069318, 11.18676134159000135 ) ) ;
#13435 = CARTESIAN_POINT ( 'NONE',  ( -3.750250575282000121, -2.234355802843000394, 0.6493866540274000343 ) ) ;
#13436 = CARTESIAN_POINT ( 'NONE',  ( 0.09626986684956309603, -79.88099558508119458, -1.271715491304152401 ) ) ;
#13437 = ORIENTED_EDGE ( 'NONE', *, *, #54768, .T. ) ;
#13438 = FACE_OUTER_BOUND ( 'NONE', #17389, .T. ) ;
#13439 = AXIS2_PLACEMENT_3D ( 'NONE', #49256, #4684, #40695 ) ;
#13440 = CARTESIAN_POINT ( 'NONE',  ( 9.611650271896843734, -79.40833333333331723, -5.539808784079876425 ) ) ;
#13441 = EDGE_CURVE ( 'NONE', #41589, #15410, #36432, .T. ) ;
#13442 = CARTESIAN_POINT ( 'NONE',  ( 1.193978368322000216, -81.89136962295700073, -0.5941311122250999555 ) ) ;
#13444 = EDGE_CURVE ( 'NONE', #28960, #29374, #2796, .T. ) ;
#13443 = CARTESIAN_POINT ( 'NONE',  ( -12.49830607528000037, -18.79028586434999681, -1.666977523253999838 ) ) ;
#13445 = CARTESIAN_POINT ( 'NONE',  ( 11.79660191402999914, -76.76735435298000709, 5.494707494196000575 ) ) ;
#13446 = CIRCLE ( 'NONE', #45544, 12.90000000000000036 ) ;
#13447 = CARTESIAN_POINT ( 'NONE',  ( -9.689272046837857033, -61.77888144139958371, -8.274769670276990396 ) ) ;
#13448 = CARTESIAN_POINT ( 'NONE',  ( 12.53241208773999915, -22.76462890193000277, -1.667936697358999965 ) ) ;
#13449 = B_SPLINE_CURVE_WITH_KNOTS ( 'NONE', 3,
 ( #28249, #18837, #46304, #23834, #49553, #45126, #4677, #22676, #40687, #19710, #2580, #43023, #56308, #43308, #33562, #29707, #37708, #24130 ),
 .UNSPECIFIED., .F., .F.,
 ( 4, 2, 2, 2, 2, 2, 2, 2, 4 ),
 ( 0.000000000000000000, 0.1250000000000000000, 0.2500000000000000000, 0.3750000000000000000, 0.5000000000000000000, 0.6250000000000000000, 0.7500000000000000000, 0.8750000000000000000, 1.000000000000000000 ),
 .UNSPECIFIED. ) ;
#13450 = ORIENTED_EDGE ( 'NONE', *, *, #25850, .T. ) ;
#13451 = VECTOR ( 'NONE', #12514, 1000.000000000000000 ) ;
#13452 = SHAPE_REPRESENTATION ( 'Battery', ( #43526 ), #49207 ) ;
#13453 = CARTESIAN_POINT ( 'NONE',  ( -8.130434485062000505, -77.24008885281497783, -7.810376049085999917 ) ) ;
#13454 = CARTESIAN_POINT ( 'NONE',  ( -1.404978054315000113, -81.29170789458800073, 0.09914529170176999973 ) ) ;
#13455 = CARTESIAN_POINT ( 'NONE',  ( 3.140974612311376646, -79.04583333333333428, -11.68767212001978706 ) ) ;
#13456 = CARTESIAN_POINT ( 'NONE',  ( 7.653824198668000456, -79.22136658247099206, -5.479973919995999587 ) ) ;
#13458 = CARTESIAN_POINT ( 'NONE',  ( -3.431352783032999731, -1.273849349033000067, 2.086989923523999924 ) ) ;
#13457 = CARTESIAN_POINT ( 'NONE',  ( -3.905352855690000347, -86.07743221058099437, 1.102748417664999980 ) ) ;
#13459 = LINE ( 'NONE', #13159, #27468 ) ;
#13460 = CARTESIAN_POINT ( 'NONE',  ( 1.209428572278999914, -79.39637299687198890, 0.7398254253092000354 ) ) ;
#13461 = ORIENTED_EDGE ( 'NONE', *, *, #48543, .F. ) ;
#13462 = CARTESIAN_POINT ( 'NONE',  ( 4.066926578147327831, -77.25590895697494886, -9.998169505304765892 ) ) ;
#13463 = CARTESIAN_POINT ( 'NONE',  ( 1.199500263597271577, -79.09791666666667709, -0.9218200799623702535 ) ) ;
#13464 = ADVANCED_FACE ( 'NONE', ( #15161 ), #33157, .F. ) ;
#13465 = ORIENTED_EDGE ( 'NONE', *, *, #18652, .T. ) ;
#13466 = EDGE_LOOP ( 'NONE', ( #51702, #29797, #6734, #30595 ) ) ;
#13467 = CARTESIAN_POINT ( 'NONE',  ( -8.850953919802000414, -79.76088734065699271, -8.146641040006999290 ) ) ;
#13468 = CYLINDRICAL_SURFACE ( 'NONE', #15261, 9.599999999999999645 ) ;
#13469 = ORIENTED_EDGE ( 'NONE', *, *, #27416, .F. ) ;
#13470 = CARTESIAN_POINT ( 'NONE',  ( 11.90740810048999876, -78.87878573459099130, 0.8057021066547999100 ) ) ;
#13471 = CIRCLE ( 'NONE', #38923, 1.000000000000000000 ) ;
#13472 = ORIENTED_EDGE ( 'NONE', *, *, #57938, .T. ) ;
#13474 = EDGE_CURVE ( 'NONE', #21405, #23950, #28732, .T. ) ;
#13473 = ORIENTED_EDGE ( 'NONE', *, *, #31603, .F. ) ;
#13475 = CARTESIAN_POINT ( 'NONE',  ( -2.152895537798944048, -2.668002774646853759, -2.435455713980514858 ) ) ;
#13476 = EDGE_CURVE ( 'NONE', #21051, #28446, #49919, .T. ) ;
#13477 = CONICAL_SURFACE ( 'NONE', #49316, 0.6999999997695030007, 0.7853981633972997312 ) ;
#13478 = CARTESIAN_POINT ( 'NONE',  ( -1.500000000000000000, -83.34999999999999432, 0.000000000000000000 ) ) ;
#13479 = CARTESIAN_POINT ( 'NONE',  ( -5.809791519574999619, -79.67570697846352346, 7.851562197947999699 ) ) ;
#13480 = B_SPLINE_SURFACE_WITH_KNOTS ( 'NONE', 3, 3, ( 
 ( #37169, #6460, #33889, #46933, #37457, #33607, #51930, #24473, #42487, #38329, #51649 ),
 ( #28295, #46641, #19173, #15904, #1763, #11489, #51351, #14723, #51064, #32720, #11200 ),
 ( #24178, #56352, #24765, #2057, #1471, #19757, #29177, #15023, #29462, #37754, #41897 ),
 ( #47224, #15323, #5578, #20058, #23589, #10910, #6755, #41603, #1183, #55181, #50772 ) ),
 .UNSPECIFIED., .F., .F., .F.,
 ( 4, 4 ),
 ( 4, 1, 1, 1, 1, 1, 1, 1, 4 ),
 ( 0.1070361703151999910, 1.138757407831999968 ),
 ( -0.003449459057608000173, 0.01897202481685000136, 0.04139350869129999888, 0.06381499256575000334, 0.08623647644019999392, 0.1086579603147000000, 0.1310794441891000028, 0.1535009280635999951, 0.1759224119379999840 ),
 .UNSPECIFIED. ) ;
#13481 = ORIENTED_EDGE ( 'NONE', *, *, #50184, .F. ) ;
#13482 = CARTESIAN_POINT ( 'NONE',  ( 1.310737403901690357, -81.69186661536872407, 0.7553186815146348820 ) ) ;
#13483 = B_SPLINE_CURVE_WITH_KNOTS ( 'NONE', 3,
 ( #30900, #22651, #40363, #49528, #13780, #18237, #9074, #32075, #23235, #9370, #9660, #54822, #22049, #49226, #35623, #53651, #36224, #58372 ),
 .UNSPECIFIED., .F., .F.,
 ( 4, 2, 2, 2, 2, 2, 2, 2, 4 ),
 ( 0.000000000000000000, 0.1250000000000000833, 0.2500000000000001665, 0.3750000000000001110, 0.5000000000000001110, 0.6250000000000001110, 0.7500000000000000000, 0.8750000000000000000, 1.000000000000000000 ),
 .UNSPECIFIED. ) ;
#13484 = ORIENTED_EDGE ( 'NONE', *, *, #36548, .F. ) ;
#13485 = CARTESIAN_POINT ( 'NONE',  ( -0.6450463279315846732, -80.06702524164226986, 1.098828897408985261 ) ) ;
#13486 = CARTESIAN_POINT ( 'NONE',  ( -3.999289396771957605, -78.69999999999997442, 0.07539443523754388310 ) ) ;
#13487 = VECTOR ( 'NONE', #27324, 1000.000000000000000 ) ;
#13488 = CARTESIAN_POINT ( 'NONE',  ( 10.35410226329999794, -55.39601732791000188, 7.619716344056000068 ) ) ;
#13489 = CARTESIAN_POINT ( 'NONE',  ( -5.052420809101000088E-14, -80.84999999994218456, 0.000000000000000000 ) ) ;
#13490 = LINE ( 'NONE', #41826, #56013 ) ;
#13491 = LINE ( 'NONE', #14080, #36494 ) ;
#13492 = CARTESIAN_POINT ( 'NONE',  ( 9.148490208346998998, -77.95585066807355190, 7.734416031130999514 ) ) ;
#13493 = B_SPLINE_CURVE_WITH_KNOTS ( 'NONE', 3,
 ( #20001, #20572, #28829, #52165 ),
 .UNSPECIFIED., .F., .F.,
 ( 4, 4 ),
 ( 0.000000000000000000, 1.000000000000000000 ),
 .UNSPECIFIED. ) ;
#13494 = CARTESIAN_POINT ( 'NONE',  ( 3.246408215754346127, -78.75374379457647933, -8.682844942750486794 ) ) ;
#13495 = CARTESIAN_POINT ( 'NONE',  ( -10.31986335554000078, -24.28918510737999981, 7.753844818030001029 ) ) ;
#13496 = CARTESIAN_POINT ( 'NONE',  ( 8.796335266379966100, -78.40208333333335133, 6.760013919724084275 ) ) ;
#13497 = CARTESIAN_POINT ( 'NONE',  ( 4.116270392846000270, -80.92330496681199747, -0.6829204583257999506 ) ) ;
#13498 = CARTESIAN_POINT ( 'NONE',  ( 4.201099985035000373, -77.91728667140098707, -8.812540045011001411 ) ) ;
#13499 = CARTESIAN_POINT ( 'NONE',  ( -12.49837451347000084, -18.79042109296999641, 1.667049596275999912 ) ) ;
#13500 = CARTESIAN_POINT ( 'NONE',  ( 12.80090744918999945, -22.76232687447999936, -1.980532734072999901 ) ) ;
#13501 = CARTESIAN_POINT ( 'NONE',  ( 1.669849926071999890, -23.37228600417000024, 12.48404299553000030 ) ) ;
#13502 = CARTESIAN_POINT ( 'NONE',  ( -1.842497806997728027, -79.98834702216801418, 10.91026042240053862 ) ) ;
#13503 = CARTESIAN_POINT ( 'NONE',  ( -0.3558927676304953214, -79.99999999999994316, 9.287066994265805064 ) ) ;
#13504 = CARTESIAN_POINT ( 'NONE',  ( -3.698639260106999949, -1.410322672877000194, -1.403610537410000081 ) ) ;
#13505 = CARTESIAN_POINT ( 'NONE',  ( -3.518954327950687855, -78.19866318821630102, -10.19196483504709505 ) ) ;
#13506 = ADVANCED_FACE ( 'NONE', ( #50323 ), #9873, .F. ) ;
#13507 = CARTESIAN_POINT ( 'NONE',  ( -1.404188869873914003, -80.81895558338473506, 0.5634542928392101135 ) ) ;
#13508 = CARTESIAN_POINT ( 'NONE',  ( -1.163246785803522698, -78.56960608111629085, 0.4728783135193991849 ) ) ;
#13509 = CARTESIAN_POINT ( 'NONE',  ( 0.3299670982549000042, -79.26668014110398985, 1.580613947285000043 ) ) ;
#13510 = DIRECTION ( 'NONE',  ( 0.000000000000000000, -1.000000000000000000, 0.000000000000000000 ) ) ;
#13511 = ADVANCED_FACE ( 'NONE', ( #50905 ), #41452, .T. ) ;
#13512 = CARTESIAN_POINT ( 'NONE',  ( -9.731251526955000841, -77.56402055093700199, -4.947535720883000643 ) ) ;
#13513 = CARTESIAN_POINT ( 'NONE',  ( 10.58601714202000110, -77.15014181984899722, -5.993221192758000804 ) ) ;
#13514 = DIRECTION ( 'NONE',  ( -0.9999433559010179051, 0.000000000000000000, -0.01064354214585019887 ) ) ;
#13516 = CARTESIAN_POINT ( 'NONE',  ( 1.398095685538000010, -78.56058528507598737, 0.2353462009024000212 ) ) ;
#13515 = CARTESIAN_POINT ( 'NONE',  ( -1.199500263597274241, -79.84791666666664867, 0.9218200799623669228 ) ) ;
#13517 = CARTESIAN_POINT ( 'NONE',  ( -0.8956573524961000121, -81.35090657403999614, -1.447939571232000011 ) ) ;
#13518 = ORIENTED_EDGE ( 'NONE', *, *, #49057, .T. ) ;
#13519 = CARTESIAN_POINT ( 'NONE',  ( 2.619126064213000316, -84.31807450217398525, 2.454366755733000005 ) ) ;
#13520 = AXIS2_PLACEMENT_3D ( 'NONE', #26782, #18249, #36240 ) ;
#13521 = CARTESIAN_POINT ( 'NONE',  ( -1.250000000000000000, -77.75000000000000000, 0.000000000000000000 ) ) ;
#13522 = CARTESIAN_POINT ( 'NONE',  ( 5.035646364706000355, -79.91077779019330762, 9.842428139517000574 ) ) ;
#13523 = DIRECTION ( 'NONE',  ( 0.7071067811865474617, 0.000000000000000000, 0.7071067811865474617 ) ) ;
#13524 = CARTESIAN_POINT ( 'NONE',  ( 1.460959015002474048, -81.72916666666669983, -0.3926218265389178064 ) ) ;
#13525 = CARTESIAN_POINT ( 'NONE',  ( -10.31986335556999990, -61.08918510704999960, 7.753844818055000587 ) ) ;
#13526 = CARTESIAN_POINT ( 'NONE',  ( 7.686826547751000938, -78.63180575231598368, 5.981002702827999506 ) ) ;
#13527 = CARTESIAN_POINT ( 'NONE',  ( -1.321087349134000055, -1.707219782537999997, 3.804044948481000166 ) ) ;
#13528 = CARTESIAN_POINT ( 'NONE',  ( 5.902036703393280348, -79.79999999999999716, -10.23561245371837103 ) ) ;
#13529 = CARTESIAN_POINT ( 'NONE',  ( 12.70926857199000004, -23.40841990708999987, -1.933876778424000076 ) ) ;
#13530 = CARTESIAN_POINT ( 'NONE',  ( -1.931087888240000217, -60.11584731951999316, 12.71658872087999903 ) ) ;
#13531 = ORIENTED_EDGE ( 'NONE', *, *, #19550, .T. ) ;
#13532 = VECTOR ( 'NONE', #31576, 1000.000000000000114 ) ;
#13533 = DIRECTION ( 'NONE',  ( 1.000000000000000000, 0.000000000000000000, 0.000000000000000000 ) ) ;
#13534 = CARTESIAN_POINT ( 'NONE',  ( 12.50240633877000107, -17.31762602171999887, 1.005381409788000058 ) ) ;
#13535 = EDGE_CURVE ( 'NONE', #15743, #20349, #42336, .T. ) ;
#13536 = DIRECTION ( 'NONE',  ( 0.000000000000000000, 1.000000000000000000, 0.000000000000000000 ) ) ;
#13537 = CIRCLE ( 'NONE', #26720, 3.799999999999999822 ) ;
#13538 = CARTESIAN_POINT ( 'NONE',  ( 0.7554284705563509839, -81.56666666666669130, -1.310679582531386167 ) ) ;
#13539 = EDGE_CURVE ( 'NONE', #49809, #9708, #32859, .T. ) ;
#13540 = CARTESIAN_POINT ( 'NONE',  ( -0.8033051684372000123, -80.47378378841000313, -1.459438184619000101 ) ) ;
#13541 = CARTESIAN_POINT ( 'NONE',  ( 10.98384481689545389, -23.22882187213949123, 0.5959944459582935394 ) ) ;
#13542 = ORIENTED_EDGE ( 'NONE', *, *, #2689, .F. ) ;
#13543 = CARTESIAN_POINT ( 'NONE',  ( 7.847929611857001220, -77.11666530948868115, -7.852092130568000705 ) ) ;
#13544 = CARTESIAN_POINT ( 'NONE',  ( -3.783546124412332290, -77.79732454329705149, -11.14641671793737210 ) ) ;
#13545 = CARTESIAN_POINT ( 'NONE',  ( -7.000000000000000000, -81.19999999999998863, -1.000000000000000000 ) ) ;
#13546 = ORIENTED_EDGE ( 'NONE', *, *, #48168, .T. ) ;
#13547 = ORIENTED_EDGE ( 'NONE', *, *, #6138, .F. ) ;
#13548 = CARTESIAN_POINT ( 'NONE',  ( -9.966229686695001533, -55.13098097352000337, -7.657726530227999540 ) ) ;
#13549 = ADVANCED_FACE ( 'NONE', ( #1037 ), #28440, .F. ) ;
#13550 = CARTESIAN_POINT ( 'NONE',  ( -4.465297566879000257, -79.74293539630998850, 8.686876450551999085 ) ) ;
#13551 = ORIENTED_EDGE ( 'NONE', *, *, #34135, .T. ) ;
#13552 = CARTESIAN_POINT ( 'NONE',  ( 7.186413748181999850, -76.51672644249900657, 10.04705466018000060 ) ) ;
#13553 = CARTESIAN_POINT ( 'NONE',  ( -9.576266473187072137, -78.63770102887031044, -4.884198570897098080 ) ) ;
#13554 = CARTESIAN_POINT ( 'NONE',  ( 1.486116868684999925, -77.93655061187999422, -0.3837144090195000468 ) ) ;
#13555 = ORIENTED_EDGE ( 'NONE', *, *, #22813, .T. ) ;
#13556 = CARTESIAN_POINT ( 'NONE',  ( 1.009320482739999969, -77.43647305011499782, 9.441330439200999791 ) ) ;
#13557 = CARTESIAN_POINT ( 'NONE',  ( 0.9273595869657466073, -80.29200840023126773, -0.8380822826822911242 ) ) ;
#13558 = CARTESIAN_POINT ( 'NONE',  ( -3.299302781710000243, -77.38961746229999505, 12.69174137596000129 ) ) ;
#13559 = CARTESIAN_POINT ( 'NONE',  ( 2.187315676234173889, -78.39085115783234414, -10.82293057966254146 ) ) ;
#13560 = CARTESIAN_POINT ( 'NONE',  ( -3.210317642309942432, -86.31452042059399332, 1.357411296278473678 ) ) ;
#13561 = AXIS2_PLACEMENT_3D ( 'NONE', #29211, #2940, #11522 ) ;
#13562 = CARTESIAN_POINT ( 'NONE',  ( 2.260091721765999928, -78.89370578835476522, -9.437303113984999214 ) ) ;
#13563 = EDGE_CURVE ( 'NONE', #15817, #54320, #40553, .T. ) ;
#13564 = CARTESIAN_POINT ( 'NONE',  ( 6.989933869880151640, -79.90691905236667480, 6.058301176545876743 ) ) ;
#13565 = CARTESIAN_POINT ( 'NONE',  ( -9.497876546326999403, -77.25168256874098915, -0.2008509664869000122 ) ) ;
#13566 = ORIENTED_EDGE ( 'NONE', *, *, #22014, .F. ) ;
#13567 = CARTESIAN_POINT ( 'NONE',  ( -9.497876546326999403, -77.35168256874098347, -0.2008509664869000122 ) ) ;
#13568 = CARTESIAN_POINT ( 'NONE',  ( -10.77133038182000035, -76.59221396288000960, -5.959359258312999508 ) ) ;
#13569 = CARTESIAN_POINT ( 'NONE',  ( 1.130428667122000075, -80.59477190545899816, -1.152972209120999958 ) ) ;
#13570 = CARTESIAN_POINT ( 'NONE',  ( 0.000000000000000000, -80.99999999999998579, -8.199999999999970868 ) ) ;
#13571 = CARTESIAN_POINT ( 'NONE',  ( -2.416613568816377011, -3.414010557351236486, -2.560321170370766009 ) ) ;
#13572 = CARTESIAN_POINT ( 'NONE',  ( 12.50483450296212773, -53.93545441819600939, -0.6958183767277665854 ) ) ;
#13573 = CARTESIAN_POINT ( 'NONE',  ( -1.984586691443999795, -76.09012359603299558, 11.75553522549000007 ) ) ;
#13574 = CARTESIAN_POINT ( 'NONE',  ( -8.251802458177941446, -61.60055625090545561, -9.431055091043617722 ) ) ;
#13575 = CARTESIAN_POINT ( 'NONE',  ( -9.625876801520000470, -77.44121332859899098, 0.2298721198045000080 ) ) ;
#13576 = CARTESIAN_POINT ( 'NONE',  ( -11.80802719753318719, -77.03357931642592860, 2.478256143328310124 ) ) ;
#13577 = CARTESIAN_POINT ( 'NONE',  ( 10.89876807034000095, -79.48100350178651752, -2.652350870517000025 ) ) ;
#13578 = DIRECTION ( 'NONE',  ( 0.7071067811865475727, 0.000000000000000000, 0.7071067811865475727 ) ) ;
#13579 = VERTEX_POINT ( 'NONE', #15464 ) ;
#13580 = CARTESIAN_POINT ( 'NONE',  ( 1.503815466746999840, -82.16902456270999267, 0.5029271919957000181 ) ) ;
#13581 = CARTESIAN_POINT ( 'NONE',  ( -1.250000000000000000, -82.59999999999999432, 0.000000000000000000 ) ) ;
#13582 = CARTESIAN_POINT ( 'NONE',  ( 1.750000000000000000, -18.75000000240999753, -12.50000000000000000 ) ) ;
#13583 = CARTESIAN_POINT ( 'NONE',  ( -10.07627163191000008, -23.24999999758999536, -7.601397897754999633 ) ) ;
#13584 = CARTESIAN_POINT ( 'NONE',  ( 1.250000000000000000, -81.74999999999998579, 0.000000000000000000 ) ) ;
#13585 = DIRECTION ( 'NONE',  ( 0.000000000000000000, 1.000000000000000000, 0.000000000000000000 ) ) ;
#13586 = FACE_OUTER_BOUND ( 'NONE', #13308, .T. ) ;
#13587 = CARTESIAN_POINT ( 'NONE',  ( 7.775008698615757829, -76.01703051611190176, 8.841530247503397888 ) ) ;
#13588 = CARTESIAN_POINT ( 'NONE',  ( 8.586577278446998918, -80.32955691727549663, 6.741381070085999738 ) ) ;
#13589 = FACE_OUTER_BOUND ( 'NONE', #26874, .T. ) ;
#13590 = ORIENTED_EDGE ( 'NONE', *, *, #36608, .T. ) ;
#13591 = CARTESIAN_POINT ( 'NONE',  ( -7.541360678298865139, -78.24750000000000227, 5.846326858574210306 ) ) ;
#13592 = CARTESIAN_POINT ( 'NONE',  ( -9.844172144369998989, -75.99875169021464671, 7.391061701651998384 ) ) ;
#13593 = CIRCLE ( 'NONE', #23962, 9.000000000000000000 ) ;
#13594 = CARTESIAN_POINT ( 'NONE',  ( 3.437187628289001040, -78.54828564506388489, -1.267161289092433307E-15 ) ) ;
#13595 = CARTESIAN_POINT ( 'NONE',  ( 13.99936781018472232, -9.295797029142999435, 0.1330447863085613691 ) ) ;
#13596 = CARTESIAN_POINT ( 'NONE',  ( -5.755176823513999729, -78.34907535878998885, 9.345691860246999383 ) ) ;
#13597 = DIRECTION ( 'NONE',  ( -0.9999548435846228323, 0.000000000000000000, -0.009503199022040218977 ) ) ;
#13598 = CARTESIAN_POINT ( 'NONE',  ( 12.50745077490000057, -17.00005551713000074, -2.011911479242000131E-09 ) ) ;
#13599 = DIRECTION ( 'NONE',  ( 1.000000000000000000, 0.000000000000000000, 0.000000000000000000 ) ) ;
#13600 = CYLINDRICAL_SURFACE ( 'NONE', #20168, 14.00000000000000000 ) ;
#13601 = EDGE_LOOP ( 'NONE', ( #22498, #25672, #40788 ) ) ;
#13602 = CIRCLE ( 'NONE', #4173, 0.5000000000000006661 ) ;
#13603 = CARTESIAN_POINT ( 'NONE',  ( -8.415968974905998934, -79.83442983025919659, -7.483677623529000122 ) ) ;
#13604 = DIRECTION ( 'NONE',  ( -0.7071067811865969777, -0.7071067811864980568, 1.359270614438996183E-10 ) ) ;
#13605 = DIRECTION ( 'NONE',  ( 0.000000000000000000, -1.000000000000000000, 0.000000000000000000 ) ) ;
#13606 = CARTESIAN_POINT ( 'NONE',  ( 3.851650068367001190, -78.43735716284257364, 2.273141292805247904 ) ) ;
#13607 = EDGE_CURVE ( 'NONE', #55326, #12605, #30986, .T. ) ;
#13609 = CARTESIAN_POINT ( 'NONE',  ( -0.6943029181025289764, -81.52241017303003900, 1.039652336598162696 ) ) ;
#13608 = AXIS2_PLACEMENT_3D ( 'NONE', #32712, #32423, #32134 ) ;
#13610 = B_SPLINE_CURVE_WITH_KNOTS ( 'NONE', 3,
 ( #41990, #28685, #33408, #51446, #10998, #47023, #42579, #20144, #15703, #21575 ),
 .UNSPECIFIED., .F., .F.,
 ( 4, 2, 2, 2, 4 ),
 ( 0.000000000000000000, 0.2500000000000000000, 0.5000000000000000000, 0.7500000000000000000, 1.000000000000000000 ),
 .UNSPECIFIED. ) ;
#13611 = CARTESIAN_POINT ( 'NONE',  ( 0.1312417595986999919, -79.11712607287400090, 11.15680847095000061 ) ) ;
#13612 = CARTESIAN_POINT ( 'NONE',  ( -1.818468715484000065E-14, -79.21250000010999770, 0.000000000000000000 ) ) ;
#13613 = CARTESIAN_POINT ( 'NONE',  ( 8.768124086712999699, -55.64999999965999677, 7.919595949288999570 ) ) ;
#13614 = DIRECTION ( 'NONE',  ( 0.000000000000000000, 0.000000000000000000, -1.000000000000000000 ) ) ;
#13615 = CARTESIAN_POINT ( 'NONE',  ( 1.407171709420391936, -78.36458333333330017, 10.75000000000000178 ) ) ;
#13616 = ADVANCED_FACE ( 'NONE', ( #15748 ), #33911, .T. ) ;
#13617 = ORIENTED_EDGE ( 'NONE', *, *, #6832, .F. ) ;
#13618 = ORIENTED_EDGE ( 'NONE', *, *, #49087, .F. ) ;
#13619 = DIRECTION ( 'NONE',  ( -0.7071067811865475727, 0.000000000000000000, 0.7071067811865475727 ) ) ;
#13620 = CARTESIAN_POINT ( 'NONE',  ( -4.321547818559999143, -77.71693998579799256, -8.507928659197000698 ) ) ;
#13621 = ORIENTED_EDGE ( 'NONE', *, *, #10858, .T. ) ;
#13622 = CARTESIAN_POINT ( 'NONE',  ( -7.601397897754999633, -18.75000000000000000, 9.369164850722000892 ) ) ;
#13623 = VERTEX_POINT ( 'NONE', #50616 ) ;
#13624 = CARTESIAN_POINT ( 'NONE',  ( 7.634438871657000192, -23.74781730700000182, 10.30764054782999928 ) ) ;
#13625 = CARTESIAN_POINT ( 'NONE',  ( -9.904830252356999765, -76.53887615466000227, 4.590139709818999769 ) ) ;
#13626 = EDGE_CURVE ( 'NONE', #48919, #26401, #30885, .T. ) ;
#13627 = CARTESIAN_POINT ( 'NONE',  ( 4.658475568430830549, -79.66666666666665719, -8.082524092276877070 ) ) ;
#13628 = CARTESIAN_POINT ( 'NONE',  ( -10.48771805366000009, -21.75560171527000008, 7.686918321049000191 ) ) ;
#13629 = B_SPLINE_CURVE_WITH_KNOTS ( 'NONE', 3,
 ( #27400, #40994, #22984, #585, #49866, #9410, #45434, #54288, #13826, #31824 ),
 .UNSPECIFIED., .F., .F.,
 ( 4, 2, 2, 2, 4 ),
 ( 0.000000000000000000, 0.2500000000000000000, 0.5000000000000000000, 0.7500000000000000000, 1.000000000000000000 ),
 .UNSPECIFIED. ) ;
#13630 = CARTESIAN_POINT ( 'NONE',  ( -4.672105271192539711, -78.18294966887039266, -7.983815220272783009 ) ) ;
#13631 = CARTESIAN_POINT ( 'NONE',  ( 3.632329907060999563, -80.11446594902099605, 10.45854222826000068 ) ) ;
#13632 = CARTESIAN_POINT ( 'NONE',  ( -3.321932689530000093, -81.00000000000000000, 10.22385755016999909 ) ) ;
#13633 = ADVANCED_FACE ( 'NONE', ( #52634 ), #21472, .F. ) ;
#13634 = AXIS2_PLACEMENT_3D ( 'NONE', #22824, #31956, #716 ) ;
#13635 = EDGE_LOOP ( 'NONE', ( #55760, #51233, #57731, #50765 ) ) ;
#13636 = ORIENTED_EDGE ( 'NONE', *, *, #18821, .F. ) ;
#13637 = CARTESIAN_POINT ( 'NONE',  ( -0.006254617009199966819, -77.47520766586539764, 9.249905062637703068 ) ) ;
#13638 = CARTESIAN_POINT ( 'NONE',  ( 10.90987126150000108, -77.25268889183898580, 1.690571823134000118 ) ) ;
#13639 = CIRCLE ( 'NONE', #8928, 12.80000000000000071 ) ;
#13640 = CARTESIAN_POINT ( 'NONE',  ( 9.500000000000001776, -77.63958333333334849, -1.243547092045940827 ) ) ;
#13641 = CARTESIAN_POINT ( 'NONE',  ( -1.565122400816999937, -78.77834523938398092, 9.577113408380000692 ) ) ;
#13642 = CARTESIAN_POINT ( 'NONE',  ( -12.96193297681999823, -76.42049510581999527, -0.3184845575242999938 ) ) ;
#13643 = CARTESIAN_POINT ( 'NONE',  ( -9.382059563581934825, -79.41218430702922149, -1.490898798910053724 ) ) ;
#13644 = CARTESIAN_POINT ( 'NONE',  ( 0.1660104325307999729, -78.07804406081000081, 1.618982269915999916 ) ) ;
#13645 = FACE_OUTER_BOUND ( 'NONE', #38302, .T. ) ;
#13646 = CARTESIAN_POINT ( 'NONE',  ( -4.969435546850999863, -78.51666441077600211, -9.746410964130999943 ) ) ;
#13647 = CARTESIAN_POINT ( 'NONE',  ( -10.01676216527999941, -23.20941515021999635, -7.658899892521000119 ) ) ;
#13648 = CARTESIAN_POINT ( 'NONE',  ( -8.301610278666615272, -79.25879058881317007, 4.784404709358717867 ) ) ;
#13649 = CARTESIAN_POINT ( 'NONE',  ( 3.130963432471999930, -82.51000322433299061, 1.661985514006000031 ) ) ;
#13650 = ORIENTED_EDGE ( 'NONE', *, *, #15995, .T. ) ;
#13651 = CARTESIAN_POINT ( 'NONE',  ( 4.651654258968999756, -78.85273590260798926, 11.27872058466000027 ) ) ;
#13652 = CARTESIAN_POINT ( 'NONE',  ( -4.555356488974000584, -76.23334861441699672, -10.42320189042000145 ) ) ;
#13653 = CARTESIAN_POINT ( 'NONE',  ( -7.605247279250050063, -78.03754162542841755, 7.597531084364455900 ) ) ;
#13654 = CARTESIAN_POINT ( 'NONE',  ( 4.458743082292000004, -77.54633475908899243, 11.11915799896999957 ) ) ;
#13655 = EDGE_CURVE ( 'NONE', #47936, #48492, #8463, .T. ) ;
#13656 = FACE_OUTER_BOUND ( 'NONE', #2470, .T. ) ;
#13657 = DIRECTION ( 'NONE',  ( 0.000000000000000000, 0.000000000000000000, -1.000000000000000000 ) ) ;
#13658 = CARTESIAN_POINT ( 'NONE',  ( 3.106054555984999688, -86.12609999968198338, -1.382904586457999851 ) ) ;
#13659 = CARTESIAN_POINT ( 'NONE',  ( 10.99801204134999999, -80.34957387780099225, -3.007190593213000085 ) ) ;
#13660 = CARTESIAN_POINT ( 'NONE',  ( 0.000000000000000000, -5.899999999999999467, 0.000000000000000000 ) ) ;
#13661 = CARTESIAN_POINT ( 'NONE',  ( -6.940497389897999803, -77.31962105010399000, 8.722619821570999576 ) ) ;
#13662 = CARTESIAN_POINT ( 'NONE',  ( 1.997276839918466829, -1.822916666666666741, 2.598917237794090784 ) ) ;
#13663 = CARTESIAN_POINT ( 'NONE',  ( -11.12160752800000019, -80.38646597062809462, 0.6534909853495001197 ) ) ;
#13664 = VERTEX_POINT ( 'NONE', #5698 ) ;
#13665 = CARTESIAN_POINT ( 'NONE',  ( 1.801614160562000189, -55.41347738061999451, 12.59687422885999908 ) ) ;
#13666 = CARTESIAN_POINT ( 'NONE',  ( -9.454379850511999805, -77.64262403538302237, 0.8787206290761000460 ) ) ;
#13667 = CARTESIAN_POINT ( 'NONE',  ( 1.170835004517000177, -2.368424145665999792, -3.621456637410000123 ) ) ;
#13668 = CARTESIAN_POINT ( 'NONE',  ( -3.513443458492000016, -78.36575305475099640, -10.65240647004999985 ) ) ;
#13669 = LINE ( 'NONE', #43892, #31393 ) ;
#13670 = CARTESIAN_POINT ( 'NONE',  ( 9.252740428349003565, -77.52916666666668277, -2.486604901413146607 ) ) ;
#13671 = CARTESIAN_POINT ( 'NONE',  ( -10.31421052434999908, -76.82175206120300004, 3.823226550887000030 ) ) ;
#13672 = CARTESIAN_POINT ( 'NONE',  ( -1.666727925310000025, -59.99174481743000342, 12.50018462905999961 ) ) ;
#13673 = CARTESIAN_POINT ( 'NONE',  ( 12.78015286811999829, -17.69674784880999852, 1.806262579046000072 ) ) ;
#13674 = CARTESIAN_POINT ( 'NONE',  ( -3.379129515849000231, -86.24207450217399185, 2.374770275150999588 ) ) ;
#13675 = DIRECTION ( 'NONE',  ( 0.000000000000000000, -1.000000000000000000, 0.000000000000000000 ) ) ;
#13676 = CARTESIAN_POINT ( 'NONE',  ( 9.929695104576000020, -54.16901065014000238, -7.973993995727001405 ) ) ;
#13677 = VECTOR ( 'NONE', #32321, 1000.000000000000114 ) ;
#13678 = CARTESIAN_POINT ( 'NONE',  ( 11.24465069584000076, -78.02216546898499416, -0.6259355293341001270 ) ) ;
#13679 = CARTESIAN_POINT ( 'NONE',  ( 0.5818457612699999837, -80.86456775278999487, -1.560998038830999857 ) ) ;
#13680 = CARTESIAN_POINT ( 'NONE',  ( -0.8239329289818000390, -78.88034258879000049, 1.174399563024999926 ) ) ;
#13681 = CIRCLE ( 'NONE', #46720, 10.14999999999999858 ) ;
#13682 = CARTESIAN_POINT ( 'NONE',  ( -1.583004792665463345, -61.25209241118189141, 12.70616254415227786 ) ) ;
#13683 = CARTESIAN_POINT ( 'NONE',  ( 1.250300346049109557, -83.04756661823621755, 0.8499747096666684376 ) ) ;
#13684 = CARTESIAN_POINT ( 'NONE',  ( -12.43646324850000084, -61.72048514535000407, 0.1256879863178999857 ) ) ;
#13685 = DIRECTION ( 'NONE',  ( 0.9999999999998321343, 0.000000000000000000, 5.794540611356191117E-07 ) ) ;
#13686 = CARTESIAN_POINT ( 'NONE',  ( -1.407171709420418138, -77.11458333333332860, -10.75000000000000000 ) ) ;
#13687 = CARTESIAN_POINT ( 'NONE',  ( 6.085875563858039072, -78.52078921777335552, -9.367360191683120618 ) ) ;
#13688 = CIRCLE ( 'NONE', #46724, 8.800000000000000711 ) ;
#13689 = EDGE_LOOP ( 'NONE', ( #10227, #13245, #7825, #20708 ) ) ;
#13690 = FACE_OUTER_BOUND ( 'NONE', #40355, .T. ) ;
#13691 = ADVANCED_FACE ( 'NONE', ( #45879 ), #49317, .F. ) ;
#13692 = CARTESIAN_POINT ( 'NONE',  ( -1.250000000000000000, -55.54999999966999980, -12.00000000000000000 ) ) ;
#13693 = CARTESIAN_POINT ( 'NONE',  ( 10.86346900787000003, -79.15912175438100462, 2.497927478100999910 ) ) ;
#13694 = CARTESIAN_POINT ( 'NONE',  ( -11.00000000000000000, -4.000000000000000000, 0.000000000000000000 ) ) ;
#13695 = ORIENTED_EDGE ( 'NONE', *, *, #53545, .T. ) ;
#13696 = ORIENTED_EDGE ( 'NONE', *, *, #1472, .T. ) ;
#13697 = EDGE_CURVE ( 'NONE', #10344, #24467, #31079, .T. ) ;
#13698 = CARTESIAN_POINT ( 'NONE',  ( 0.8346931312170999817, -80.71870569687999364, -1.265782155144000054 ) ) ;
#13699 = ORIENTED_EDGE ( 'NONE', *, *, #32827, .F. ) ;
#13700 = DIRECTION ( 'NONE',  ( 0.000000000000000000, 0.000000000000000000, -1.000000000000000000 ) ) ;
#13701 = ORIENTED_EDGE ( 'NONE', *, *, #50470, .F. ) ;
#13702 = CARTESIAN_POINT ( 'NONE',  ( 1.132506419232103712, -80.38497993291565535, 0.5291395119344256548 ) ) ;
#13703 = FACE_OUTER_BOUND ( 'NONE', #58068, .T. ) ;
#13704 = CARTESIAN_POINT ( 'NONE',  ( -9.254388464354001087, -79.80752053325198858, 5.469807505829999528 ) ) ;
#13705 = CARTESIAN_POINT ( 'NONE',  ( 1.669724228656999987, -23.36897676534000112, -12.48434610067999984 ) ) ;
#13706 = CARTESIAN_POINT ( 'NONE',  ( 0.8348675186263999626, -81.57621146183899441, 3.662562863923999767 ) ) ;
#13707 = CARTESIAN_POINT ( 'NONE',  ( -9.405479261938486601, -79.38837580768372959, 1.346545511743854506 ) ) ;
#13708 = CARTESIAN_POINT ( 'NONE',  ( 10.74994452723989902, -78.34149450793825054, -1.150020074288363947 ) ) ;
#13710 = EDGE_CURVE ( 'NONE', #25542, #48463, #4729, .T. ) ;
#13709 = CARTESIAN_POINT ( 'NONE',  ( 9.607004209881999657, -78.54473239578000232, 7.045343969285000618 ) ) ;
#13711 = ORIENTED_EDGE ( 'NONE', *, *, #23098, .T. ) ;
#13712 = VERTEX_POINT ( 'NONE', #13757 ) ;
#13713 = CARTESIAN_POINT ( 'NONE',  ( -3.250000000000000000, -1.600000000000000089, 0.000000000000000000 ) ) ;
#13714 = CARTESIAN_POINT ( 'NONE',  ( -1.718598679931974349, -61.04962933016155802, -12.71111582771588999 ) ) ;
#13715 = CARTESIAN_POINT ( 'NONE',  ( -1.565122400816999937, -78.59743646237099313, 9.577113408380000692 ) ) ;
#13716 = CARTESIAN_POINT ( 'NONE',  ( 0.4852795099922571631, -86.17851881763698429, -4.610955397177554538 ) ) ;
#13717 = CARTESIAN_POINT ( 'NONE',  ( -0.3587980661367572432, -85.97359605476890465, 3.418821484678626010 ) ) ;
#13718 = CARTESIAN_POINT ( 'NONE',  ( 7.228795249850000104, -77.50422151684000482, -10.56189739613000000 ) ) ;
#13719 = CARTESIAN_POINT ( 'NONE',  ( -9.022377653937999398, -77.30613138518998539, -8.854484771337999049 ) ) ;
#13720 = TOROIDAL_SURFACE ( 'NONE', #3368, 17.50000000000000000, 5.000000000000000000 ) ;
#13721 = CARTESIAN_POINT ( 'NONE',  ( 2.020917172280999985, -76.38672914931899527, 10.69515428681999936 ) ) ;
#13722 = FACE_OUTER_BOUND ( 'NONE', #17398, .T. ) ;
#13723 = B_SPLINE_CURVE_WITH_KNOTS ( 'NONE', 3,
 ( #17492, #4507, #53219, #49385, #39355, #57363, #52649, #58230, #52936, #40519, #34620, #12203, #21913, #39636, #35187, #17795, #35479, #8343, #48237, #7773, #3911, #13051, #44357, #26622 ),
 .UNSPECIFIED., .F., .F.,
 ( 4, 2, 2, 2, 2, 2, 2, 2, 2, 2, 2, 4 ),
 ( 0.000000000000000000, 0.1250000000000002776, 0.2500000000000005551, 0.3750000000000008327, 0.4375000000000006106, 0.5000000000000004441, 0.6249999999999993339, 0.7499999999999983347, 0.8124999999999977796, 0.8437499999999975575, 0.8749999999999972244, 1.000000000000000000 ),
 .UNSPECIFIED. ) ;
#13724 = CARTESIAN_POINT ( 'NONE',  ( -4.096785958912999348, -78.80273445295348722, -0.8034250144825000328 ) ) ;
#13725 = CARTESIAN_POINT ( 'NONE',  ( 6.985849709488999970, -80.94433431827630443, -8.837815942395002011 ) ) ;
#13726 = CARTESIAN_POINT ( 'NONE',  ( 9.596002108778145967, -76.60208333333332575, 7.374560639699001996 ) ) ;
#13727 = CARTESIAN_POINT ( 'NONE',  ( 9.492740219875408059, -76.89866259748522737, -7.042134608814008878 ) ) ;
#13728 = CARTESIAN_POINT ( 'NONE',  ( 10.75000000000000000, -79.84999999999999432, -2.184490103126999767E-14 ) ) ;
#13729 = CARTESIAN_POINT ( 'NONE',  ( -1.295435361468000091, -77.74096878701278968, -0.3166359884281000348 ) ) ;
#13730 = DIRECTION ( 'NONE',  ( -5.794542751833290187E-07, -4.446058653751146425E-20, 0.9999999999998322453 ) ) ;
#13731 = CARTESIAN_POINT ( 'NONE',  ( -6.474781754604000739, -80.47795770475610766, -9.218806710208998112 ) ) ;
#13732 = CARTESIAN_POINT ( 'NONE',  ( -1.217465845835394411, -79.02083333333330017, -0.3271848554491003647 ) ) ;
#13733 = EDGE_LOOP ( 'NONE', ( #31465, #25213, #5683, #53201 ) ) ;
#13734 = CARTESIAN_POINT ( 'NONE',  ( 0.5847500590559170375, -23.30655143818054498, 10.98448857562229897 ) ) ;
#13735 = FACE_OUTER_BOUND ( 'NONE', #33484, .T. ) ;
#13736 = CARTESIAN_POINT ( 'NONE',  ( -1.234140985588999984, -81.23472830739800088, 0.5054425604136000283 ) ) ;
#13737 = CARTESIAN_POINT ( 'NONE',  ( -7.809619239761000031, -79.88027893010598746, -5.839499659979000334 ) ) ;
#13738 = CARTESIAN_POINT ( 'NONE',  ( 7.287838312904000304, -78.18963704368999856, -10.78085041437000058 ) ) ;
#13739 = EDGE_CURVE ( 'NONE', #20818, #48919, #41469, .T. ) ;
#13740 = DIRECTION ( 'NONE',  ( 0.000000000000000000, 0.000000000000000000, -1.000000000000000000 ) ) ;
#13741 = CARTESIAN_POINT ( 'NONE',  ( 12.60413670420000010, -23.30716680861999990, -1.799502287691000069 ) ) ;
#13742 = ORIENTED_EDGE ( 'NONE', *, *, #44937, .F. ) ;
#13743 = FACE_OUTER_BOUND ( 'NONE', #30017, .T. ) ;
#13744 = DIRECTION ( 'NONE',  ( 0.7071067811865475727, 0.000000000000000000, 0.7071067811865475727 ) ) ;
#13745 = CARTESIAN_POINT ( 'NONE',  ( -1.296597938961999930, -81.75360849247699946, -0.1914542273854999976 ) ) ;
#13746 = CARTESIAN_POINT ( 'NONE',  ( 10.75000000000000000, -76.75000000000000000, 0.000000000000000000 ) ) ;
#13747 = CARTESIAN_POINT ( 'NONE',  ( 9.333674174720000494, -78.19108065130299678, -1.884914489352999878 ) ) ;
#13749 = CARTESIAN_POINT ( 'NONE',  ( 2.863963203921999767, -1.094488518283999845, 2.815564610575000071 ) ) ;
#13748 = CARTESIAN_POINT ( 'NONE',  ( 0.2928406956622999768, -85.03526194493599633, -4.164595335608999527 ) ) ;
#13750 = DIRECTION ( 'NONE',  ( 0.000000000000000000, -1.000000000000000000, 0.000000000000000000 ) ) ;
#13751 = FACE_OUTER_BOUND ( 'NONE', #49619, .T. ) ;
#13752 = ORIENTED_EDGE ( 'NONE', *, *, #6351, .F. ) ;
#13753 = CARTESIAN_POINT ( 'NONE',  ( 0.1205599503558857782, -77.22598671500267642, -10.74930044307334143 ) ) ;
#13754 = DIRECTION ( 'NONE',  ( 0.000000000000000000, 0.000000000000000000, -1.000000000000000000 ) ) ;
#13755 = EDGE_LOOP ( 'NONE', ( #9999, #12189, #47633, #42178, #18898 ) ) ;
#13756 = ORIENTED_EDGE ( 'NONE', *, *, #29377, .F. ) ;
#13757 = CARTESIAN_POINT ( 'NONE',  ( 0.000000000000000000, -86.39999999999999147, -10.14999999999897007 ) ) ;
#13758 = CARTESIAN_POINT ( 'NONE',  ( 8.190859204290999784, -55.64999999967000122, 7.342331066867000544 ) ) ;
#13759 = CARTESIAN_POINT ( 'NONE',  ( 0.000000000000000000, -7.000000000000000000, 0.000000000000000000 ) ) ;
#13760 = EDGE_LOOP ( 'NONE', ( #33462, #6139, #28585, #23503 ) ) ;
#13761 = ADVANCED_FACE ( 'NONE', ( #8755 ), #53629, .T. ) ;
#13762 = CARTESIAN_POINT ( 'NONE',  ( -3.103176923767000162, -78.29540922883299459, -11.64328410086999988 ) ) ;
#13763 = ORIENTED_EDGE ( 'NONE', *, *, #24578, .T. ) ;
#13764 = CIRCLE ( 'NONE', #21315, 1.250000000000000000 ) ;
#13765 = ORIENTED_EDGE ( 'NONE', *, *, #11053, .F. ) ;
#13766 = CARTESIAN_POINT ( 'NONE',  ( 0.5319755900005730398, -2.738347930379791517, -3.208410176395029012 ) ) ;
#13767 = AXIS2_PLACEMENT_3D ( 'NONE', #14486, #5628, #18645 ) ;
#13768 = AXIS2_PLACEMENT_3D ( 'NONE', #44883, #53740, #35118 ) ;
#13769 = CARTESIAN_POINT ( 'NONE',  ( 10.07627163191000008, -55.55000000209000177, -7.601397897754999633 ) ) ;
#13770 = CARTESIAN_POINT ( 'NONE',  ( -12.85144117169000033, -20.24527983099999773, -1.980464439859999981 ) ) ;
#13771 = VERTEX_POINT ( 'NONE', #806 ) ;
#13773 = ADVANCED_FACE ( 'NONE', ( #14341, #4326 ), #17913, .T. ) ;
#13772 = CARTESIAN_POINT ( 'NONE',  ( 0.7834266488161117925, -81.73351092137228591, 1.338899150759432333 ) ) ;
#13774 = ORIENTED_EDGE ( 'NONE', *, *, #29568, .F. ) ;
#13775 = CARTESIAN_POINT ( 'NONE',  ( 5.642655093990001092, -79.27719169461070692, -7.355059082576608454 ) ) ;
#13776 = CARTESIAN_POINT ( 'NONE',  ( 0.000000000000000000, -55.54999999966999980, -12.50000000000000000 ) ) ;
#13777 = DIRECTION ( 'NONE',  ( 0.000000000000000000, 0.000000000000000000, -1.000000000000000000 ) ) ;
#13778 = CARTESIAN_POINT ( 'NONE',  ( -0.5200379331666001859, -18.54844303602364164, 10.98772212209854438 ) ) ;
#13779 = DIRECTION ( 'NONE',  ( 0.7071067811864980568, 1.533578360404995178E-11, -0.7071067811865969777 ) ) ;
#13780 = CARTESIAN_POINT ( 'NONE',  ( 9.396085398178598780, -78.60208333333329733, 7.220923959705271677 ) ) ;
#13781 = CARTESIAN_POINT ( 'NONE',  ( -3.545645331619000196, -77.54891093671713520, 11.44309676683000454 ) ) ;
#13782 = CARTESIAN_POINT ( 'NONE',  ( 6.922474547212758900, -78.79240049070052976, -6.137042015094014147 ) ) ;
#13783 = CARTESIAN_POINT ( 'NONE',  ( 11.84266115483542237, -77.13516788874333940, -2.236516232491894129 ) ) ;
#13784 = CARTESIAN_POINT ( 'NONE',  ( -8.958641849965999882, -25.20112647804999995, 8.950065109822000764 ) ) ;
#13785 = CARTESIAN_POINT ( 'NONE',  ( -5.684882048478777428, -77.67303331842424541, -7.397090001915298529 ) ) ;
#13786 = CARTESIAN_POINT ( 'NONE',  ( -10.26699006316255591, -76.75833333333331154, 5.917523019358029934 ) ) ;
#13787 = CARTESIAN_POINT ( 'NONE',  ( 3.799029931709000163, -82.16542549782599281, -1.620315315797000055 ) ) ;
#13788 = CARTESIAN_POINT ( 'NONE',  ( -3.708203932498999933, -76.29999999999999716, 11.41267819554000162 ) ) ;
#13789 = CARTESIAN_POINT ( 'NONE',  ( 3.074963689382999910, -77.34391332859900103, -9.149746207635999440 ) ) ;
#13790 = CARTESIAN_POINT ( 'NONE',  ( -12.48408657659000021, -18.63026141570000149, 1.669508654504000100 ) ) ;
#13791 = CARTESIAN_POINT ( 'NONE',  ( 12.51072239526000196, -63.10294702885996543, -0.7871079366006996647 ) ) ;
#13792 = CARTESIAN_POINT ( 'NONE',  ( -0.006333666751184999569, -25.33262644299999877, 12.77652491955999992 ) ) ;
#13793 = DIRECTION ( 'NONE',  ( 1.894056206342980493E-11, -1.538486802511980436E-07, 0.9999999999999882316 ) ) ;
#13794 = CARTESIAN_POINT ( 'NONE',  ( 3.547276196037999707, -85.47133100267899408, 0.03730513092754000198 ) ) ;
#13795 = CARTESIAN_POINT ( 'NONE',  ( -0.4356580584946000423, -1.352709358523000116, 3.764349720514999831 ) ) ;
#13796 = CARTESIAN_POINT ( 'NONE',  ( -0.9995835529977281642, -80.94791666666662877, 0.7681833999686391579 ) ) ;
#13797 = CARTESIAN_POINT ( 'NONE',  ( 10.53003223722000037, -55.47547470607999998, 7.612971414697999428 ) ) ;
#13798 = CARTESIAN_POINT ( 'NONE',  ( -1.317248530341201818, -80.39383545476231063, -0.8131718307597066708 ) ) ;
#13799 = CARTESIAN_POINT ( 'NONE',  ( 12.78015149461000100, -61.10330660662999946, -1.806228889759999845 ) ) ;
#13800 = CARTESIAN_POINT ( 'NONE',  ( 7.624341766629000539, -55.53514853726999689, -10.42531125022999916 ) ) ;
#13801 = CARTESIAN_POINT ( 'NONE',  ( -10.01235002622999914, -23.29848884437999956, -7.653559626096999580 ) ) ;
#13802 = CARTESIAN_POINT ( 'NONE',  ( -9.269928330473998557, -77.48231152193199023, 5.765743207788000646 ) ) ;
#13803 = AXIS2_PLACEMENT_3D ( 'NONE', #41893, #50181, #15020 ) ;
#13804 = ADVANCED_FACE ( 'NONE', ( #40641 ), #53057, .F. ) ;
#13805 = CARTESIAN_POINT ( 'NONE',  ( 9.377644441546999943, -77.67925969475899706, 7.928150093746000771 ) ) ;
#13806 = CYLINDRICAL_SURFACE ( 'NONE', #19425, 11.00000000000000000 ) ;
#13808 = CARTESIAN_POINT ( 'NONE',  ( 1.045500971020000058, -79.10632414226799369, 0.9575944129536000382 ) ) ;
#13807 = LINE ( 'NONE', #45719, #40188 ) ;
#13809 = CARTESIAN_POINT ( 'NONE',  ( -1.354012292646000093, -83.30884224245099290, -0.7194680089321999761 ) ) ;
#13810 = VECTOR ( 'NONE', #4002, 1000.000000000000000 ) ;
#13811 = ORIENTED_EDGE ( 'NONE', *, *, #50627, .T. ) ;
#13812 = CIRCLE ( 'NONE', #13768, 2.000000000000000000 ) ;
#13813 = EDGE_CURVE ( 'NONE', #20471, #40525, #55591, .T. ) ;
#13814 = CARTESIAN_POINT ( 'NONE',  ( -3.556690925232000478, -83.35607450217399617, 0.4834121147714999789 ) ) ;
#13815 = CARTESIAN_POINT ( 'NONE',  ( 10.18685315996999918, -79.41692849819099820, 6.201925135593000071 ) ) ;
#13816 = CARTESIAN_POINT ( 'NONE',  ( 10.19393895163000074, -80.85504031229137922, 4.279748970186999735 ) ) ;
#13817 = CIRCLE ( 'NONE', #3458, 9.599999999999999645 ) ;
#13818 = CARTESIAN_POINT ( 'NONE',  ( -1.980584515756000030, -60.06485150062000145, -12.76303204342999997 ) ) ;
#13819 = DIRECTION ( 'NONE',  ( 0.000000000000000000, 0.000000000000000000, -1.000000000000000000 ) ) ;
#13820 = CARTESIAN_POINT ( 'NONE',  ( -8.728447447808001414, -76.78120346591698819, 6.810956705545000212 ) ) ;
#13821 = DIRECTION ( 'NONE',  ( -1.000000000000000000, 0.000000000000000000, 0.000000000000000000 ) ) ;
#13822 = CARTESIAN_POINT ( 'NONE',  ( -9.480927541711999140, -78.34756746102598868, -2.229732866345000009 ) ) ;
#13823 = AXIS2_PLACEMENT_3D ( 'NONE', #14720, #2053, #45759 ) ;
#13824 = CARTESIAN_POINT ( 'NONE',  ( 4.011554133421999957, -1.048748962127999951, -0.3473264786097000067 ) ) ;
#13825 = CARTESIAN_POINT ( 'NONE',  ( 5.629119960535821754, -76.46453612599496807, -10.39280916107768959 ) ) ;
#13826 = CARTESIAN_POINT ( 'NONE',  ( -9.431008682118280362, -61.60059307736693057, 8.251849285865670680 ) ) ;
#13827 = CARTESIAN_POINT ( 'NONE',  ( 10.71369944335147473, -78.82916666666667993, -2.879226727952063580 ) ) ;
#13828 = VERTEX_POINT ( 'NONE', #4852 ) ;
#13829 = CARTESIAN_POINT ( 'NONE',  ( -0.2678032735318023327, -53.58567224679264029, -12.70526550764705753 ) ) ;
#13830 = CARTESIAN_POINT ( 'NONE',  ( -3.903182590741000269, -79.60171332859900417, 8.688219438824999585 ) ) ;
#13831 = DIRECTION ( 'NONE',  ( 0.000000000000000000, -1.000000000000000000, 0.000000000000000000 ) ) ;
#13832 = CARTESIAN_POINT ( 'NONE',  ( 0.9218200799623741393, -81.57708333333334849, -1.199500263597268690 ) ) ;
#13833 = CARTESIAN_POINT ( 'NONE',  ( -12.60413670417000098, -55.49283319101999723, -1.799502287691000069 ) ) ;
#13834 = FACE_OUTER_BOUND ( 'NONE', #46094, .T. ) ;
#13835 = ORIENTED_EDGE ( 'NONE', *, *, #55067, .T. ) ;
#13836 = EDGE_CURVE ( 'NONE', #23858, #378, #37725, .T. ) ;
#13837 = CARTESIAN_POINT ( 'NONE',  ( -10.35967608510999938, -78.02428934957498541, -4.287644625136000087 ) ) ;
#13838 = CARTESIAN_POINT ( 'NONE',  ( 10.36745710150462330, -60.56601929499611714, -7.635228183650348832 ) ) ;
#13839 = EDGE_LOOP ( 'NONE', ( #31691, #40500, #36846, #40212 ) ) ;
#13840 = VERTEX_POINT ( 'NONE', #9569 ) ;
#13841 = CARTESIAN_POINT ( 'NONE',  ( 8.414570695956999913, -60.64999999943950826, 8.414570695956999913 ) ) ;
#13842 = CARTESIAN_POINT ( 'NONE',  ( -9.358268528169000788, -79.29296057154398625, -2.797054701638000296 ) ) ;
#13843 = ORIENTED_EDGE ( 'NONE', *, *, #47920, .F. ) ;
#13845 = EDGE_CURVE ( 'NONE', #12674, #28730, #13393, .T. ) ;
#13844 = CARTESIAN_POINT ( 'NONE',  ( -8.648668203041999902, -77.25441573198799006, -8.819734393706001541 ) ) ;
#13846 = CARTESIAN_POINT ( 'NONE',  ( 8.121699804427876757, -24.83626205760389993, -9.841121124182388158 ) ) ;
#13847 = B_SPLINE_CURVE_WITH_KNOTS ( 'NONE', 3,
 ( #18761, #15197, #42073, #32309, #28765, #51234, #55061, #10785, #28177, #42370 ),
 .UNSPECIFIED., .F., .F.,
 ( 4, 2, 2, 2, 4 ),
 ( 0.000000000000000000, 0.2500000000000000000, 0.5000000000000000000, 0.7500000000000000000, 1.000000000000000000 ),
 .UNSPECIFIED. ) ;
#13848 = CARTESIAN_POINT ( 'NONE',  ( -1.008674225483999987, -77.84257259131000239, -1.303690889073000125 ) ) ;
#13849 = ADVANCED_FACE ( 'NONE', ( #13690 ), #41476, .T. ) ;
#13850 = VERTEX_POINT ( 'NONE', #13984 ) ;
#13851 = CARTESIAN_POINT ( 'NONE',  ( 7.092659876394000307, -77.87782305011499773, 6.312768414564000174 ) ) ;
#13852 = B_SPLINE_CURVE_WITH_KNOTS ( 'NONE', 3,
 ( #17098, #35082, #53118, #52737, #48604, #34420, #51879, #33842, #38859, #24997, #25858, #21143, #39443, #20286, #15856, #16436, #24715, #48040 ),
 .UNSPECIFIED., .F., .F.,
 ( 4, 2, 2, 2, 2, 2, 2, 2, 4 ),
 ( 0.000000000000000000, 0.1249999999999998335, 0.2499999999999997224, 0.3749999999999997224, 0.4999999999999997780, 0.6249999999999997780, 0.7499999999999998890, 0.8749999999999998890, 1.000000000000000000 ),
 .UNSPECIFIED. ) ;
#13853 = CARTESIAN_POINT ( 'NONE',  ( 0.4786272935714176446, -80.25641286416187370, -1.154639604756080073 ) ) ;
#13854 = CARTESIAN_POINT ( 'NONE',  ( -8.012867221502000703, -78.51278494331999980, 9.287323121044000374 ) ) ;
#13855 = VECTOR ( 'NONE', #26236, 1000.000000000000000 ) ;
#13856 = CARTESIAN_POINT ( 'NONE',  ( -3.140974612311351777, -78.90416666666668277, -11.68767212001978884 ) ) ;
#13857 = CARTESIAN_POINT ( 'NONE',  ( 4.545264886168000729, -77.58620964842175738, 8.573871732259998879 ) ) ;
#13858 = CARTESIAN_POINT ( 'NONE',  ( 6.330346032565856262, -79.91530064090616747, 6.754712701908596628 ) ) ;
#13859 = CARTESIAN_POINT ( 'NONE',  ( 10.42531125074000009, -18.73514854687000053, 7.624341767140999870 ) ) ;
#13860 = ORIENTED_EDGE ( 'NONE', *, *, #2135, .F. ) ;
#13861 = CARTESIAN_POINT ( 'NONE',  ( 0.000000000000000000, -23.25000000000000000, 12.00000000000000000 ) ) ;
#13862 = CARTESIAN_POINT ( 'NONE',  ( 2.858906827459719580, -77.25017575896374922, -8.796993064675801222 ) ) ;
#13863 = CARTESIAN_POINT ( 'NONE',  ( 0.3742884389835000047, -79.49753512672899092, -1.469294133937999902 ) ) ;
#13864 = VECTOR ( 'NONE', #39891, 1000.000000000000114 ) ;
#13865 = CARTESIAN_POINT ( 'NONE',  ( 0.6775591888709999733, -77.82597717995859909, -1.132025780260999870 ) ) ;
#13866 = CARTESIAN_POINT ( 'NONE',  ( -3.469432447681296328, -3.362854700287415621, -0.6005825324968658840 ) ) ;
#13867 = EDGE_CURVE ( 'NONE', #51104, #29318, #2072, .T. ) ;
#13868 = CARTESIAN_POINT ( 'NONE',  ( 7.961052042476000068, -61.33567434991999789, -9.783216378940000624 ) ) ;
#13869 = CARTESIAN_POINT ( 'NONE',  ( -11.55418265775999842, -79.02479797882000412, 4.110954701505000308 ) ) ;
#13870 = CARTESIAN_POINT ( 'NONE',  ( 6.725657209017000149, -77.30646084297899279, -9.843613558058999402 ) ) ;
#13871 = CARTESIAN_POINT ( 'NONE',  ( -12.76303204291999904, -55.53514849259999409, -1.980584515756000030 ) ) ;
#13872 = CARTESIAN_POINT ( 'NONE',  ( -9.398705699948999737, -76.96053832859900012, -2.091559270920000380 ) ) ;
#13873 = CARTESIAN_POINT ( 'NONE',  ( 11.68679759850510358, -76.82009992810888832, 3.010188169988853524 ) ) ;
#13874 = DIRECTION ( 'NONE',  ( 0.000000000000000000, 0.000000000000000000, -1.000000000000000000 ) ) ;
#13875 = ORIENTED_EDGE ( 'NONE', *, *, #29617, .T. ) ;
#13876 = CARTESIAN_POINT ( 'NONE',  ( -1.368292558779000023, -82.92709261769098816, 0.5331262435804999811 ) ) ;
#13877 = DIRECTION ( 'NONE',  ( 0.000000000000000000, 0.000000000000000000, 1.000000000000000000 ) ) ;
#13878 = CARTESIAN_POINT ( 'NONE',  ( 7.635227771886311743, -23.76609606960563070, 10.36745004610104637 ) ) ;
#13879 = CARTESIAN_POINT ( 'NONE',  ( 2.697636866285999968, -77.64139156892099436, -11.67213861177999945 ) ) ;
#13880 = CARTESIAN_POINT ( 'NONE',  ( -0.3862712429687000237, -82.25000000000000000, -1.188820645369000006 ) ) ;
#13881 = CARTESIAN_POINT ( 'NONE',  ( 1.496210884224999926, -83.05662218692300769, 0.7325374182646999799 ) ) ;
#13882 = CARTESIAN_POINT ( 'NONE',  ( -10.23070583620000207, -78.53354445816799512, 6.145580569783000158 ) ) ;
#13883 = CARTESIAN_POINT ( 'NONE',  ( 6.669449228234999971, -78.25509805011499509, -7.075468016816000016 ) ) ;
#13884 = CARTESIAN_POINT ( 'NONE',  ( -9.596198845516999754, -77.71369001827098089, -0.8161970854479000392 ) ) ;
#13885 = CARTESIAN_POINT ( 'NONE',  ( 2.844842352609428637, -76.05516034136756787, 11.40062995561528680 ) ) ;
#13886 = CARTESIAN_POINT ( 'NONE',  ( -9.543280303650000462, -79.56693931322499225, -5.301053389303000074 ) ) ;
#13887 = CARTESIAN_POINT ( 'NONE',  ( 3.476140009346946336, -85.79678895079199208, 2.524824982687709607 ) ) ;
#13888 = VERTEX_POINT ( 'NONE', #26673 ) ;
#13889 = EDGE_CURVE ( 'NONE', #36858, #13850, #23171, .T. ) ;
#13890 = CARTESIAN_POINT ( 'NONE',  ( 10.69843650790000034, -76.34117774079464880, 6.089250768039999429 ) ) ;
#13891 = CARTESIAN_POINT ( 'NONE',  ( 2.236739703425203896, -78.43735716284257364, -3.872902730369248925 ) ) ;
#13892 = CARTESIAN_POINT ( 'NONE',  ( -7.508490145779999736, -78.99519950844198490, -8.005410190140000992 ) ) ;
#13893 = CARTESIAN_POINT ( 'NONE',  ( -1.001315002179000047, -17.31477588286000113, -12.50000000000000000 ) ) ;
#13894 = CARTESIAN_POINT ( 'NONE',  ( 12.50385602704033694, -17.21562691850715865, -0.8579623880475349962 ) ) ;
#13895 = CARTESIAN_POINT ( 'NONE',  ( 7.601397897754999633, -60.04999999657000131, 10.07627163191000008 ) ) ;
#13896 = CARTESIAN_POINT ( 'NONE',  ( 10.74999999999999822, -76.75923966921678243, 1.248172908123839076 ) ) ;
#13897 = EDGE_LOOP ( 'NONE', ( #7750, #3537, #50676, #30892 ) ) ;
#13898 = AXIS2_PLACEMENT_3D ( 'NONE', #14645, #50398, #9947 ) ;
#13899 = CARTESIAN_POINT ( 'NONE',  ( -9.674930971187000850, -79.16750321980599381, 5.536272326541999078 ) ) ;
#13900 = CARTESIAN_POINT ( 'NONE',  ( 12.70556836324320926, -16.77227722580009228, 0.2598513551428152102 ) ) ;
#13901 = CARTESIAN_POINT ( 'NONE',  ( 11.49045096393965082, -79.78080184933774888, -2.827711266468116325 ) ) ;
#13902 = CARTESIAN_POINT ( 'NONE',  ( -2.265513599700895053, -78.40681307243320930, 3.757367661055261987 ) ) ;
#13903 = CARTESIAN_POINT ( 'NONE',  ( 12.52785920748583059, -60.59405666895393239, 1.668536824535970631 ) ) ;
#13904 = AXIS2_PLACEMENT_3D ( 'NONE', #10748, #24602, #23721 ) ;
#13905 = CARTESIAN_POINT ( 'NONE',  ( 3.941639820121999094, -79.15290945932498801, 10.32188786877999931 ) ) ;
#13906 = DIRECTION ( 'NONE',  ( 0.000000000000000000, -1.000000000000000000, 0.000000000000000000 ) ) ;
#13907 = CIRCLE ( 'NONE', #17577, 10.20000000000000107 ) ;
#13908 = DIRECTION ( 'NONE',  ( 0.000000000000000000, -1.000000000000000000, 0.000000000000000000 ) ) ;
#13909 = VECTOR ( 'NONE', #27405, 1000.000000000000114 ) ;
#13910 = CARTESIAN_POINT ( 'NONE',  ( 1.199500263597271799, -81.19791666666667140, -0.9218200799623701425 ) ) ;
#13911 = B_SPLINE_CURVE_WITH_KNOTS ( 'NONE', 3,
 ( #29410, #52443, #8723, #21714, #22000, #8144, #48885, #8427, #57727, #17284, #21137, #26716, #58023, #17584, #12283, #35571, #39144, #40312, #48598, #34701, #52732, #7853, #21430, #993, #27229, #4524, #45563, #32526, #36100, #49402, #49697, #54117, #5108, #8951, #40827, #18979, #45268, #36971, #40534, #54984, #129, #9830, #50569, #18105, #49992, #58248, #4817, #10124, #44672, #4225, #23107, #22816, #419, #18397, #22223, #36388, #54415, #13951, #31947, #9538, #27521, #709, #36680, #15706, #32818, #33701, #56157, #11001, #56445, #46740, #42872, #50864, #37260, #46152, #51740, #28395, #2429, #10410, #46442, #42582, #5676, #33411, #11289, #5970, #29269, #6846, #33115, #24856, #51156, #23975, #28986, #16000, #19553, #55274, #23687, #55868, #20432, #1276, #41993, #1561, #38427, #33987, #37551 ),
 .UNSPECIFIED., .F., .F.,
 ( 4, 2, 2, 2, 1, 1, 1, 1, 1, 2, 2, 2, 2, 2, 1, 1, 1, 1, 2, 2, 2, 2, 2, 1, 1, 1, 2, 2, 2, 1, 1, 1, 1, 1, 2, 2, 2, 2, 2, 1, 1, 1, 1, 2, 2, 2, 2, 2, 1, 1, 1, 1, 1, 2, 2, 2, 2, 2, 1, 1, 1, 1, 1, 2, 2, 2, 4 ),
 ( 0.000000000000000000, 0.06249999999999299172, 0.09374999999998949451, 0.1093749999999877598, 0.1171874999999868716, 0.1210937499999864414, 0.1230468749999862610, 0.1240234374999861777, 0.1245117187499861083, 0.1247558593749860389, 0.1249999999999859696, 0.1874999999999704681, 0.2187499999999626965, 0.2343749999999588107, 0.2421874999999568678, 0.2460937499999558964, 0.2480468749999554245, 0.2490234374999552025, 0.2495117187499550637, 0.2499999999999549249, 0.3124999999999380496, 0.3437499999999296119, 0.3593749999999253930, 0.3671874999999233391, 0.3710937499999223954, 0.3730468749999218958, 0.3740234374999217293, 0.3749999999999216183, 0.4374999999999110711, 0.4687499999999057976, 0.4843749999999031886, 0.4921874999999019118, 0.4960937499999012457, 0.4980468749999010236, 0.4990234374999010236, 0.4999999999999010236, 0.5624999999999098499, 0.5937499999999141798, 0.6093749999999164002, 0.6171874999999173994, 0.6210937499999178435, 0.6230468749999181766, 0.6240234374999182876, 0.6245117187499182876, 0.6249999999999183986, 0.6874999999999239497, 0.7187499999999266143, 0.7343749999999279465, 0.7421874999999286127, 0.7460937499999290567, 0.7480468749999292788, 0.7490234374999293898, 0.7495117187499295008, 0.7497558593749296119, 0.7499999999999296119, 0.8124999999999150679, 0.8437499999999077405, 0.8593749999999040767, 0.8671874999999023004, 0.8710937499999014122, 0.8730468749999009681, 0.8740234374999007461, 0.8745117187499007461, 0.8747558593749006350, 0.8749999999999006350, 0.9374999999999502620, 1.000000000000000000 ),
 .UNSPECIFIED. ) ;
#13912 = CARTESIAN_POINT ( 'NONE',  ( 5.413904038987143785, -79.33333333333332860, 9.393203674808290771 ) ) ;
#13913 = CARTESIAN_POINT ( 'NONE',  ( -8.596418555780466875, -78.44791666666665719, 6.606377239730298001 ) ) ;
#13914 = CARTESIAN_POINT ( 'NONE',  ( -12.54705830248999909, -24.53699017355999956, 1.287129557046000183 ) ) ;
#13915 = ORIENTED_EDGE ( 'NONE', *, *, #30353, .F. ) ;
#13916 = ORIENTED_EDGE ( 'NONE', *, *, #48693, .T. ) ;
#13917 = FACE_OUTER_BOUND ( 'NONE', #5637, .T. ) ;
#13918 = CARTESIAN_POINT ( 'NONE',  ( -3.463640081230069168, -77.69897920905084732, -10.20056251384204771 ) ) ;
#13919 = ORIENTED_EDGE ( 'NONE', *, *, #44976, .T. ) ;
#13920 = CARTESIAN_POINT ( 'NONE',  ( -11.08400893144000143, -76.26062989717654261, -1.489506537590000068 ) ) ;
#13921 = CARTESIAN_POINT ( 'NONE',  ( 8.252521514711000705, -24.93405767894999769, 9.650901483139000092 ) ) ;
#13922 = CARTESIAN_POINT ( 'NONE',  ( 8.588902834722000890, -61.93240111547999760, 9.317946123669999636 ) ) ;
#13923 = CARTESIAN_POINT ( 'NONE',  ( -0.9994182591520053283, -82.54857722637443374, 0.7676657006752972690 ) ) ;
#13924 = CARTESIAN_POINT ( 'NONE',  ( -6.457621509944139859, -78.16366907265800990, -6.622725915400998531 ) ) ;
#13925 = CARTESIAN_POINT ( 'NONE',  ( 5.865103843792000227, -78.43489146390899691, -9.561319920857000554 ) ) ;
#13926 = CARTESIAN_POINT ( 'NONE',  ( -8.651034356561854821, -79.51480282387936427, 4.057597226198490503 ) ) ;
#13927 = VERTEX_POINT ( 'NONE', #41442 ) ;
#13928 = CARTESIAN_POINT ( 'NONE',  ( -8.894916816479799593, -25.22809132934175835, 9.073484344813371294 ) ) ;
#13929 = EDGE_LOOP ( 'NONE', ( #49801, #58345, #8993, #55754 ) ) ;
#13930 = CARTESIAN_POINT ( 'NONE',  ( 2.155228666668488557, -77.45640456078321279, 8.995333024866518201 ) ) ;
#13931 = CARTESIAN_POINT ( 'NONE',  ( -4.789974786805000662, -77.95913546579699016, -9.946872946892002076 ) ) ;
#13932 = CARTESIAN_POINT ( 'NONE',  ( -9.247932426686000795, -77.50168256874098915, -0.1955654147372000162 ) ) ;
#13933 = CARTESIAN_POINT ( 'NONE',  ( -8.680270256945998852, -77.29685085726399052, 3.860428508128000313 ) ) ;
#13934 = CARTESIAN_POINT ( 'NONE',  ( -13.12320710921999911, -76.00574241823001387, -0.02004563557600999926 ) ) ;
#13935 = EDGE_CURVE ( 'NONE', #16006, #45077, #43563, .T. ) ;
#13936 = DIRECTION ( 'NONE',  ( -1.000000000000000000, 0.000000000000000000, 0.000000000000000000 ) ) ;
#13937 = CARTESIAN_POINT ( 'NONE',  ( -0.7213013439201000354, -77.79963621190999845, -1.458901041394999876 ) ) ;
#13938 = CARTESIAN_POINT ( 'NONE',  ( 7.648026766735999793, -23.25000000582000226, -10.12290050089000104 ) ) ;
#13939 = CARTESIAN_POINT ( 'NONE',  ( 10.28297802758999957, -78.15146380445199270, -3.734674224488999883 ) ) ;
#13940 = CARTESIAN_POINT ( 'NONE',  ( -10.30458248778999852, -23.76332651811999952, -7.636263891322999875 ) ) ;
#13941 = CARTESIAN_POINT ( 'NONE',  ( -8.190836719257360343, -59.98964892062407728, 7.342356150419296235 ) ) ;
#13942 = CARTESIAN_POINT ( 'NONE',  ( 2.606288821829000124, -83.58068022547898579, -2.467995869495000161 ) ) ;
#13943 = ORIENTED_EDGE ( 'NONE', *, *, #38015, .T. ) ;
#13944 = CARTESIAN_POINT ( 'NONE',  ( -1.794013086462000084, -79.82776776362139515, 12.18547446480999952 ) ) ;
#13945 = CARTESIAN_POINT ( 'NONE',  ( 8.239941435165000883, -76.45166803430799973, 7.842062413654000252 ) ) ;
#13946 = CARTESIAN_POINT ( 'NONE',  ( -7.609103215824061905, -78.03758286351242646, 7.593670151128505630 ) ) ;
#13947 = CARTESIAN_POINT ( 'NONE',  ( -0.4254240051736286610, -3.385416666666666075, 3.249999999999997780 ) ) ;
#13948 = DIRECTION ( 'NONE',  ( 0.000000000000000000, -1.000000000000000000, -9.096334742604000621E-12 ) ) ;
#13949 = CIRCLE ( 'NONE', #23399, 14.00000000000000000 ) ;
#13950 = CARTESIAN_POINT ( 'NONE',  ( 9.050966799188000067, -59.94999999969999749, -7.919595949288999570 ) ) ;
#13951 = CARTESIAN_POINT ( 'NONE',  ( 7.526684410834897143, -80.91343724093917444, 7.679016378754886851 ) ) ;
#13952 = CARTESIAN_POINT ( 'NONE',  ( 3.151000900302999952, -77.92702448625199452, 8.870309342620000592 ) ) ;
#13953 = CARTESIAN_POINT ( 'NONE',  ( 12.70556836347999941, -25.22772277227999993, 2.424222353299999887E-09 ) ) ;
#13954 = CARTESIAN_POINT ( 'NONE',  ( -4.503658352096000073, -77.48303910811499406, -10.19664954867000084 ) ) ;
#13955 = CARTESIAN_POINT ( 'NONE',  ( -1.001315002657000131, -61.48522411647999775, 12.50000000000000000 ) ) ;
#13956 = CARTESIAN_POINT ( 'NONE',  ( 4.337443150956000082, -81.11643595646388860, -9.985393166669998877 ) ) ;
#13957 = ORIENTED_EDGE ( 'NONE', *, *, #34070, .F. ) ;
#13958 = EDGE_CURVE ( 'NONE', #525, #12605, #3039, .T. ) ;
#13959 = CARTESIAN_POINT ( 'NONE',  ( -9.083128615135207085, -77.12447916667788661, 2.440148005863599145 ) ) ;
#13960 = CARTESIAN_POINT ( 'NONE',  ( 6.257930884930855697, -77.96595801179425678, 6.827456521059489525 ) ) ;
#13961 = DIRECTION ( 'NONE',  ( -0.4045849533089092009, -0.8201353736500186509, 0.4045849533089092009 ) ) ;
#13962 = CARTESIAN_POINT ( 'NONE',  ( -10.93308570624999909, -78.28404402574500409, -2.507139558745000052 ) ) ;
#13963 = CARTESIAN_POINT ( 'NONE',  ( -1.439896632895311113, -79.81458333333331723, -11.00000000000000355 ) ) ;
#13964 = CARTESIAN_POINT ( 'NONE',  ( 6.055527902613000002, -77.71999999999999886, 7.319875806370000682 ) ) ;
#13965 = LINE ( 'NONE', #55287, #53379 ) ;
#13966 = CARTESIAN_POINT ( 'NONE',  ( 3.250000000000000000, -1.850000000000000089, 0.000000000000000000 ) ) ;
#13967 = CARTESIAN_POINT ( 'NONE',  ( 0.000000000000000000, -46.43897132165000130, 0.000000000000000000 ) ) ;
#13968 = CARTESIAN_POINT ( 'NONE',  ( -0.7860676397883000766, -84.35142953870898452, 4.097394633328000246 ) ) ;
#13969 = FACE_OUTER_BOUND ( 'NONE', #36285, .T. ) ;
#13970 = EDGE_CURVE ( 'NONE', #35427, #46904, #56190, .T. ) ;
#13972 = ADVANCED_FACE ( 'NONE', ( #12458 ), #19189, .F. ) ;
#13971 = CARTESIAN_POINT ( 'NONE',  ( -5.483474447459000700, -78.90417670422999663, 11.73017812283000083 ) ) ;
#13973 = B_SPLINE_SURFACE_WITH_KNOTS ( 'NONE', 3, 3, ( 
 ( #54322, #5011, #13271, #31262, #12972, #18601, #41027, #22428, #30, #17414, #39842, #26845, #58152, #22128, #53732, #8266, #40139, #9153, #17719, #4428, #44875, #8855, #4726, #36002, #26547, #31858, #618, #13568, #54026, #45469, #49899, #49606, #30970, #9444, #27137 ),
 ( #45176, #3839, #57857, #26267, #44280, #35398, #8555, #4129, #55185, #14727, #36879, #2060, #46938, #5876, #23885, #902, #5300, #10321, #41607, #5582, #37174, #54611, #23593, #51068, #1187, #46352, #28299, #50776, #46644, #19465, #10032, #6173, #24476, #55479, #37460 ),
 ( #15027, #15327, #6463, #41902, #10616, #32435, #54891, #42490, #24182, #28013, #1476, #10913, #50480, #33319, #28597, #32725, #23310, #33021, #46060, #42197, #19178, #1767, #9733, #41318, #19760, #37757, #55778, #51355, #28891, #36590, #14149, #32149, #18883, #50188, #27722 ),
 ( #45766, #14440, #20061, #51654, #38048, #16489, #43350, #11204, #48089, #34468, #56356, #30036, #47521, #3203, #20626, #56071, #43645, #7907, #48369, #38627, #52215, #51933, #56643, #2908, #11773, #16201, #25622, #16777, #56929, #52498, #34758, #12056, #2344, #33611, #43931 ) ),
 .UNSPECIFIED., .F., .F., .F.,
 ( 4, 4 ),
 ( 4, 1, 1, 1, 1, 1, 1, 1, 1, 1, 1, 1, 1, 1, 1, 1, 1, 1, 1, 1, 1, 1, 1, 1, 1, 1, 1, 1, 1, 1, 1, 1, 4 ),
 ( -0.02000000000003999967, 1.020000000000000018 ),
 ( 0.4279355161862000156, 0.4461630610136000374, 0.4643906058410000037, 0.4826181506684000255, 0.5008456954957999363, 0.5190732403232000136, 0.5373007851505999799, 0.5555283299780000572, 0.5737558748054000235, 0.5919834196327999898, 0.6102109644601999561, 0.6284385092876000334, 0.6466660541149999997, 0.6648935989424000770, 0.6831211437698000433, 0.7013486885972000096, 0.7195762334245999758, 0.7378037782519999421, 0.7560313230794000194, 0.7742588679067999857, 0.7924864127342000630, 0.8107139575616000293, 0.8289415023890001066, 0.8471690472163999619, 0.8653965920437999282, 0.8836241368712000055, 0.9018516816985999718, 0.9200792265260000491, 0.9383067713534000154, 0.9565343161808000927, 0.9747618610081999480, 0.9929894058356000253, 1.011216950662999992 ),
 .UNSPECIFIED. ) ;
#13974 = CARTESIAN_POINT ( 'NONE',  ( 10.72689817447000138, -77.43694788753698788, -3.031213639016000272 ) ) ;
#13975 = FACE_OUTER_BOUND ( 'NONE', #53203, .T. ) ;
#13976 = CARTESIAN_POINT ( 'NONE',  ( 1.276747624218999899, -79.09543374892000145, -0.8772774337639999143 ) ) ;
#13977 = CARTESIAN_POINT ( 'NONE',  ( 1.980611416589732610, -60.32597731768191096, 12.74335092666149194 ) ) ;
#13978 = CARTESIAN_POINT ( 'NONE',  ( 0.5734623601598806131, -82.90586325100210274, -1.399525524612139638 ) ) ;
#13979 = CARTESIAN_POINT ( 'NONE',  ( -12.54902678216000034, -61.80971938179000347, 0.4616712539285000028 ) ) ;
#13980 = CARTESIAN_POINT ( 'NONE',  ( -5.970499261319586637, -80.17821983607609582, -8.939495840307154495 ) ) ;
#13981 = CARTESIAN_POINT ( 'NONE',  ( 9.393203674808285442, -77.20833333333332860, -5.413904038987152667 ) ) ;
#13982 = CARTESIAN_POINT ( 'NONE',  ( -11.04080913941738196, -79.33578427474678563, 1.980439979086550117 ) ) ;
#13983 = ORIENTED_EDGE ( 'NONE', *, *, #57496, .T. ) ;
#13984 = CARTESIAN_POINT ( 'NONE',  ( -1.250000000000000000, -81.59999999999999432, 0.000000000000000000 ) ) ;
#13985 = CARTESIAN_POINT ( 'NONE',  ( 0.5668640744809375631, -61.71659694886578507, 12.50470739229114692 ) ) ;
#13986 = CARTESIAN_POINT ( 'NONE',  ( 11.08725735368000009, -79.64937592841299363, 1.152095891907999992 ) ) ;
#13987 = DIRECTION ( 'NONE',  ( 0.000000000000000000, -1.000000000000000000, 0.000000000000000000 ) ) ;
#13988 = ORIENTED_EDGE ( 'NONE', *, *, #38950, .F. ) ;
#13989 = ORIENTED_EDGE ( 'NONE', *, *, #46593, .F. ) ;
#13990 = CARTESIAN_POINT ( 'NONE',  ( -1.462679955183999958, -81.45713598324900317, 0.6839453740269999527 ) ) ;
#13991 = ORIENTED_EDGE ( 'NONE', *, *, #37762, .F. ) ;
#13992 = ORIENTED_EDGE ( 'NONE', *, *, #33434, .F. ) ;
#13993 = CARTESIAN_POINT ( 'NONE',  ( 1.157571443481175466, -80.38088009010486701, 0.4716244123812511901 ) ) ;
#13994 = DIRECTION ( 'NONE',  ( 0.000000000000000000, -1.000000000000000000, 0.000000000000000000 ) ) ;
#13995 = CIRCLE ( 'NONE', #52647, 14.00000000000000000 ) ;
#13996 = CARTESIAN_POINT ( 'NONE',  ( 3.211401065378436837, -82.36145831624757818, -1.243768903017549832 ) ) ;
#13997 = CARTESIAN_POINT ( 'NONE',  ( 0.4450739772392999782, -24.87813214802000061, -12.43586747594999942 ) ) ;
#13998 = CARTESIAN_POINT ( 'NONE',  ( 3.384788216402000227, -81.21931966961800242, 1.194551770192000095 ) ) ;
#13999 = DIRECTION ( 'NONE',  ( 0.000000000000000000, 1.000000000000000000, -5.913433368273000022E-14 ) ) ;
#14000 = CARTESIAN_POINT ( 'NONE',  ( -8.784324219567999137, -78.80339885845999959, -8.047797807107999191 ) ) ;
#14001 = B_SPLINE_CURVE_WITH_KNOTS ( 'NONE', 3,
 ( #1512, #19501, #13901, #5623, #23052, #37496, #55517, #54650, #14767, #9484, #6207, #23634, #41068, #14189, #15064, #32186, #32765, #50226, #41647, #33058, #27762, #1226, #19216, #50812, #28338, #10355, #45805, #46390, #23347, #941, #18923, #24511, #7369, #47838, #2667, #38083, #7084, #25654, #47559, #20662, #11239, #38660, #15367, #25370, #16236, #56106, #29782, #47263, #2944, #48123, #33360, #52533, #56680, #28930, #20944, #38371, #11527, #20093, #43109, #56393, #15944, #34504, #51393, #10949, #29505, #19800, #34215, #12090, #38947, #55814, #52251, #15652, #42815, #43385, #11808, #56962, #2096, #16524, #30073 ),
 .UNSPECIFIED., .F., .F.,
 ( 4, 2, 2, 2, 2, 2, 2, 2, 2, 2, 2, 2, 2, 2, 2, 2, 2, 1, 2, 2, 2, 2, 2, 2, 2, 2, 2, 2, 2, 2, 2, 2, 2, 2, 2, 2, 2, 2, 2, 4 ),
 ( 0.000000000000000000, 0.03125000000000011102, 0.06250000000000022204, 0.07812500000000023592, 0.09375000000000023592, 0.1250000000000002498, 0.1562500000000002776, 0.1875000000000002776, 0.2187500000000002776, 0.2500000000000002776, 0.2656250000000002776, 0.2812500000000002776, 0.3125000000000002776, 0.3437500000000003331, 0.3750000000000003331, 0.4062500000000003331, 0.4218750000000003331, 0.4375000000000003331, 0.4531250000000003331, 0.4687500000000003331, 0.5000000000000003331, 0.5312500000000003331, 0.5625000000000003331, 0.5937500000000003331, 0.6093750000000002220, 0.6250000000000002220, 0.6562500000000002220, 0.6875000000000002220, 0.7187500000000002220, 0.7500000000000002220, 0.7812500000000002220, 0.7968750000000001110, 0.8125000000000001110, 0.8437500000000001110, 0.8750000000000001110, 0.9062500000000001110, 0.9375000000000001110, 0.9687500000000001110, 0.9843750000000000000, 1.000000000000000000 ),
 .UNSPECIFIED. ) ;
#14002 = ORIENTED_EDGE ( 'NONE', *, *, #20260, .F. ) ;
#14003 = ORIENTED_EDGE ( 'NONE', *, *, #14664, .T. ) ;
#14004 = CARTESIAN_POINT ( 'NONE',  ( 0.000000000000000000, -80.59999999999999432, 0.000000000000000000 ) ) ;
#14005 = CARTESIAN_POINT ( 'NONE',  ( -1.668607604570410352, -18.20618368758860584, -12.52787843850897076 ) ) ;
#14006 = FACE_OUTER_BOUND ( 'NONE', #34021, .T. ) ;
#14007 = CARTESIAN_POINT ( 'NONE',  ( 0.2659376973789999710, -79.90663654304400154, -1.306848610430999980 ) ) ;
#14008 = CARTESIAN_POINT ( 'NONE',  ( 9.045658679128999680, -78.98589546046697762, 3.115350657311999782 ) ) ;
#14009 = CARTESIAN_POINT ( 'NONE',  ( -4.524698840038064773, -86.31452044229999387, -0.4331261292401809571 ) ) ;
#14010 = CARTESIAN_POINT ( 'NONE',  ( 1.150732408062571599, -85.92646434825654467, 3.779866689363247545 ) ) ;
#14011 = CARTESIAN_POINT ( 'NONE',  ( -3.259705057564000530, -77.31377916175999587, 12.53941704951999903 ) ) ;
#14012 = CARTESIAN_POINT ( 'NONE',  ( -0.7850755733694999572, -79.21775351646000729, -1.063938263677999929 ) ) ;
#14013 = CARTESIAN_POINT ( 'NONE',  ( -12.60552511010000032, -23.28917723430000208, -1.799501877793999949 ) ) ;
#14014 = PLANE ( 'NONE',  #27382 ) ;
#14015 = CARTESIAN_POINT ( 'NONE',  ( -3.128751238076999730, -81.92924548946498930, -2.764149595522999991 ) ) ;
#14016 = CARTESIAN_POINT ( 'NONE',  ( -6.711381441964999972, -80.12410361490928778, 9.048015653393999713 ) ) ;
#14017 = CARTESIAN_POINT ( 'NONE',  ( -3.028287605162000240, -79.17036001420198943, -9.201769410957998829 ) ) ;
#14018 = CARTESIAN_POINT ( 'NONE',  ( -11.54010588699839168, -76.71678478382965238, -2.556919625331205204 ) ) ;
#14019 = CARTESIAN_POINT ( 'NONE',  ( 11.89973958376643992, -76.19973958328499464, -1.558524492839146403 ) ) ;
#14020 = CARTESIAN_POINT ( 'NONE',  ( 1.324344358081999795, -78.98128437153999926, 0.1571239973995999795 ) ) ;
#14021 = VECTOR ( 'NONE', #45344, 1000.000000000000114 ) ;
#14022 = CARTESIAN_POINT ( 'NONE',  ( 0.000000000000000000, -81.00000000000000000, 0.000000000000000000 ) ) ;
#14023 = CARTESIAN_POINT ( 'NONE',  ( -11.03620408507000050, -80.41776233274890728, -2.260839449595000161 ) ) ;
#14024 = CARTESIAN_POINT ( 'NONE',  ( -2.422546195149999804, -2.247237677196999961, 2.935532677474999907 ) ) ;
#14025 = CARTESIAN_POINT ( 'NONE',  ( 1.250000000000000000, -79.25000000000000000, 0.000000000000000000 ) ) ;
#14026 = ORIENTED_EDGE ( 'NONE', *, *, #25276, .F. ) ;
#14027 = CARTESIAN_POINT ( 'NONE',  ( -10.75000000000000000, -78.60000000000000853, 0.000000000000000000 ) ) ;
#14028 = ADVANCED_FACE ( 'NONE', ( #42904 ), #48489, .F. ) ;
#14029 = CARTESIAN_POINT ( 'NONE',  ( 2.322774810132999690, -78.26209495713698061, -11.19403484768000112 ) ) ;
#14030 = DIRECTION ( 'NONE',  ( 0.000000000000000000, -1.000000000000000000, -1.398881011027999911E-13 ) ) ;
#14031 = CYLINDRICAL_SURFACE ( 'NONE', #38736, 2.600000000000000089 ) ;
#14032 = CARTESIAN_POINT ( 'NONE',  ( 2.062670899361999766, -55.49360215019999742, 12.83044027758000105 ) ) ;
#14034 = CARTESIAN_POINT ( 'NONE',  ( -10.59876350475000173, -77.43341004451998799, 7.550195564144000393 ) ) ;
#14033 = B_SPLINE_CURVE_WITH_KNOTS ( 'NONE', 3,
 ( #2787, #42652, #20221, #37626 ),
 .UNSPECIFIED., .F., .F.,
 ( 4, 4 ),
 ( 0.000000000000000000, 1.000000000000000000 ),
 .UNSPECIFIED. ) ;
#14035 = CARTESIAN_POINT ( 'NONE',  ( -3.921304417499244188, -79.50486137303013834, 10.00992689042903905 ) ) ;
#14036 = AXIS2_PLACEMENT_3D ( 'NONE', #14004, #9005, #45907 ) ;
#14037 = CARTESIAN_POINT ( 'NONE',  ( 8.364738374805998689, -79.36026001420199805, 4.543950435144999744 ) ) ;
#14038 = CARTESIAN_POINT ( 'NONE',  ( 9.538705796123998937, -76.68836589309999852, -8.097544982435998406 ) ) ;
#14039 = VERTEX_POINT ( 'NONE', #12179 ) ;
#14040 = CARTESIAN_POINT ( 'NONE',  ( -9.723174505940001211, -24.47697504200000296, -7.958760297012999807 ) ) ;
#14041 = CARTESIAN_POINT ( 'NONE',  ( -10.88539795434999924, -77.76091993224399346, -2.484616007705999774 ) ) ;
#14042 = EDGE_CURVE ( 'NONE', #24542, #1524, #1890, .T. ) ;
#14043 = CARTESIAN_POINT ( 'NONE',  ( -0.1202781060011000047, -80.91550986868499251, -1.403348216202000120 ) ) ;
#14044 = CARTESIAN_POINT ( 'NONE',  ( 7.627487606609999915, -23.29778595484999926, -10.35845616727999996 ) ) ;
#14045 = CARTESIAN_POINT ( 'NONE',  ( 8.631984821280999753, -78.73816148727799202, -3.755001005681000148 ) ) ;
#14047 = CARTESIAN_POINT ( 'NONE',  ( 2.863963203921999767, -1.129155184950999979, 2.815564610575000071 ) ) ;
#14046 = CARTESIAN_POINT ( 'NONE',  ( -3.863554442403000166, -85.94560505905998582, 1.090945864652000052 ) ) ;
#14048 = CARTESIAN_POINT ( 'NONE',  ( 0.000000000000000000, -90.29999999999999716, 0.000000000000000000 ) ) ;
#14049 = CARTESIAN_POINT ( 'NONE',  ( -0.8374915928969000056, -80.72513535138099883, -0.9453856285906999668 ) ) ;
#14050 = VERTEX_POINT ( 'NONE', #43195 ) ;
#14051 = CARTESIAN_POINT ( 'NONE',  ( 6.710021342196546890, -77.27873848259581280, -8.417207788637705690 ) ) ;
#14052 = CARTESIAN_POINT ( 'NONE',  ( -1.310679582531386389, -78.94166666666664867, -0.7554284705563492075 ) ) ;
#14053 = CARTESIAN_POINT ( 'NONE',  ( 0.000000000000000000, -75.00000000000000000, 0.000000000000000000 ) ) ;
#14054 = ORIENTED_EDGE ( 'NONE', *, *, #41008, .T. ) ;
#14055 = ORIENTED_EDGE ( 'NONE', *, *, #33434, .T. ) ;
#14056 = CARTESIAN_POINT ( 'NONE',  ( -11.15966350340000091, -79.67123644811400140, 4.490997254915999548 ) ) ;
#14057 = FACE_OUTER_BOUND ( 'NONE', #16344, .T. ) ;
#14058 = DIRECTION ( 'NONE',  ( -1.000000000000000000, 0.000000000000000000, 0.000000000000000000 ) ) ;
#14059 = ORIENTED_EDGE ( 'NONE', *, *, #50912, .F. ) ;
#14060 =( GEOMETRIC_REPRESENTATION_CONTEXT ( 3 ) GLOBAL_UNCERTAINTY_ASSIGNED_CONTEXT ( ( #48713 ) ) GLOBAL_UNIT_ASSIGNED_CONTEXT ( ( #24611, #6013, #24322 ) ) REPRESENTATION_CONTEXT ( 'NONE', 'WORKASPACE' ) );
#14061 = CARTESIAN_POINT ( 'NONE',  ( 2.241689414777999989, -78.05124539001899109, 11.83936654731000004 ) ) ;
#14062 = EDGE_CURVE ( 'NONE', #26404, #28211, #2838, .T. ) ;
#14063 = EDGE_LOOP ( 'NONE', ( #19007, #53052, #54625 ) ) ;
#14064 = ORIENTED_EDGE ( 'NONE', *, *, #26142, .F. ) ;
#14065 = CARTESIAN_POINT ( 'NONE',  ( -2.256754848263711644, -2.664732714192036500, -2.338051317333970758 ) ) ;
#14066 = CARTESIAN_POINT ( 'NONE',  ( -1.570796326794938524, -78.68541666666666856, 11.99999999999999645 ) ) ;
#14067 = CARTESIAN_POINT ( 'NONE',  ( -12.85140862673999784, -21.75560170163999985, -1.980464483675000054 ) ) ;
#14068 = ORIENTED_EDGE ( 'NONE', *, *, #49087, .T. ) ;
#14069 = CARTESIAN_POINT ( 'NONE',  ( 0.9403724367845377463, -82.79329554165276761, -0.8236006839109907274 ) ) ;
#14071 = EDGE_LOOP ( 'NONE', ( #37173, #11468, #30014, #14786 ) ) ;
#14070 = B_SPLINE_CURVE_WITH_KNOTS ( 'NONE', 3,
 ( #50972, #19666, #32634, #37076, #46263, #32928, #37954, #24389, #10523, #42689, #55977, #28506, #51558, #46556, #2253, #55682, #6081, #33806 ),
 .UNSPECIFIED., .F., .F.,
 ( 4, 2, 2, 2, 2, 2, 2, 2, 4 ),
 ( 0.000000000000000000, 0.1250000000000000000, 0.2500000000000000000, 0.3750000000000000000, 0.5000000000000000000, 0.6250000000000000000, 0.7500000000000000000, 0.8750000000000000000, 1.000000000000000000 ),
 .UNSPECIFIED. ) ;
#14072 = CARTESIAN_POINT ( 'NONE',  ( -0.8487208968565155276, -79.71719264087836621, -0.9500917389677994151 ) ) ;
#14073 = AXIS2_PLACEMENT_3D ( 'NONE', #35220, #26372, #21663 ) ;
#14074 = DIRECTION ( 'NONE',  ( 0.000000000000000000, 0.000000000000000000, 1.000000000000000000 ) ) ;
#14075 = ADVANCED_FACE ( 'NONE', ( #43479 ), #21034, .F. ) ;
#14076 = CARTESIAN_POINT ( 'NONE',  ( 0.000000000000000000, -75.15999999999999659, 0.000000000000000000 ) ) ;
#14077 = CIRCLE ( 'NONE', #11274, 0.5000000000000006661 ) ;
#14078 = CARTESIAN_POINT ( 'NONE',  ( -1.432420283025999996, -76.08353766477399915, 11.09153081809999897 ) ) ;
#14079 = CARTESIAN_POINT ( 'NONE',  ( 10.26699006316251683, -77.09166666666665435, 5.917523019358090330 ) ) ;
#14080 = CARTESIAN_POINT ( 'NONE',  ( -0.7999999999999001243, -18.84999999997999964, -12.00000000000000000 ) ) ;
#14081 = CARTESIAN_POINT ( 'NONE',  ( 7.653559502261000347, -55.50150862742999891, -10.01234990226999955 ) ) ;
#14082 = CARTESIAN_POINT ( 'NONE',  ( -1.552995512644810727, -78.71162349006438319, -9.118897746246291902 ) ) ;
#14083 = CARTESIAN_POINT ( 'NONE',  ( 11.75000000000000000, -76.45000000000000284, 0.000000000000000000 ) ) ;
#14084 = CARTESIAN_POINT ( 'NONE',  ( 1.980532734072999901, -19.23767313188999850, -12.80090744966999949 ) ) ;
#14085 = CARTESIAN_POINT ( 'NONE',  ( -0.4872545538094000261, -79.22957563311599927, -1.241463230931000084 ) ) ;
#14086 = CARTESIAN_POINT ( 'NONE',  ( -8.083004225747728810, -77.64177325540374852, -4.658611240203036630 ) ) ;
#14087 = CARTESIAN_POINT ( 'NONE',  ( -3.075537641221584018, -76.69583333333332575, 11.44417895085269876 ) ) ;
#14088 = CARTESIAN_POINT ( 'NONE',  ( -1.334631830339999770, -81.68828455456798565, -3.731588630313000365 ) ) ;
#14089 = CARTESIAN_POINT ( 'NONE',  ( -12.61277494329999982, -18.80332099654000189, 1.798398135845000079 ) ) ;
#14090 = CARTESIAN_POINT ( 'NONE',  ( 13.13047446164998711, -59.58578169018999660, -0.8260994316375004365 ) ) ;
#14091 = CARTESIAN_POINT ( 'NONE',  ( -1.890224871707000043, -23.74789248015000354, 12.68696160873999901 ) ) ;
#14092 = CARTESIAN_POINT ( 'NONE',  ( 12.00000000112311227, -79.25000000000001421, -1.256637052497524998 ) ) ;
#14093 = CARTESIAN_POINT ( 'NONE',  ( 9.392881678679827928, -79.99999999999998579, 1.479774839917263440 ) ) ;
#14094 = CARTESIAN_POINT ( 'NONE',  ( 2.171457335693999902, -1.642097686686999847, -3.105636093276999965 ) ) ;
#14095 = EDGE_CURVE ( 'NONE', #56909, #12948, #42213, .T. ) ;
#14096 = CARTESIAN_POINT ( 'NONE',  ( 0.7681833999686413783, -80.82291666666668561, 0.9995835529977274980 ) ) ;
#14097 = CARTESIAN_POINT ( 'NONE',  ( 1.532229593839658177, -54.67701036644005086, -12.51228690871818117 ) ) ;
#14098 = CARTESIAN_POINT ( 'NONE',  ( 10.24996238029999951, -57.04828923575999511, 7.705119999435999567 ) ) ;
#14100 = EDGE_CURVE ( 'NONE', #38037, #47780, #10376, .T. ) ;
#14099 = CARTESIAN_POINT ( 'NONE',  ( -1.933650113856000052, -23.40786253026000097, -12.70909635754000000 ) ) ;
#14101 = CARTESIAN_POINT ( 'NONE',  ( 10.36873448126860886, -78.14542693329265433, -2.835127193485178054 ) ) ;
#14102 = CARTESIAN_POINT ( 'NONE',  ( 2.067335093441000193, -2.868853494984999752, 2.806303441592000070 ) ) ;
#14103 = CARTESIAN_POINT ( 'NONE',  ( 0.6295237254636258939, -80.66666666666665719, -1.092232985442821658 ) ) ;
#14104 = CARTESIAN_POINT ( 'NONE',  ( 6.606416481926000728, -77.54361311763999254, -10.35137867379999932 ) ) ;
#14105 = DIRECTION ( 'NONE',  ( 0.7071067811865969777, -1.534448722697995070E-11, -0.7071067811864980568 ) ) ;
#14106 = CARTESIAN_POINT ( 'NONE',  ( -1.256882289721999779, -78.75903577859999416, 0.6559773548962000156 ) ) ;
#14107 = CARTESIAN_POINT ( 'NONE',  ( -1.519651782304000109, -81.72970439103998785, -0.4528301974880000191 ) ) ;
#14108 = VERTEX_POINT ( 'NONE', #21606 ) ;
#14109 = CARTESIAN_POINT ( 'NONE',  ( 1.861591581734000078, -85.74949735065199263, 3.016529892209999897 ) ) ;
#14110 = CARTESIAN_POINT ( 'NONE',  ( -3.693060907207000199, -79.52346302158100855, 11.34006851057000098 ) ) ;
#14111 = CARTESIAN_POINT ( 'NONE',  ( -1.088868221116000123, -80.19055927822239482, -11.00213361798000022 ) ) ;
#14112 = EDGE_CURVE ( 'NONE', #52197, #39336, #56566, .T. ) ;
#14113 = CYLINDRICAL_SURFACE ( 'NONE', #3052, 10.75000000000000000 ) ;
#14114 = CARTESIAN_POINT ( 'NONE',  ( -3.106054822367000146, -86.10000002299598520, 1.382903988153999952 ) ) ;
#14115 = DIRECTION ( 'NONE',  ( 0.000000000000000000, -1.000000000000000000, 0.000000000000000000 ) ) ;
#14116 = FACE_OUTER_BOUND ( 'NONE', #23920, .T. ) ;
#14117 = VECTOR ( 'NONE', #14557, 1000.000000000000000 ) ;
#14118 = CARTESIAN_POINT ( 'NONE',  ( 5.420640129221999892, -77.59535537052001075, 11.42023903890000014 ) ) ;
#14119 = CARTESIAN_POINT ( 'NONE',  ( 9.577678893670999116, -79.01112094065199187, -1.184610362647000148 ) ) ;
#14120 = CARTESIAN_POINT ( 'NONE',  ( -8.156245788203044356, -76.13854166665944945, 7.337572461140913660 ) ) ;
#14121 = ORIENTED_EDGE ( 'NONE', *, *, #500, .F. ) ;
#14122 = CARTESIAN_POINT ( 'NONE',  ( 1.401388975520859947, -80.71718075262650416, -0.6178868534844423888 ) ) ;
#14123 = CARTESIAN_POINT ( 'NONE',  ( -6.633041932324000634, -79.56653998579798781, 6.683243331267000542 ) ) ;
#14124 = DIRECTION ( 'NONE',  ( 0.000000000000000000, 0.000000000000000000, -1.000000000000000000 ) ) ;
#14125 = CARTESIAN_POINT ( 'NONE',  ( 1.302799686710000016, -77.90148386876100517, 0.2851120931344000020 ) ) ;
#14126 = CARTESIAN_POINT ( 'NONE',  ( 1.250000000000000000, -76.40000000064199526, 0.000000000000000000 ) ) ;
#14127 = EDGE_LOOP ( 'NONE', ( #5780, #11970, #30092, #12320, #18613, #6514, #8455, #14523, #3692, #21243, #35687, #15991 ) ) ;
#14128 = CARTESIAN_POINT ( 'NONE',  ( -1.544822269226999945, -77.17104737372439160, -11.21622675622000109 ) ) ;
#14129 = CARTESIAN_POINT ( 'NONE',  ( -1.667936697358999965, -19.23537109840999904, 12.53241208775999915 ) ) ;
#14130 = ORIENTED_EDGE ( 'NONE', *, *, #33717, .F. ) ;
#14131 = LINE ( 'NONE', #27704, #1930 ) ;
#14132 = CARTESIAN_POINT ( 'NONE',  ( -0.6514213267380000172, -79.77076566372298316, 9.745581310452999801 ) ) ;
#14133 = VERTEX_POINT ( 'NONE', #54373 ) ;
#14134 = CYLINDRICAL_SURFACE ( 'NONE', #57210, 1.750000000000001332 ) ;
#14135 = CARTESIAN_POINT ( 'NONE',  ( 0.000000000000000000, -75.20000000000000284, 7.200000000000000178 ) ) ;
#14136 = CIRCLE ( 'NONE', #34860, 8.500000000000000000 ) ;
#14137 = CARTESIAN_POINT ( 'NONE',  ( -0.5697605620548999994, -78.36688828910999405, -1.546692981914000065 ) ) ;
#14138 = ORIENTED_EDGE ( 'NONE', *, *, #26362, .F. ) ;
#14139 = CARTESIAN_POINT ( 'NONE',  ( -9.391369684923001060, -77.05817305011500196, 1.399863080762999923 ) ) ;
#14140 = EDGE_CURVE ( 'NONE', #4628, #29025, #25459, .T. ) ;
#14141 = CARTESIAN_POINT ( 'NONE',  ( -0.8629689471358689135, -80.16484394472540487, -0.9039662746332275400 ) ) ;
#14142 = CARTESIAN_POINT ( 'NONE',  ( -10.68064082909000057, -77.44512210326000456, 7.608522161463999289 ) ) ;
#14143 = CARTESIAN_POINT ( 'NONE',  ( -1.342463812738999916E-14, -80.75000000002938805, -13.94999999997000018 ) ) ;
#14144 = B_SPLINE_CURVE_WITH_KNOTS ( 'NONE', 3,
 ( #36465, #28178, #41777, #54492, #41193, #782, #14315, #41483, #18762, #54773, #1069, #32310, #14609, #19056, #37045, #19346, #55946, #46817 ),
 .UNSPECIFIED., .F., .F.,
 ( 4, 2, 2, 2, 2, 2, 2, 2, 4 ),
 ( 0.000000000000000000, 0.06249999999999433786, 0.1249999999999886757, 0.2499999999999873435, 0.4999999999999846789, 0.7499999999999829026, 0.8124999999999845679, 0.8749999999999862332, 1.000000000000000000 ),
 .UNSPECIFIED. ) ;
#14145 = CARTESIAN_POINT ( 'NONE',  ( 6.811742960620783549, -79.90924285524151571, 6.259193223187502042 ) ) ;
#14146 = CARTESIAN_POINT ( 'NONE',  ( -1.999231267869926443, -78.95052081507967046, -3.478840346404192374 ) ) ;
#14147 = ORIENTED_EDGE ( 'NONE', *, *, #44181, .F. ) ;
#14148 = CARTESIAN_POINT ( 'NONE',  ( -8.324924863653999196, -77.20749743507077767, 4.923709561474999497 ) ) ;
#14149 = CARTESIAN_POINT ( 'NONE',  ( 1.328206530128999807, -76.61626955243001191, -12.23810562210000086 ) ) ;
#14150 = CARTESIAN_POINT ( 'NONE',  ( 1.493900225960000050, -80.58901284111300356, -0.2592381030950999810 ) ) ;
#14151 = VECTOR ( 'NONE', #13319, 1000.000000000000000 ) ;
#14152 = CARTESIAN_POINT ( 'NONE',  ( -1.304001331138744835, -2.254477797239900827, 3.271227269354120892 ) ) ;
#14153 = AXIS2_PLACEMENT_3D ( 'NONE', #17670, #22081, #35656 ) ;
#14154 = CARTESIAN_POINT ( 'NONE',  ( 8.652376385632999600, -62.06264602932999708, -9.414489258850998965 ) ) ;
#14155 = CARTESIAN_POINT ( 'NONE',  ( -9.356096982537000173, -78.99605726074999268, 7.928589704419000128 ) ) ;
#14156 = DIRECTION ( 'NONE',  ( 1.000000000000000000, 0.000000000000000000, 0.000000000000000000 ) ) ;
#14157 = CARTESIAN_POINT ( 'NONE',  ( 12.71162569433669276, -17.76025712763402709, -1.720540999442599972 ) ) ;
#14158 = CARTESIAN_POINT ( 'NONE',  ( 4.012560540388999009, -77.03813998579801137, -8.871969369447000986 ) ) ;
#14159 = CARTESIAN_POINT ( 'NONE',  ( -12.01728813451669176, -77.04247429093877031, 1.133778321476297535 ) ) ;
#14160 = CARTESIAN_POINT ( 'NONE',  ( 6.617191270873545861, -76.11991961324837064, -11.22154644849154081 ) ) ;
#14161 = ORIENTED_EDGE ( 'NONE', *, *, #16105, .F. ) ;
#14163 = EDGE_CURVE ( 'NONE', #46988, #20674, #34831, .T. ) ;
#14162 = CARTESIAN_POINT ( 'NONE',  ( 0.3210957952920999725, -81.66406578914998704, -1.312678830453999801 ) ) ;
#14164 = CARTESIAN_POINT ( 'NONE',  ( 0.2122939316688999822, -79.65754610911000100, -1.334248387208000208 ) ) ;
#14165 = DIRECTION ( 'NONE',  ( -1.000000000000000000, 0.000000000000000000, 0.000000000000000000 ) ) ;
#14166 = CARTESIAN_POINT ( 'NONE',  ( 10.42503750987000011, -77.20732252214099844, -5.902083371034000159 ) ) ;
#14167 = CARTESIAN_POINT ( 'NONE',  ( 8.130366562757448179, -77.00000000000001421, -4.953553662479941444 ) ) ;
#14168 = CARTESIAN_POINT ( 'NONE',  ( -0.5790013745696001024, -82.86714454159299237, -1.562055304842999925 ) ) ;
#14169 = CARTESIAN_POINT ( 'NONE',  ( 12.04731061283000138, -77.76045519273699824, 0.2409951698105000095 ) ) ;
#14170 = CARTESIAN_POINT ( 'NONE',  ( -8.705161348370999974, -77.74211384739999176, -4.119875709756000148 ) ) ;
#14171 = CARTESIAN_POINT ( 'NONE',  ( 2.294676624047414126, -76.05915692578440712, 11.52361598551882516 ) ) ;
#14172 = CARTESIAN_POINT ( 'NONE',  ( 10.85828250482999913, -79.78483005723899169, 1.128302723381999995 ) ) ;
#14173 = CARTESIAN_POINT ( 'NONE',  ( 3.380118192975979152, -85.79678895079199208, -1.504925579246046530 ) ) ;
#14174 = VERTEX_POINT ( 'NONE', #49357 ) ;
#14175 = LINE ( 'NONE', #643, #48359 ) ;
#14176 = CARTESIAN_POINT ( 'NONE',  ( 3.699999999670000594, -78.39678895079168797, -1.355252715606880543E-15 ) ) ;
#14177 = EDGE_CURVE ( 'NONE', #13366, #1523, #54666, .T. ) ;
#14178 = CIRCLE ( 'NONE', #42479, 1.250000000000000000 ) ;
#14179 = CARTESIAN_POINT ( 'NONE',  ( -10.65673661723999999, -78.97122537111499696, 2.626400817186000047 ) ) ;
#14180 = EDGE_CURVE ( 'NONE', #41402, #38250, #22638, .T. ) ;
#14181 = DIRECTION ( 'NONE',  ( 0.000000000000000000, -1.000000000000000000, 0.000000000000000000 ) ) ;
#14182 = CARTESIAN_POINT ( 'NONE',  ( 0.4258703671788000023, -76.00112020995099726, -12.49690866505999942 ) ) ;
#14183 = LINE ( 'NONE', #50512, #2909 ) ;
#14184 = CARTESIAN_POINT ( 'NONE',  ( 9.830798712624998714, -17.90910918523000106, -7.765013391413999599 ) ) ;
#14185 = CARTESIAN_POINT ( 'NONE',  ( 14.00000000000000000, -80.70000000000000284, -1.714505518806294638E-15 ) ) ;
#14186 = ORIENTED_EDGE ( 'NONE', *, *, #56179, .T. ) ;
#14187 = CARTESIAN_POINT ( 'NONE',  ( 9.395013887366999938, -79.00408516179498974, 5.999026139886999509 ) ) ;
#14188 = CARTESIAN_POINT ( 'NONE',  ( 12.70395600760365795, -17.39327811306810645, 1.447166682387068137 ) ) ;
#14189 = CARTESIAN_POINT ( 'NONE',  ( -4.106759750389861630, -79.64664839926052764, -11.09893327577296773 ) ) ;
#14190 = CARTESIAN_POINT ( 'NONE',  ( -1.164165648490407268, -81.57056345355888993, 0.4549354940310009754 ) ) ;
#14191 = AXIS2_PLACEMENT_3D ( 'NONE', #55214, #5049, #41062 ) ;
#14192 = CARTESIAN_POINT ( 'NONE',  ( 12.50728630775800809, -61.79975539279633523, -0.1757873579559299515 ) ) ;
#14193 = DIRECTION ( 'NONE',  ( -1.000000000000000000, 0.000000000000000000, 0.000000000000000000 ) ) ;
#14194 = CIRCLE ( 'NONE', #3825, 0.5000000000000004441 ) ;
#14195 = EDGE_CURVE ( 'NONE', #13166, #32124, #17517, .T. ) ;
#14196 = CYLINDRICAL_SURFACE ( 'NONE', #47859, 1.750000000000000000 ) ;
#14197 = LINE ( 'NONE', #18354, #22674 ) ;
#14198 = CARTESIAN_POINT ( 'NONE',  ( -4.985602094412718621, -78.53757981385534492, -9.778117948741643417 ) ) ;
#14199 = CARTESIAN_POINT ( 'NONE',  ( 12.70451796513349763, -53.62354927360125600, -0.5205401192079295303 ) ) ;
#14200 = ORIENTED_EDGE ( 'NONE', *, *, #44844, .T. ) ;
#14201 = VERTEX_POINT ( 'NONE', #58206 ) ;
#14202 = CARTESIAN_POINT ( 'NONE',  ( 8.472259919707001430, -78.67418998579800871, 5.354284829591000161 ) ) ;
#14203 = CARTESIAN_POINT ( 'NONE',  ( 8.197432492207889609, -78.79411831125318599, -6.956612881758995393 ) ) ;
#14204 = ORIENTED_EDGE ( 'NONE', *, *, #50879, .F. ) ;
#14205 = DIRECTION ( 'NONE',  ( 0.000000000000000000, -1.000000000000000000, 0.000000000000000000 ) ) ;
#14206 = CARTESIAN_POINT ( 'NONE',  ( 7.633478499826000352, -23.20098177597000344, 10.36292345935000014 ) ) ;
#14207 = EDGE_CURVE ( 'NONE', #18212, #13840, #12603, .T. ) ;
#14208 = EDGE_CURVE ( 'NONE', #18144, #20659, #19779, .T. ) ;
#14209 = CARTESIAN_POINT ( 'NONE',  ( 7.761030428359000588, -60.88151201342000007, 9.835168816244998169 ) ) ;
#14210 = CARTESIAN_POINT ( 'NONE',  ( -11.14725709413418997, -77.08267626182042420, -4.956903492521361976 ) ) ;
#14211 = CARTESIAN_POINT ( 'NONE',  ( -8.885737597169484303, -77.99140041745337726, 8.035151442397836519 ) ) ;
#14212 = CARTESIAN_POINT ( 'NONE',  ( 2.315902194296999728, -78.40765512090699474, -10.97517055051999968 ) ) ;
#14213 = CARTESIAN_POINT ( 'NONE',  ( -1.714140276207581914, -81.00000000000000000, 10.66650235410891767 ) ) ;
#14214 = EDGE_LOOP ( 'NONE', ( #15227, #51567, #51259 ) ) ;
#14215 = CARTESIAN_POINT ( 'NONE',  ( -9.250000000000000000, -77.49999999999998579, -1.203901273580999948E-14 ) ) ;
#14216 = CIRCLE ( 'NONE', #23661, 5.100000000000000533 ) ;
#14217 = VERTEX_POINT ( 'NONE', #51407 ) ;
#14218 = CARTESIAN_POINT ( 'NONE',  ( 2.146749720031601250, -77.45647823904469931, 8.997362320892142051 ) ) ;
#14219 = CARTESIAN_POINT ( 'NONE',  ( -1.996894868142000012, -77.31962480082998468, 10.85801781015000067 ) ) ;
#14220 = CARTESIAN_POINT ( 'NONE',  ( -8.485281374238999419, -59.94999999967000548, 8.485281374238999419 ) ) ;
#14221 = CARTESIAN_POINT ( 'NONE',  ( -5.159044788988000008, -77.47084909945098730, -8.219183903844999861 ) ) ;
#14222 = DIRECTION ( 'NONE',  ( 0.000000000000000000, -1.000000000000000000, 0.000000000000000000 ) ) ;
#14223 = CARTESIAN_POINT ( 'NONE',  ( -1.570796326794884790, -78.51458333333332007, -12.00000000000000355 ) ) ;
#14224 = CARTESIAN_POINT ( 'NONE',  ( 1.621809933883000099, -78.46781504927000128, 0.1356303529659999840 ) ) ;
#14225 = CARTESIAN_POINT ( 'NONE',  ( 0.000000000000000000, -81.89999999962999766, 0.000000000000000000 ) ) ;
#14226 = CARTESIAN_POINT ( 'NONE',  ( -9.408410525920000822, -79.47180445808699290, -5.582976599613999724 ) ) ;
#14227 = CARTESIAN_POINT ( 'NONE',  ( 1.667916687244999974, -60.09849137196000157, -12.49168433582000226 ) ) ;
#14228 = DIRECTION ( 'NONE',  ( 1.000000000000000000, 0.000000000000000000, 2.044033345361000115E-13 ) ) ;
#14229 = CARTESIAN_POINT ( 'NONE',  ( -2.308137181837000451, -83.21992897967898273, -2.748863001877999590 ) ) ;
#14230 = ORIENTED_EDGE ( 'NONE', *, *, #10590, .F. ) ;
#14231 = CARTESIAN_POINT ( 'NONE',  ( -3.807671504463999934, -79.34114693175598632, 11.71356677268999924 ) ) ;
#14232 = AXIS2_PLACEMENT_3D ( 'NONE', #52428, #25549, #3132 ) ;
#14233 = CARTESIAN_POINT ( 'NONE',  ( -11.47220708781999932, -76.21374791087299627, -0.7050395033892999930 ) ) ;
#14234 = CARTESIAN_POINT ( 'NONE',  ( 9.574729143547433097, -77.88772600167752103, 4.887204184123924655 ) ) ;
#14235 = CARTESIAN_POINT ( 'NONE',  ( 4.374544387491000386, -77.35642955112200525, -11.15253550093999912 ) ) ;
#14236 = CARTESIAN_POINT ( 'NONE',  ( -10.00831378477999856, -18.62769332291999902, 7.646786280044999273 ) ) ;
#14237 = CIRCLE ( 'NONE', #1048, 9.500000000000000000 ) ;
#14239 = FACE_OUTER_BOUND ( 'NONE', #54405, .T. ) ;
#14238 = CARTESIAN_POINT ( 'NONE',  ( 1.538071403320016461, -78.43541666666665435, -11.74999999999999822 ) ) ;
#14240 = CARTESIAN_POINT ( 'NONE',  ( 1.107543465625472345, -3.400486210132132481, -3.341007379328037707 ) ) ;
#14241 = CARTESIAN_POINT ( 'NONE',  ( -8.751877897654001259, -78.60919638534799958, -3.466385404677000182 ) ) ;
#14242 = CARTESIAN_POINT ( 'NONE',  ( -3.620209227049993039, -85.94828561723799965, 1.611820994701015364 ) ) ;
#14243 = CARTESIAN_POINT ( 'NONE',  ( -6.771245932390999478, -78.53127452059300140, -8.709304295962999376 ) ) ;
#14244 = CARTESIAN_POINT ( 'NONE',  ( -6.940239200437514633, -76.07416453009285817, 9.811877043595169212 ) ) ;
#14245 = CARTESIAN_POINT ( 'NONE',  ( -9.059593803572999704, -80.91060369710268674, 6.284180259888000109 ) ) ;
#14246 = ORIENTED_EDGE ( 'NONE', *, *, #45154, .T. ) ;
#14247 = CARTESIAN_POINT ( 'NONE',  ( 9.500000000000000000, -78.04999999999999716, 0.000000000000000000 ) ) ;
#14248 = CARTESIAN_POINT ( 'NONE',  ( -9.546819346421999697, -24.68527546640000025, 8.130850183241999929 ) ) ;
#14249 = CARTESIAN_POINT ( 'NONE',  ( -2.309466437479000156, -77.58981958342698704, 10.97654204954999990 ) ) ;
#14250 = CARTESIAN_POINT ( 'NONE',  ( -9.871730464199000465, -79.77354899574598335, 4.797141237513000256 ) ) ;
#14251 = DIRECTION ( 'NONE',  ( 0.000000000000000000, 1.000000000000000000, 0.000000000000000000 ) ) ;
#14252 = EDGE_CURVE ( 'NONE', #30580, #7174, #4128, .T. ) ;
#14253 = FACE_OUTER_BOUND ( 'NONE', #36729, .T. ) ;
#14254 = CARTESIAN_POINT ( 'NONE',  ( -1.078940792280719041, -78.61703581007959940, -10.72803815209405087 ) ) ;
#14255 = CARTESIAN_POINT ( 'NONE',  ( -0.9999999970759999579, -75.20000000292399989, 7.199999982805000087 ) ) ;
#14256 = CARTESIAN_POINT ( 'NONE',  ( -3.891865087805000289, -83.26917953870899680, -1.503306748519000147 ) ) ;
#14257 = CARTESIAN_POINT ( 'NONE',  ( -1.500000000000000000, -79.50000000000000000, 0.000000000000000000 ) ) ;
#14258 = CYLINDRICAL_SURFACE ( 'NONE', #50995, 0.5000000000000004441 ) ;
#14259 = PRESENTATION_LAYER_ASSIGNMENT (  '', '', ( #48261 ) ) ;
#14260 = CARTESIAN_POINT ( 'NONE',  ( -10.21813353151999948, -76.74205734789899225, 4.735332084273999875 ) ) ;
#14261 = CARTESIAN_POINT ( 'NONE',  ( -0.8033051684372000123, -80.35535114066999540, -1.459438184619000101 ) ) ;
#14262 = CARTESIAN_POINT ( 'NONE',  ( 0.1346575116716999809, -78.38684357976998740, 1.313219419913000063 ) ) ;
#14263 = DIRECTION ( 'NONE',  ( 0.000000000000000000, -1.000000000000000000, 0.000000000000000000 ) ) ;
#14264 = CARTESIAN_POINT ( 'NONE',  ( 1.501921250453331025, -81.50907291683472522, 0.1730332911310038246 ) ) ;
#14265 = CARTESIAN_POINT ( 'NONE',  ( 1.010008291100382483, -83.16719236129050330, 1.155447337432020438 ) ) ;
#14266 = CARTESIAN_POINT ( 'NONE',  ( -7.595992864760312102, -80.16301844581369096, -7.606389479688519195 ) ) ;
#14267 = CARTESIAN_POINT ( 'NONE',  ( -5.787029044103459974, -78.56271173619120418, 10.31969192858259099 ) ) ;
#14268 = EDGE_CURVE ( 'NONE', #10604, #33417, #47146, .T. ) ;
#14269 = ORIENTED_EDGE ( 'NONE', *, *, #22210, .T. ) ;
#14270 = CARTESIAN_POINT ( 'NONE',  ( -0.9597372295412756049, -81.65614046397973880, -0.8042208309310099335 ) ) ;
#14271 = EDGE_CURVE ( 'NONE', #31547, #9471, #11536, .T. ) ;
#14272 = SURFACE_STYLE_FILL_AREA ( #11040 ) ;
#14273 = CARTESIAN_POINT ( 'NONE',  ( -10.64923527428000050, -79.86726667242790256, 3.293689214829000012 ) ) ;
#14274 = ORIENTED_EDGE ( 'NONE', *, *, #37862, .F. ) ;
#14275 = ORIENTED_EDGE ( 'NONE', *, *, #34220, .T. ) ;
#14276 = CARTESIAN_POINT ( 'NONE',  ( -0.5537454541186001000, -82.14093423380400338, -1.341729424668000048 ) ) ;
#14277 = AXIS2_PLACEMENT_3D ( 'NONE', #31126, #16423, #12276 ) ;
#14278 = ORIENTED_EDGE ( 'NONE', *, *, #38507, .T. ) ;
#14279 = DIRECTION ( 'NONE',  ( -1.000000000000000000, 0.000000000000000000, 0.000000000000000000 ) ) ;
#14280 = EDGE_LOOP ( 'NONE', ( #52473, #32853, #53469, #10521 ) ) ;
#14281 = CONICAL_SURFACE ( 'NONE', #23684, 1.099999997149000430, 0.7853981633972997312 ) ;
#14282 = CARTESIAN_POINT ( 'NONE',  ( 1.048462055999483722, -80.39633018666535236, 0.6817341454441373516 ) ) ;
#14283 = CARTESIAN_POINT ( 'NONE',  ( 0.000000000000000000, -18.84999999999999787, 11.89999999977000122 ) ) ;
#14284 = CARTESIAN_POINT ( 'NONE',  ( -2.780564399470054404, -80.04895832527154198, 2.032809336423852198 ) ) ;
#14285 = ADVANCED_FACE ( 'NONE', ( #3250, #56402 ), #20385, .T. ) ;
#14286 = CARTESIAN_POINT ( 'NONE',  ( 2.287265073136303783, -78.24504505375756480, -8.963578713372259088 ) ) ;
#14287 = B_SPLINE_CURVE_WITH_KNOTS ( 'NONE', 3,
 ( #22456, #35428, #49337, #3866, #57886, #58180, #36030, #17442, #4455, #54056, #49038, #35733, #13591, #40166, #4160, #35141, #13298, #12720 ),
 .UNSPECIFIED., .F., .F.,
 ( 4, 2, 2, 2, 2, 2, 2, 2, 4 ),
 ( 0.000000000000000000, 0.1250000000000000555, 0.2500000000000001110, 0.3750000000000001665, 0.5000000000000002220, 0.6250000000000001110, 0.7500000000000001110, 0.8750000000000000000, 1.000000000000000000 ),
 .UNSPECIFIED. ) ;
#14288 = FACE_OUTER_BOUND ( 'NONE', #55749, .T. ) ;
#14289 = ORIENTED_EDGE ( 'NONE', *, *, #1014, .T. ) ;
#14290 = EDGE_LOOP ( 'NONE', ( #10097, #39817, #30380 ) ) ;
#14291 = DIRECTION ( 'NONE',  ( -0.9999548435846228323, 0.000000000000000000, -0.009503199022040218977 ) ) ;
#14292 = LINE ( 'NONE', #18162, #25369 ) ;
#14293 = CARTESIAN_POINT ( 'NONE',  ( 0.000000000000000000, -76.39999999999899671, 0.000000000000000000 ) ) ;
#14294 = CARTESIAN_POINT ( 'NONE',  ( 12.50000000000000000, -23.25000000000000000, 0.000000000000000000 ) ) ;
#14295 = CARTESIAN_POINT ( 'NONE',  ( 6.983565664416999219, -78.39846965846798810, -6.737990796766999857 ) ) ;
#14296 = CARTESIAN_POINT ( 'NONE',  ( -1.180685663403765906, -79.24320892454549892, -0.4090891148645076081 ) ) ;
#14297 = CARTESIAN_POINT ( 'NONE',  ( 2.344520508141321180, -85.88574262156167549, 3.128943653696025340 ) ) ;
#14298 = CARTESIAN_POINT ( 'NONE',  ( 12.49589899905999957, -77.14726523887000553, -3.422742383397000321 ) ) ;
#14299 = CARTESIAN_POINT ( 'NONE',  ( 0.7503380909894999951, -79.97566409777999752, 1.262315685543000221 ) ) ;
#14300 = CARTESIAN_POINT ( 'NONE',  ( -1.630052463839491317, -77.66104693750340004, -9.305255440227826469 ) ) ;
#14301 = CARTESIAN_POINT ( 'NONE',  ( -1.004305231718999991, -3.500000000000000000, 3.090933677959000203 ) ) ;
#14302 = CARTESIAN_POINT ( 'NONE',  ( -3.045010225283240501, -76.59478582781956391, 11.45375641726638705 ) ) ;
#14303 = CARTESIAN_POINT ( 'NONE',  ( 0.5574170278374001031, -79.09443340893348307, -4.135139127346999288 ) ) ;
#14304 = CARTESIAN_POINT ( 'NONE',  ( 1.618170588614999961, -80.40257597021090419, -11.14857479085000058 ) ) ;
#14305 = CARTESIAN_POINT ( 'NONE',  ( -0.8547114690830001082, -78.88883667140099476, 9.761549055228000427 ) ) ;
#14306 = DIRECTION ( 'NONE',  ( -0.9999548435846228323, 0.000000000000000000, -0.009503199022040218977 ) ) ;
#14307 = CARTESIAN_POINT ( 'NONE',  ( 3.383036395707000210, -82.48655496681199395, 0.3412503010523000313 ) ) ;
#14308 = CARTESIAN_POINT ( 'NONE',  ( 0.6849175148897999055, -77.93358067473459982, -1.144319635748999975 ) ) ;
#14309 = CARTESIAN_POINT ( 'NONE',  ( 0.000000000000000000, -4.000000000000000000, 0.000000000000000000 ) ) ;
#14310 = CARTESIAN_POINT ( 'NONE',  ( 4.000000000000000000, -75.00000000000001421, -0.5999999999999999778 ) ) ;
#14311 = CARTESIAN_POINT ( 'NONE',  ( -3.796701970596999764, -2.811752266991999871, 0.2667143827384000354 ) ) ;
#14312 = DIRECTION ( 'NONE',  ( 0.000000000000000000, -1.000000000000000000, 0.000000000000000000 ) ) ;
#14313 = ORIENTED_EDGE ( 'NONE', *, *, #9108, .T. ) ;
#14314 = CARTESIAN_POINT ( 'NONE',  ( -5.052420809101000088E-14, -80.89999999999999147, -13.99999999999777955 ) ) ;
#14315 = CARTESIAN_POINT ( 'NONE',  ( 8.111636311571439606, -60.31614597266276689, -7.429974109831698925 ) ) ;
#14316 = FACE_OUTER_BOUND ( 'NONE', #41868, .T. ) ;
#14317 = CARTESIAN_POINT ( 'NONE',  ( 8.467134758521000393, -79.12048981539898307, 4.837118142732999893 ) ) ;
#14318 = CONICAL_SURFACE ( 'NONE', #39762, 12.84999999993999964, 0.7853981633972997312 ) ;
#14319 = CARTESIAN_POINT ( 'NONE',  ( 1.750000000001000089, -18.74999999009000007, -12.56594317857000043 ) ) ;
#14320 = CARTESIAN_POINT ( 'NONE',  ( -8.940100391463808194, -79.55319689977089581, 5.969627096040645675 ) ) ;
#14321 = AXIS2_PLACEMENT_3D ( 'NONE', #57611, #54865, #45443 ) ;
#14322 = CARTESIAN_POINT ( 'NONE',  ( -11.00000000000000000, -78.69999999999998863, 0.000000000000000000 ) ) ;
#14323 = CARTESIAN_POINT ( 'NONE',  ( 9.724573642157064768, -78.49540306821776880, 6.592917362395923853 ) ) ;
#14324 = ORIENTED_EDGE ( 'NONE', *, *, #53342, .T. ) ;
#14325 = LINE ( 'NONE', #29072, #43872 ) ;
#14326 = CARTESIAN_POINT ( 'NONE',  ( -5.756396345943000092, -77.16116605027188768, 9.567080340993001641 ) ) ;
#14327 = B_SPLINE_CURVE_WITH_KNOTS ( 'NONE', 3,
 ( #51229, #24638, #19925, #6630, #14603, #32890, #5462, #2217, #6040, #20218, #37624, #19049, #37334, #37039, #37915, #45929, #50935, #42650 ),
 .UNSPECIFIED., .F., .F.,
 ( 4, 2, 2, 2, 2, 2, 2, 2, 4 ),
 ( 0.000000000000000000, 0.1250000000000000278, 0.2500000000000000555, 0.3750000000000000000, 0.5000000000000000000, 0.6250000000000000000, 0.7500000000000000000, 0.8750000000000001110, 1.000000000000000000 ),
 .UNSPECIFIED. ) ;
#14328 = CARTESIAN_POINT ( 'NONE',  ( -1.502550642848000217, -81.34707958231599889, 0.1060307108173999951 ) ) ;
#14329 = CARTESIAN_POINT ( 'NONE',  ( 7.668949790003000366, -22.77129148951999937, -10.21381326472000062 ) ) ;
#14331 = CARTESIAN_POINT ( 'NONE',  ( -0.4617212151683000032, -1.201502266992000134, 3.989551193614000013 ) ) ;
#14330 = CARTESIAN_POINT ( 'NONE',  ( 1.255787003026999971, -83.46042981021199125, -3.934655318183000183 ) ) ;
#14332 = CARTESIAN_POINT ( 'NONE',  ( 0.7681833999686413783, -82.32291666666665719, 0.9995835529977274980 ) ) ;
#14333 = CARTESIAN_POINT ( 'NONE',  ( 0.9995835529977264988, -82.69791666666664298, -0.7681833999686417114 ) ) ;
#14334 = CARTESIAN_POINT ( 'NONE',  ( -1.108343018679999847, -79.20368156769499990, -0.7155276831893999656 ) ) ;
#14335 = ORIENTED_EDGE ( 'NONE', *, *, #50760, .F. ) ;
#14336 = DIRECTION ( 'NONE',  ( 0.000000000000000000, -1.000000000000000000, 0.000000000000000000 ) ) ;
#14337 = LINE ( 'NONE', #9346, #32278 ) ;
#14338 = CARTESIAN_POINT ( 'NONE',  ( 3.914500761937001361, -78.91452044229970397, 7.829001523874034696 ) ) ;
#14339 = ORIENTED_EDGE ( 'NONE', *, *, #44361, .T. ) ;
#14340 = ORIENTED_EDGE ( 'NONE', *, *, #37078, .F. ) ;
#14341 = FACE_BOUND ( 'NONE', #22309, .T. ) ;
#14342 = CARTESIAN_POINT ( 'NONE',  ( 0.000000000000000000, -77.50000000000000000, -2.299999999999999822 ) ) ;
#14343 = CARTESIAN_POINT ( 'NONE',  ( 0.000000000000000000, -81.99999999999998579, 0.000000000000000000 ) ) ;
#14344 = ORIENTED_EDGE ( 'NONE', *, *, #33961, .T. ) ;
#14345 = CARTESIAN_POINT ( 'NONE',  ( 11.43454631689000145, -77.91559881290099554, -3.800910706745999956 ) ) ;
#14346 = EDGE_LOOP ( 'NONE', ( #55920, #52345, #38832, #28574, #51789 ) ) ;
#14347 = VERTEX_POINT ( 'NONE', #48135 ) ;
#14348 = CARTESIAN_POINT ( 'NONE',  ( -3.220112201118367157, -2.612390273010157138, -0.4917168695184507277 ) ) ;
#14349 = ORIENTED_EDGE ( 'NONE', *, *, #9108, .F. ) ;
#14350 = EDGE_CURVE ( 'NONE', #28435, #27557, #55639, .T. ) ;
#14351 = CARTESIAN_POINT ( 'NONE',  ( 1.570391623911302492, -76.53481037454862701, -11.99908637137544076 ) ) ;
#14352 = DIRECTION ( 'NONE',  ( 1.000000000000000000, 0.000000000000000000, 0.000000000000000000 ) ) ;
#14353 = VERTEX_POINT ( 'NONE', #34227 ) ;
#14354 = LINE ( 'NONE', #27640, #25239 ) ;
#14355 = EDGE_LOOP ( 'NONE', ( #22024, #2751, #36379, #41750 ) ) ;
#14356 = CARTESIAN_POINT ( 'NONE',  ( -8.082019532840464038, -79.14197076906785355, -4.658078629671525306 ) ) ;
#14357 = CARTESIAN_POINT ( 'NONE',  ( -0.5548702034695790486, -77.97035308862197667, -9.688443984839716805 ) ) ;
#14358 = AXIS2_PLACEMENT_3D ( 'NONE', #5585, #50191, #50778 ) ;
#14359 = CARTESIAN_POINT ( 'NONE',  ( -12.00000000000000000, -79.79999999999999716, 6.639246269807000381E-13 ) ) ;
#14360 = DIRECTION ( 'NONE',  ( -1.000000000000000000, 0.000000000000000000, 0.000000000000000000 ) ) ;
#14361 = CARTESIAN_POINT ( 'NONE',  ( 5.177752511601999785, -76.60280117385499921, 9.912858493839999952 ) ) ;
#14362 = LINE ( 'NONE', #10244, #49521 ) ;
#14363 = TOROIDAL_SURFACE ( 'NONE', #2134, 1.250000000000000000, 0.5000000000000000000 ) ;
#14364 = EDGE_CURVE ( 'NONE', #44478, #26509, #9792, .T. ) ;
#14365 = CARTESIAN_POINT ( 'NONE',  ( 1.552784181637999916, -76.45944931795999366, -11.12081786967999975 ) ) ;
#14366 = CARTESIAN_POINT ( 'NONE',  ( 8.412275655993779466, -78.81594285012758405, -3.858088829829057431 ) ) ;
#14367 = CARTESIAN_POINT ( 'NONE',  ( 3.747061555208543115, -76.54862165773606364, 11.14272879161189600 ) ) ;
#14368 = CARTESIAN_POINT ( 'NONE',  ( 5.225564025660000667, -77.83486167140100065, 7.798039823611999211 ) ) ;
#14369 = DIRECTION ( 'NONE',  ( -0.7071067811865474617, 0.000000000000000000, -0.7071067811865474617 ) ) ;
#14370 = CARTESIAN_POINT ( 'NONE',  ( -9.210028442906166291, -80.14621276956458473, -6.014467946005654042 ) ) ;
#14371 = CARTESIAN_POINT ( 'NONE',  ( 6.040704753788179282, -78.11963179743526098, -10.46256944259450883 ) ) ;
#14372 = CARTESIAN_POINT ( 'NONE',  ( -2.914365214892999933, -81.32367549782598815, 2.926598508534000054 ) ) ;
#14373 = AXIS2_PLACEMENT_3D ( 'NONE', #51619, #32987, #2313 ) ;
#14374 = CARTESIAN_POINT ( 'NONE',  ( -11.75000000000000000, -76.20000000000000284, -1.391479524197000231E-14 ) ) ;
#14375 = CARTESIAN_POINT ( 'NONE',  ( -1.192783596312423589, -83.07577989394255269, 0.3769634839055466813 ) ) ;
#14376 = CARTESIAN_POINT ( 'NONE',  ( 9.411694425802703989, -77.13749999999998863, -1.492218284488986191 ) ) ;
#14377 = DIRECTION ( 'NONE',  ( 0.000000000000000000, 1.000000000000000000, -7.105427357601000597E-14 ) ) ;
#14378 = B_SPLINE_SURFACE_WITH_KNOTS ( 'NONE', 3, 3, ( 
 ( #28525, #15250, #37974, #27651, #6393, #36804, #55998, #24408, #32076, #42126, #50408, #55702, #33243, #10841, #28817, #14365, #46866, #9957, #27938, #50117, #9661, #45693, #5232, #45986, #5512, #23522, #41533, #39430, #25845, #2844, #20841, #38267, #42710, #47735, #20560 ),
 ( #11995, #11710, #20273, #2559, #38558, #15545, #7269, #47452, #25270, #48024, #33541, #38845, #56288, #51865, #51580, #48306, #2275, #11137, #39136, #6977, #7558, #11418, #15839, #43873, #3140, #24980, #56863, #7845, #29399, #12275, #29973, #34109, #33827, #16422, #43002 ),
 ( #25557, #47159, #56574, #34406, #16132, #52152, #52435, #43577, #21129, #3422, #57147, #16711, #34693, #52723, #30264, #21422, #29113, #6689, #24698, #44738, #8715, #35564, #9016, #36164, #27295, #49765, #4289, #16998, #21992, #35266, #34978, #31717, #26136, #53008, #22587 ),
 ( #21706, #4589, #53894, #45036, #8135, #44436, #44157, #27001, #12561, #40000, #9305, #18171, #35865, #53298, #53590, #40600, #22288, #57437, #196, #30559, #3703, #54183, #58015, #12842, #45331, #49468, #13721, #3989, #17276, #4881, #22878, #8418, #17576, #48590, #39711 ) ),
 .UNSPECIFIED., .F., .F., .F.,
 ( 4, 4 ),
 ( 4, 1, 1, 1, 1, 1, 1, 1, 1, 1, 1, 1, 1, 1, 1, 1, 1, 1, 1, 1, 1, 1, 1, 1, 1, 1, 1, 1, 1, 1, 1, 1, 4 ),
 ( -0.1772706441294000235, 1.177270644128999955 ),
 ( -0.009208997693793000497, 0.005755623558620999794, 0.02072024481102999888, 0.03568486606345000478, 0.05064948731585999786, 0.06561410856827000482, 0.08057872982069000378, 0.09554335107309999686, 0.1105079723255000118, 0.1254725935778999990, 0.1404372148303000001, 0.1554018360827999767, 0.1703664573352000056, 0.1853310785876000066, 0.2002956998400000077, 0.2152603210924000088, 0.2302249423447999821, 0.2451895635972000109, 0.2601541848496000120, 0.2751188061020999887, 0.2900834273544999897, 0.3050480486068999908, 0.3200126698593000474, 0.3349772911116999929, 0.3499419123640999940, 0.3649065336164999951, 0.3798711548689999717, 0.3948357761214000283, 0.4098003973737999739, 0.4247650186261999750, 0.4397296398786000315, 0.4546942611309999771, 0.4696588823833999782 ),
 .UNSPECIFIED. ) ;
#14379 = VECTOR ( 'NONE', #23414, 1000.000000000000000 ) ;
#14380 = CARTESIAN_POINT ( 'NONE',  ( -3.237660394099999728, -1.425056440564000049, 1.969183889131999932 ) ) ;
#14381 = CARTESIAN_POINT ( 'NONE',  ( 10.38646360829999971, -59.57795407677000554, 7.655555357447999754 ) ) ;
#14382 = CARTESIAN_POINT ( 'NONE',  ( -1.576170184332999824, -24.16086967216000048, -12.55466896104999996 ) ) ;
#14383 = FACE_OUTER_BOUND ( 'NONE', #15158, .T. ) ;
#14384 = CARTESIAN_POINT ( 'NONE',  ( -0.8748660084214999744, -2.439568282128000032, 3.373992119635000009 ) ) ;
#14385 = CARTESIAN_POINT ( 'NONE',  ( -0.8537148449507000469, -54.09501854057999992, -12.43377424869000158 ) ) ;
#14386 = EDGE_CURVE ( 'NONE', #18069, #30361, #46222, .T. ) ;
#14387 = CARTESIAN_POINT ( 'NONE',  ( -0.1636246173744673738, -80.61458333333328596, -1.249999999999999778 ) ) ;
#14388 = CARTESIAN_POINT ( 'NONE',  ( 2.765208115035000080, -77.51648380221600121, -11.96450597650000169 ) ) ;
#14389 = CARTESIAN_POINT ( 'NONE',  ( 7.624341764923000753, -18.73514850530999709, 10.42531124853000080 ) ) ;
#14391 = CARTESIAN_POINT ( 'NONE',  ( 1.495190308928000089, -78.61595697280399975, 0.2516904690231000497 ) ) ;
#14390 = CARTESIAN_POINT ( 'NONE',  ( 1.310679582531385501, -79.69166666666669130, 0.7554284705563518720 ) ) ;
#14392 = CARTESIAN_POINT ( 'NONE',  ( -1.072796787723000023, -76.37353418688999795, -12.01405072592999979 ) ) ;
#14393 = ORIENTED_EDGE ( 'NONE', *, *, #18790, .T. ) ;
#14394 = CARTESIAN_POINT ( 'NONE',  ( 2.986994850445999994, -82.51432450217399150, -1.707899905183000167 ) ) ;
#14395 = CARTESIAN_POINT ( 'NONE',  ( -9.301394811601999990, -79.17722582056299530, -7.464576829628999377 ) ) ;
#14396 = CARTESIAN_POINT ( 'NONE',  ( 10.60070852584000001, -80.43093146505920288, -3.881634873714000289 ) ) ;
#14397 = CARTESIAN_POINT ( 'NONE',  ( 9.168564808419466416, -78.33948019894700110, -1.229073866473058718 ) ) ;
#14398 = CARTESIAN_POINT ( 'NONE',  ( 3.409064975549345178, -85.48333334097100078, 0.4838537520227722544 ) ) ;
#14399 = CARTESIAN_POINT ( 'NONE',  ( 2.976864594307000011, -77.54805815623998910, -10.81463766284999828 ) ) ;
#14400 = CARTESIAN_POINT ( 'NONE',  ( 10.11462613662204646, -23.38712935484991107, -7.639894945624773115 ) ) ;
#14401 = CARTESIAN_POINT ( 'NONE',  ( -3.250000000000000000, -1.500000000000000000, 0.000000000000000000 ) ) ;
#14402 = CARTESIAN_POINT ( 'NONE',  ( 3.373947135798999852, -1.509678536415000050, -2.197671934948000061 ) ) ;
#14403 = CARTESIAN_POINT ( 'NONE',  ( 9.711109801449000045, -79.03601937949099465, 1.878356537329999965 ) ) ;
#14404 = DIRECTION ( 'NONE',  ( 1.000000000000000000, 0.000000000000000000, 0.000000000000000000 ) ) ;
#14405 = VERTEX_POINT ( 'NONE', #43977 ) ;
#14406 = CARTESIAN_POINT ( 'NONE',  ( -1.811016405462518852, -54.73826444593738216, -12.71771640060642206 ) ) ;
#14407 = CARTESIAN_POINT ( 'NONE',  ( 4.117154990835999229, -79.41762000473400462, -8.556557796581000019 ) ) ;
#14408 = CARTESIAN_POINT ( 'NONE',  ( 9.499693205731109202, -80.00008708754018016, -1.997583897032410100E-06 ) ) ;
#14409 = ORIENTED_EDGE ( 'NONE', *, *, #31239, .T. ) ;
#14410 = AXIS2_PLACEMENT_3D ( 'NONE', #44784, #4337, #50104 ) ;
#14411 = CYLINDRICAL_SURFACE ( 'NONE', #41583, 10.20000000000000107 ) ;
#14412 = CARTESIAN_POINT ( 'NONE',  ( 0.000000000000000000, -74.70999999999999375, 0.000000000000000000 ) ) ;
#14413 = ORIENTED_EDGE ( 'NONE', *, *, #90, .F. ) ;
#14414 = CARTESIAN_POINT ( 'NONE',  ( 5.675825126306000001, -79.16335487410098892, 10.88946240266999865 ) ) ;
#14415 = CARTESIAN_POINT ( 'NONE',  ( 10.74143315901999962, -78.16829362456198282, -1.466515226187000032 ) ) ;
#14416 = CARTESIAN_POINT ( 'NONE',  ( 7.958763982157000427, -54.32301960771999916, 9.723170657500999070 ) ) ;
#14417 = EDGE_LOOP ( 'NONE', ( #56960, #18388, #44000, #51757 ) ) ;
#14418 = ORIENTED_EDGE ( 'NONE', *, *, #48488, .F. ) ;
#14419 = AXIS2_PLACEMENT_3D ( 'NONE', #53368, #13510, #44228 ) ;
#14420 = CARTESIAN_POINT ( 'NONE',  ( 12.50386483992548570, -24.78505343634600777, -0.8574420492259948734 ) ) ;
#14421 = CIRCLE ( 'NONE', #49336, 11.70000000000000107 ) ;
#14422 = EDGE_CURVE ( 'NONE', #9344, #54221, #32018, .T. ) ;
#14423 = PRESENTATION_STYLE_ASSIGNMENT (( #4994 ) ) ;
#14424 = CARTESIAN_POINT ( 'NONE',  ( 9.647254834573999460, -80.12796490456099718, -1.526580663425000095 ) ) ;
#14425 = ORIENTED_EDGE ( 'NONE', *, *, #24530, .T. ) ;
#14426 = FACE_OUTER_BOUND ( 'NONE', #22515, .T. ) ;
#14427 = LINE ( 'NONE', #18586, #20206 ) ;
#14428 = ADVANCED_FACE ( 'NONE', ( #35983 ), #49813, .F. ) ;
#14429 = CARTESIAN_POINT ( 'NONE',  ( -12.77302471391999994, -24.72230123305000049, -1.481949986259999852 ) ) ;
#14430 = CARTESIAN_POINT ( 'NONE',  ( -9.204193785523999694, -77.08969805011498977, -2.332437886131999871 ) ) ;
#14431 = CARTESIAN_POINT ( 'NONE',  ( -0.7033595694237251283, -80.17773795642190748, -1.034965556745985893 ) ) ;
#14432 = CARTESIAN_POINT ( 'NONE',  ( 0.8544064497059326024, -77.86067708349810346, -1.110392862171576622 ) ) ;
#14433 = CARTESIAN_POINT ( 'NONE',  ( -3.851650068366999857, -78.43735716283408976, 2.793213950329999913E-10 ) ) ;
#14434 = FACE_OUTER_BOUND ( 'NONE', #34841, .T. ) ;
#14435 = EDGE_CURVE ( 'NONE', #11113, #50856, #1340, .T. ) ;
#14436 = CARTESIAN_POINT ( 'NONE',  ( 0.2063409356571887232, -78.21362681902969882, 1.524325540200904827 ) ) ;
#14437 = CARTESIAN_POINT ( 'NONE',  ( -3.990537183407945498, -80.24166666280596871, -0.6977800654927414081 ) ) ;
#14438 = EDGE_LOOP ( 'NONE', ( #44258, #48580, #29276, #48914, #49489 ) ) ;
#14439 = CARTESIAN_POINT ( 'NONE',  ( 0.000000000000000000, 4.040000000000000036, 0.000000000000000000 ) ) ;
#14440 = CARTESIAN_POINT ( 'NONE',  ( 12.02702378446000075, -75.68921984486000554, -1.341316611471999876 ) ) ;
#14441 = CARTESIAN_POINT ( 'NONE',  ( -1.407171709420418138, -77.61458333333330017, -10.75000000000000000 ) ) ;
#14442 = AXIS2_PLACEMENT_3D ( 'NONE', #6632, #38209, #43517 ) ;
#14443 = CARTESIAN_POINT ( 'NONE',  ( -2.546061316244721873, -2.288581701949032876, 2.429709843700893490 ) ) ;
#14444 = DIRECTION ( 'NONE',  ( 0.000000000000000000, 1.000000000000000000, 0.000000000000000000 ) ) ;
#14445 = CARTESIAN_POINT ( 'NONE',  ( -10.39285214024000048, -78.43813172011999768, 6.510605926401999533 ) ) ;
#14446 = CARTESIAN_POINT ( 'NONE',  ( -8.987350104473000201, -77.14201387919399622, 8.369597699504998545 ) ) ;
#14447 = CARTESIAN_POINT ( 'NONE',  ( 0.000000000000000000, -74.70999999999999375, 0.000000000000000000 ) ) ;
#14448 = CARTESIAN_POINT ( 'NONE',  ( -10.74684349920000059, -80.03966949086598959, 2.363312785431999963 ) ) ;
#14449 = CARTESIAN_POINT ( 'NONE',  ( 10.11462613664634347, -60.18712935448241552, -7.639894945646048541 ) ) ;
#14450 = CARTESIAN_POINT ( 'NONE',  ( 7.572826708286753750, -77.22926875571705807, -9.331956626295818680 ) ) ;
#14451 = CARTESIAN_POINT ( 'NONE',  ( 11.21665020278000036, -78.50049515372108999, 0.06973997782872000395 ) ) ;
#14452 = TOROIDAL_SURFACE ( 'NONE', #10683, 17.50000000000000000, 5.000000000000000000 ) ;
#14453 = B_SPLINE_SURFACE_WITH_KNOTS ( 'NONE', 3, 3, ( 
 ( #5655, #1542, #41676, #1257, #14800, #55545, #15096, #32794, #10388, #5948, #19534, #43421, #43142, #44281, #35399, #25405, #17126, #30108, #34539, #21838, #25118, #8267, #16271, #56714, #3273, #47872, #48723, #44002, #3840, #3552, #52572, #57282, #39271, #21265, #57564 ),
 ( #35109, #53430, #7978, #48436, #39843, #12693, #57858, #11841, #48159, #2701, #29822, #30686, #39560, #26268, #34250, #7690, #7402, #12973, #20695, #25691, #7118, #38694, #25975, #2981, #43720, #20979, #12410, #38983, #56994, #16556, #16846, #34828, #52856, #30400, #41319 ),
 ( #18602, #35704, #36591, #619, #13863, #49305, #18307, #36880, #329, #36300, #40738, #9154, #41028, #9734, #903, #23311, #54323, #49008, #54027, #31859, #8856, #30971, #49900, #27723, #9445, #53733, #14150, #5012, #8556, #27435, #31559, #4727, #26846, #23017, #54612 ),
 ( #45470, #31263, #44574, #54892, #32150, #18884, #50189, #26548, #45767, #5301, #4130, #22129, #40140, #17720, #44876, #58153, #22725, #4429, #22429, #40442, #27138, #45177, #31, #18011, #36003, #13569, #49607, #10617, #33612, #51069, #15616, #42781, #33022, #28598, #32726 ) ),
 .UNSPECIFIED., .F., .F., .F.,
 ( 4, 4 ),
 ( 4, 1, 1, 1, 1, 1, 1, 1, 1, 1, 1, 1, 1, 1, 1, 1, 1, 1, 1, 1, 1, 1, 1, 1, 1, 1, 1, 1, 1, 1, 1, 1, 4 ),
 ( -0.05371687727926999917, 1.053716877278999986 ),
 ( -0.02000000000000000042, 0.01250000000000000069, 0.04499999999999999833, 0.07749999999999999944, 0.1100000000000000006, 0.1424999999999999878, 0.1749999999999999889, 0.2074999999999999900, 0.2399999999999999911, 0.2725000000000000200, 0.3049999999999999933, 0.3375000000000000222, 0.3699999999999999956, 0.4025000000000000244, 0.4349999999999999978, 0.4675000000000000266, 0.5000000000000000000, 0.5324999999999999734, 0.5649999999999999467, 0.5975000000000000311, 0.6300000000000000044, 0.6624999999999999778, 0.6949999999999999512, 0.7275000000000000355, 0.7600000000000000089, 0.7924999999999999822, 0.8249999999999999556, 0.8575000000000000400, 0.8900000000000000133, 0.9224999999999999867, 0.9549999999999999600, 0.9875000000000000444, 1.020000000000000018 ),
 .UNSPECIFIED. ) ;
#14454 = B_SPLINE_CURVE_WITH_KNOTS ( 'NONE', 3,
 ( #26765, #53351, #9072, #27059, #17052, #48932, #26470, #12616, #53952, #40056, #250, #30898, #8191, #13778, #3760, #49822, #27357, #36222 ),
 .UNSPECIFIED., .F., .F.,
 ( 4, 2, 2, 2, 2, 2, 2, 2, 4 ),
 ( 0.000000000000000000, 0.06250000000000160982, 0.1250000000000032196, 0.2500000000000014433, 0.4999999999999981126, 0.7499999999999947820, 0.8124999999999947820, 0.8749999999999948930, 1.000000000000000000 ),
 .UNSPECIFIED. ) ;
#14455 = ORIENTED_EDGE ( 'NONE', *, *, #51935, .T. ) ;
#14456 = CARTESIAN_POINT ( 'NONE',  ( -1.479613214588597625, -81.26615285871807259, -0.3067698822034324313 ) ) ;
#14457 = CARTESIAN_POINT ( 'NONE',  ( 1.249910393070341685, -78.83987707960370983, -0.1637800131244415147 ) ) ;
#14458 = CARTESIAN_POINT ( 'NONE',  ( 10.24999999991999999, -82.10000000007899246, -6.817370023903000320E-10 ) ) ;
#14459 = CARTESIAN_POINT ( 'NONE',  ( 0.000000000000000000, -74.70999999999999375, 0.000000000000000000 ) ) ;
#14460 = CARTESIAN_POINT ( 'NONE',  ( 7.644093100845071653, -23.52380578988460513, 10.09634101412665075 ) ) ;
#14461 = AXIS2_PLACEMENT_3D ( 'NONE', #9681, #19705, #28545 ) ;
#14462 = CARTESIAN_POINT ( 'NONE',  ( -9.926966510012999123, -77.52975978748899877, 6.625016102256999773 ) ) ;
#14463 = CARTESIAN_POINT ( 'NONE',  ( 9.062046460520999602, -77.42945172698098588, -3.260755114102000363 ) ) ;
#14464 = CARTESIAN_POINT ( 'NONE',  ( 7.257927454905483522, -76.02152169444083540, 9.258411468306171344 ) ) ;
#14465 = CARTESIAN_POINT ( 'NONE',  ( -8.917244775899000331, -79.00895807477898813, -6.494958043606000153 ) ) ;
#14466 = CARTESIAN_POINT ( 'NONE',  ( -3.165820273081872305, -85.94828564506399005, 1.338596575002511724 ) ) ;
#14467 = EDGE_LOOP ( 'NONE', ( #57382, #14858, #46854, #27186, #28, #35028 ) ) ;
#14468 = CONICAL_SURFACE ( 'NONE', #41827, 1.500000000188000060, 0.7853981633972997312 ) ;
#14469 = LINE ( 'NONE', #54916, #4043 ) ;
#14470 = CARTESIAN_POINT ( 'NONE',  ( 4.774672647477999909, -79.91637558193269797, -11.01515226630999855 ) ) ;
#14471 = DIRECTION ( 'NONE',  ( 0.000000000000000000, 1.000000000000000000, 0.000000000000000000 ) ) ;
#14472 = CARTESIAN_POINT ( 'NONE',  ( -10.57894479237893748, -76.18802083340513320, -2.843887423799716263 ) ) ;
#14473 = CARTESIAN_POINT ( 'NONE',  ( 1.439896632895302675, -79.23541666666665151, -11.00000000000000355 ) ) ;
#14474 = CARTESIAN_POINT ( 'NONE',  ( 0.000000000000000000, -81.19999999999998863, -8.000000000000000000 ) ) ;
#14475 = CARTESIAN_POINT ( 'NONE',  ( 0.000000000000000000, -55.54999999966999980, 12.50000000000000000 ) ) ;
#14476 = CARTESIAN_POINT ( 'NONE',  ( 8.252512830340000605, -17.06594982557999884, -9.650910120430999939 ) ) ;
#14477 = CARTESIAN_POINT ( 'NONE',  ( -7.714303428875997959, -52.49705297113997204, -12.53545825868000385 ) ) ;
#14478 = ORIENTED_EDGE ( 'NONE', *, *, #6294, .T. ) ;
#14479 = EDGE_CURVE ( 'NONE', #6792, #33386, #23866, .T. ) ;
#14480 = CARTESIAN_POINT ( 'NONE',  ( -10.69024338110999928, -78.73172173177698596, -3.158052726529999799 ) ) ;
#14481 = DIRECTION ( 'NONE',  ( -0.9999463328794432337, 0.000000000000000000, 0.01036008498777044214 ) ) ;
#14482 = DIRECTION ( 'NONE',  ( 0.000000000000000000, -3.446666965303000135E-11, -1.000000000000000000 ) ) ;
#14483 = CARTESIAN_POINT ( 'NONE',  ( -1.629962280006342690, -76.83873742058555933, 11.96830011435914365 ) ) ;
#14485 = CARTESIAN_POINT ( 'NONE',  ( 12.50000000000000000, -61.48359816765000119, 1.003641516062000250 ) ) ;
#14484 = CARTESIAN_POINT ( 'NONE',  ( 0.8380226388207999699, -80.97828694247898795, 1.018961948080000068 ) ) ;
#14486 = CARTESIAN_POINT ( 'NONE',  ( -1.823750004803999641E-14, -80.79999999999999716, 0.000000000000000000 ) ) ;
#14487 = CARTESIAN_POINT ( 'NONE',  ( 10.45205659047000069, -22.76232685227000019, 7.651160337221999619 ) ) ;
#14488 = PRODUCT_DEFINITION_SHAPE ( 'NONE', 'NONE',  #58410 ) ;
#14489 = CARTESIAN_POINT ( 'NONE',  ( 5.684557159767942736, -79.82291666666664298, 7.396918292183182864 ) ) ;
#14490 = CARTESIAN_POINT ( 'NONE',  ( 1.684399200443891909, -78.31284097919404985, 10.84576505037703953 ) ) ;
#14491 = VECTOR ( 'NONE', #1291, 1000.000000000000000 ) ;
#14492 = CARTESIAN_POINT ( 'NONE',  ( 0.000000000000000000, -62.90094976977999863, 0.000000000000000000 ) ) ;
#14493 = ORIENTED_EDGE ( 'NONE', *, *, #26277, .T. ) ;
#14494 = ORIENTED_EDGE ( 'NONE', *, *, #38573, .T. ) ;
#14495 = CARTESIAN_POINT ( 'NONE',  ( -0.6670706960860000034, -77.75963998579798897, 10.00022801703000042 ) ) ;
#14496 = CARTESIAN_POINT ( 'NONE',  ( 6.499026777884298056, -78.77679667229833171, -8.564691133015255531 ) ) ;
#14497 = ADVANCED_FACE ( 'NONE', ( #46041 ), #6587, .T. ) ;
#14498 = VERTEX_POINT ( 'NONE', #10014 ) ;
#14499 = CARTESIAN_POINT ( 'NONE',  ( 2.076475668830000121, -76.11013824524211202, 10.98918251355999942 ) ) ;
#14500 = CARTESIAN_POINT ( 'NONE',  ( 3.416150720453857481, -83.98020834565045334, 0.4395479122176694786 ) ) ;
#14501 = AXIS2_PLACEMENT_3D ( 'NONE', #49421, #26089, #8971 ) ;
#14502 = CARTESIAN_POINT ( 'NONE',  ( 10.53494356941000021, -60.02715052954999919, 7.618393677181999557 ) ) ;
#14503 = CARTESIAN_POINT ( 'NONE',  ( 9.211672236691230253, -76.85627983199107405, 7.998575932842224567 ) ) ;
#14504 = CARTESIAN_POINT ( 'NONE',  ( 2.697673772653688573, -77.69297794779137689, -11.67229829829229715 ) ) ;
#14505 = CARTESIAN_POINT ( 'NONE',  ( -6.324515969367999979, -78.84343660893600259, -9.263833350438000380 ) ) ;
#14506 = CARTESIAN_POINT ( 'NONE',  ( 1.787953089535764484, -1.772425210045708521, -2.745890603803126329 ) ) ;
#14507 = EDGE_CURVE ( 'NONE', #37067, #53695, #22998, .T. ) ;
#14508 = EDGE_LOOP ( 'NONE', ( #13336, #29308, #34033, #25292 ) ) ;
#14509 = CARTESIAN_POINT ( 'NONE',  ( 10.36935812844000004, -78.07876026662599145, -2.835297515976000327 ) ) ;
#14510 = ORIENTED_EDGE ( 'NONE', *, *, #10448, .F. ) ;
#14511 = CARTESIAN_POINT ( 'NONE',  ( 9.247895922801244950, -77.35175846627117835, 0.2043318676645352883 ) ) ;
#14512 = CARTESIAN_POINT ( 'NONE',  ( 9.391860901740999523, -77.22419567483399305, 5.803232400709999794 ) ) ;
#14513 = CARTESIAN_POINT ( 'NONE',  ( 1.310679582531385279, -77.79166666666667140, 0.7554284705563519831 ) ) ;
#14514 = CARTESIAN_POINT ( 'NONE',  ( -9.139898499914998808, -77.36662839264398883, 2.826942883852999966 ) ) ;
#14515 = CARTESIAN_POINT ( 'NONE',  ( -9.850513606030963487, -17.69492088480771841, -7.836738268704446675 ) ) ;
#14516 = CARTESIAN_POINT ( 'NONE',  ( -0.5440519240141012958, -2.111768684982749278, -3.229414189797041423 ) ) ;
#14517 = CARTESIAN_POINT ( 'NONE',  ( -1.491326706514000122, -77.80317096599999616, -0.6515838025032999470 ) ) ;
#14518 = CARTESIAN_POINT ( 'NONE',  ( -3.126658837318000206, -81.89157046129098205, -2.762344429551999880 ) ) ;
#14519 = CARTESIAN_POINT ( 'NONE',  ( 3.292343003156000147, -79.07851149742998587, -10.43303857396000112 ) ) ;
#14520 = CARTESIAN_POINT ( 'NONE',  ( -7.753906807039999904, -24.28933445982999828, -10.31979621049999807 ) ) ;
#14521 = CARTESIAN_POINT ( 'NONE',  ( 12.60413652829999975, -55.49283065365000311, -1.799502287743000029 ) ) ;
#14522 = CARTESIAN_POINT ( 'NONE',  ( -1.575900344810000187, -85.74518770028200265, 3.224971915196999994 ) ) ;
#14523 = ORIENTED_EDGE ( 'NONE', *, *, #25016, .F. ) ;
#14524 = CARTESIAN_POINT ( 'NONE',  ( -6.043427764450784778, -79.48333333333329165, -10.48543666025109822 ) ) ;
#14525 = CARTESIAN_POINT ( 'NONE',  ( 3.001482106993999643, -76.63078604711199660, 11.21790237008999824 ) ) ;
#14526 = CARTESIAN_POINT ( 'NONE',  ( 4.627417567202060766, -77.93975844766031003, 9.702993547770001115 ) ) ;
#14527 = CARTESIAN_POINT ( 'NONE',  ( -4.085659785884999451, -78.46880095406299915, 11.26159174134999930 ) ) ;
#14528 = CARTESIAN_POINT ( 'NONE',  ( -9.992014434680999813, -17.83915351714000153, 7.762970980311999725 ) ) ;
#14530 = LINE ( 'NONE', #27519, #33534 ) ;
#14529 = CARTESIAN_POINT ( 'NONE',  ( 5.917523019358082337, -78.46666666666666856, -10.26699006316252394 ) ) ;
#14531 = ADVANCED_FACE ( 'NONE', ( #1458 ), #49882, .F. ) ;
#14532 = CARTESIAN_POINT ( 'NONE',  ( 3.127772079701002017, -2.541048934001464144, 1.756767877748572459 ) ) ;
#14533 = CARTESIAN_POINT ( 'NONE',  ( 10.01235002620999914, -55.50151115525000023, -7.653559626076999578 ) ) ;
#14534 = CARTESIAN_POINT ( 'NONE',  ( -3.140027144888994037, -85.94828564506399005, 1.398030157552013319 ) ) ;
#14535 = CARTESIAN_POINT ( 'NONE',  ( 9.014158510551999015, -78.19118402616200569, 6.557403976990999972 ) ) ;
#14536 = DIRECTION ( 'NONE',  ( 0.000000000000000000, -1.000000000000000000, 0.000000000000000000 ) ) ;
#14537 = CARTESIAN_POINT ( 'NONE',  ( -1.784822011179000079, -80.34680229102650628, 10.88032703863999906 ) ) ;
#14538 = ORIENTED_EDGE ( 'NONE', *, *, #9493, .F. ) ;
#14539 = VECTOR ( 'NONE', #4487, 1000.000000000000000 ) ;
#14540 = CARTESIAN_POINT ( 'NONE',  ( -8.383077572658999443, -77.61109903538302035, 4.458862939031999595 ) ) ;
#14541 = CARTESIAN_POINT ( 'NONE',  ( -2.160078058180999960, -2.884790208251000188, -3.326435979223000050 ) ) ;
#14542 = CARTESIAN_POINT ( 'NONE',  ( 0.1392748842281999744, -77.07232906639299586, 11.21600254538999941 ) ) ;
#14543 = CARTESIAN_POINT ( 'NONE',  ( -0.6514878906251000412, -79.68927193274799947, 10.95625855609000077 ) ) ;
#14545 = CARTESIAN_POINT ( 'NONE',  ( 7.619389973898000434, -23.40786254230999930, -10.35398617733999949 ) ) ;
#14544 = B_SPLINE_CURVE_WITH_KNOTS ( 'NONE', 3,
 ( #52791, #9087, #35338, #27073, #26484, #48375, #26206, #7913, #8788, #34765, #21775, #13502, #58383, #17645, #35045, #53363, #26779, #48659 ),
 .UNSPECIFIED., .F., .F.,
 ( 4, 2, 2, 2, 2, 2, 2, 2, 4 ),
 ( 0.000000000000000000, 0.1250000000000000278, 0.2500000000000000555, 0.3750000000000001110, 0.5000000000000001110, 0.6250000000000001110, 0.7500000000000002220, 0.8750000000000002220, 1.000000000000000000 ),
 .UNSPECIFIED. ) ;
#14546 = CARTESIAN_POINT ( 'NONE',  ( -10.31401527466070256, -76.75508539453620926, 3.823154250450220282 ) ) ;
#14547 = PLANE ( 'NONE',  #2536 ) ;
#14548 = CARTESIAN_POINT ( 'NONE',  ( -8.803761571499403971, -53.58431590319399618, -9.164326402776838520 ) ) ;
#14549 = EDGE_CURVE ( 'NONE', #89, #41814, #36571, .T. ) ;
#14550 = CARTESIAN_POINT ( 'NONE',  ( 2.283273990875999804, -82.66792953870898941, 3.491867166086000118 ) ) ;
#14551 = CARTESIAN_POINT ( 'NONE',  ( -10.45205659047000069, -22.76232685227000019, -7.651160337221999619 ) ) ;
#14552 = EDGE_CURVE ( 'NONE', #12597, #37604, #14131, .T. ) ;
#14553 = CARTESIAN_POINT ( 'NONE',  ( -10.18847629493000007, -78.54730665117000399, -7.991150893161999669 ) ) ;
#14554 = CARTESIAN_POINT ( 'NONE',  ( 0.1398360057836000037, -77.15060249292598371, 11.26119045437999944 ) ) ;
#14555 = CARTESIAN_POINT ( 'NONE',  ( 1.617840321509000034, -79.98033874124999443, 0.3973055507782000118 ) ) ;
#14556 = CARTESIAN_POINT ( 'NONE',  ( -0.1405144323591999977, -77.90426997500999562, 1.241437707376999988 ) ) ;
#14557 = DIRECTION ( 'NONE',  ( 0.000000000000000000, 1.000000000000000000, -3.788597347406000047E-11 ) ) ;
#14558 = CARTESIAN_POINT ( 'NONE',  ( -1.118453976065381994, -81.69126296042138335, 1.015803637914979740 ) ) ;
#14559 = CARTESIAN_POINT ( 'NONE',  ( -13.89248034750000116, -32.39159251014999796, -2.632538494498000187E-05 ) ) ;
#14560 = DIRECTION ( 'NONE',  ( -1.590618475122999970E-12, 1.000000000000000000, 3.446049153258000297E-10 ) ) ;
#14561 = CARTESIAN_POINT ( 'NONE',  ( 1.194177587799142071, -79.82664734801842599, -0.3688301857723336186 ) ) ;
#14562 = ORIENTED_EDGE ( 'NONE', *, *, #38137, .F. ) ;
#14563 = CARTESIAN_POINT ( 'NONE',  ( -0.8771444964703341007, -81.66363988412527419, -0.8900962782329024936 ) ) ;
#14564 = DIRECTION ( 'NONE',  ( 1.000000000000000000, 0.000000000000000000, 0.000000000000000000 ) ) ;
#14565 = CARTESIAN_POINT ( 'NONE',  ( 2.301467643382999917, -78.53268586533900475, -10.90676452780999917 ) ) ;
#14566 = CIRCLE ( 'NONE', #24012, 1.250000000000000000 ) ;
#14567 = FACE_OUTER_BOUND ( 'NONE', #8657, .T. ) ;
#14568 = ORIENTED_EDGE ( 'NONE', *, *, #10939, .T. ) ;
#14569 = VERTEX_POINT ( 'NONE', #9426 ) ;
#14570 = CARTESIAN_POINT ( 'NONE',  ( -0.8036425357743999243, -80.96676881378600399, 1.285729672962000025 ) ) ;
#14571 = EDGE_LOOP ( 'NONE', ( #19595, #20540, #18736, #19544 ) ) ;
#14572 = EDGE_LOOP ( 'NONE', ( #42540, #11296, #16521, #14782, #6072 ) ) ;
#14573 = CARTESIAN_POINT ( 'NONE',  ( -1.499999999985999866, -82.00000000001401190, -1.019196462549000076E-10 ) ) ;
#14574 = CARTESIAN_POINT ( 'NONE',  ( -10.03847181063980365, -55.00634590446541949, -7.678636148863311917 ) ) ;
#14575 = APPLICATION_PROTOCOL_DEFINITION ( 'draft international standard', 'automotive_design', 1998, #36048 ) ;
#14576 = CARTESIAN_POINT ( 'NONE',  ( 3.177654278060972448, -79.35520832797827495, -1.327594666548604252 ) ) ;
#14577 = CARTESIAN_POINT ( 'NONE',  ( -3.442307367123000450, -78.72356001420199334, 9.412654989800000038 ) ) ;
#14578 = AXIS2_PLACEMENT_3D ( 'NONE', #27550, #50603, #27841 ) ;
#14579 = CARTESIAN_POINT ( 'NONE',  ( 5.968579026041624047, -78.28091924325941875, -7.066778786571805249 ) ) ;
#14580 = LINE ( 'NONE', #19318, #40443 ) ;
#14581 = EDGE_CURVE ( 'NONE', #36091, #19028, #45672, .T. ) ;
#14582 = ORIENTED_EDGE ( 'NONE', *, *, #35938, .T. ) ;
#14583 = ORIENTED_EDGE ( 'NONE', *, *, #8897, .T. ) ;
#14584 = CARTESIAN_POINT ( 'NONE',  ( -8.777663923591063622, -77.57446822344188320, 2.920505049390259344 ) ) ;
#14585 = CARTESIAN_POINT ( 'NONE',  ( 0.000000000000000000, -92.79999999999999716, 0.000000000000000000 ) ) ;
#14586 = CARTESIAN_POINT ( 'NONE',  ( -1.310679582531389498, -79.45833333333332860, 0.7554284705563444335 ) ) ;
#14587 = EDGE_CURVE ( 'NONE', #11048, #8218, #8996, .T. ) ;
#14588 = CARTESIAN_POINT ( 'NONE',  ( 1.931736162949456714, -60.56670395682250074, -12.72978979893091100 ) ) ;
#14589 = CARTESIAN_POINT ( 'NONE',  ( 7.658860137760000519, -78.57246790065498487, 5.959242465009999989 ) ) ;
#14590 = CARTESIAN_POINT ( 'NONE',  ( -1.180685663403765906, -79.20987559121225274, -0.4090891148645076081 ) ) ;
#14591 = CARTESIAN_POINT ( 'NONE',  ( 2.336986715456273789, -85.88603725345878104, 3.134951688163078121 ) ) ;
#14592 = CARTESIAN_POINT ( 'NONE',  ( 6.777770385731999525, -76.50513797953000505, -9.662258766526001352 ) ) ;
#14593 = CARTESIAN_POINT ( 'NONE',  ( -0.6709475781581999421, -80.79689136786998915, -1.436741477991000160 ) ) ;
#14594 = CARTESIAN_POINT ( 'NONE',  ( -12.83044027760000105, -23.30639784948999704, -2.062670899361999766 ) ) ;
#14595 = CARTESIAN_POINT ( 'NONE',  ( -8.645873396781713183, -76.64070860396672913, 7.966348362312300146 ) ) ;
#14596 = CARTESIAN_POINT ( 'NONE',  ( -3.126997180111000141, -81.86019317200199907, -2.762599942562999900 ) ) ;
#14597 = CARTESIAN_POINT ( 'NONE',  ( -7.960542989054001595, -80.70355283024726134, 7.971132368775000643 ) ) ;
#14598 = CARTESIAN_POINT ( 'NONE',  ( -9.565996717342001077, -79.08326001420199702, -1.527434585433000036 ) ) ;
#14599 = CARTESIAN_POINT ( 'NONE',  ( -1.750000000001000089, -23.25000000990999993, -12.56594317857000043 ) ) ;
#14600 = CARTESIAN_POINT ( 'NONE',  ( 2.112107237196000131, -79.24607046129089838, -2.850184828360999845 ) ) ;
#14601 = CARTESIAN_POINT ( 'NONE',  ( -0.8668440880359000733, -77.79058141039379848, -1.013523202003999923 ) ) ;
#14602 = EDGE_CURVE ( 'NONE', #40041, #43983, #48351, .T. ) ;
#14603 = CARTESIAN_POINT ( 'NONE',  ( -9.596002108778193929, -78.34791666666664867, 7.374560639698937159 ) ) ;
#14604 = LINE ( 'NONE', #28468, #32587 ) ;
#14605 = CARTESIAN_POINT ( 'NONE',  ( 2.113064247614999669, -3.523836441412999676, -3.165785623842000351 ) ) ;
#14606 = CARTESIAN_POINT ( 'NONE',  ( 0.000000000000000000, -60.04999999966999980, 12.50000000000000000 ) ) ;
#14607 = EDGE_LOOP ( 'NONE', ( #47260, #34229, #50775 ) ) ;
#14608 = CARTESIAN_POINT ( 'NONE',  ( 1.230457122658317193, -78.93333333333330870, -11.74999999999977263 ) ) ;
#14609 = CARTESIAN_POINT ( 'NONE',  ( 7.434020715870190088, -60.31691643837059047, -8.107762507646533834 ) ) ;
#14610 = CARTESIAN_POINT ( 'NONE',  ( 9.393805349124416892, -77.49942542969233727, 7.217729611353487229 ) ) ;
#14611 = AXIS2_PLACEMENT_3D ( 'NONE', #6645, #15504, #50367 ) ;
#14612 = VECTOR ( 'NONE', #25995, 1000.000000000000000 ) ;
#14613 = CARTESIAN_POINT ( 'NONE',  ( -1.494867482892000110, -79.44193905623698981, -9.636143388403000998 ) ) ;
#14614 = DIRECTION ( 'NONE',  ( 0.000000000000000000, 1.000000000000000000, 0.000000000000000000 ) ) ;
#14615 = CARTESIAN_POINT ( 'NONE',  ( -0.01336421990532181761, -79.47521759444254030, 10.74992168017122651 ) ) ;
#14616 = CARTESIAN_POINT ( 'NONE',  ( 6.678307047331999868, -79.06363998579800523, -7.238412584370999880 ) ) ;
#14617 = ADVANCED_FACE ( 'NONE', ( #31991 ), #45608, .F. ) ;
#14618 = AXIS2_PLACEMENT_3D ( 'NONE', #4265, #41152, #45006 ) ;
#14619 = LINE ( 'NONE', #42664, #25932 ) ;
#14620 = CARTESIAN_POINT ( 'NONE',  ( 11.02299141721000098, -77.92552186078398790, -0.5079658554739000520 ) ) ;
#14621 = CARTESIAN_POINT ( 'NONE',  ( -0.8185753169346000613, -81.82567404918501097, 1.379521242779999879 ) ) ;
#14622 = DIRECTION ( 'NONE',  ( 0.000000000000000000, 1.000000000000000000, 0.000000000000000000 ) ) ;
#14623 = CARTESIAN_POINT ( 'NONE',  ( 2.781615572646999990, -78.16968490469898256, -8.992986673707997980 ) ) ;
#14625 = CARTESIAN_POINT ( 'NONE',  ( -3.399186938124999724, -80.19999999999998863, -10.46162167925000119 ) ) ;
#14624 = CARTESIAN_POINT ( 'NONE',  ( 1.224557693228000010, -83.94529094328899532, 3.769144257100999873 ) ) ;
#14626 = CARTESIAN_POINT ( 'NONE',  ( -8.650571159592999493, -79.65525584965399730, 4.057379972786000266 ) ) ;
#14627 = DIRECTION ( 'NONE',  ( 0.000000000000000000, 0.000000000000000000, -1.000000000000000000 ) ) ;
#14628 = DIRECTION ( 'NONE',  ( -0.7071067811865474617, 0.000000000000000000, 0.7071067811865474617 ) ) ;
#14629 = CARTESIAN_POINT ( 'NONE',  ( -12.80000000000000071, -6.000000000000000000, 0.000000000000000000 ) ) ;
#14630 = DIRECTION ( 'NONE',  ( 0.000000000000000000, -1.000000000000000000, 0.000000000000000000 ) ) ;
#14631 = CARTESIAN_POINT ( 'NONE',  ( 3.914500761937000028, -78.91452044229970397, -4.793880828366022505E-16 ) ) ;
#14632 = ORIENTED_EDGE ( 'NONE', *, *, #35515, .T. ) ;
#14633 = CARTESIAN_POINT ( 'NONE',  ( -3.970056213021999625, -79.10344746201099042, 11.35542513096999961 ) ) ;
#14634 = CARTESIAN_POINT ( 'NONE',  ( -12.50000000000000000, -61.48359816765000119, -1.003641516062000250 ) ) ;
#14635 = FACE_OUTER_BOUND ( 'NONE', #34315, .T. ) ;
#14636 = VERTEX_POINT ( 'NONE', #32277 ) ;
#14637 = CARTESIAN_POINT ( 'NONE',  ( 4.881373948557000020, -78.28194079526799953, -10.89071580847000220 ) ) ;
#14638 = ORIENTED_EDGE ( 'NONE', *, *, #23512, .F. ) ;
#14639 = ORIENTED_EDGE ( 'NONE', *, *, #17980, .F. ) ;
#14640 = VERTEX_POINT ( 'NONE', #176 ) ;
#14641 = CARTESIAN_POINT ( 'NONE',  ( 2.185988871226999475, -82.21467895096598966, -2.793952356700000195 ) ) ;
#14642 = CARTESIAN_POINT ( 'NONE',  ( 1.250000000000000000, -23.25000000000000000, -12.00000000000000000 ) ) ;
#14643 = VECTOR ( 'NONE', #15118, 1000.000000000000000 ) ;
#14644 = ORIENTED_EDGE ( 'NONE', *, *, #28325, .T. ) ;
#14645 = CARTESIAN_POINT ( 'NONE',  ( 0.000000000000000000, -81.99999999999998579, 7.000000000000000000 ) ) ;
#14646 = ORIENTED_EDGE ( 'NONE', *, *, #42170, .T. ) ;
#14647 = CARTESIAN_POINT ( 'NONE',  ( -1.250000000000000000, -79.59999999999999432, 0.000000000000000000 ) ) ;
#14648 = CIRCLE ( 'NONE', #35360, 12.57042253521000141 ) ;
#14649 = CARTESIAN_POINT ( 'NONE',  ( -9.446590193405137725, -78.36828669642795830, -2.221657378611725964 ) ) ;
#14650 = CARTESIAN_POINT ( 'NONE',  ( 0.9597843051886902899, -79.79999999999998295, -11.74187349997137630 ) ) ;
#14651 = CARTESIAN_POINT ( 'NONE',  ( -10.75000000000000000, -80.09999999999999432, -1.711887504597999906E-14 ) ) ;
#14652 = CARTESIAN_POINT ( 'NONE',  ( 10.03482481951295391, -79.24652767382275442, 6.603860533736427563 ) ) ;
#14653 = CARTESIAN_POINT ( 'NONE',  ( -11.08400893143999966, -76.27673592799600044, -1.489506537590000068 ) ) ;
#14654 = CARTESIAN_POINT ( 'NONE',  ( -9.431008681915484360, -24.80059307780060252, 8.251849286025537467 ) ) ;
#14655 = CARTESIAN_POINT ( 'NONE',  ( -7.626500777253000685, -60.11584731951999316, -10.35747145894000099 ) ) ;
#14656 = CARTESIAN_POINT ( 'NONE',  ( 8.129070811701460286, -78.81050004387087426, -4.417681596447804893 ) ) ;
#14657 = CARTESIAN_POINT ( 'NONE',  ( 4.510718562000938903, -76.54328005551209912, 10.84945785253482065 ) ) ;
#14658 = CARTESIAN_POINT ( 'NONE',  ( 1.702514374278000009, -77.71013501420199532, -9.256252642129998875 ) ) ;
#14659 = CARTESIAN_POINT ( 'NONE',  ( -1.308081345731999967, -80.61872908778599367, 0.2599445073669000017 ) ) ;
#14660 = CARTESIAN_POINT ( 'NONE',  ( -10.20656157772921446, -80.13085429318095976, -4.103012457657285950 ) ) ;
#14661 = FACE_OUTER_BOUND ( 'NONE', #56770, .T. ) ;
#14662 = CARTESIAN_POINT ( 'NONE',  ( 3.909635449501999815, -80.60603455456799793, -0.6486381549911000022 ) ) ;
#14663 = CARTESIAN_POINT ( 'NONE',  ( -12.54715396801999994, -17.46815137273999952, 1.292200816715999956 ) ) ;
#14664 = EDGE_CURVE ( 'NONE', #26037, #13102, #54712, .T. ) ;
#14665 = CARTESIAN_POINT ( 'NONE',  ( 0.9973843665736694675, -82.90183089828425977, 0.7531913344093712492 ) ) ;
#14666 = FACE_OUTER_BOUND ( 'NONE', #13689, .T. ) ;
#14667 = DIRECTION ( 'NONE',  ( -0.7071067811864975017, -0.7071067811865974218, 1.156400220097994687E-08 ) ) ;
#14668 = CARTESIAN_POINT ( 'NONE',  ( -9.596002108778193929, -79.34791666666664867, 7.374560639698937159 ) ) ;
#14669 = CARTESIAN_POINT ( 'NONE',  ( -9.963467980718000661, -60.48274967040000405, -7.659239661670000032 ) ) ;
#14670 = LINE ( 'NONE', #35941, #33587 ) ;
#14671 = CARTESIAN_POINT ( 'NONE',  ( 12.71106812363992766, -24.25135172970251674, -1.717582538846509799 ) ) ;
#14672 = CARTESIAN_POINT ( 'NONE',  ( 0.5372315382144975393, -79.69542381488500382, 1.412885547448977652 ) ) ;
#14673 = FACE_OUTER_BOUND ( 'NONE', #8324, .T. ) ;
#14674 = CARTESIAN_POINT ( 'NONE',  ( 0.6744326473074000461, -2.684874118045999847, -3.419700858360999796 ) ) ;
#14675 = CARTESIAN_POINT ( 'NONE',  ( 12.54980660768000078, -25.04777352165000082, -0.05651102257795000139 ) ) ;
#14676 = CARTESIAN_POINT ( 'NONE',  ( 10.75026368982902625, -77.20550397114976704, 0.6886793354171069081 ) ) ;
#14677 = DIRECTION ( 'NONE',  ( 1.000000000000000000, 0.000000000000000000, 0.000000000000000000 ) ) ;
#14679 = CARTESIAN_POINT ( 'NONE',  ( -10.65673661723999999, -78.83077053430758951, 2.626400817186000047 ) ) ;
#14678 = DIRECTION ( 'NONE',  ( 1.000000000000000000, 0.000000000000000000, 0.000000000000000000 ) ) ;
#14680 = CARTESIAN_POINT ( 'NONE',  ( -11.87662555441000123, -76.76958523746999674, -2.105724559057000178 ) ) ;
#14681 = ORIENTED_EDGE ( 'NONE', *, *, #47821, .T. ) ;
#14682 = EDGE_CURVE ( 'NONE', #34093, #8523, #34879, .T. ) ;
#14683 = CARTESIAN_POINT ( 'NONE',  ( -2.548476486054999768, -83.71296544543099571, -3.035003859434000084 ) ) ;
#14684 = CARTESIAN_POINT ( 'NONE',  ( -11.04073130536000136, -80.15336828462439200, -1.710558420931999946 ) ) ;
#14685 = CARTESIAN_POINT ( 'NONE',  ( -7.648026766733999615, -18.74999999413999774, -10.12290050089000104 ) ) ;
#14686 = CARTESIAN_POINT ( 'NONE',  ( 12.77649732931999971, -62.10828417218999675, -0.06479631635404999035 ) ) ;
#14687 = CARTESIAN_POINT ( 'NONE',  ( 6.433795189870999742, -77.57529449924099652, -9.188274595716000803 ) ) ;
#14688 = CARTESIAN_POINT ( 'NONE',  ( 9.850507815892393992, -24.30508874547875919, -7.836744050302931974 ) ) ;
#14689 = CARTESIAN_POINT ( 'NONE',  ( -9.088317367618000020, -78.86622446787298202, 3.186800494491000002 ) ) ;
#14690 = DIRECTION ( 'NONE',  ( -1.000000000000000000, 0.000000000000000000, 0.000000000000000000 ) ) ;
#14691 = CARTESIAN_POINT ( 'NONE',  ( 3.485499217011999828, -78.91452042059380290, 0.000000000000000000 ) ) ;
#14692 = CARTESIAN_POINT ( 'NONE',  ( 8.991649895478447618, -80.99999999999998579, -6.337868273171067379 ) ) ;
#14693 = EDGE_LOOP ( 'NONE', ( #14246, #54042, #49956, #36203, #41297, #11281 ) ) ;
#14694 = CIRCLE ( 'NONE', #56312, 4.100000000000000533 ) ;
#14695 = CARTESIAN_POINT ( 'NONE',  ( 0.2584144827513251697, -53.57154603042778263, -12.70558781483102884 ) ) ;
#14696 = CARTESIAN_POINT ( 'NONE',  ( -7.960542989054001595, -80.63576427697100257, 7.971132368775000643 ) ) ;
#14697 = DIRECTION ( 'NONE',  ( 0.000000000000000000, 0.000000000000000000, -1.000000000000000000 ) ) ;
#14698 = ADVANCED_FACE ( 'NONE', ( #9872, #50032 ), #54160, .F. ) ;
#14699 = CIRCLE ( 'NONE', #20363, 14.00000000000000000 ) ;
#14700 = ORIENTED_EDGE ( 'NONE', *, *, #15421, .T. ) ;
#14701 = CARTESIAN_POINT ( 'NONE',  ( 1.460959015002474493, -78.62916666666664867, -0.3926218265389176953 ) ) ;
#14702 = EDGE_CURVE ( 'NONE', #245, #10285, #3780, .T. ) ;
#14703 = DIRECTION ( 'NONE',  ( 0.7071067811864980568, 0.7071067811865969777, -8.992977225616968835E-09 ) ) ;
#14704 = EDGE_LOOP ( 'NONE', ( #32808, #16049, #47723, #30880 ) ) ;
#14705 = CARTESIAN_POINT ( 'NONE',  ( -5.342744711435999605, -77.84767930019499715, -10.92875150845999954 ) ) ;
#14706 = CARTESIAN_POINT ( 'NONE',  ( 11.10788134493000179, -77.25391046760299218, 1.523724958095000082 ) ) ;
#14707 = CARTESIAN_POINT ( 'NONE',  ( 9.355938762769536510, -61.97483710998693596, -8.610912454485829315 ) ) ;
#14708 = ORIENTED_EDGE ( 'NONE', *, *, #40880, .F. ) ;
#14709 = CARTESIAN_POINT ( 'NONE',  ( -0.9751240804252407912, -80.54658200636069409, 0.7826983233412607710 ) ) ;
#14710 =( NAMED_UNIT ( * ) SI_UNIT ( $, .STERADIAN. ) SOLID_ANGLE_UNIT ( ) );
#14711 = CARTESIAN_POINT ( 'NONE',  ( -2.217000330786000450, -79.28367578985398723, 9.512392227823999846 ) ) ;
#14712 = ORIENTED_EDGE ( 'NONE', *, *, #54184, .F. ) ;
#14713 = CARTESIAN_POINT ( 'NONE',  ( 12.61271781517999990, -55.60306329017999616, 1.798333084008999938 ) ) ;
#14714 = CARTESIAN_POINT ( 'NONE',  ( 8.532660243322236937, -25.12798380540222709, -9.433531203469305737 ) ) ;
#14715 = VERTEX_POINT ( 'NONE', #22859 ) ;
#14716 = CARTESIAN_POINT ( 'NONE',  ( -12.66316452095000145, -25.17866137669000182, 0.04044945982123000078 ) ) ;
#14717 = ADVANCED_FACE ( 'NONE', ( #43917 ), #8278, .F. ) ;
#14718 = CARTESIAN_POINT ( 'NONE',  ( -2.712012240502000182, -77.52810194988499859, 9.099584490865000319 ) ) ;
#14719 = DIRECTION ( 'NONE',  ( 0.000000000000000000, -1.000000000000000000, 0.000000000000000000 ) ) ;
#14720 = CARTESIAN_POINT ( 'NONE',  ( 7.247844507162001015, -55.54999999966999980, 9.722718241315000398 ) ) ;
#14721 = CARTESIAN_POINT ( 'NONE',  ( -1.750000000000000000, -18.75000000310999937, -12.50000000000000000 ) ) ;
#14722 = CARTESIAN_POINT ( 'NONE',  ( -11.68767212001979061, -78.82083333333331154, -3.140974612311365988 ) ) ;
#14723 = CARTESIAN_POINT ( 'NONE',  ( 9.365691051289999791, -76.94004530392098218, 2.708750943512000298 ) ) ;
#14724 = CARTESIAN_POINT ( 'NONE',  ( -1.030512144556630316, -79.28444148747665565, 1.103585378104965375 ) ) ;
#14725 = CARTESIAN_POINT ( 'NONE',  ( -4.000000000000000000, -78.69999999915415856, 2.834003763004000336E-08 ) ) ;
#14726 = ORIENTED_EDGE ( 'NONE', *, *, #55099, .F. ) ;
#14727 = CARTESIAN_POINT ( 'NONE',  ( -11.91862232004000077, -75.99721375889998853, 3.079279237876999531 ) ) ;
#14728 = TOROIDAL_SURFACE ( 'NONE', #46806, 13.50000000000000000, 0.5000000000000000000 ) ;
#14729 = CARTESIAN_POINT ( 'NONE',  ( -3.505468337749547914, -2.356789511367288092, -0.3314898072761500725 ) ) ;
#14730 = CARTESIAN_POINT ( 'NONE',  ( -10.12290050255000118, -60.04999997790999799, 7.648026768390999486 ) ) ;
#14731 = CARTESIAN_POINT ( 'NONE',  ( -3.911342194028000208, -78.58183531049999715, -11.62327352135999980 ) ) ;
#14732 = CARTESIAN_POINT ( 'NONE',  ( -1.984586691443999795, -76.02233504275700682, 11.75553522549000007 ) ) ;
#14733 = VECTOR ( 'NONE', #29416, 1000.000000000000000 ) ;
#14734 = CARTESIAN_POINT ( 'NONE',  ( -3.241578942234993654, -85.83735717367099483, 1.443243930775013784 ) ) ;
#14735 = AXIS2_PLACEMENT_3D ( 'NONE', #31297, #46089, #54642 ) ;
#14736 = CARTESIAN_POINT ( 'NONE',  ( 0.000000000000000000, -76.19999999999998863, 0.000000000000000000 ) ) ;
#14737 = CARTESIAN_POINT ( 'NONE',  ( -6.768773376071942849, -78.12766118154397077, -9.992519656028999719 ) ) ;
#14738 = CARTESIAN_POINT ( 'NONE',  ( -11.04065564777999953, -79.23587641477011800, 1.980412446595999798 ) ) ;
#14739 = AXIS2_PLACEMENT_3D ( 'NONE', #49474, #53902, #777 ) ;
#14740 = ORIENTED_EDGE ( 'NONE', *, *, #24334, .F. ) ;
#14741 = CARTESIAN_POINT ( 'NONE',  ( 1.213634779058999857, -83.30620538201100089, 0.5941895605367999433 ) ) ;
#14742 = FACE_OUTER_BOUND ( 'NONE', #25037, .T. ) ;
#14743 = CARTESIAN_POINT ( 'NONE',  ( 7.610716808838798642, -23.52015489479942190, 10.41172350877303820 ) ) ;
#14744 = CARTESIAN_POINT ( 'NONE',  ( 11.75000000000000000, -77.04999999999999716, 0.000000000000000000 ) ) ;
#14745 = CARTESIAN_POINT ( 'NONE',  ( 1.930008848924000153, -2.712975590836000261, 3.173250220514999942 ) ) ;
#14746 = CARTESIAN_POINT ( 'NONE',  ( -8.196454039252000001, -78.57433465545000217, -8.832548491656998735 ) ) ;
#14747 = CARTESIAN_POINT ( 'NONE',  ( 6.193386186315999353, -78.02635213868897779, 7.375308638433999420 ) ) ;
#14748 = CARTESIAN_POINT ( 'NONE',  ( -9.758470251469047341, -76.15243675912641663, 6.544191908880855557 ) ) ;
#14749 = CARTESIAN_POINT ( 'NONE',  ( -3.250000000000000000, -3.500000000000000000, -1.188926645705999921E-13 ) ) ;
#14750 = CARTESIAN_POINT ( 'NONE',  ( 4.358902656273643039, -85.80681307243297340, 0.5003316865781948231 ) ) ;
#14751 = ORIENTED_EDGE ( 'NONE', *, *, #15451, .F. ) ;
#14752 = ADVANCED_FACE ( 'NONE', ( #15747 ), #6011, .F. ) ;
#14753 = CARTESIAN_POINT ( 'NONE',  ( 12.00000000000000000, -75.80000000000001137, -2.990830162875999918E-13 ) ) ;
#14754 = CARTESIAN_POINT ( 'NONE',  ( -8.876652416960000735, -79.81871893549168817, -8.305429993361000740 ) ) ;
#14755 = CARTESIAN_POINT ( 'NONE',  ( 10.43010923569933368, -79.22936352839808194, 6.024574312383253805 ) ) ;
#14756 = EDGE_CURVE ( 'NONE', #45960, #32054, #48481, .T. ) ;
#14757 = CARTESIAN_POINT ( 'NONE',  ( -10.26699006316252749, -76.84166666666664014, -5.917523019358070790 ) ) ;
#14758 = CARTESIAN_POINT ( 'NONE',  ( -4.277738290159001089, -79.08359478844498369, -10.10766895494000117 ) ) ;
#14759 = B_SPLINE_CURVE_WITH_KNOTS ( 'NONE', 3,
 ( #44385, #43826, #21940, #39950, #57966, #39385, #57390, #54430, #18120, #36115 ),
 .UNSPECIFIED., .F., .F.,
 ( 4, 2, 2, 2, 4 ),
 ( 0.000000000000000000, 0.2500000000000000555, 0.5000000000000001110, 0.7500000000000000000, 1.000000000000000000 ),
 .UNSPECIFIED. ) ;
#14760 = LINE ( 'NONE', #32757, #4414 ) ;
#14761 = LINE ( 'NONE', #54644, #15171 ) ;
#14762 = CARTESIAN_POINT ( 'NONE',  ( 8.588893914429998944, -16.86760216306999993, -9.317954958010000510 ) ) ;
#14763 = CARTESIAN_POINT ( 'NONE',  ( -12.50240681834000078, -24.68234730741999883, 1.005418943852999902 ) ) ;
#14764 = VERTEX_POINT ( 'NONE', #39621 ) ;
#14765 = LINE ( 'NONE', #19144, #7004 ) ;
#14766 = CARTESIAN_POINT ( 'NONE',  ( 12.70556836347999941, -16.77227722772000007, -1.774194455291999869E-09 ) ) ;
#14767 = CARTESIAN_POINT ( 'NONE',  ( 6.128871534568974155, -79.71851631894477919, -10.04897160984813453 ) ) ;
#14768 = CARTESIAN_POINT ( 'NONE',  ( -3.777881236680218358, -78.40681307243319509, -0.07122001971131411424 ) ) ;
#14769 = CARTESIAN_POINT ( 'NONE',  ( -12.22285758008880308, -77.44360420965402625, 1.403409555567897149 ) ) ;
#14770 = DIRECTION ( 'NONE',  ( 0.000000000000000000, 1.000000000000000000, 0.000000000000000000 ) ) ;
#14771 = EDGE_CURVE ( 'NONE', #18221, #15288, #18265, .T. ) ;
#14772 = CARTESIAN_POINT ( 'NONE',  ( -6.226806355049928854, -76.99999999999998579, -7.114065959849781073 ) ) ;
#14773 = CARTESIAN_POINT ( 'NONE',  ( 10.98449824368628391, -23.30634943316888652, -0.5845455749771567566 ) ) ;
#14774 = AXIS2_PLACEMENT_3D ( 'NONE', #45462, #40128, #5005 ) ;
#14775 = CARTESIAN_POINT ( 'NONE',  ( -1.239721164836000256, -79.18402316759998882, -0.6954227484140999005 ) ) ;
#14776 = CARTESIAN_POINT ( 'NONE',  ( -12.50412681318974251, -54.28010473027888594, -1.235016000149057325 ) ) ;
#14777 = CIRCLE ( 'NONE', #22326, 9.599999999999999645 ) ;
#14778 = CARTESIAN_POINT ( 'NONE',  ( 3.915560572087711577, -79.29607338083805246, 10.25359469989230732 ) ) ;
#14779 = CARTESIAN_POINT ( 'NONE',  ( -1.164828128805999992E-14, -72.75000000040999737, 0.000000000000000000 ) ) ;
#14780 = ORIENTED_EDGE ( 'NONE', *, *, #43056, .T. ) ;
#14781 = AXIS2_PLACEMENT_3D ( 'NONE', #46055, #58147, #6169 ) ;
#14782 = ORIENTED_EDGE ( 'NONE', *, *, #49164, .F. ) ;
#14783 = CARTESIAN_POINT ( 'NONE',  ( -9.896988620242000323, -78.89193998579798972, -1.580285165976000217 ) ) ;
#14784 = CARTESIAN_POINT ( 'NONE',  ( 5.997500730681496250, -78.77227202905815773, -8.921341173856349727 ) ) ;
#14785 = VECTOR ( 'NONE', #25892, 999.9999999999998863 ) ;
#14786 = ORIENTED_EDGE ( 'NONE', *, *, #18366, .F. ) ;
#14787 = ADVANCED_FACE ( 'NONE', ( #12753 ), #39046, .F. ) ;
#14788 = CYLINDRICAL_SURFACE ( 'NONE', #8589, 1.500000000000000000 ) ;
#14789 = CARTESIAN_POINT ( 'NONE',  ( -2.832192856027651917, -83.05520834853042800, 1.959254550120464566 ) ) ;
#14790 = CARTESIAN_POINT ( 'NONE',  ( -9.469866204336648607, -79.39351776117217696, 0.7547688023506700095 ) ) ;
#14791 = CARTESIAN_POINT ( 'NONE',  ( 7.658894224196000522, -60.00939395830999956, 10.01676912202999858 ) ) ;
#14792 = CARTESIAN_POINT ( 'NONE',  ( 12.12015523194605571, -76.29028875741708760, -1.390668883284736923 ) ) ;
#14793 = CARTESIAN_POINT ( 'NONE',  ( -9.964686285863574966, -77.50307273982538447, 6.650189363608897786 ) ) ;
#14794 = CARTESIAN_POINT ( 'NONE',  ( 9.453938376997999882, -79.06132735295099678, 6.036651369377000087 ) ) ;
#14795 = ORIENTED_EDGE ( 'NONE', *, *, #14042, .F. ) ;
#14796 = CYLINDRICAL_SURFACE ( 'NONE', #16190, 9.500000000000000000 ) ;
#14797 = ORIENTED_EDGE ( 'NONE', *, *, #5534, .F. ) ;
#14798 = B_SPLINE_CURVE_WITH_KNOTS ( 'NONE', 3,
 ( #15036, #5590, #55786, #6179, #10919, #18895, #50488, #33030, #41327, #10624, #50783, #24191, #28023, #33327, #19185, #10328, #15336, #42208, #46068, #51364, #1774, #23603, #19769, #37765, #46946, #6471, #55193, #24482, #911, #45085, #9357, #49810, #13766, #9646, #40942, #31470, #27634, #45971, #18506, #530, #32346, #36501, #36789, #9941, #27347, #32061, #53942, #58359, #27919, #45677, #49513, #45382, #50393, #13475, #54807, #14065, #18222, #44783, #22928, #9064, #5215, #54527, #58063, #23219, #17623, #26754, #41226, #40649, #27049, #5496, #50102, #14348, #4636, #17923 ),
 .UNSPECIFIED., .F., .F.,
 ( 4, 2, 2, 1, 1, 1, 2, 2, 2, 2, 1, 1, 2, 2, 2, 2, 2, 2, 2, 1, 1, 2, 2, 2, 2, 1, 1, 2, 2, 2, 2, 1, 1, 2, 2, 2, 2, 1, 1, 1, 2, 2, 2, 4 ),
 ( 0.000000000000000000, 0.06250000000000086042, 0.09375000000000129063, 0.1093750000000015266, 0.1171875000000015821, 0.1210937500000015543, 0.1230468750000015821, 0.1250000000000016098, 0.1875000000000031364, 0.2187500000000039135, 0.2343750000000043299, 0.2421875000000045519, 0.2460937500000047184, 0.2500000000000048850, 0.3125000000000050515, 0.3437500000000050515, 0.3593750000000051070, 0.3750000000000051625, 0.4375000000000052180, 0.4687500000000052736, 0.4843750000000052736, 0.4921875000000052736, 0.5000000000000052180, 0.5625000000000053291, 0.5937500000000054401, 0.6093750000000054401, 0.6171875000000054401, 0.6210937500000053291, 0.6250000000000052180, 0.6875000000000052180, 0.7187500000000053291, 0.7343750000000054401, 0.7421875000000054401, 0.7460937500000054401, 0.7500000000000053291, 0.8125000000000044409, 0.8437500000000039968, 0.8593750000000038858, 0.8671875000000037748, 0.8710937500000036637, 0.8730468750000036637, 0.8750000000000036637, 0.9375000000000018874, 1.000000000000000000 ),
 .UNSPECIFIED. ) ;
#14799 = CARTESIAN_POINT ( 'NONE',  ( 7.016739011427143957, -77.40660838192772530, 6.033546689316169775 ) ) ;
#14800 = CARTESIAN_POINT ( 'NONE',  ( 0.3256773761571999937, -79.38679175127299459, -1.278468177226000035 ) ) ;
#14801 = DIRECTION ( 'NONE',  ( 1.000000000000000000, 0.000000000000000000, 0.000000000000000000 ) ) ;
#14802 = ADVANCED_FACE ( 'NONE', ( #34605 ), #10233, .F. ) ;
#14803 = CARTESIAN_POINT ( 'NONE',  ( -1.163821121499999833, -78.55288933763399939, -1.119256147183999905 ) ) ;
#14804 = CARTESIAN_POINT ( 'NONE',  ( -6.043427764450784778, -77.48333333333332007, -10.48543666025109822 ) ) ;
#14805 = DIRECTION ( 'NONE',  ( 0.000000000000000000, 0.000000000000000000, -1.000000000000000000 ) ) ;
#14806 = CARTESIAN_POINT ( 'NONE',  ( 1.169626569868999821, -78.08157881489999852, 1.131652196797999999 ) ) ;
#14807 = CARTESIAN_POINT ( 'NONE',  ( 4.046592082650999345, -82.45273712795798815, -0.2667243773544999974 ) ) ;
#14808 = CARTESIAN_POINT ( 'NONE',  ( 10.90877671396000004, -78.68521853677198408, 0.8284967960653000230 ) ) ;
#14809 = CARTESIAN_POINT ( 'NONE',  ( -7.756281347471999155, -24.22006031113999569, -10.15825374573999973 ) ) ;
#14810 = CARTESIAN_POINT ( 'NONE',  ( 12.69616050746999925, -57.04828923575999511, -1.799475304559999822 ) ) ;
#14811 = CARTESIAN_POINT ( 'NONE',  ( 3.235517445292999561, -82.38490367749800214, -1.192293695388999986 ) ) ;
#14812 = ORIENTED_EDGE ( 'NONE', *, *, #11235, .T. ) ;
#14813 = DIRECTION ( 'NONE',  ( 1.000000000000000000, 0.000000000000000000, 0.000000000000000000 ) ) ;
#14814 = CARTESIAN_POINT ( 'NONE',  ( 1.476447168807000221, -81.17305232442998886, 0.5783644924166000401 ) ) ;
#14815 = CARTESIAN_POINT ( 'NONE',  ( 7.103732877834134207, -77.91783737943933374, 8.098743610684461913 ) ) ;
#14816 = CARTESIAN_POINT ( 'NONE',  ( -7.615853692923001184, -78.49593026948699048, 9.247423260715999405 ) ) ;
#14817 = CARTESIAN_POINT ( 'NONE',  ( -1.750000000001000089, -18.74999999009000007, 12.56594317857000043 ) ) ;
#14818 = CARTESIAN_POINT ( 'NONE',  ( 10.40652105080773815, -78.87097662156874378, 2.787377815128531999 ) ) ;
#14819 = CARTESIAN_POINT ( 'NONE',  ( 2.661529024748306327, -3.056711299679849336, 2.302964992746549200 ) ) ;
#14820 = CARTESIAN_POINT ( 'NONE',  ( -5.764562846862999912, -79.11565584965399012, 7.830301022820999712 ) ) ;
#14821 = CARTESIAN_POINT ( 'NONE',  ( -4.341134711875000107, -78.66604404360498393, -8.352589043283000336 ) ) ;
#14822 = CARTESIAN_POINT ( 'NONE',  ( -6.908074975177432187, -86.07389998728979208, -5.681417088837856788 ) ) ;
#14823 = CARTESIAN_POINT ( 'NONE',  ( -10.00926467875000014, -76.92433028348600033, 4.638537167971000130 ) ) ;
#14824 = CARTESIAN_POINT ( 'NONE',  ( -10.85634995915000012, -76.18870722365406323, -5.741293403527000017 ) ) ;
#14825 = CARTESIAN_POINT ( 'NONE',  ( -3.078559409956000081, -80.49385671464260383, -10.70699195275999926 ) ) ;
#14826 = ORIENTED_EDGE ( 'NONE', *, *, #13813, .F. ) ;
#14827 = EDGE_CURVE ( 'NONE', #32490, #40010, #27193, .T. ) ;
#14828 = CARTESIAN_POINT ( 'NONE',  ( -1.929975092515999968, -60.00107256231000008, -12.72537404212999768 ) ) ;
#14829 = VECTOR ( 'NONE', #21814, 1000.000000000000000 ) ;
#14830 = CARTESIAN_POINT ( 'NONE',  ( -1.407065915474770446, -80.48551767968157833, 10.74861335954481056 ) ) ;
#14831 = EDGE_CURVE ( 'NONE', #521, #36712, #39382, .T. ) ;
#14832 = CARTESIAN_POINT ( 'NONE',  ( -10.86658628928999981, -76.78604516064498853, -2.781249891074999869 ) ) ;
#14833 = CARTESIAN_POINT ( 'NONE',  ( 9.694840914897000062, -79.52071780675198909, -5.145296513660000848 ) ) ;
#14834 = VECTOR ( 'NONE', #51533, 1000.000000000000000 ) ;
#14835 = DIRECTION ( 'NONE',  ( 0.000000000000000000, -1.000000000000000000, 0.000000000000000000 ) ) ;
#14836 = CARTESIAN_POINT ( 'NONE',  ( -1.852268148096546385, -82.93958331894259572, 3.560113889582741997 ) ) ;
#14837 = CARTESIAN_POINT ( 'NONE',  ( 1.924380748938630393E-07, -79.75000000000001421, -9.249538042332323684 ) ) ;
#14838 = DIRECTION ( 'NONE',  ( 0.9999999999995751176, 0.000000000000000000, 9.217549097710770925E-07 ) ) ;
#14839 = CARTESIAN_POINT ( 'NONE',  ( 4.037760978116000210, -83.87042953870898998, -1.050253016718000199 ) ) ;
#14840 = AXIS2_PLACEMENT_3D ( 'NONE', #823, #50982, #46855 ) ;
#14841 = CARTESIAN_POINT ( 'NONE',  ( 1.310679582531387943, -79.70833333333334281, -0.7554284705563468760 ) ) ;
#14842 = CARTESIAN_POINT ( 'NONE',  ( 10.15323015671000029, -54.56919784871999468, -7.760928569184999404 ) ) ;
#14843 = ADVANCED_FACE ( 'NONE', ( #4082, #13225 ), #4685, .T. ) ;
#14844 = CARTESIAN_POINT ( 'NONE',  ( 11.26616169758000119, -77.92955615878399556, 0.05236123134324999900 ) ) ;
#14845 = CARTESIAN_POINT ( 'NONE',  ( 1.417725061834000044, -80.03561217387999704, -0.8748226493128999914 ) ) ;
#14846 = CARTESIAN_POINT ( 'NONE',  ( -1.381259992031000028, -78.43489003055999831, 0.3875572711764000422 ) ) ;
#14847 = CARTESIAN_POINT ( 'NONE',  ( 1.570796326794909881, -79.43541666666665435, -11.99999999999999822 ) ) ;
#14848 = CARTESIAN_POINT ( 'NONE',  ( -0.5205927694291033747, -81.34712621142415401, -1.418571885323605786 ) ) ;
#14849 = CARTESIAN_POINT ( 'NONE',  ( 9.250000000000000000, -79.74999999999998579, 1.907449677260999760E-14 ) ) ;
#14850 = CARTESIAN_POINT ( 'NONE',  ( -7.482244971425966895, -80.16420082495498889, -7.718414027147809442 ) ) ;
#14851 = CARTESIAN_POINT ( 'NONE',  ( -1.980532734072999901, -22.76232686847000153, -12.80090744964000038 ) ) ;
#14852 = CARTESIAN_POINT ( 'NONE',  ( -0.9057099665792408549, -81.03819025148258959, 0.9057972107843319520 ) ) ;
#14853 = ORIENTED_EDGE ( 'NONE', *, *, #20617, .T. ) ;
#14854 = CARTESIAN_POINT ( 'NONE',  ( -0.4933197585330857393, -81.69281355437695424, -1.148584473005615170 ) ) ;
#14855 = CARTESIAN_POINT ( 'NONE',  ( -9.643902624173000149, -79.49921224881200033, -5.356946570292000054 ) ) ;
#14856 = CARTESIAN_POINT ( 'NONE',  ( 6.055527902613000002, -78.11999999999999034, 7.319875806370000682 ) ) ;
#14857 = ORIENTED_EDGE ( 'NONE', *, *, #34220, .F. ) ;
#14858 = ORIENTED_EDGE ( 'NONE', *, *, #53886, .T. ) ;
#14859 = CARTESIAN_POINT ( 'NONE',  ( -1.490057467831999993, -81.56212029435899069, -0.2804833236429000176 ) ) ;
#14860 = ORIENTED_EDGE ( 'NONE', *, *, #52320, .T. ) ;
#14861 = ORIENTED_EDGE ( 'NONE', *, *, #46354, .T. ) ;
#14862 = CARTESIAN_POINT ( 'NONE',  ( -0.1963495408493673433, -81.88541666667427421, 1.499999999999999334 ) ) ;
#14863 = CARTESIAN_POINT ( 'NONE',  ( -1.172866835075395020, -77.78255208343296090, -0.9024179113435036870 ) ) ;
#14864 = APPLICATION_PROTOCOL_DEFINITION ( 'draft international standard', 'automotive_design', 1998, #33019 ) ;
#14865 = CARTESIAN_POINT ( 'NONE',  ( 1.691954025052836430, -79.70208332662505768, 2.999979231498003163 ) ) ;
#14866 = CARTESIAN_POINT ( 'NONE',  ( 2.075550720420999973, -78.46226001420198770, -9.805082477504999616 ) ) ;
#14867 = CARTESIAN_POINT ( 'NONE',  ( 1.828541268174307399, -78.24096508442137576, -9.067390816575571222 ) ) ;
#14868 = FACE_OUTER_BOUND ( 'NONE', #25606, .T. ) ;
#14869 = VECTOR ( 'NONE', #45600, 1000.000000000000114 ) ;
#14870 = EDGE_LOOP ( 'NONE', ( #2823, #50238, #2868, #20315, #52917, #47495, #44338, #55280, #26821, #45832, #4990 ) ) ;
#14871 = ORIENTED_EDGE ( 'NONE', *, *, #55835, .T. ) ;
#14872 = CARTESIAN_POINT ( 'NONE',  ( 12.60356226360999798, -56.04922971106000062, 1.750000000000000000 ) ) ;
#14873 = CARTESIAN_POINT ( 'NONE',  ( -10.98749645531777652, -76.93354319426246946, -4.929334125398809441 ) ) ;
#14874 = CARTESIAN_POINT ( 'NONE',  ( 10.18773063539611812, -78.17416963246105865, -3.499611392789568676 ) ) ;
#14875 = ADVANCED_FACE ( 'NONE', ( #53686 ), #36552, .F. ) ;
#14876 = CARTESIAN_POINT ( 'NONE',  ( 0.8338927958996298351, -17.19946422253883966, 12.50366901602930447 ) ) ;
#14877 = CARTESIAN_POINT ( 'NONE',  ( -2.572125540837000290, -78.37350109675199406, -9.357076443458000270 ) ) ;
#14878 = AXIS2_PLACEMENT_3D ( 'NONE', #1891, #28719, #2176 ) ;
#14879 = CYLINDRICAL_SURFACE ( 'NONE', #6787, 3.250000000000000000 ) ;
#14880 = CARTESIAN_POINT ( 'NONE',  ( 1.775602382380404354, -85.90660159999292489, 3.534306991046110014 ) ) ;
#14881 = CARTESIAN_POINT ( 'NONE',  ( 6.043427764450763462, -76.73333333333330586, 10.48543666025111065 ) ) ;
#14882 = B_SPLINE_CURVE_WITH_KNOTS ( 'NONE', 3,
 ( #28040, #18910, #10058, #50211, #18626, #45793, #23040, #41632 ),
 .UNSPECIFIED., .F., .F.,
 ( 4, 2, 2, 4 ),
 ( 0.000000000000000000, 0.5000000000000000000, 0.7500000000000000000, 1.000000000000000000 ),
 .UNSPECIFIED. ) ;
#14883 = CARTESIAN_POINT ( 'NONE',  ( 1.298035947816999824, -80.35461938843998553, -0.6866955795318000488 ) ) ;
#14884 = FACE_OUTER_BOUND ( 'NONE', #23005, .T. ) ;
#14885 = CARTESIAN_POINT ( 'NONE',  ( -4.013993253630999902, -78.65351518583565849, 0.5807183705604999080 ) ) ;
#14886 = CARTESIAN_POINT ( 'NONE',  ( 0.7090065431140329943, -79.41388741558243680, -1.333103239968771447 ) ) ;
#14887 = CARTESIAN_POINT ( 'NONE',  ( 3.140974612311327796, -76.65416666666669698, 11.68767212001979594 ) ) ;
#14888 = CARTESIAN_POINT ( 'NONE',  ( -8.547594633831460342, -76.65220310981916896, -6.557508948702818863 ) ) ;
#14889 = CARTESIAN_POINT ( 'NONE',  ( 3.345231861902000059, -81.04982046129099160, 1.180667782100000007 ) ) ;
#14891 = CARTESIAN_POINT ( 'NONE',  ( -0.5996107393304999089, -78.63399600787198551, 1.191235959310000148 ) ) ;
#14890 = FACE_OUTER_BOUND ( 'NONE', #9352, .T. ) ;
#14892 = DIRECTION ( 'NONE',  ( -1.000000000000000000, 0.000000000000000000, 0.000000000000000000 ) ) ;
#14893 = CARTESIAN_POINT ( 'NONE',  ( 7.094389250268374525, -80.00000000000000000, -6.397685483451420296 ) ) ;
#14894 = CARTESIAN_POINT ( 'NONE',  ( 6.226899213932999722, -78.49568698277398937, -9.208165984944999494 ) ) ;
#14895 = CARTESIAN_POINT ( 'NONE',  ( 1.250000000000000222, -79.23958333333331439, -0.1636246173744659582 ) ) ;
#14896 = ORIENTED_EDGE ( 'NONE', *, *, #45220, .T. ) ;
#14897 = CARTESIAN_POINT ( 'NONE',  ( -10.22919423418071005, -78.84166666666666856, -5.911015991358792299 ) ) ;
#14898 = FACE_OUTER_BOUND ( 'NONE', #32639, .T. ) ;
#14899 = CARTESIAN_POINT ( 'NONE',  ( -3.785211018891809776, -77.59942841202766317, 11.15200902601148769 ) ) ;
#14900 = DIRECTION ( 'NONE',  ( -1.140590449755075033E-08, -0.7071067811865474617, 0.7071067811865474617 ) ) ;
#14901 = ADVANCED_FACE ( 'NONE', ( #54851 ), #52800, .F. ) ;
#14902 = CARTESIAN_POINT ( 'NONE',  ( 1.667916687331000070, -60.09848884406000025, 12.49168451100999988 ) ) ;
#14903 = CARTESIAN_POINT ( 'NONE',  ( 12.53073434187000146, -77.67626658266999584, -3.509976885708000260 ) ) ;
#14904 = CARTESIAN_POINT ( 'NONE',  ( 4.287079134832745275, -79.44247393178839900, 9.901961492083930949 ) ) ;
#14905 = AXIS2_PLACEMENT_3D ( 'NONE', #58261, #40840, #13374 ) ;
#14906 = CARTESIAN_POINT ( 'NONE',  ( 4.192487693857999353, -79.04023998579799581, -8.677185653192001524 ) ) ;
#14907 = DIRECTION ( 'NONE',  ( -1.000000000000000000, 0.000000000000000000, 0.000000000000000000 ) ) ;
#14908 = CARTESIAN_POINT ( 'NONE',  ( 10.88908634000999953, -77.47532284559098059, -2.468401097160000113 ) ) ;
#14909 = EDGE_CURVE ( 'NONE', #3462, #19523, #53984, .T. ) ;
#14910 = CARTESIAN_POINT ( 'NONE',  ( -1.360024375902000093, -81.81732711469500430, 0.6474833154074999264 ) ) ;
#14911 = CARTESIAN_POINT ( 'NONE',  ( 12.50000000000000000, -15.06282895647999887, 0.000000000000000000 ) ) ;
#14912 = CARTESIAN_POINT ( 'NONE',  ( -3.430696936678000242, -78.42549936685999512, 8.765929102848000198 ) ) ;
#14913 = EDGE_CURVE ( 'NONE', #32054, #9701, #7378, .T. ) ;
#14915 = CARTESIAN_POINT ( 'NONE',  ( 7.648026766715999791, -55.54999999381000464, 10.12290050087000104 ) ) ;
#14914 = CARTESIAN_POINT ( 'NONE',  ( -3.724867944340000125, -84.42629260435599292, -0.4865481737740000034 ) ) ;
#14916 = CARTESIAN_POINT ( 'NONE',  ( -2.317989000404999889, -79.67544805011499420, -9.269382932261999386 ) ) ;
#14917 = DIRECTION ( 'NONE',  ( 0.7071067811864973907, 0.7071067811865973107, -2.112640561316990679E-08 ) ) ;
#14918 = CARTESIAN_POINT ( 'NONE',  ( 1.315649220613000159, -79.40213206121900669, -0.09814633906038999767 ) ) ;
#14919 = CARTESIAN_POINT ( 'NONE',  ( 12.50745077485999879, -53.80005551680000053, -2.012158279073999839E-09 ) ) ;
#14920 = CARTESIAN_POINT ( 'NONE',  ( -7.624341764923000753, -18.73514850530999709, -10.42531124853000080 ) ) ;
#14921 = CIRCLE ( 'NONE', #50811, 11.00000000000000000 ) ;
#14922 = ORIENTED_EDGE ( 'NONE', *, *, #8897, .F. ) ;
#14923 = CARTESIAN_POINT ( 'NONE',  ( 7.313768098873999257, -79.02375777975099425, 9.313141831727000053 ) ) ;
#14924 = CARTESIAN_POINT ( 'NONE',  ( 0.000000000000000000, -87.59999999999999432, 0.000000000000000000 ) ) ;
#14925 = DIRECTION ( 'NONE',  ( -1.000000000000000000, 0.000000000000000000, 0.000000000000000000 ) ) ;
#14926 = ORIENTED_EDGE ( 'NONE', *, *, #53604, .F. ) ;
#14927 = APPLICATION_CONTEXT ( 'automotive_design' ) ;
#14928 = CARTESIAN_POINT ( 'NONE',  ( 11.93224739473999918, -77.87500106391100019, 0.2386934378577999782 ) ) ;
#14929 = ORIENTED_EDGE ( 'NONE', *, *, #14913, .F. ) ;
#14930 = ORIENTED_EDGE ( 'NONE', *, *, #43557, .F. ) ;
#14931 = DIRECTION ( 'NONE',  ( 1.000000000000000000, 0.000000000000000000, 0.000000000000000000 ) ) ;
#14932 = EDGE_CURVE ( 'NONE', #55147, #12394, #45285, .T. ) ;
#14933 = ORIENTED_EDGE ( 'NONE', *, *, #39148, .F. ) ;
#14934 = CARTESIAN_POINT ( 'NONE',  ( 1.377877372877000184, -80.65768892718899963, -3.268489530280999755 ) ) ;
#14935 = CARTESIAN_POINT ( 'NONE',  ( 10.48774103543000180, -58.55472018357999531, 7.686941364784000363 ) ) ;
#14936 = VERTEX_POINT ( 'NONE', #32979 ) ;
#14937 = CARTESIAN_POINT ( 'NONE',  ( 1.092468167825580094, -82.80859976460473604, -0.6286521223243165535 ) ) ;
#14938 = CARTESIAN_POINT ( 'NONE',  ( -7.626500777218999438, -55.48415267986000288, 10.35747145890000098 ) ) ;
#14939 = EDGE_LOOP ( 'NONE', ( #50041, #23064, #50974, #54735, #4280 ) ) ;
#14940 = CARTESIAN_POINT ( 'NONE',  ( 9.393203674808285442, -80.70833333333332860, -5.413904038987152667 ) ) ;
#14941 = CARTESIAN_POINT ( 'NONE',  ( -0.8122579684721802362, -79.32966908951244989, -1.270466924700469180 ) ) ;
#14942 = CARTESIAN_POINT ( 'NONE',  ( 3.630949683904999947, -79.79999999999999716, -11.17491406647000041 ) ) ;
#14943 = ADVANCED_FACE ( 'NONE', ( #38001 ), #10277, .F. ) ;
#14944 = CARTESIAN_POINT ( 'NONE',  ( -10.71797595155061877, -80.09332378991105372, 0.9698581247420646756 ) ) ;
#14945 = CARTESIAN_POINT ( 'NONE',  ( 8.439151210957692939, -78.63560278023904004, -8.898801520529000086 ) ) ;
#14946 = CIRCLE ( 'NONE', #57347, 2.500000000000000000 ) ;
#14947 = CARTESIAN_POINT ( 'NONE',  ( 4.746041175454999816, -77.41566667364776322, -8.464384343845999581 ) ) ;
#14948 = CARTESIAN_POINT ( 'NONE',  ( -7.695020077040999773, -76.20149010202899831, 8.115451295621999961 ) ) ;
#14949 = CARTESIAN_POINT ( 'NONE',  ( 8.393801617969296913, -79.55998208041128805, -4.599114686830800380 ) ) ;
#14950 = EDGE_CURVE ( 'NONE', #56949, #10301, #32774, .T. ) ;
#14951 = CARTESIAN_POINT ( 'NONE',  ( -7.613962827161000035, -55.49360374314999689, -10.53101998745000145 ) ) ;
#14952 = CARTESIAN_POINT ( 'NONE',  ( -7.828848276711099174, -78.64487340676903671, -4.926425388625121471 ) ) ;
#14953 = CARTESIAN_POINT ( 'NONE',  ( 6.541589835834063393, -76.52783443949311959, 9.760510139220190950 ) ) ;
#14954 = CARTESIAN_POINT ( 'NONE',  ( 8.713118354389999709, -77.85151001420200600, 3.557876713735000251 ) ) ;
#14955 = CARTESIAN_POINT ( 'NONE',  ( -1.120379678216000041, -79.17996300973499046, -0.7232983489183999470 ) ) ;
#14956 = CARTESIAN_POINT ( 'NONE',  ( -4.797609507281214825, -80.18923283849920836, -9.904543496687123749 ) ) ;
#14957 = CARTESIAN_POINT ( 'NONE',  ( 9.500000000000000000, -77.04999999999999716, 0.000000000000000000 ) ) ;
#14958 = CARTESIAN_POINT ( 'NONE',  ( -3.888905289927000020, -78.44153455456849144, -0.7628755026328000177 ) ) ;
#14959 = DIRECTION ( 'NONE',  ( -1.000000000000000000, 0.000000000000000000, 0.000000000000000000 ) ) ;
#14960 = CARTESIAN_POINT ( 'NONE',  ( 7.359424254351999650, -77.99911332859899460, 6.245857008621999107 ) ) ;
#14961 = CARTESIAN_POINT ( 'NONE',  ( -9.797074649825203707, -78.06619525258034287, 4.439059621284440205 ) ) ;
#14962 = CARTESIAN_POINT ( 'NONE',  ( 1.142427346679885547, -82.88327974481559579, 0.5074387660638589592 ) ) ;
#14963 = CARTESIAN_POINT ( 'NONE',  ( 6.187590335240950701, -77.08125000000001137, -7.247098261820500653 ) ) ;
#14964 = CARTESIAN_POINT ( 'NONE',  ( -4.000000000000000000, -78.69999999915415856, 2.834003763004000336E-08 ) ) ;
#14965 = CARTESIAN_POINT ( 'NONE',  ( 12.76303204513999923, -55.53514852210999919, -1.980584515753000208 ) ) ;
#14966 = CARTESIAN_POINT ( 'NONE',  ( -0.8579432262127338893, -78.03348889011373046, 0.9468520969737713733 ) ) ;
#14967 = CYLINDRICAL_SURFACE ( 'NONE', #47057, 0.6000000000000008660 ) ;
#14968 = CARTESIAN_POINT ( 'NONE',  ( -5.683881862889148984, -79.67335042278446622, -7.396142196161008542 ) ) ;
#14969 = FACE_OUTER_BOUND ( 'NONE', #48621, .T. ) ;
#14970 = CARTESIAN_POINT ( 'NONE',  ( 1.021972327705173322, -79.53347328969611851, -1.113959016257049628 ) ) ;
#14971 = CARTESIAN_POINT ( 'NONE',  ( 13.63885489310999510, -22.78578169018999944, -7.254376133916000668 ) ) ;
#14972 = CARTESIAN_POINT ( 'NONE',  ( 6.584508673715999905, -78.32564415034599392, 7.154582167228999978 ) ) ;
#14973 = CARTESIAN_POINT ( 'NONE',  ( 12.77649732927999970, -25.30828417252000051, -0.06479631635390999123 ) ) ;
#14974 = CARTESIAN_POINT ( 'NONE',  ( 5.620651130188175415, -77.28197757598998408, 9.267943761422831273 ) ) ;
#14975 = CARTESIAN_POINT ( 'NONE',  ( -0.9935076046663652294, -24.96816187757334049, -12.70250268216760681 ) ) ;
#14976 = CARTESIAN_POINT ( 'NONE',  ( -5.052374247686000075, -75.84546611944999484, -10.65162165865999988 ) ) ;
#14977 = ORIENTED_EDGE ( 'NONE', *, *, #38413, .T. ) ;
#14978 = CARTESIAN_POINT ( 'NONE',  ( -3.696868630880000062, -83.59271544543099708, -1.427985666462000092 ) ) ;
#14979 = CARTESIAN_POINT ( 'NONE',  ( -11.28597752728000003, -80.71071295308820481, -0.2623390868082999816 ) ) ;
#14980 = CARTESIAN_POINT ( 'NONE',  ( 7.546403568604966416, -78.30109726589176944, -5.349046595936441939 ) ) ;
#14981 = CARTESIAN_POINT ( 'NONE',  ( 12.77651047021000075, -62.10895689102999739, -0.04321256188117000158 ) ) ;
#14982 = CARTESIAN_POINT ( 'NONE',  ( -8.728447447808001414, -76.84899201919300538, 6.810956705545000212 ) ) ;
#14983 = CYLINDRICAL_SURFACE ( 'NONE', #24805, 1.250000000000000000 ) ;
#14984 = AXIS2_PLACEMENT_3D ( 'NONE', #36435, #467, #55033 ) ;
#14985 = CARTESIAN_POINT ( 'NONE',  ( -2.191084135724000070, -77.72224322018799114, 9.489933931099999498 ) ) ;
#14986 = CARTESIAN_POINT ( 'NONE',  ( 0.5269479332349999989, -83.23821404977199734, 1.580352090963000000 ) ) ;
#14987 = DIRECTION ( 'NONE',  ( -1.000000000000000000, 0.000000000000000000, 0.000000000000000000 ) ) ;
#14988 = DIRECTION ( 'NONE',  ( 0.7071067811864981678, 0.000000000000000000, -0.7071067811865970887 ) ) ;
#14989 = ORIENTED_EDGE ( 'NONE', *, *, #12169, .T. ) ;
#14990 = FACE_OUTER_BOUND ( 'NONE', #36686, .T. ) ;
#14991 = PLANE ( 'NONE',  #14373 ) ;
#14992 = CARTESIAN_POINT ( 'NONE',  ( 7.496935112050000072, -80.51537353295650234, 8.408636027568000770 ) ) ;
#14993 = CIRCLE ( 'NONE', #48922, 9.199999999999999289 ) ;
#14994 = CARTESIAN_POINT ( 'NONE',  ( -0.7022187824378000043, -82.19906693409399168, -1.095132696781000003 ) ) ;
#14995 = ORIENTED_EDGE ( 'NONE', *, *, #45102, .F. ) ;
#14996 = CARTESIAN_POINT ( 'NONE',  ( 0.9384621721472999889, -78.44722272595291201, 0.9475573338641000154 ) ) ;
#14997 = B_SPLINE_CURVE_WITH_KNOTS ( 'NONE', 3,
 ( #56543, #12810, #30809, #57115, #25816, #26382, #44402, #43260, #3954, #38528, #21387, #16104, #34663 ),
 .UNSPECIFIED., .F., .F.,
 ( 4, 2, 2, 1, 2, 2, 4 ),
 ( 0.000000000000000000, 0.2499999999999998890, 0.4999999999999997780, 0.6249999999999997780, 0.6874999999999995559, 0.7499999999999995559, 1.000000000000000000 ),
 .UNSPECIFIED. ) ;
#14998 = CARTESIAN_POINT ( 'NONE',  ( -4.543693065121372499, -77.58445504582732610, -8.146396484383414460 ) ) ;
#14999 = CARTESIAN_POINT ( 'NONE',  ( -0.7889670424319170650, -80.67174664738183765, -0.9893556795060300946 ) ) ;
#15000 = ORIENTED_EDGE ( 'NONE', *, *, #30539, .T. ) ;
#15001 = CARTESIAN_POINT ( 'NONE',  ( 4.975516581814000361, -78.41739492409399759, -11.10075516933000017 ) ) ;
#15002 = CARTESIAN_POINT ( 'NONE',  ( -1.930989144707000005, -20.24634220924000161, 12.80900240957999969 ) ) ;
#15003 = VECTOR ( 'NONE', #47116, 1000.000000000000114 ) ;
#15004 = ORIENTED_EDGE ( 'NONE', *, *, #32148, .F. ) ;
#15005 = EDGE_LOOP ( 'NONE', ( #23513, #12195, #33660, #7291 ) ) ;
#15006 = VECTOR ( 'NONE', #38114, 1000.000000000000114 ) ;
#15007 = ADVANCED_FACE ( 'NONE', ( #42452 ), #1437, .F. ) ;
#15008 = CARTESIAN_POINT ( 'NONE',  ( -1.250000000000000000, -80.59999999999999432, 0.000000000000000000 ) ) ;
#15009 = EDGE_CURVE ( 'NONE', #23097, #49897, #55140, .T. ) ;
#15010 = CARTESIAN_POINT ( 'NONE',  ( 1.407249749486563895, -77.73544497621409732, -10.74983756269776514 ) ) ;
#15011 = CARTESIAN_POINT ( 'NONE',  ( 9.202039358297998461, -80.16043756281898425, 2.360608321670000453 ) ) ;
#15012 = ORIENTED_EDGE ( 'NONE', *, *, #52048, .T. ) ;
#15013 = CARTESIAN_POINT ( 'NONE',  ( -8.130813118348999780, -54.11476110100999648, 9.546856411314999846 ) ) ;
#15014 = CARTESIAN_POINT ( 'NONE',  ( 10.04567131160781557, -24.55088387374295067, -7.921299640536786590 ) ) ;
#15015 = ORIENTED_EDGE ( 'NONE', *, *, #47427, .T. ) ;
#15016 = DIRECTION ( 'NONE',  ( 0.000000000000000000, 0.000000000000000000, -1.000000000000000000 ) ) ;
#15017 = CARTESIAN_POINT ( 'NONE',  ( 8.503129636637000388, -77.72314415034598767, -4.225430575863000193 ) ) ;
#15018 = FACE_OUTER_BOUND ( 'NONE', #5708, .T. ) ;
#15019 = CARTESIAN_POINT ( 'NONE',  ( -1.168247351827577551, -80.12911975281166121, -0.4458151081181576658 ) ) ;
#15020 = DIRECTION ( 'NONE',  ( 1.000000000000000000, 0.000000000000000000, 0.000000000000000000 ) ) ;
#15021 = CARTESIAN_POINT ( 'NONE',  ( -11.14643061761961818, -76.74479870980059104, 0.7341212784377569855 ) ) ;
#15022 = EDGE_CURVE ( 'NONE', #15410, #18144, #27088, .T. ) ;
#15023 = CARTESIAN_POINT ( 'NONE',  ( 9.451694958653000356, -76.99163136579679190, 2.733625046654999835 ) ) ;
#15024 = CARTESIAN_POINT ( 'NONE',  ( 1.504596964206185161, -78.10654535218401406, 0.1305286778095537392 ) ) ;
#15025 = CARTESIAN_POINT ( 'NONE',  ( 2.793917098883578642, -79.25885415185018701, -2.879926396557028312 ) ) ;
#15026 = AXIS2_PLACEMENT_3D ( 'NONE', #38181, #23732, #20189 ) ;
#15027 = CARTESIAN_POINT ( 'NONE',  ( 11.65396969189999865, -75.71350996453999471, -2.860942225950000140 ) ) ;
#15028 = FACE_OUTER_BOUND ( 'NONE', #43954, .T. ) ;
#15029 = AXIS2_PLACEMENT_3D ( 'NONE', #31070, #44099, #22531 ) ;
#15030 = CARTESIAN_POINT ( 'NONE',  ( 7.619389973917000347, -60.20786254198000620, -10.35398617735999949 ) ) ;
#15032 = EDGE_CURVE ( 'NONE', #470, #48419, #13011, .T. ) ;
#15031 = CARTESIAN_POINT ( 'NONE',  ( -12.26143800982999998, -79.05353869690000579, -0.2371146996492999870 ) ) ;
#15033 = CARTESIAN_POINT ( 'NONE',  ( 12.24159337356999977, -76.37751877473299089, -0.9828625608234000666 ) ) ;
#15034 = B_SPLINE_CURVE_WITH_KNOTS ( 'NONE', 3,
 ( #5963, #38126, #6549, #45851, #24267, #41692, #54975, #55265, #51732, #23966, #1270, #14524, #33404, #41985, #19261, #56150, #37839, #42574 ),
 .UNSPECIFIED., .F., .F.,
 ( 4, 2, 2, 2, 2, 2, 2, 2, 4 ),
 ( 0.000000000000000000, 0.1250000000000000000, 0.2500000000000000000, 0.3750000000000000000, 0.5000000000000000000, 0.6250000000000000000, 0.7500000000000000000, 0.8750000000000000000, 1.000000000000000000 ),
 .UNSPECIFIED. ) ;
#15035 = LINE ( 'NONE', #9741, #44974 ) ;
#15036 = CARTESIAN_POINT ( 'NONE',  ( 3.250000000000000000, -2.850000000000000089, 0.000000000000000000 ) ) ;
#15037 = CARTESIAN_POINT ( 'NONE',  ( 10.79003353078767091, -77.76296722650485549, -5.409130585825370652 ) ) ;
#15038 = CARTESIAN_POINT ( 'NONE',  ( 0.000000000000000000, -75.15999999999999659, 0.000000000000000000 ) ) ;
#15039 = ADVANCED_FACE ( 'NONE', ( #1149 ), #21947, .F. ) ;
#15040 = ORIENTED_EDGE ( 'NONE', *, *, #31457, .T. ) ;
#15041 = CARTESIAN_POINT ( 'NONE',  ( -1.441964492907930273, -81.22566618236561453, 0.4560415640900693512 ) ) ;
#15042 = CARTESIAN_POINT ( 'NONE',  ( 1.538071403320016461, -77.93541666666664014, -11.74999999999999822 ) ) ;
#15043 = CARTESIAN_POINT ( 'NONE',  ( -9.434983556464704435, -77.21406646732883416, -0.1995201537112713253 ) ) ;
#15044 = CIRCLE ( 'NONE', #42374, 14.00000000000000000 ) ;
#15045 = CARTESIAN_POINT ( 'NONE',  ( 1.217465845835393967, -78.77083333333330017, 0.3271848554491025851 ) ) ;
#15046 = CARTESIAN_POINT ( 'NONE',  ( 2.922428402108999901, -1.987477233353000194, -2.537670070524999932 ) ) ;
#15047 = CARTESIAN_POINT ( 'NONE',  ( 7.527227981725999939, -78.33017081663599868, 9.409389490551998136 ) ) ;
#15048 = CARTESIAN_POINT ( 'NONE',  ( 0.8552902072924000176, -78.33901425910798366, -9.592793577801000282 ) ) ;
#15050 = CARTESIAN_POINT ( 'NONE',  ( 9.468749999988999022, -76.98125000001098783, 2.084568677130999610E-09 ) ) ;
#15049 = CARTESIAN_POINT ( 'NONE',  ( -8.776627003607282873, -76.14201958266359327, 7.813090293080676041 ) ) ;
#15051 = CARTESIAN_POINT ( 'NONE',  ( 6.695505957611000092, -79.34904856920998384, 8.622387486181999350 ) ) ;
#15052 = CARTESIAN_POINT ( 'NONE',  ( 3.451879464910978079, -85.80681307243298761, -1.536875756006047533 ) ) ;
#15053 = VERTEX_POINT ( 'NONE', #43029 ) ;
#15054 = CARTESIAN_POINT ( 'NONE',  ( 0.7833523767573995489, -81.06795188156627319, -1.316067733153899688 ) ) ;
#15055 = CARTESIAN_POINT ( 'NONE',  ( -12.00019890019965096, -76.39977373798492977, -1.177339121803222359E-06 ) ) ;
#15056 = CARTESIAN_POINT ( 'NONE',  ( 9.393203674808260573, -77.29166666666665719, 5.413904038987188194 ) ) ;
#15057 = CARTESIAN_POINT ( 'NONE',  ( 9.632126701410999914, -79.28024126877399169, 5.261763182588000021 ) ) ;
#15058 = CARTESIAN_POINT ( 'NONE',  ( -10.93918996500858043, -80.09187350056868127, 1.167787996473995671 ) ) ;
#15059 = CARTESIAN_POINT ( 'NONE',  ( 5.578188741145999607, -79.40460703100998785, 7.763689502541000209 ) ) ;
#15060 = CARTESIAN_POINT ( 'NONE',  ( 10.53494359615000064, -18.77285042833999995, -7.618393753193999807 ) ) ;
#15061 = CARTESIAN_POINT ( 'NONE',  ( 8.583665412795216554, -17.02814425026380718, 9.102144266516488003 ) ) ;
#15062 = EDGE_LOOP ( 'NONE', ( #19054, #38112, #47488 ) ) ;
#15063 = CARTESIAN_POINT ( 'NONE',  ( -10.07641688825555271, -76.38559964190847040, -4.852212949701282696 ) ) ;
#15064 = CARTESIAN_POINT ( 'NONE',  ( -5.422116380438207983, -79.63706600996927421, -10.51876813104020059 ) ) ;
#15065 = CARTESIAN_POINT ( 'NONE',  ( 9.599999999916001059, -90.40000000008399184, -6.531555804621000072E-10 ) ) ;
#15066 = CARTESIAN_POINT ( 'NONE',  ( 10.93488396298730336, -77.73714250434947814, 5.001126911209347270 ) ) ;
#15068 = DIRECTION ( 'NONE',  ( 0.000000000000000000, -1.000000000000000000, 0.000000000000000000 ) ) ;
#15067 = CARTESIAN_POINT ( 'NONE',  ( -0.4818272427706999927, -82.25167760925999971, -1.167471054476999948 ) ) ;
#15069 = CARTESIAN_POINT ( 'NONE',  ( -9.066922875887595268, -78.90000278671779199, -6.603977477736625801 ) ) ;
#15070 = CARTESIAN_POINT ( 'NONE',  ( 8.485281374238999419, 0.000000000000000000, 8.485281374238999419 ) ) ;
#15071 = CARTESIAN_POINT ( 'NONE',  ( 10.48774103543000180, -21.75472018390999907, 7.686941364778000718 ) ) ;
#15072 = CARTESIAN_POINT ( 'NONE',  ( 0.2600691642747999799, -78.43909607169999276, 1.281852779972999734 ) ) ;
#15073 = CARTESIAN_POINT ( 'NONE',  ( 0.000000000000000000, 4.040000000000000036, 0.000000000000000000 ) ) ;
#15074 = CARTESIAN_POINT ( 'NONE',  ( 8.867210690492070668, -78.64994923118607062, -6.468415063504793672 ) ) ;
#15075 = DIRECTION ( 'NONE',  ( 0.000000000000000000, 0.000000000000000000, -1.000000000000000000 ) ) ;
#15076 = ORIENTED_EDGE ( 'NONE', *, *, #11752, .T. ) ;
#15077 = EDGE_LOOP ( 'NONE', ( #35463, #43436, #19085, #51123 ) ) ;
#15078 = B_SPLINE_CURVE_WITH_KNOTS ( 'NONE', 3,
 ( #22934, #23511, #31773, #55101, #18803, #45977, #40947, #32935, #9652, #54812 ),
 .UNSPECIFIED., .F., .F.,
 ( 4, 2, 2, 2, 4 ),
 ( 0.000000000000000000, 0.2500000000000000000, 0.5000000000000000000, 0.7500000000000000000, 1.000000000000000000 ),
 .UNSPECIFIED. ) ;
#15079 = CARTESIAN_POINT ( 'NONE',  ( 2.853743189566999534E-14, -82.05000000008600125, 0.000000000000000000 ) ) ;
#15080 = CARTESIAN_POINT ( 'NONE',  ( 8.845698630191822787, -78.80205931604734815, -6.110774902956666033 ) ) ;
#15081 = AXIS2_PLACEMENT_3D ( 'NONE', #53249, #12800, #58266 ) ;
#15082 = ORIENTED_EDGE ( 'NONE', *, *, #27863, .F. ) ;
#15083 = CARTESIAN_POINT ( 'NONE',  ( 9.038965287783000235, -16.66737759107000372, 9.029769469460999787 ) ) ;
#15084 = AXIS2_PLACEMENT_3D ( 'NONE', #32338, #4629, #36204 ) ;
#15085 = CARTESIAN_POINT ( 'NONE',  ( -1.310679582531389276, -80.35833333333332007, 0.7554284705563443225 ) ) ;
#15086 = CARTESIAN_POINT ( 'NONE',  ( 8.852327248605000420, -79.13956593151999641, 7.934268801159999107 ) ) ;
#15087 = CARTESIAN_POINT ( 'NONE',  ( 9.963467980718000661, -60.48274967040000405, 7.659239661670000032 ) ) ;
#15089 = EDGE_CURVE ( 'NONE', #46308, #36059, #55270, .T. ) ;
#15088 = CARTESIAN_POINT ( 'NONE',  ( 11.84749940521009393, -76.81854709368607814, 2.910134059890192582 ) ) ;
#15090 = CARTESIAN_POINT ( 'NONE',  ( 11.88398914487867941, -78.28982288711439708, -1.513536703370712999 ) ) ;
#15091 = CARTESIAN_POINT ( 'NONE',  ( 3.371435477143000181, -79.41539981197399811, -10.69820234502000034 ) ) ;
#15092 = VERTEX_POINT ( 'NONE', #48615 ) ;
#15093 = CARTESIAN_POINT ( 'NONE',  ( -10.04567131160781557, -24.55088387374295067, 7.921299640536786590 ) ) ;
#15094 = ORIENTED_EDGE ( 'NONE', *, *, #26526, .T. ) ;
#15095 = CARTESIAN_POINT ( 'NONE',  ( 7.337322956731747503, -77.40219940825448930, 5.633178353381969927 ) ) ;
#15096 = CARTESIAN_POINT ( 'NONE',  ( 1.315649220613000159, -79.48601699803499798, -0.09814633906038999767 ) ) ;
#15097 = CYLINDRICAL_SURFACE ( 'NONE', #25326, 0.6000000000000008660 ) ;
#15098 = CARTESIAN_POINT ( 'NONE',  ( -1.521132372192000037, -77.47794916437754864, 0.2748539626865999508 ) ) ;
#15099 = CARTESIAN_POINT ( 'NONE',  ( 10.24474360436999909, -76.45078410675000669, -6.192822469190000234 ) ) ;
#15100 = DIRECTION ( 'NONE',  ( 1.000000000000000000, 0.000000000000000000, 0.000000000000000000 ) ) ;
#15101 = CARTESIAN_POINT ( 'NONE',  ( 1.153380192234999990, -78.70114559065000037, 1.148206073167999941 ) ) ;
#15102 = CARTESIAN_POINT ( 'NONE',  ( -10.86532694299999946, -79.50758784453798000, -2.005633084294999868 ) ) ;
#15103 = CARTESIAN_POINT ( 'NONE',  ( 12.72966770608134546, -60.56881200341882021, 1.931346186347591809 ) ) ;
#15104 = ADVANCED_FACE ( 'NONE', ( #43315 ), #41330, .F. ) ;
#15105 = CARTESIAN_POINT ( 'NONE',  ( 12.80900240954000147, -58.55365779174999830, -1.930989144707000005 ) ) ;
#15106 = CARTESIAN_POINT ( 'NONE',  ( 3.088334425740999922, -85.58531592346599837, 1.744636951369000100 ) ) ;
#15107 = AXIS2_PLACEMENT_3D ( 'NONE', #22566, #3681, #40578 ) ;
#15108 = ORIENTED_EDGE ( 'NONE', *, *, #36357, .F. ) ;
#15109 = CARTESIAN_POINT ( 'NONE',  ( -10.59387557900170940, -77.20000000000000284, 2.870323072861859615 ) ) ;
#15110 = DIRECTION ( 'NONE',  ( 0.7071067811865474617, 0.000000000000000000, 0.7071067811865474617 ) ) ;
#15111 = CARTESIAN_POINT ( 'NONE',  ( -0.3512719843520540897, -77.97766118670328694, 10.74453117849748374 ) ) ;
#15112 = CARTESIAN_POINT ( 'NONE',  ( -9.690626710582000314, -78.11611985355399668, -7.043281791253000357 ) ) ;
#15113 = CARTESIAN_POINT ( 'NONE',  ( -7.633478597825000378, -18.79901960220000134, 10.36292351978000070 ) ) ;
#15114 = B_SPLINE_CURVE_WITH_KNOTS ( 'NONE', 3,
 ( #8188, #56920, #34168, #16477, #20615, #44207, #30609, #48080, #7610, #43059, #47511, #52489, #43340, #47790, #20897, #15897, #2897, #30316, #34458, #3194, #11482, #26189, #39185, #52205, #48357, #20328, #57200, #16768, #53061, #7897, #35029 ),
 .UNSPECIFIED., .F., .F.,
 ( 4, 1, 1, 1, 1, 1, 1, 1, 1, 1, 1, 1, 1, 1, 1, 1, 1, 1, 1, 1, 1, 1, 1, 1, 1, 1, 1, 1, 4 ),
 ( 0.000000000000000000, 0.01409448528475833011, 0.05073813331262903153, 0.08738178134047794310, 0.1240254293683486497, 0.1606690773962193564, 0.1973127254240683026, 0.2339563734519607419, 0.2706000214798749970, 0.3072436695075715374, 0.3438873175354857925, 0.3805309655634000476, 0.4171746135913142473, 0.4538182616192285579, 0.4904619096469250983, 0.5271055576748392424, 0.5637492057027536640, 0.6003928537306677526, 0.6370365017583644596, 0.6736801497862785482, 0.7103237978141928588, 0.7469674458421071694, 0.7836110938698035433, 0.8202547418977179650, 0.8568983899256321646, 0.8935420379535463642, 0.9301856859814607859, 0.9668293340091570487, 1.000000000000000000 ),
 .UNSPECIFIED. ) ;
#15115 = CARTESIAN_POINT ( 'NONE',  ( 1.232757602695059962, -78.02051921516918753, 0.3250462290969571844 ) ) ;
#15116 = CARTESIAN_POINT ( 'NONE',  ( 0.4318235569510932015, -2.884823844453682895, -3.492932053398966730 ) ) ;
#15117 = CARTESIAN_POINT ( 'NONE',  ( -10.12290050122000018, -55.54999999974999980, 7.648026767069000087 ) ) ;
#15118 = DIRECTION ( 'NONE',  ( 0.000000000000000000, -1.000000000000000000, 0.000000000000000000 ) ) ;
#15119 = CARTESIAN_POINT ( 'NONE',  ( 3.576074390005976156, -85.88547955769999476, -1.592170899228053438 ) ) ;
#15120 = CARTESIAN_POINT ( 'NONE',  ( 3.831242997621999713, -77.30563908551199859, 10.34520717408000046 ) ) ;
#15121 = CARTESIAN_POINT ( 'NONE',  ( 11.13784153760999907, -76.43460365348362018, 5.174080857020999957 ) ) ;
#15122 = CARTESIAN_POINT ( 'NONE',  ( -12.00000000000000000, -78.29999999999999716, 0.000000000000000000 ) ) ;
#15123 = VERTEX_POINT ( 'NONE', #19357 ) ;
#15124 = CARTESIAN_POINT ( 'NONE',  ( -0.8719406389885000497, -81.33395355416099903, -1.009106372638000071 ) ) ;
#15125 = CARTESIAN_POINT ( 'NONE',  ( -1.539858032099693741, -77.08353792532550131, 11.67459080161200546 ) ) ;
#15126 = CARTESIAN_POINT ( 'NONE',  ( 0.9887300587116000239, -61.73410057736000311, -12.65963207093999898 ) ) ;
#15127 = CARTESIAN_POINT ( 'NONE',  ( -7.648026768019999366, -23.24999998419999869, -10.12290050217000115 ) ) ;
#15128 = CARTESIAN_POINT ( 'NONE',  ( -8.728447447808001414, -76.71341491264000467, 6.810956705545000212 ) ) ;
#15129 = CARTESIAN_POINT ( 'NONE',  ( -10.44304457033000055, -78.34495714178498815, 3.377400876517000050 ) ) ;
#15130 = FACE_OUTER_BOUND ( 'NONE', #13635, .T. ) ;
#15131 = CARTESIAN_POINT ( 'NONE',  ( -3.970500524723944213, -83.24791665559489218, -0.8021306198144204647 ) ) ;
#15132 = EDGE_CURVE ( 'NONE', #34146, #49594, #45517, .T. ) ;
#15133 = CARTESIAN_POINT ( 'NONE',  ( -5.177348173361999706, -76.16656866488499134, -10.99455251688000068 ) ) ;
#15134 = CARTESIAN_POINT ( 'NONE',  ( 0.000000000000000000, 0.000000000000000000, 0.000000000000000000 ) ) ;
#15135 = CIRCLE ( 'NONE', #42491, 0.5000000000000004441 ) ;
#15136 = CARTESIAN_POINT ( 'NONE',  ( 3.633024531674999835, -85.56019503318798058, 2.052118945875000211 ) ) ;
#15137 = AXIS2_PLACEMENT_3D ( 'NONE', #1088, #24075, #18207 ) ;
#15138 = CARTESIAN_POINT ( 'NONE',  ( 0.9218200799623742503, -79.67708333333332860, -1.199500263597268912 ) ) ;
#15139 = CARTESIAN_POINT ( 'NONE',  ( 7.761025538834000592, -54.71850014388999739, -9.835174270505000038 ) ) ;
#15140 = CARTESIAN_POINT ( 'NONE',  ( 2.988858019399999844, -77.42296592294499646, -10.85820852157999994 ) ) ;
#15141 = CARTESIAN_POINT ( 'NONE',  ( 0.4771943503223999850, -80.47772667965000437, -1.596102929133000004 ) ) ;
#15142 = CARTESIAN_POINT ( 'NONE',  ( 0.3401063316509999601, -79.66751968469999667, -1.168206624324999998 ) ) ;
#15143 = LINE ( 'NONE', #5701, #12266 ) ;
#15144 = CARTESIAN_POINT ( 'NONE',  ( -1.510119349581099168, -81.75199297495029782, -0.03898315715275646465 ) ) ;
#15145 = CARTESIAN_POINT ( 'NONE',  ( -14.00000000000000000, -32.66217755555999958, -5.544640309346000075E-06 ) ) ;
#15146 = VERTEX_POINT ( 'NONE', #85 ) ;
#15147 = CARTESIAN_POINT ( 'NONE',  ( 1.099580560635592841, -79.81033228112796962, -0.6005170649868118993 ) ) ;
#15148 = CARTESIAN_POINT ( 'NONE',  ( -8.266608573639034674, -53.82766203646255576, 9.697383820226121998 ) ) ;
#15149 = ORIENTED_EDGE ( 'NONE', *, *, #17014, .F. ) ;
#15150 = B_SPLINE_CURVE_WITH_KNOTS ( 'NONE', 3,
 ( #26259, #13559, #58143, #48999, #3829, #21829, #8259, #39834, #8546, #9146, #57555, #13263, #31253, #21254, #53136, #48715, #16837, #17710, #44272, #49295, #17116, #18003, #7969, #35993, #31551, #44865, #57847, #54018, #57273, #23, #25966, #43992, #12964, #21545, #22420, #35696, #49598, #34819, #35102, #30962, #27130, #45168, #52847, #39260, #17406, #12684, #26538, #39550, #12400, #3543, #44565, #4119, #22120, #40130, #53724, #8846, #26837, #4419, #22717, #50182, #19171, #10316, #15021, #33015, #19460 ),
 .UNSPECIFIED., .F., .F.,
 ( 4, 1, 1, 1, 1, 1, 1, 1, 1, 1, 1, 1, 1, 1, 1, 1, 1, 1, 1, 1, 1, 1, 1, 1, 1, 1, 1, 1, 1, 1, 1, 1, 1, 1, 1, 1, 1, 1, 1, 1, 1, 1, 1, 1, 1, 1, 1, 1, 1, 1, 1, 1, 1, 1, 1, 1, 1, 1, 1, 1, 1, 1, 4 ),
 ( 0.000000000000000000, 0.01249977652363656183, 0.02874978397244884118, 0.04499979142126112053, 0.06124979887007339641, 0.07749980631888567228, 0.09374981376769794816, 0.1099998212165102240, 0.1262498286653224999, 0.1424998361141347758, 0.1587498435629470794, 0.1749998510117593276, 0.1912498584605716312, 0.2074998659093838793, 0.2237498733581961829, 0.2399998808070084588, 0.2562498882558207347, 0.2724998957046330661, 0.2887499031534452865, 0.3049999106022575623, 0.3212499180510698382, 0.3374999254998821696, 0.3537499329486944455, 0.3699999403975066659, 0.3862499478463189417, 0.4024999552951312731, 0.4187499627439435490, 0.4349999701927558249, 0.4512499776415680453, 0.4674999850903803766, 0.4837499925391926525, 0.4999999999880049284, 0.5162500074368171488, 0.5325000148856294802, 0.5487500223344417005, 0.5650000297832540319, 0.5812500372320663633, 0.5975000446808785837, 0.6137500521296909151, 0.6300000595785031354, 0.6462500670273154668, 0.6625000744761276872, 0.6787500819249399076, 0.6950000893737522389, 0.7112500968225645703, 0.7275001042713769017, 0.7437501117201891221, 0.7600001191690013425, 0.7762501266178136738, 0.7925001340666258942, 0.8087501415154382256, 0.8250001489642504460, 0.8412501564130627774, 0.8575001638618751088, 0.8737501713106873291, 0.8900001787594996605, 0.9062501862083118809, 0.9225001936571242123, 0.9387502011059364326, 0.9550002085547486530, 0.9712502160035609844, 0.9875002234523733158, 1.000000000000000000 ),
 .UNSPECIFIED. ) ;
#15151 = CARTESIAN_POINT ( 'NONE',  ( 0.009713482255590434947, -81.72619256271893562, -1.249622119345054294 ) ) ;
#15152 = CARTESIAN_POINT ( 'NONE',  ( 8.591781367357000931, -78.69610392334999460, 7.101823234627000048 ) ) ;
#15153 = CARTESIAN_POINT ( 'NONE',  ( 5.896171905175000560, -77.96999999999999886, 7.127247495676000355 ) ) ;
#15154 = ORIENTED_EDGE ( 'NONE', *, *, #23496, .T. ) ;
#15155 = ORIENTED_EDGE ( 'NONE', *, *, #33060, .T. ) ;
#15156 = CONICAL_SURFACE ( 'NONE', #46282, 8.749999999256001360, 0.7853981633972997312 ) ;
#15157 = CARTESIAN_POINT ( 'NONE',  ( -1.378883651915999931, -81.12136574827599134, -0.3297563563739999704 ) ) ;
#15158 = EDGE_LOOP ( 'NONE', ( #36297, #37811, #35251, #3129 ) ) ;
#15159 = EDGE_LOOP ( 'NONE', ( #19154, #40715, #26181, #51705 ) ) ;
#15160 = CARTESIAN_POINT ( 'NONE',  ( -1.194090705999000024, -17.55968341096999552, 12.43436538489999954 ) ) ;
#15161 = FACE_OUTER_BOUND ( 'NONE', #44178, .T. ) ;
#15162 = SHAPE_DEFINITION_REPRESENTATION ( #17268, #13452 ) ;
#15163 = CARTESIAN_POINT ( 'NONE',  ( 1.047413828337867114, -82.14947915040829685, -3.245710299348970818 ) ) ;
#15164 = EDGE_CURVE ( 'NONE', #55842, #17140, #11115, .T. ) ;
#15165 = CARTESIAN_POINT ( 'NONE',  ( 3.632230827930608807, -78.25714950312151075, -8.507066908565283470 ) ) ;
#15166 = DIRECTION ( 'NONE',  ( 0.000000000000000000, 0.000000000000000000, -1.000000000000000000 ) ) ;
#15167 = VERTEX_POINT ( 'NONE', #4770 ) ;
#15169 = ORIENTED_EDGE ( 'NONE', *, *, #24516, .F. ) ;
#15168 = EDGE_CURVE ( 'NONE', #31705, #50394, #9480, .T. ) ;
#15170 = CARTESIAN_POINT ( 'NONE',  ( 12.56594317819999951, -55.54999998572999687, 1.750000000000000000 ) ) ;
#15171 = VECTOR ( 'NONE', #36331, 1000.000000000000000 ) ;
#15172 = CARTESIAN_POINT ( 'NONE',  ( -12.70556836322084848, -25.22772277445464795, 0.2597962961080404476 ) ) ;
#15173 = CARTESIAN_POINT ( 'NONE',  ( -7.601397897754999633, -60.04999999966999980, -9.369164850722000892 ) ) ;
#15174 = CARTESIAN_POINT ( 'NONE',  ( -0.9935076046646102998, -61.76816187723938611, -12.70250268221170309 ) ) ;
#15175 = VECTOR ( 'NONE', #53647, 1000.000000000000000 ) ;
#15176 = CARTESIAN_POINT ( 'NONE',  ( 7.405962610586999340, -77.46393856462499627, -6.270759699041999369 ) ) ;
#15177 = CARTESIAN_POINT ( 'NONE',  ( 0.000000000000000000, -75.19999999999998863, 0.000000000000000000 ) ) ;
#15178 = CARTESIAN_POINT ( 'NONE',  ( 2.094528727916130872, -85.89549859647340213, 3.327249167043359268 ) ) ;
#15179 = CARTESIAN_POINT ( 'NONE',  ( -2.858407197967999913, -79.75000000000000000, -8.797272775729998884 ) ) ;
#15180 = B_SPLINE_SURFACE_WITH_KNOTS ( 'NONE', 3, 3, ( 
 ( #4011, #44761, #22016, #58038, #17598, #4310, #22311, #40327, #53919, #13453, #23481, #45944, #19067, #28483, #10206, #23197, #33199, #41788, #50080, #19356, #46825, #18773, #6056, #41492, #54502, #37349, #55364, #51246, #46534, #24066, #1078, #37055, #10796, #28778, #14620 ),
 ( #55071, #32612, #41202, #6352, #14326, #15207, #32906, #50661, #42084, #1653, #19643, #32323, #27897, #28185, #24368, #14908, #5764, #36476, #37642, #55658, #46239, #23772, #42379, #18483, #792, #14041, #32035, #1359, #9625, #50949, #27613, #36764, #45653, #5194, #54783 ),
 ( #50368, #10499, #9917, #5476, #19942, #52398, #34652, #29074, #47981, #39095, #6938, #2806, #20800, #11669, #34362, #37931, #11952, #47119, #52680, #57103, #38806, #56825, #16671, #16380, #56247, #29930, #6646, #38518, #48269, #7519, #12235, #7226, #11382, #33786, #51537 ),
 ( #30224, #55956, #21092, #7805, #15505, #25806, #43249, #3097, #25516, #1948, #33500, #20520, #11093, #24656, #42666, #2235, #43533, #20233, #38227, #15797, #51828, #47696, #29358, #42961, #47406, #24941, #2517, #56533, #16093, #34074, #52110, #29643, #25229, #57397, #10072 ) ),
 .UNSPECIFIED., .F., .F., .F.,
 ( 4, 4 ),
 ( 4, 1, 1, 1, 1, 1, 1, 1, 1, 1, 1, 1, 1, 1, 1, 1, 1, 1, 1, 1, 1, 1, 1, 1, 1, 1, 1, 1, 1, 1, 1, 1, 4 ),
 ( -0.1387574078320999993, 1.138757407831999968 ),
 ( 0.4815154597993999697, 0.4980358005410999711, 0.5145561412828000281, 0.5310764820244999740, 0.5475968227662000309, 0.5641171635078000568, 0.5806375042495000027, 0.5971578449912000597, 0.6136781857329000056, 0.6301985264746000626, 0.6467188672163000085, 0.6632392079580000654, 0.6797595486996000913, 0.6962798894413000372, 0.7128002301829999832, 0.7293205709246999291, 0.7458409116664000971, 0.7623612524081000430, 0.7788815931497999889, 0.7954019338913999038, 0.8119222746331000717, 0.8284426153748000177, 0.8449629561165000746, 0.8614832968581999095, 0.8780036375998999665, 0.8945239783415001034, 0.9110443190832000493, 0.9275646598248999952, 0.9440850005665999412, 0.9606053413082999981, 0.9771256820500000551, 0.9936460227917000010, 1.010166363533000045 ),
 .UNSPECIFIED. ) ;
#15181 = CARTESIAN_POINT ( 'NONE',  ( -1.320073427535999988, -80.60725624888000596, 0.6433150820290999272 ) ) ;
#15182 = CARTESIAN_POINT ( 'NONE',  ( -8.775882267141646764, -77.51967193750340357, 3.496961574127103400 ) ) ;
#15183 = EDGE_CURVE ( 'NONE', #24970, #55907, #5447, .T. ) ;
#15184 = CARTESIAN_POINT ( 'NONE',  ( 0.01555524843309799218, -76.57477272176625149, 11.74989434732423099 ) ) ;
#15185 = CARTESIAN_POINT ( 'NONE',  ( 12.50745077494999968, -61.79994448255000350, 2.662030659623000237E-09 ) ) ;
#15186 = CARTESIAN_POINT ( 'NONE',  ( -0.9178039125309811475, -79.67705081187436633, 1.199110755174137788 ) ) ;
#15187 = CARTESIAN_POINT ( 'NONE',  ( 4.479242302639000251, -77.90741001420200007, 8.589153267943999026 ) ) ;
#15188 = DIRECTION ( 'NONE',  ( 0.000000000000000000, -0.1122098755727947705, 0.9936845293270585300 ) ) ;
#15189 = CARTESIAN_POINT ( 'NONE',  ( 1.667917367065999912, -18.71943464842000182, -12.49306764015999960 ) ) ;
#15191 = CARTESIAN_POINT ( 'NONE',  ( 1.044910384896000188, -16.94473505805000002, -12.77260826199000121 ) ) ;
#15190 = CARTESIAN_POINT ( 'NONE',  ( 1.000000000000000000, -82.50000000000000000, 0.000000000000000000 ) ) ;
#15192 = LINE ( 'NONE', #33480, #16661 ) ;
#15193 = CARTESIAN_POINT ( 'NONE',  ( 0.000000000000000000, -23.84999999976950136, 11.89999999977000122 ) ) ;
#15194 = CARTESIAN_POINT ( 'NONE',  ( 3.190249742999000215, -2.056098507945999465, -2.075671974272999876 ) ) ;
#15195 = CARTESIAN_POINT ( 'NONE',  ( -1.416116075149735476, -1.657507861446844588, 3.334501019042391157 ) ) ;
#15196 = VERTEX_POINT ( 'NONE', #22180 ) ;
#15197 = CARTESIAN_POINT ( 'NONE',  ( 9.621717088333529233, -61.42064477329430616, 8.060172376500883473 ) ) ;
#15198 = CARTESIAN_POINT ( 'NONE',  ( -9.250000000000000000, -78.99999999999998579, 0.000000000000000000 ) ) ;
#15199 = CARTESIAN_POINT ( 'NONE',  ( -9.799999999999998934, -92.13603921945998820, 1.133246274598000030E-12 ) ) ;
#15200 = CARTESIAN_POINT ( 'NONE',  ( 0.3875071078916553224, -78.45000632268018137, 1.188430056412658642 ) ) ;
#15201 = CARTESIAN_POINT ( 'NONE',  ( -6.529936244858999927, -79.82726403785699176, 7.094943507923000325 ) ) ;
#15202 = CARTESIAN_POINT ( 'NONE',  ( 1.750000000001000089, -19.24922971542000028, -12.60356226396999979 ) ) ;
#15203 = CARTESIAN_POINT ( 'NONE',  ( 7.954951288349001004, -23.44678171330999916, 9.722718241315000398 ) ) ;
#15204 = CARTESIAN_POINT ( 'NONE',  ( -2.513426006153157033, -79.49377681576562793, 10.45203454596306081 ) ) ;
#15205 = CARTESIAN_POINT ( 'NONE',  ( 5.939680743703000668E-14, -6.000000000000000000, 0.000000000000000000 ) ) ;
#15206 = DIRECTION ( 'NONE',  ( 0.000000000000000000, -1.000000000000000000, 0.000000000000000000 ) ) ;
#15207 = CARTESIAN_POINT ( 'NONE',  ( -8.749953746289000023, -77.18972575893728560, 6.935671482060999260 ) ) ;
#15208 = CARTESIAN_POINT ( 'NONE',  ( 0.4316438933813000478, -81.26137701033098892, 1.544936262575999919 ) ) ;
#15209 = CARTESIAN_POINT ( 'NONE',  ( -0.7507646060929270559, -82.02611842029168088, 1.015794618571693064 ) ) ;
#15210 = AXIS2_PLACEMENT_3D ( 'NONE', #15385, #34236, #55534 ) ;
#15211 = CARTESIAN_POINT ( 'NONE',  ( 9.412698430168999764, -77.77175129689300093, 0.1109178415546999974 ) ) ;
#15213 = CARTESIAN_POINT ( 'NONE',  ( -11.69999999991999928, -75.99999999992400035, -2.424604595008000056E-09 ) ) ;
#15212 = CARTESIAN_POINT ( 'NONE',  ( -3.504159990688000104, -82.98328762115399115, -1.353600025171000087 ) ) ;
#15214 = CARTESIAN_POINT ( 'NONE',  ( 5.645287065787000458, -79.51485584965399767, 7.708789581145000014 ) ) ;
#15215 = CARTESIAN_POINT ( 'NONE',  ( -1.500000000000000444, -80.88958333333332007, 0.1963495408493560745 ) ) ;
#15216 = CARTESIAN_POINT ( 'NONE',  ( 5.841136755832899929, -80.27119191073492743, -9.025644075688319390 ) ) ;
#15217 = EDGE_CURVE ( 'NONE', #55158, #31908, #18648, .T. ) ;
#15218 = CARTESIAN_POINT ( 'NONE',  ( -7.595496139713672434, -77.16257047061313301, -7.607272242958681652 ) ) ;
#15219 = CARTESIAN_POINT ( 'NONE',  ( 5.492755654603074689, -79.68750000055037219, -7.555491173184210929 ) ) ;
#15220 = AXIS2_PLACEMENT_3D ( 'NONE', #27933, #6092, #41822 ) ;
#15221 = DIRECTION ( 'NONE',  ( -0.9999999999999694689, -2.469236275681924191E-07, 1.232399280382961306E-12 ) ) ;
#15222 = ORIENTED_EDGE ( 'NONE', *, *, #23189, .F. ) ;
#15223 = VERTEX_POINT ( 'NONE', #53784 ) ;
#15224 = CARTESIAN_POINT ( 'NONE',  ( -11.95950202284999975, -79.19309835455399593, 1.295167635372999948 ) ) ;
#15225 = CARTESIAN_POINT ( 'NONE',  ( 0.3273202981720256255, -78.24590025175641017, -1.217754575872296741 ) ) ;
#15226 = LINE ( 'NONE', #1377, #32218 ) ;
#15227 = ORIENTED_EDGE ( 'NONE', *, *, #42254, .F. ) ;
#15228 = CARTESIAN_POINT ( 'NONE',  ( -6.752419751440000617, -78.20055284899699188, -9.840748444448999876 ) ) ;
#15229 = ORIENTED_EDGE ( 'NONE', *, *, #32581, .F. ) ;
#15230 = ORIENTED_EDGE ( 'NONE', *, *, #46254, .F. ) ;
#15231 = VERTEX_POINT ( 'NONE', #35753 ) ;
#15232 = CARTESIAN_POINT ( 'NONE',  ( 3.345256759276000302, -81.01217470615398497, 1.180600418122999873 ) ) ;
#15233 = CARTESIAN_POINT ( 'NONE',  ( 1.574959781464393860, -79.26172491759977845, 9.368679406100806517 ) ) ;
#15234 = ORIENTED_EDGE ( 'NONE', *, *, #11201, .F. ) ;
#15235 = CARTESIAN_POINT ( 'NONE',  ( 0.09617818635378815040, -82.73177828884955431, -1.246062951507001415 ) ) ;
#15236 = ORIENTED_EDGE ( 'NONE', *, *, #15522, .T. ) ;
#15237 = AXIS2_PLACEMENT_3D ( 'NONE', #31095, #451, #40271 ) ;
#15238 = CARTESIAN_POINT ( 'NONE',  ( -1.287989364273000037, -2.461525618456000153, 3.148088515452999836 ) ) ;
#15240 = ORIENTED_EDGE ( 'NONE', *, *, #12974, .F. ) ;
#15239 = ADVANCED_FACE ( 'NONE', ( #54656 ), #14196, .F. ) ;
#15241 = CARTESIAN_POINT ( 'NONE',  ( -5.685171361304339754, -79.17317559803932170, -7.397381645113899395 ) ) ;
#15242 = CARTESIAN_POINT ( 'NONE',  ( 1.445648592326100879, -79.02717926386495151, 0.5087904774525755514 ) ) ;
#15243 = CARTESIAN_POINT ( 'NONE',  ( -0.8507363746134872784, -79.80000000000001137, -11.77153046305032902 ) ) ;
#15244 = CARTESIAN_POINT ( 'NONE',  ( -12.50483450108329642, -17.13545459011075422, 0.6958188036703752966 ) ) ;
#15245 = CARTESIAN_POINT ( 'NONE',  ( 1.882180247600000245, -78.60946749706478442, 9.519879562373999349 ) ) ;
#15246 = CARTESIAN_POINT ( 'NONE',  ( -10.07624512687999996, -76.23402931670899818, -4.852130239470000106 ) ) ;
#15247 = FACE_OUTER_BOUND ( 'NONE', #51277, .T. ) ;
#15248 = CARTESIAN_POINT ( 'NONE',  ( 0.3271848554491016414, -81.14583333333331439, -1.217465845835393967 ) ) ;
#15249 = B_SPLINE_CURVE_WITH_KNOTS ( 'NONE', 3,
 ( #18042, #22752, #31591, #45498, #49634, #9181, #27166, #5044, #23043, #41058, #36620, #23913, #33639, #11228, #15056, #46379, #15934, #42230 ),
 .UNSPECIFIED., .F., .F.,
 ( 4, 2, 2, 2, 2, 2, 2, 2, 4 ),
 ( 0.000000000000000000, 0.1250000000000000000, 0.2500000000000000000, 0.3750000000000000000, 0.5000000000000000000, 0.6250000000000000000, 0.7500000000000000000, 0.8750000000000000000, 1.000000000000000000 ),
 .UNSPECIFIED. ) ;
#15250 = CARTESIAN_POINT ( 'NONE',  ( -10.71544265974000076, -76.80223585847799939, 2.915930582825000172 ) ) ;
#15251 = EDGE_CURVE ( 'NONE', #52629, #800, #53482, .T. ) ;
#15252 = CARTESIAN_POINT ( 'NONE',  ( -4.009976957963860222, -78.68938149694008644, -8.341196569951419448 ) ) ;
#15253 = CARTESIAN_POINT ( 'NONE',  ( 6.622872397097998132, -76.52713920344137932, 9.705607225355446843 ) ) ;
#15254 = CARTESIAN_POINT ( 'NONE',  ( 0.4820079653409431453, -23.51614597298007681, -10.98957811953319563 ) ) ;
#15255 = CARTESIAN_POINT ( 'NONE',  ( 1.137658753740000028, -79.42802612664000605, 0.6959227610743999870 ) ) ;
#15256 = ADVANCED_FACE ( 'NONE', ( #44921 ), #12029, .F. ) ;
#15257 = CARTESIAN_POINT ( 'NONE',  ( -7.623780002575291093, -80.16446064207195832, -7.929242475467390250 ) ) ;
#15258 = CARTESIAN_POINT ( 'NONE',  ( -3.002690198994237392, -3.070074872230420748, 1.241492466252928750 ) ) ;
#15259 = CARTESIAN_POINT ( 'NONE',  ( -3.276814203403000114, -78.43767549782629089, 1.049547044727999978 ) ) ;
#15260 = CARTESIAN_POINT ( 'NONE',  ( 7.475611960616999951, -79.75467010736198858, -9.493926176044999110 ) ) ;
#15261 = AXIS2_PLACEMENT_3D ( 'NONE', #36207, #23499, #50388 ) ;
#15262 = CARTESIAN_POINT ( 'NONE',  ( 11.37395959471070483, -76.22187500001194849, 3.693278803254645748 ) ) ;
#15263 = CARTESIAN_POINT ( 'NONE',  ( -0.4818985169295156301, -83.00656079444637214, 1.153343561654186722 ) ) ;
#15264 = CARTESIAN_POINT ( 'NONE',  ( -8.852458463678310352, -76.25659527127551485, -7.727683512292325752 ) ) ;
#15265 = CARTESIAN_POINT ( 'NONE',  ( 0.000000000000000000, -86.39999999999999147, 0.000000000000000000 ) ) ;
#15266 = CARTESIAN_POINT ( 'NONE',  ( 1.199999995295999877, -81.00000000470399186, -6.999999972240000368 ) ) ;
#15267 = CARTESIAN_POINT ( 'NONE',  ( -8.954424297038181990, -79.62125597785718867, -2.398079499860812369 ) ) ;
#15268 = CARTESIAN_POINT ( 'NONE',  ( 1.304222966381000104, -81.40108199494899566, 0.2785293583740000023 ) ) ;
#15269 = CARTESIAN_POINT ( 'NONE',  ( -8.768124086712999699, -59.94999999969000015, 7.919595949288999570 ) ) ;
#15270 = CARTESIAN_POINT ( 'NONE',  ( 0.000000000000000000, -87.09999999999999432, 0.000000000000000000 ) ) ;
#15271 = CARTESIAN_POINT ( 'NONE',  ( -9.164385193226218362, -25.21567483134532139, -8.803702036953628962 ) ) ;
#15272 = CARTESIAN_POINT ( 'NONE',  ( -3.664701384210835577, -77.85298049213145077, 10.19847459208089724 ) ) ;
#15273 = CARTESIAN_POINT ( 'NONE',  ( 0.000000000000000000, -55.54999999966999980, -12.50000000000000000 ) ) ;
#15274 = B_SPLINE_CURVE_WITH_KNOTS ( 'NONE', 3,
 ( #19443, #47493, #6145, #20601, #19734, #11466, #55752, #37435, #56041, #55155, #24155, #14998, #28275, #24451, #29438, #32994, #51040, #10587 ),
 .UNSPECIFIED., .F., .F.,
 ( 4, 2, 2, 2, 2, 2, 2, 2, 4 ),
 ( 0.000000000000000000, 0.1250000000000000000, 0.2500000000000000000, 0.3750000000000000000, 0.5000000000000000000, 0.6250000000000000000, 0.7500000000000000000, 0.8750000000000000000, 1.000000000000000000 ),
 .UNSPECIFIED. ) ;
#15275 = CARTESIAN_POINT ( 'NONE',  ( 7.218984044805001332, -79.16787878630005082, 8.267423174273998754 ) ) ;
#15276 = CARTESIAN_POINT ( 'NONE',  ( 11.29076395134999977, -76.98561308323999697, -2.900214329540999891 ) ) ;
#15277 = EDGE_LOOP ( 'NONE', ( #29947, #4705, #50447, #42397, #20038 ) ) ;
#15278 = CARTESIAN_POINT ( 'NONE',  ( -3.724883260595999612, -85.03571544543099492, -0.4864224331464999662 ) ) ;
#15279 = CARTESIAN_POINT ( 'NONE',  ( -3.071993112688999883, -80.60579489507729534, 10.86300919910000040 ) ) ;
#15280 = CARTESIAN_POINT ( 'NONE',  ( 9.250000000000000000, -78.34999999999999432, 0.000000000000000000 ) ) ;
#15281 = CARTESIAN_POINT ( 'NONE',  ( -12.00000000000000000, -55.54999999966999980, 0.000000000000000000 ) ) ;
#15282 = CARTESIAN_POINT ( 'NONE',  ( -9.457500717944000712, -78.44685747529899800, -6.031068363571000290 ) ) ;
#15283 = CARTESIAN_POINT ( 'NONE',  ( 12.46164872704999915, -55.12834420008999814, -1.631615798669999950 ) ) ;
#15284 = CARTESIAN_POINT ( 'NONE',  ( 5.053427186728000287, -78.72410532222798452, 8.198541555267000902 ) ) ;
#15285 = B_SPLINE_CURVE_WITH_KNOTS ( 'NONE', 3,
 ( #2783, #47680, #24924, #24350 ),
 .UNSPECIFIED., .F., .F.,
 ( 4, 4 ),
 ( 0.000000000000000000, 1.000000000000000000 ),
 .UNSPECIFIED. ) ;
#15286 = CARTESIAN_POINT ( 'NONE',  ( 4.043181936102999252, -84.02832601947699231, 1.029191484053000094 ) ) ;
#15287 = CARTESIAN_POINT ( 'NONE',  ( 5.519612068167639052, -80.24166666702031137, -9.574916337700171809 ) ) ;
#15288 = VERTEX_POINT ( 'NONE', #5925 ) ;
#15289 = ADVANCED_FACE ( 'NONE', ( #51405 ), #45584, .F. ) ;
#15290 = CARTESIAN_POINT ( 'NONE',  ( 0.000000000000000000, -80.74999999950000529, 0.000000000000000000 ) ) ;
#15291 = CARTESIAN_POINT ( 'NONE',  ( -8.418594644163000851, -80.75615502098555964, -7.485750452785000064 ) ) ;
#15292 = CARTESIAN_POINT ( 'NONE',  ( 2.595899973196303723, -78.97680030866433754, -2.796371309837623720 ) ) ;
#15293 = EDGE_LOOP ( 'NONE', ( #49754, #45436, #48422, #14455 ) ) ;
#15294 = ADVANCED_FACE ( 'NONE', ( #41597 ), #58269, .F. ) ;
#15295 = CARTESIAN_POINT ( 'NONE',  ( -0.2406813341972999787, -78.74489846623899325, -1.311734976874999958 ) ) ;
#15296 = CARTESIAN_POINT ( 'NONE',  ( -7.558619072263999428, -78.87198591599799613, -8.058856703501000140 ) ) ;
#15297 = CARTESIAN_POINT ( 'NONE',  ( 12.60413652834999887, -60.10716934574000447, 1.799502287743000029 ) ) ;
#15298 = CARTESIAN_POINT ( 'NONE',  ( 4.046534287111000161, -79.83266315943599523, -10.82105705926999839 ) ) ;
#15299 = ORIENTED_EDGE ( 'NONE', *, *, #44940, .F. ) ;
#15300 = CARTESIAN_POINT ( 'NONE',  ( 7.599120132820000428, -78.58017081663599868, 9.499258065358000991 ) ) ;
#15301 = CARTESIAN_POINT ( 'NONE',  ( 9.338174682402000215, -77.82187845315299057, -6.595492338295000145 ) ) ;
#15302 = CARTESIAN_POINT ( 'NONE',  ( -10.98753362943491929, -23.45184359403960528, -0.5244447725538564642 ) ) ;
#15304 = EDGE_LOOP ( 'NONE', ( #35395, #29957, #40225, #1457 ) ) ;
#15303 = VECTOR ( 'NONE', #47085, 1000.000000000000000 ) ;
#15305 = ORIENTED_EDGE ( 'NONE', *, *, #5534, .T. ) ;
#15306 = ORIENTED_EDGE ( 'NONE', *, *, #24648, .T. ) ;
#15307 = CARTESIAN_POINT ( 'NONE',  ( 0.4701211166820882248, -80.44441647165540132, 1.158161630332676273 ) ) ;
#15308 = AXIS2_PLACEMENT_3D ( 'NONE', #38975, #25111, #34530 ) ;
#15309 = CARTESIAN_POINT ( 'NONE',  ( 9.393383141732488895, -77.80837651054207527, -5.413844486429424840 ) ) ;
#15310 = CARTESIAN_POINT ( 'NONE',  ( 9.226480760116999136, -79.12131249856399506, -2.263195259622999611 ) ) ;
#15311 = ORIENTED_EDGE ( 'NONE', *, *, #17826, .T. ) ;
#15312 = CARTESIAN_POINT ( 'NONE',  ( 12.83675912438999944, -55.57244613998999938, 2.062833085520999976 ) ) ;
#15313 = CARTESIAN_POINT ( 'NONE',  ( -10.90022919700999893, -78.56903125995000892, 0.6003077901278000006 ) ) ;
#15314 = ORIENTED_EDGE ( 'NONE', *, *, #31742, .T. ) ;
#15315 = CARTESIAN_POINT ( 'NONE',  ( -12.43652404745000162, -24.92065244538000002, -0.1284256373645999982 ) ) ;
#15316 = CARTESIAN_POINT ( 'NONE',  ( -1.269916711065999904, -77.12416915034599185, -9.409822520238998678 ) ) ;
#15317 = FACE_BOUND ( 'NONE', #22109, .T. ) ;
#15318 = VECTOR ( 'NONE', #36130, 999.9999999999998863 ) ;
#15319 = CARTESIAN_POINT ( 'NONE',  ( -1.145477160176213927, -80.13298459133737595, -0.5001054580953478990 ) ) ;
#15320 = CARTESIAN_POINT ( 'NONE',  ( -7.674627477118999508, -59.55077028051999832, 10.14950121126999960 ) ) ;
#15321 = CARTESIAN_POINT ( 'NONE',  ( 4.599093535406832522, -78.71332913613842663, -8.568652848198281546 ) ) ;
#15322 = AXIS2_PLACEMENT_3D ( 'NONE', #22454, #4453, #30711 ) ;
#15323 = CARTESIAN_POINT ( 'NONE',  ( -9.641544011188999619, -77.26545691997898757, 0.6359099666973999643 ) ) ;
#15324 = CARTESIAN_POINT ( 'NONE',  ( -1.522056959221183225, -78.83826870896211858, 0.2244679071987824293 ) ) ;
#15325 = EDGE_CURVE ( 'NONE', #3325, #21397, #51658, .T. ) ;
#15326 = CARTESIAN_POINT ( 'NONE',  ( 0.2808874063080823991, -82.09166668342933804, -4.003087784603879484 ) ) ;
#15327 = CARTESIAN_POINT ( 'NONE',  ( 12.02702378446000075, -75.72388651151999284, -1.341316611471999876 ) ) ;
#15328 = CARTESIAN_POINT ( 'NONE',  ( 10.47020627418439531, -77.72916666666667140, -2.813789756862242974 ) ) ;
#15329 = EDGE_CURVE ( 'NONE', #15756, #45004, #12293, .T. ) ;
#15330 = B_SPLINE_CURVE_WITH_KNOTS ( 'NONE', 3,
 ( #42897, #25739, #7741, #21027 ),
 .UNSPECIFIED., .F., .F.,
 ( 4, 4 ),
 ( 0.000000000000000000, 1.000000000000000000 ),
 .UNSPECIFIED. ) ;
#15331 = DIRECTION ( 'NONE',  ( -1.000000000000000000, 0.000000000000000000, 0.000000000000000000 ) ) ;
#15332 = DIRECTION ( 'NONE',  ( -0.7071067811865474617, 0.000000000000000000, -0.7071067811865474617 ) ) ;
#15333 = CARTESIAN_POINT ( 'NONE',  ( 7.081057523560999378, -79.12198300536000772, -10.01287680343000019 ) ) ;
#15334 = CARTESIAN_POINT ( 'NONE',  ( -1.925872869407999843, -76.74636341947798712, -12.12904120624999926 ) ) ;
#15335 = CARTESIAN_POINT ( 'NONE',  ( -7.664266801483791802, -60.54946977258678231, -7.892048199457517121 ) ) ;
#15336 = CARTESIAN_POINT ( 'NONE',  ( 2.461679710009094801, -2.793789481889469961, -2.122462569764226092 ) ) ;
#15337 = CARTESIAN_POINT ( 'NONE',  ( 10.10840608942275942, -77.75407225199086270, -6.586910062449264913 ) ) ;
#15338 = CARTESIAN_POINT ( 'NONE',  ( 10.54265532893000312, -78.52773149672268005, 3.830212845596999927 ) ) ;
#15339 = ORIENTED_EDGE ( 'NONE', *, *, #1740, .T. ) ;
#15340 = CARTESIAN_POINT ( 'NONE',  ( -1.223837560276999969, -82.48513558557799286, 0.5728811815464999180 ) ) ;
#15341 = CARTESIAN_POINT ( 'NONE',  ( 5.450064804415999831, -77.22001278094698762, 7.901637168149001411 ) ) ;
#15342 = CARTESIAN_POINT ( 'NONE',  ( 0.5999999999999999778, -23.15000000000999947, -11.79999999999999893 ) ) ;
#15343 = VECTOR ( 'NONE', #47232, 1000.000000000000000 ) ;
#15344 = CARTESIAN_POINT ( 'NONE',  ( -1.092232985442824100, -82.95833333333330017, 0.6295237254636200097 ) ) ;
#15345 = FACE_OUTER_BOUND ( 'NONE', #37666, .T. ) ;
#15346 = CARTESIAN_POINT ( 'NONE',  ( -10.67791114319000023, -78.54720534002599663, -5.583725037239000599 ) ) ;
#15347 = CARTESIAN_POINT ( 'NONE',  ( 3.260206397764000119, -78.11865170860198759, 9.177731198418999981 ) ) ;
#15348 = EDGE_CURVE ( 'NONE', #17469, #11901, #1676, .T. ) ;
#15350 = CARTESIAN_POINT ( 'NONE',  ( 0.000000000000000000, -77.04999999999999716, 0.000000000000000000 ) ) ;
#15349 = CARTESIAN_POINT ( 'NONE',  ( -6.183423720564950266, -76.11889232786028003, 10.01094227326205122 ) ) ;
#15351 = CARTESIAN_POINT ( 'NONE',  ( 0.5930780265196999856, -81.91886708904999637, 1.214178601635999888 ) ) ;
#15352 = CARTESIAN_POINT ( 'NONE',  ( -10.58864275599752958, -79.58633413285787128, 1.856070104963200906 ) ) ;
#15353 = ORIENTED_EDGE ( 'NONE', *, *, #51262, .F. ) ;
#15354 = CARTESIAN_POINT ( 'NONE',  ( 0.9995835529977264988, -82.19791666666664298, -0.7681833999686417114 ) ) ;
#15355 = CIRCLE ( 'NONE', #8763, 1.250000000000000444 ) ;
#15356 = CARTESIAN_POINT ( 'NONE',  ( 0.5999999999999999778, -5.000000000000000000, 0.5999999999999999778 ) ) ;
#15357 = DIRECTION ( 'NONE',  ( 0.9999999999995751176, 0.000000000000000000, 9.217549102787771002E-07 ) ) ;
#15358 = CARTESIAN_POINT ( 'NONE',  ( -3.548303639235999896, -79.58925716643398118, -10.38621961377000069 ) ) ;
#15359 = FACE_OUTER_BOUND ( 'NONE', #28680, .T. ) ;
#15360 = CARTESIAN_POINT ( 'NONE',  ( -4.085185354070000940, -80.05359608450199005, 8.504900574379000489 ) ) ;
#15361 = CARTESIAN_POINT ( 'NONE',  ( 8.478741751137999216, -17.12187496603999648, -9.108230428607001272 ) ) ;
#15362 = FACE_OUTER_BOUND ( 'NONE', #36275, .T. ) ;
#15363 = ORIENTED_EDGE ( 'NONE', *, *, #13935, .F. ) ;
#15365 = AXIS2_PLACEMENT_3D ( 'NONE', #15496, #56812, #34350 ) ;
#15364 = CARTESIAN_POINT ( 'NONE',  ( -11.08513710546999853, -79.26246662722100211, 1.988391287278999942 ) ) ;
#15366 = CARTESIAN_POINT ( 'NONE',  ( 8.899186938124000079, -76.04999999999999716, -6.465637775218000094 ) ) ;
#15367 = CARTESIAN_POINT ( 'NONE',  ( 11.83165817387121876, -79.30168238477698139, 0.2954418266251981340 ) ) ;
#15368 = CARTESIAN_POINT ( 'NONE',  ( 3.407095545933004122, -78.62148120184446043, -4.172488654716057829E-16 ) ) ;
#15369 = CARTESIAN_POINT ( 'NONE',  ( 11.19652597747931289, -77.73269495442998789, 4.381814868441350264 ) ) ;
#15370 = EDGE_CURVE ( 'NONE', #26684, #47937, #15114, .T. ) ;
#15371 = VECTOR ( 'NONE', #19069, 1000.000000000000227 ) ;
#15372 = CARTESIAN_POINT ( 'NONE',  ( 1.249826681154805552, -81.35774364365171607, 0.1170858793740336135 ) ) ;
#15373 = CARTESIAN_POINT ( 'NONE',  ( -1.268608120215463542, -78.14294593744003237, 0.1161361650036817905 ) ) ;
#15374 = PLANE ( 'NONE',  #10971 ) ;
#15375 = CARTESIAN_POINT ( 'NONE',  ( 3.872097870353349514, -82.21166587810114379, -0.8230394299192180796 ) ) ;
#15376 = FACE_OUTER_BOUND ( 'NONE', #40415, .T. ) ;
#15377 = CARTESIAN_POINT ( 'NONE',  ( -7.022618521819972592, -79.38035044383605054, 8.435084348146190791 ) ) ;
#15378 = CARTESIAN_POINT ( 'NONE',  ( 12.70556836343000029, -53.57227722738999631, -1.774194422348999890E-09 ) ) ;
#15379 = ORIENTED_EDGE ( 'NONE', *, *, #50576, .F. ) ;
#15380 = VERTEX_POINT ( 'NONE', #7038 ) ;
#15381 = CARTESIAN_POINT ( 'NONE',  ( 5.441664396738000065, -79.05162331913099649, -8.019902302782998760 ) ) ;
#15382 = CARTESIAN_POINT ( 'NONE',  ( 9.994252366402587739, -78.82006649457892422, -3.959790582201482501 ) ) ;
#15383 = CIRCLE ( 'NONE', #56854, 0.5000000000000004441 ) ;
#15384 = ORIENTED_EDGE ( 'NONE', *, *, #15749, .F. ) ;
#15385 = CARTESIAN_POINT ( 'NONE',  ( -1.392423410630999929E-14, -75.80000000000001137, 0.000000000000000000 ) ) ;
#15386 = CARTESIAN_POINT ( 'NONE',  ( -10.09604776472000154, -78.19984377886000004, 6.324672719602999926 ) ) ;
#15387 = CARTESIAN_POINT ( 'NONE',  ( 12.50000000000000000, -60.04999999966999980, 0.000000000000000000 ) ) ;
#15388 = DIRECTION ( 'NONE',  ( -1.000000000000000000, 0.000000000000000000, 0.000000000000000000 ) ) ;
#15389 = CARTESIAN_POINT ( 'NONE',  ( -11.74114114509063533, -78.53398672592838636, 2.380251238623568799 ) ) ;
#15390 = AXIS2_PLACEMENT_3D ( 'NONE', #44003, #21266, #3553 ) ;
#15391 = CARTESIAN_POINT ( 'NONE',  ( 5.622824352109999424, -80.06846743556140211, -9.705769245306999693 ) ) ;
#15392 = EDGE_LOOP ( 'NONE', ( #28797, #37580, #28725 ) ) ;
#15393 = CARTESIAN_POINT ( 'NONE',  ( 12.00000000000000000, -23.25000000000000000, 1.250000000000000000 ) ) ;
#15394 = VERTEX_POINT ( 'NONE', #25898 ) ;
#15395 = CARTESIAN_POINT ( 'NONE',  ( 7.430943141216144632, -77.40086315431187813, 5.508475347222059781 ) ) ;
#15396 = CARTESIAN_POINT ( 'NONE',  ( 6.574300740938999077, -77.66621510448898391, -8.869200617850999890 ) ) ;
#15397 = CARTESIAN_POINT ( 'NONE',  ( -10.58742881249942869, -77.82311968649129597, 3.705126192729017109 ) ) ;
#15398 = UNCERTAINTY_MEASURE_WITH_UNIT (LENGTH_MEASURE( 1.000000000000000082E-05 ), #35539, 'distance_accuracy_value', 'NONE');
#15399 = CARTESIAN_POINT ( 'NONE',  ( 1.482146596920999926, -77.70947474015589762, -0.6406678853001999130 ) ) ;
#15400 = CIRCLE ( 'NONE', #45594, 9.700000000000001066 ) ;
#15401 = CARTESIAN_POINT ( 'NONE',  ( 11.08637824332000044, -76.46937053406000473, -3.603444353441000114 ) ) ;
#15402 = DIRECTION ( 'NONE',  ( 1.000000000000000000, 0.000000000000000000, 0.000000000000000000 ) ) ;
#15403 = CARTESIAN_POINT ( 'NONE',  ( -0.6794254437148999903, -78.97955343955000274, -1.478865823597000029 ) ) ;
#15404 = AXIS2_PLACEMENT_3D ( 'NONE', #3237, #57246, #56961 ) ;
#15405 = CARTESIAN_POINT ( 'NONE',  ( 10.81514082164000001, -79.22666430121098813, -2.260668630147000258 ) ) ;
#15406 = CARTESIAN_POINT ( 'NONE',  ( 7.648026768036999989, -60.04999998387000204, 10.12290050219000115 ) ) ;
#15407 = PRESENTATION_STYLE_ASSIGNMENT (( #10990 ) ) ;
#15408 = CARTESIAN_POINT ( 'NONE',  ( 0.000000000000000000, -39.30476017083000073, 0.000000000000000000 ) ) ;
#15409 = CARTESIAN_POINT ( 'NONE',  ( -2.847992527146999908, -83.06632269734298291, 2.115064691465000202 ) ) ;
#15410 = VERTEX_POINT ( 'NONE', #29453 ) ;
#15411 = CARTESIAN_POINT ( 'NONE',  ( -10.17815165094191165, -77.19999999999998863, 4.038522141417139721 ) ) ;
#15412 = CARTESIAN_POINT ( 'NONE',  ( 0.4877854313978999268, -80.47814348455999323, -1.631527605715999973 ) ) ;
#15413 = CARTESIAN_POINT ( 'NONE',  ( 0.4922963458217056165, -77.97152273167989733, 10.74989978380444811 ) ) ;
#15414 = CARTESIAN_POINT ( 'NONE',  ( 3.249499231398999655, -78.71296479287700265, -11.53069031867000049 ) ) ;
#15415 = CARTESIAN_POINT ( 'NONE',  ( -7.619712398446999657, -18.59595871862000038, 10.35409979026999849 ) ) ;
#15416 = CARTESIAN_POINT ( 'NONE',  ( 1.030546858859699766, -78.44986307349660137, -0.7510367337251727671 ) ) ;
#15417 = CARTESIAN_POINT ( 'NONE',  ( 2.464672433998302381, -3.436673042811343670, -2.513837925488545455 ) ) ;
#15418 = CARTESIAN_POINT ( 'NONE',  ( -5.099999999822000696, -75.20000000017779485, 7.533999751109999828E-10 ) ) ;
#15419 = CARTESIAN_POINT ( 'NONE',  ( -4.724527880064000485, -78.55937680961498870, 8.267358256580001452 ) ) ;
#15421 = EDGE_CURVE ( 'NONE', #39914, #11684, #20052, .T. ) ;
#15420 = CARTESIAN_POINT ( 'NONE',  ( -0.9465222407332000154, -81.15663953506998496, -0.8164530897714000757 ) ) ;
#15422 = CARTESIAN_POINT ( 'NONE',  ( 10.83471462526000018, -77.22393005650599207, 2.076220934837999632 ) ) ;
#15423 = CARTESIAN_POINT ( 'NONE',  ( 4.297951556683999641, -76.80344829822820429, -11.50435740523999861 ) ) ;
#15424 = CARTESIAN_POINT ( 'NONE',  ( -6.043427764450786555, -78.38333333333332575, -10.48543666025110177 ) ) ;
#15425 = ORIENTED_EDGE ( 'NONE', *, *, #30633, .F. ) ;
#15426 = CARTESIAN_POINT ( 'NONE',  ( -0.4870599102559999838, -82.31550708645799830, -1.180149847382000017 ) ) ;
#15427 = CARTESIAN_POINT ( 'NONE',  ( -1.044910384896000188, -61.85526494161999977, -12.77260826204000033 ) ) ;
#15428 = LINE ( 'NONE', #51459, #6934 ) ;
#15429 = CARTESIAN_POINT ( 'NONE',  ( -6.884807209879999057, -78.40630526502499720, -8.855368954042999619 ) ) ;
#15430 = CARTESIAN_POINT ( 'NONE',  ( -10.65673661723999999, -78.79031659410199495, 2.626400817186000047 ) ) ;
#15431 = CARTESIAN_POINT ( 'NONE',  ( 7.647735717248999698, -23.72294882383999948, -10.13404777202000062 ) ) ;
#15432 = CARTESIAN_POINT ( 'NONE',  ( -3.296924740810961207, -83.05520832018719091, 2.288194650150326748 ) ) ;
#15433 = CARTESIAN_POINT ( 'NONE',  ( -10.09635298639777723, -60.32373519955906715, 7.644087781989489905 ) ) ;
#15434 = CARTESIAN_POINT ( 'NONE',  ( 9.000350940039702152, -78.50278833705510806, 7.564101958034004980 ) ) ;
#15435 = CARTESIAN_POINT ( 'NONE',  ( -8.274781782374516226, -53.82110650087535220, -9.689260013561808549 ) ) ;
#15436 = VERTEX_POINT ( 'NONE', #45092 ) ;
#15437 = CARTESIAN_POINT ( 'NONE',  ( -0.1383183815461396793, -79.98410570061048475, 1.242547978336307368 ) ) ;
#15438 = CARTESIAN_POINT ( 'NONE',  ( -7.624341766629000539, -55.53514853726999689, 10.42531125022999916 ) ) ;
#15439 = ADVANCED_FACE ( 'NONE', ( #26467 ), #31476, .T. ) ;
#15440 = AXIS2_PLACEMENT_3D ( 'NONE', #16807, #52816, #28925 ) ;
#15441 = CARTESIAN_POINT ( 'NONE',  ( 7.618386520025000053, -55.57287536619999457, -10.53495200518000097 ) ) ;
#15442 = CARTESIAN_POINT ( 'NONE',  ( 11.23689443680000011, -77.53191129495199618, 0.7524413429202000403 ) ) ;
#15443 = CARTESIAN_POINT ( 'NONE',  ( 0.09717712410696000003, -79.38911183579999431, 1.316523976680999963 ) ) ;
#15444 = LINE ( 'NONE', #33438, #39562 ) ;
#15445 = CARTESIAN_POINT ( 'NONE',  ( -0.9969507628167146862, -82.31880644388637336, -1.182831566122873879 ) ) ;
#15446 = CARTESIAN_POINT ( 'NONE',  ( -13.98934701301999972, -32.57813015402999923, -1.420884290613999911E-05 ) ) ;
#15447 = B_SPLINE_CURVE_WITH_KNOTS ( 'NONE', 3,
 ( #22954, #32088, #49538, #31491, #45109, #4662, #9966, #840, #22662, #37104 ),
 .UNSPECIFIED., .F., .F.,
 ( 4, 2, 2, 2, 4 ),
 ( 0.000000000000000000, 0.2500000000000000000, 0.5000000000000000000, 0.7500000000000000000, 1.000000000000000000 ),
 .UNSPECIFIED. ) ;
#15448 = CARTESIAN_POINT ( 'NONE',  ( -1.980464483675000054, -20.24439829391000245, -12.85140862646999871 ) ) ;
#15449 = VECTOR ( 'NONE', #54046, 1000.000000000000000 ) ;
#15450 = CARTESIAN_POINT ( 'NONE',  ( 1.199500263597271577, -78.09791666666667709, -0.9218200799623702535 ) ) ;
#15451 = EDGE_CURVE ( 'NONE', #27560, #29877, #49640, .T. ) ;
#15452 = ORIENTED_EDGE ( 'NONE', *, *, #4244, .F. ) ;
#15453 = CARTESIAN_POINT ( 'NONE',  ( -0.8609083542497767416, -81.66505337382136531, -0.9059207732458428586 ) ) ;
#15454 =( NAMED_UNIT ( * ) PLANE_ANGLE_UNIT ( ) SI_UNIT ( $, .RADIAN. ) );
#15455 = EDGE_CURVE ( 'NONE', #42095, #41372, #9949, .T. ) ;
#15456 = CARTESIAN_POINT ( 'NONE',  ( 10.47694508628999976, -78.66886758034799243, 3.806339902057000124 ) ) ;
#15457 = DIRECTION ( 'NONE',  ( 0.000000000000000000, -1.000000000000000000, 0.000000000000000000 ) ) ;
#15458 = ORIENTED_EDGE ( 'NONE', *, *, #22500, .F. ) ;
#15459 = ORIENTED_EDGE ( 'NONE', *, *, #31708, .F. ) ;
#15460 = CARTESIAN_POINT ( 'NONE',  ( -0.2635301427987000178, -82.15747177493101105, -1.396495434320000006 ) ) ;
#15461 = EDGE_LOOP ( 'NONE', ( #34734, #36508, #48221, #37369 ) ) ;
#15462 = ORIENTED_EDGE ( 'NONE', *, *, #17570, .F. ) ;
#15463 = CARTESIAN_POINT ( 'NONE',  ( 2.065394024360999836, -18.57838567354000148, 12.82193048528000112 ) ) ;
#15464 = CARTESIAN_POINT ( 'NONE',  ( 0.5999999999999999778, -5.200000000000000178, -0.5999999999999999778 ) ) ;
#15465 = APPLICATION_PROTOCOL_DEFINITION ( 'draft international standard', 'automotive_design', 1998, #55283 ) ;
#15466 = CARTESIAN_POINT ( 'NONE',  ( -13.13047446164998711, -59.58578169018999660, 0.8260994316375004365 ) ) ;
#15467 = CARTESIAN_POINT ( 'NONE',  ( 4.448768332841000372, -79.15906001420199800, 8.980869306721999124 ) ) ;
#15468 = CARTESIAN_POINT ( 'NONE',  ( 5.148067466022420824, -78.27213350022245208, -7.684922334373290198 ) ) ;
#15469 = CARTESIAN_POINT ( 'NONE',  ( 5.622824352109999424, -79.86510177573269686, -9.705769245306999693 ) ) ;
#15470 = ORIENTED_EDGE ( 'NONE', *, *, #54006, .F. ) ;
#15471 = VERTEX_POINT ( 'NONE', #37963 ) ;
#15472 = CARTESIAN_POINT ( 'NONE',  ( 4.000000000000000000, -75.00000000000001421, 0.5999999999999999778 ) ) ;
#15473 = CARTESIAN_POINT ( 'NONE',  ( 3.250000000000000000, -3.350000000000000089, 0.000000000000000000 ) ) ;
#15474 = EDGE_CURVE ( 'NONE', #47432, #42525, #47566, .T. ) ;
#15475 = DIRECTION ( 'NONE',  ( -0.7071067811865474617, 0.7071067811865474617, -2.341635337278152801E-09 ) ) ;
#15476 = CARTESIAN_POINT ( 'NONE',  ( -8.073459667400001649, -78.31665343849398653, -5.384232384047000330 ) ) ;
#15477 = LINE ( 'NONE', #24036, #45484 ) ;
#15478 = CARTESIAN_POINT ( 'NONE',  ( 1.750000000000000000, -20.24935285954000008, 12.65372179284999810 ) ) ;
#15479 = CARTESIAN_POINT ( 'NONE',  ( -8.012523733904361123, -77.36708638852499575, -8.990154430768210858 ) ) ;
#15480 = CARTESIAN_POINT ( 'NONE',  ( 0.3786699527928999442, -79.91281982998998501, -1.660248773968999947 ) ) ;
#15481 = AXIS2_PLACEMENT_3D ( 'NONE', #30953, #26531, #7960 ) ;
#15482 = CARTESIAN_POINT ( 'NONE',  ( -8.278253510431028417, -76.63709233168063406, 8.338544273060703560 ) ) ;
#15483 = CARTESIAN_POINT ( 'NONE',  ( 1.878467530605369307, -79.21093747608632896, -11.84982925898997230 ) ) ;
#15484 = CARTESIAN_POINT ( 'NONE',  ( 1.509159946879168546, -79.50498243737588666, 0.09554436634639965065 ) ) ;
#15485 = CARTESIAN_POINT ( 'NONE',  ( 9.909302118288000116, -78.69441332859899774, 0.1618955519762999840 ) ) ;
#15486 = CARTESIAN_POINT ( 'NONE',  ( -7.283709231223095770, -80.36666666667369441, -8.098811904880690804 ) ) ;
#15487 = CARTESIAN_POINT ( 'NONE',  ( 1.667961445601999992, -20.25199022618999933, -12.58338334675000070 ) ) ;
#15489 = CARTESIAN_POINT ( 'NONE',  ( 1.460729357738999923, -17.90908756796999768, -12.44211643240000065 ) ) ;
#15488 = CARTESIAN_POINT ( 'NONE',  ( -7.601397897754999633, -23.24999999688999708, -10.07627163191000008 ) ) ;
#15490 = CARTESIAN_POINT ( 'NONE',  ( 0.000000000000000000, -92.13603921945998820, 0.000000000000000000 ) ) ;
#15491 = DIRECTION ( 'NONE',  ( -0.7071067811865475727, 0.000000000000000000, 0.7071067811865475727 ) ) ;
#15492 = DIRECTION ( 'NONE',  ( 0.000000000000000000, 1.000000000000000000, 0.000000000000000000 ) ) ;
#15493 = CARTESIAN_POINT ( 'NONE',  ( -11.70000000000000107, -80.79999999999999716, 0.000000000000000000 ) ) ;
#15494 = VERTEX_POINT ( 'NONE', #19095 ) ;
#15495 = CARTESIAN_POINT ( 'NONE',  ( 6.760013919724077169, -78.37708333333331723, -8.796335266379971429 ) ) ;
#15496 = CARTESIAN_POINT ( 'NONE',  ( 0.000000000000000000, -82.00000000000000000, 0.000000000000000000 ) ) ;
#15497 = CARTESIAN_POINT ( 'NONE',  ( 0.000000000000000000, -81.00000000000000000, 0.000000000000000000 ) ) ;
#15498 = CARTESIAN_POINT ( 'NONE',  ( 1.213359460643753218, -78.36975490881563644, 0.3041480126303982567 ) ) ;
#15499 = CARTESIAN_POINT ( 'NONE',  ( 9.210329749041999747, -79.12592023966598731, -2.015277344078000077 ) ) ;
#15500 = CARTESIAN_POINT ( 'NONE',  ( -12.43645963087999995, -53.88248289507999544, -0.05235777564057000205 ) ) ;
#15501 = CARTESIAN_POINT ( 'NONE',  ( -0.02668022986331678933, -79.47531791158665726, 10.74989935270009589 ) ) ;
#15502 = CARTESIAN_POINT ( 'NONE',  ( -10.42531125074000009, -18.73514854687000053, -7.624341767140999870 ) ) ;
#15503 = ADVANCED_FACE ( 'NONE', ( #10237 ), #38449, .T. ) ;
#15504 = DIRECTION ( 'NONE',  ( 0.000000000000000000, -1.000000000000000000, 0.000000000000000000 ) ) ;
#15505 = CARTESIAN_POINT ( 'NONE',  ( -5.644242139785000667, -77.28891753183799551, 9.380681032049000834 ) ) ;
#15506 = AXIS2_PLACEMENT_3D ( 'NONE', #43993, #44566, #21546 ) ;
#15507 = EDGE_CURVE ( 'NONE', #8180, #36778, #27758, .T. ) ;
#15508 = CARTESIAN_POINT ( 'NONE',  ( 0.5479250432661000314, -82.06079781537400208, -1.507621479251000096 ) ) ;
#15509 = DIRECTION ( 'NONE',  ( 0.000000000000000000, 0.7071067811866525998, -0.7071067811864425456 ) ) ;
#15511 = CARTESIAN_POINT ( 'NONE',  ( 2.598917237794081014, -2.802083333333333037, 1.997276839918480373 ) ) ;
#15510 = CARTESIAN_POINT ( 'NONE',  ( 3.840603960130999806, -83.70479011275499204, 0.9776252842081999406 ) ) ;
#15512 = CARTESIAN_POINT ( 'NONE',  ( 5.684029094576000141, -79.80575194988499277, -7.680196531179999120 ) ) ;
#15513 = CARTESIAN_POINT ( 'NONE',  ( -1.250000000000000000, -83.49999999999998579, 0.000000000000000000 ) ) ;
#15514 = CARTESIAN_POINT ( 'NONE',  ( 7.608898304480751662, -80.28757492195111922, -7.593877026215479553 ) ) ;
#15515 = CARTESIAN_POINT ( 'NONE',  ( -10.75000000000000000, -77.10000000000000853, 0.000000000000000000 ) ) ;
#15516 = CARTESIAN_POINT ( 'NONE',  ( 3.595196526684544924, -79.64062500096297015, -8.672428006415348278 ) ) ;
#15517 = ORIENTED_EDGE ( 'NONE', *, *, #57139, .T. ) ;
#15518 = B_SPLINE_CURVE_WITH_KNOTS ( 'NONE', 3,
 ( #20277, #11143, #37392, #55411, #33832, #24413 ),
 .UNSPECIFIED., .F., .F.,
 ( 4, 1, 1, 4 ),
 ( 0.000000000000000000, 0.3333333333333000081, 0.6666666666667000474, 1.000000000000000000 ),
 .UNSPECIFIED. ) ;
#15519 = CARTESIAN_POINT ( 'NONE',  ( 11.43764105185000091, -79.83449565003729731, 2.691257544168000226 ) ) ;
#15520 = AXIS2_PLACEMENT_3D ( 'NONE', #50019, #24307, #23137 ) ;
#15521 = CARTESIAN_POINT ( 'NONE',  ( -0.1636548025077330659, -78.21466361286708491, -1.249383312717734063 ) ) ;
#15522 = EDGE_CURVE ( 'NONE', #8076, #8174, #33724, .T. ) ;
#15523 = LINE ( 'NONE', #51552, #23729 ) ;
#15524 = EDGE_LOOP ( 'NONE', ( #32273, #53046, #3893, #16187 ) ) ;
#15525 = CARTESIAN_POINT ( 'NONE',  ( 11.76923221829999910, -77.38667338628398795, 1.980068107414000300 ) ) ;
#15526 = ORIENTED_EDGE ( 'NONE', *, *, #6214, .T. ) ;
#15527 = EDGE_LOOP ( 'NONE', ( #53116, #36720, #21076 ) ) ;
#15528 = DIRECTION ( 'NONE',  ( 0.000000000000000000, 1.000000000000000000, 0.000000000000000000 ) ) ;
#15529 = ORIENTED_EDGE ( 'NONE', *, *, #11263, .F. ) ;
#15530 = CARTESIAN_POINT ( 'NONE',  ( -3.481115695920999897, -78.72741664101050674, -0.6826852699798000579 ) ) ;
#15531 = CARTESIAN_POINT ( 'NONE',  ( 1.529360311630938885, -79.26210760543997935, 9.376159717299817231 ) ) ;
#15532 = ORIENTED_EDGE ( 'NONE', *, *, #19037, .F. ) ;
#15533 = CARTESIAN_POINT ( 'NONE',  ( 0.2662832580731058774, -82.74250220263775191, -1.221068703491243079 ) ) ;
#15534 = CARTESIAN_POINT ( 'NONE',  ( -3.360781121377000247, -2.567928536415000185, -0.5239545519189000577 ) ) ;
#15535 = ORIENTED_EDGE ( 'NONE', *, *, #58090, .T. ) ;
#15536 = CARTESIAN_POINT ( 'NONE',  ( -1.342463812738999916E-14, -80.75000000002938805, 0.000000000000000000 ) ) ;
#15537 = CARTESIAN_POINT ( 'NONE',  ( 1.411986188763491912, -77.96846487410871873, -0.5961744733279076280 ) ) ;
#15538 = CARTESIAN_POINT ( 'NONE',  ( -10.44136617523937360, -79.79999999999998295, -5.814006440372521567 ) ) ;
#15539 = CARTESIAN_POINT ( 'NONE',  ( 9.723199427898999048, -54.32306055827000080, -7.958735709912999390 ) ) ;
#15540 = CARTESIAN_POINT ( 'NONE',  ( 5.927986824875999261, -77.92729559796964622, -7.683077610609999830 ) ) ;
#15541 = CARTESIAN_POINT ( 'NONE',  ( -5.279550234765999939, -76.41977030724000031, -9.859017853534000508 ) ) ;
#15542 = CARTESIAN_POINT ( 'NONE',  ( -10.07979664880000037, -76.57175206120300004, 3.736335038366999761 ) ) ;
#15543 = CARTESIAN_POINT ( 'NONE',  ( -1.443009460674115063, -81.32505097460641252, 0.4563349844573089120 ) ) ;
#15544 = VECTOR ( 'NONE', #50857, 1000.000000000000114 ) ;
#15545 = CARTESIAN_POINT ( 'NONE',  ( -1.650172555132999985, -76.77799580226398746, 10.99074904627999949 ) ) ;
#15546 = CARTESIAN_POINT ( 'NONE',  ( -7.233763587253225325, -78.65360029633727379, -5.764933821213369392 ) ) ;
#15547 = CARTESIAN_POINT ( 'NONE',  ( 2.370075440808774747, -76.55841085529293366, 11.50824778498618528 ) ) ;
#15548 = CARTESIAN_POINT ( 'NONE',  ( 4.871830346738000195, -77.67463667140098948, -8.179061320855998574 ) ) ;
#15549 = B_SPLINE_CURVE_WITH_KNOTS ( 'NONE', 3,
 ( #52714, #12265, #9297, #13713 ),
 .UNSPECIFIED., .F., .F.,
 ( 4, 4 ),
 ( 0.000000000000000000, 1.000000000000000000 ),
 .UNSPECIFIED. ) ;
#15550 = CARTESIAN_POINT ( 'NONE',  ( -1.319155384867000125, -80.16637687155399306, 0.1959724986398999891 ) ) ;
#15551 = VECTOR ( 'NONE', #48456, 1000.000000000000000 ) ;
#15552 = CARTESIAN_POINT ( 'NONE',  ( -5.669906390347031255, -80.18205586309346700, -9.426039327529041500 ) ) ;
#15553 = CARTESIAN_POINT ( 'NONE',  ( -2.396502291928098938, -3.041257940394757497, 2.195690585843919074 ) ) ;
#15554 = CARTESIAN_POINT ( 'NONE',  ( -3.062422382194999848, -79.88067549782599031, 1.872246422039999914 ) ) ;
#15556 = EDGE_CURVE ( 'NONE', #1911, #5139, #25252, .T. ) ;
#15555 = CARTESIAN_POINT ( 'NONE',  ( -11.20868100329999884, -79.54611832227699608, 4.514961651145999788 ) ) ;
#15557 = CARTESIAN_POINT ( 'NONE',  ( 11.80338905328919985, -76.21406250001351168, 1.871110305591846101 ) ) ;
#15558 = CARTESIAN_POINT ( 'NONE',  ( -0.4931998282677043655, -83.00735135618793947, 1.148627814754535903 ) ) ;
#15559 = CARTESIAN_POINT ( 'NONE',  ( 7.714303428875997959, -63.10294702886003648, 12.53545825868000385 ) ) ;
#15560 = CARTESIAN_POINT ( 'NONE',  ( -6.558766225408620976, -76.27778056724990563, -9.749046883922389384 ) ) ;
#15561 = CARTESIAN_POINT ( 'NONE',  ( 10.24996238031000040, -20.24828923609000242, 7.705119999441000012 ) ) ;
#15562 = CARTESIAN_POINT ( 'NONE',  ( -10.18948929999999997, -60.01532694310999716, -7.645397820753000673 ) ) ;
#15563 = AXIS2_PLACEMENT_3D ( 'NONE', #20368, #20084, #24211 ) ;
#15564 = CARTESIAN_POINT ( 'NONE',  ( -1.208084210770999922, -81.59953248847399720, 0.5648970606752000689 ) ) ;
#15565 = CARTESIAN_POINT ( 'NONE',  ( -1.310679582531386389, -80.44166666666664867, -0.7554284705563492075 ) ) ;
#15566 = CARTESIAN_POINT ( 'NONE',  ( 10.75000000000000000, -77.25000000000000000, 0.000000000000000000 ) ) ;
#15567 = CARTESIAN_POINT ( 'NONE',  ( 9.332554555131792995, -78.15887491149307209, -5.380831548737815773 ) ) ;
#15568 = CARTESIAN_POINT ( 'NONE',  ( 11.75000000000000000, -78.45000000000000284, 0.000000000000000000 ) ) ;
#15569 = CARTESIAN_POINT ( 'NONE',  ( -6.920341278396000106, -79.42070997529405929, -8.518972542050999408 ) ) ;
#15570 = CARTESIAN_POINT ( 'NONE',  ( 11.92652830712999901, -76.51755275073999485, 1.801729816758000036 ) ) ;
#15571 = ORIENTED_EDGE ( 'NONE', *, *, #44348, .F. ) ;
#15572 = CARTESIAN_POINT ( 'NONE',  ( 2.151480633118999730, -85.51671544543098946, -3.328229532786999734 ) ) ;
#15573 = CARTESIAN_POINT ( 'NONE',  ( -6.997899816120000338, -80.78065832509547306, -8.858414569421000806 ) ) ;
#15574 = EDGE_CURVE ( 'NONE', #21570, #15196, #18805, .T. ) ;
#15575 = CARTESIAN_POINT ( 'NONE',  ( 9.086775583825666303, -78.33514619779819554, -1.734270726548393871 ) ) ;
#15576 = CARTESIAN_POINT ( 'NONE',  ( 9.848035040981065080, -53.97131634258318655, 8.114786739967440710 ) ) ;
#15577 = CARTESIAN_POINT ( 'NONE',  ( 0.5473670387515998659, -77.03056763920500316, -11.20350390113000039 ) ) ;
#15578 = LINE ( 'NONE', #55739, #38949 ) ;
#15579 = CARTESIAN_POINT ( 'NONE',  ( 6.263319273733999992, -78.14860065712299786, 7.458587492396000052 ) ) ;
#15580 = CARTESIAN_POINT ( 'NONE',  ( -1.552248384014999871, -82.85925875911100036, 0.6048007385293000526 ) ) ;
#15581 = DIRECTION ( 'NONE',  ( -0.7071067811865475727, 0.000000000000000000, 0.7071067811865475727 ) ) ;
#15582 = CARTESIAN_POINT ( 'NONE',  ( 1.452792874191000116, -80.27788208903798761, 0.7047031062512999489 ) ) ;
#15583 = EDGE_LOOP ( 'NONE', ( #14812, #7976, #57421, #19673 ) ) ;
#15584 = CARTESIAN_POINT ( 'NONE',  ( -0.5999999999999999778, -5.000000000000000000, -4.000000000000000000 ) ) ;
#15585 = CARTESIAN_POINT ( 'NONE',  ( -3.399999999999706812, -78.71338090247236607, -0.3817310692536478589 ) ) ;
#15586 = EDGE_LOOP ( 'NONE', ( #4172, #41065, #6443, #55208 ) ) ;
#15587 = CARTESIAN_POINT ( 'NONE',  ( 1.166929042523999982, -78.84412371300099664, -0.6456414311070000078 ) ) ;
#15588 = CARTESIAN_POINT ( 'NONE',  ( 6.762881825298999949, -78.98435533332899183, -8.737352176957999816 ) ) ;
#15589 = CIRCLE ( 'NONE', #48589, 0.8000000000000000444 ) ;
#15590 = EDGE_CURVE ( 'NONE', #35380, #1475, #3812, .T. ) ;
#15591 = CARTESIAN_POINT ( 'NONE',  ( 0.02044571250362530943, -80.72695277621694743, -1.249496931604304084 ) ) ;
#15592 = ORIENTED_EDGE ( 'NONE', *, *, #90, .T. ) ;
#15593 = B_SPLINE_CURVE_WITH_KNOTS ( 'NONE', 3,
 ( #43393, #39242, #2387, #15375, #56113, #56688, #33654, #10956, #7377, #16245 ),
 .UNSPECIFIED., .F., .F.,
 ( 4, 1, 1, 1, 1, 1, 1, 4 ),
 ( 0.000000000000000000, 1.019445619974785175E-05, 0.2000061087224714595, 0.4000020229887432111, 0.5999979372550151568, 0.7999938515212868806, 0.9999897657875587154, 1.000000000000000000 ),
 .UNSPECIFIED. ) ;
#15594 = CARTESIAN_POINT ( 'NONE',  ( 10.68616709762000028, -77.53559594867499527, -6.049920594266999352 ) ) ;
#15595 = CARTESIAN_POINT ( 'NONE',  ( -6.211037838955999923, -77.19823840584228947, -9.120711488545000023 ) ) ;
#15596 = AXIS2_PLACEMENT_3D ( 'NONE', #9955, #5804, #19394 ) ;
#15597 = CARTESIAN_POINT ( 'NONE',  ( -11.75000000000000000, -78.70000000000000284, -1.701764645356999850E-14 ) ) ;
#15598 = VERTEX_POINT ( 'NONE', #15828 ) ;
#15599 = ORIENTED_EDGE ( 'NONE', *, *, #10261, .T. ) ;
#15600 = CARTESIAN_POINT ( 'NONE',  ( 0.8777382552776737956, -80.41361731832262194, 0.8895207107364466736 ) ) ;
#15601 = CARTESIAN_POINT ( 'NONE',  ( 10.75000000000000000, -77.85000000000000853, 0.000000000000000000 ) ) ;
#15602 = CARTESIAN_POINT ( 'NONE',  ( 6.728605944993000243, -79.81563540107202925, -7.080011783993000130 ) ) ;
#15603 = ORIENTED_EDGE ( 'NONE', *, *, #51191, .T. ) ;
#15604 = CARTESIAN_POINT ( 'NONE',  ( 12.77651065919999951, -53.49103388577999851, -0.04307580168117999125 ) ) ;
#15605 = CARTESIAN_POINT ( 'NONE',  ( -5.250095168255000111, -79.65848498002199563, -9.571408815458999797 ) ) ;
#15606 = ORIENTED_EDGE ( 'NONE', *, *, #49457, .T. ) ;
#15607 = CARTESIAN_POINT ( 'NONE',  ( -12.59682790092999838, -23.38734115225999943, -1.801645751184999922 ) ) ;
#15608 = CARTESIAN_POINT ( 'NONE',  ( -2.038544480927432900, -78.72609999968184979, -3.380937442862103737 ) ) ;
#15609 = LINE ( 'NONE', #33604, #20462 ) ;
#15610 = FACE_OUTER_BOUND ( 'NONE', #36000, .T. ) ;
#15611 = DIRECTION ( 'NONE',  ( 0.000000000000000000, 0.000000000000000000, -1.000000000000000000 ) ) ;
#15612 = CARTESIAN_POINT ( 'NONE',  ( -12.72924182832285567, -18.22450359994043723, -1.930521792048641716 ) ) ;
#15613 = CARTESIAN_POINT ( 'NONE',  ( -0.2201962894297133100, -78.46348357500299642, -1.520989522816315054 ) ) ;
#15614 = CARTESIAN_POINT ( 'NONE',  ( -8.796335266379978535, -79.65208333333333712, -6.760013919724068288 ) ) ;
#15615 = CARTESIAN_POINT ( 'NONE',  ( -7.986976573804001056, -24.72634345633999686, 10.07613380457000041 ) ) ;
#15616 = CARTESIAN_POINT ( 'NONE',  ( -1.102025757167999886, -80.84283502236499430, 1.180137589876000037 ) ) ;
#15617 = EDGE_CURVE ( 'NONE', #48410, #57766, #33816, .T. ) ;
#15618 = CARTESIAN_POINT ( 'NONE',  ( 8.300970689365454902, -78.10833333333330586, -4.784380313523529438 ) ) ;
#15619 = CARTESIAN_POINT ( 'NONE',  ( 10.01752098898000121, -59.99172009619000079, -7.660412494194000388 ) ) ;
#15620 = CARTESIAN_POINT ( 'NONE',  ( -9.042566447131001439, -79.00702013305000548, -8.284387575507999202 ) ) ;
#15621 = CARTESIAN_POINT ( 'NONE',  ( -11.80208112487999905, -77.08840224925098994, -3.396125071686999952 ) ) ;
#15622 = CARTESIAN_POINT ( 'NONE',  ( 2.486604901413133728, -78.75416666666667709, 9.252740428349007118 ) ) ;
#15623 = ADVANCED_FACE ( 'NONE', ( #6967 ), #7259, .F. ) ;
#15624 = CARTESIAN_POINT ( 'NONE',  ( -9.679134854984988934, -78.10097625800554511, -7.212729867296981290 ) ) ;
#15625 = CARTESIAN_POINT ( 'NONE',  ( -9.805641529082999241, -79.29034910077353970, -5.446788484474000214 ) ) ;
#15626 = VERTEX_POINT ( 'NONE', #25260 ) ;
#15627 = CARTESIAN_POINT ( 'NONE',  ( 0.2545367188273338632, -80.11228258266474711, 1.524467069150255982 ) ) ;
#15628 = CARTESIAN_POINT ( 'NONE',  ( 5.511604622365999795, -77.15613704016388397, 7.990859100417000427 ) ) ;
#15629 = CARTESIAN_POINT ( 'NONE',  ( 0.000000000000000000, -4.000000000000000000, 0.000000000000000000 ) ) ;
#15630 = CARTESIAN_POINT ( 'NONE',  ( 3.113304451009999863, -78.39783470746900207, -10.55022916317000181 ) ) ;
#15631 = CARTESIAN_POINT ( 'NONE',  ( -2.222171105826999504, -3.370715166820999809, -3.169094681224999821 ) ) ;
#15632 = AXIS2_PLACEMENT_3D ( 'NONE', #45706, #32962, #23248 ) ;
#15633 = CARTESIAN_POINT ( 'NONE',  ( -0.8050603620646999969, -78.56086622188500712, -12.13813858862000217 ) ) ;
#15634 = CARTESIAN_POINT ( 'NONE',  ( -9.704555048820999730, -77.77756575905399927, -0.8254132364208000006 ) ) ;
#15636 = CARTESIAN_POINT ( 'NONE',  ( -4.716969252534931378, -77.08541666667790082, 8.182319320987406996 ) ) ;
#15635 = CARTESIAN_POINT ( 'NONE',  ( -11.30495782231091972, -76.17783368164089097, 3.211150208059951883 ) ) ;
#15637 = CARTESIAN_POINT ( 'NONE',  ( 10.63911585229000067, -79.29457588320700268, 2.446340097336999975 ) ) ;
#15638 = CARTESIAN_POINT ( 'NONE',  ( 0.000000000000000000, -74.64999999999999147, 0.000000000000000000 ) ) ;
#15639 = ORIENTED_EDGE ( 'NONE', *, *, #2118, .T. ) ;
#15640 = CARTESIAN_POINT ( 'NONE',  ( 0.000000000000000000, -86.20000000000000284, 0.000000000000000000 ) ) ;
#15641 = CARTESIAN_POINT ( 'NONE',  ( -3.437217408589642531, -78.70000000000000284, -1.942147800595412255 ) ) ;
#15642 = EDGE_CURVE ( 'NONE', #7307, #41589, #51855, .T. ) ;
#15643 = DIRECTION ( 'NONE',  ( 1.000000000000000000, 0.000000000000000000, 0.000000000000000000 ) ) ;
#15644 = CARTESIAN_POINT ( 'NONE',  ( -9.650948395536001811, -61.73402498629999968, 8.252474012569001260 ) ) ;
#15645 = CARTESIAN_POINT ( 'NONE',  ( -10.96988615177242110, -80.09454209194464624, 0.8125309799759529161 ) ) ;
#15646 = CARTESIAN_POINT ( 'NONE',  ( -6.632355475618000540, -79.14317342320499904, -6.884978231758999812 ) ) ;
#15647 = CARTESIAN_POINT ( 'NONE',  ( 0.000000000000000000, 4.040000000000000036, 0.000000000000000000 ) ) ;
#15648 = CARTESIAN_POINT ( 'NONE',  ( -12.70556836319933858, -53.57227722548667970, -0.2598513551041126690 ) ) ;
#15649 = ORIENTED_EDGE ( 'NONE', *, *, #55472, .F. ) ;
#15650 = CARTESIAN_POINT ( 'NONE',  ( -7.438698978239999704, -79.34417565622699442, -8.455750828251000328 ) ) ;
#15651 = DIRECTION ( 'NONE',  ( 0.000000000000000000, -1.000000000000000000, 0.000000000000000000 ) ) ;
#15652 = CARTESIAN_POINT ( 'NONE',  ( -3.301984850800046001, -78.94713398100178381, 11.36385870249712582 ) ) ;
#15653 = CARTESIAN_POINT ( 'NONE',  ( -3.437217181655296105, -78.67390000031815589, 1.942148107221360220 ) ) ;
#15655 = CARTESIAN_POINT ( 'NONE',  ( 0.5173187029184005414, -81.44118298419677160, 1.138630597744533679 ) ) ;
#15654 = CARTESIAN_POINT ( 'NONE',  ( -9.599999999999999645, -92.13603921945998820, 0.000000000000000000 ) ) ;
#15656 = EDGE_CURVE ( 'NONE', #21408, #41593, #25664, .T. ) ;
#15657 = CARTESIAN_POINT ( 'NONE',  ( -0.8704825706172066857, -78.71539928414449605, -0.9315426300253514258 ) ) ;
#15658 = DIRECTION ( 'NONE',  ( 0.000000000000000000, 1.000000000000000000, 0.000000000000000000 ) ) ;
#15659 = CARTESIAN_POINT ( 'NONE',  ( 12.00000000000000000, -76.64999999999999147, 0.000000000000000000 ) ) ;
#15660 = EDGE_CURVE ( 'NONE', #13623, #40049, #49760, .T. ) ;
#15661 = CARTESIAN_POINT ( 'NONE',  ( -12.71658872082999814, -55.48415267986000288, 1.931087888240000217 ) ) ;
#15662 = CARTESIAN_POINT ( 'NONE',  ( 2.787230247158716256, -78.45418832451430546, 10.40622211214603787 ) ) ;
#15663 = CARTESIAN_POINT ( 'NONE',  ( 0.000000000000000000, 4.040000000000000036, 0.000000000000000000 ) ) ;
#15664 = VERTEX_POINT ( 'NONE', #32210 ) ;
#15665 = ORIENTED_EDGE ( 'NONE', *, *, #55298, .F. ) ;
#15666 = CARTESIAN_POINT ( 'NONE',  ( -3.756378708322000382, -77.15821184318100734, 11.89142995536000136 ) ) ;
#15667 = CARTESIAN_POINT ( 'NONE',  ( 4.118279509176275610, -78.75630550986022627, -9.929848109398376366 ) ) ;
#15668 = ORIENTED_EDGE ( 'NONE', *, *, #54272, .T. ) ;
#15669 = CARTESIAN_POINT ( 'NONE',  ( 9.108265402975000313, -17.12189187203999907, 8.478706101062000400 ) ) ;
#15670 = EDGE_CURVE ( 'NONE', #21736, #54376, #9507, .T. ) ;
#15671 = CARTESIAN_POINT ( 'NONE',  ( 1.500000000000000000, -80.15000000000000568, 0.000000000000000000 ) ) ;
#15672 = CONICAL_SURFACE ( 'NONE', #43953, 3.699999993671000187, 0.7853981633972997312 ) ;
#15673 = CARTESIAN_POINT ( 'NONE',  ( -7.544476508856000407, -78.31480665116998807, -9.220210271162999405 ) ) ;
#15674 = AXIS2_PLACEMENT_3D ( 'NONE', #18631, #28043, #23045 ) ;
#15675 = LINE ( 'NONE', #34527, #2372 ) ;
#15676 = CARTESIAN_POINT ( 'NONE',  ( -8.343860018000999190, -59.94999999967000548, -8.343860018000999190 ) ) ;
#15677 = CARTESIAN_POINT ( 'NONE',  ( -1.500000000000000000, -80.00000000000000000, 0.000000000000000000 ) ) ;
#15678 = CARTESIAN_POINT ( 'NONE',  ( -1.639962962630000076, -78.72057076119999408, 11.09633417262999977 ) ) ;
#15679 = TOROIDAL_SURFACE ( 'NONE', #43044, 1.250000000000000000, 0.5000000000000000000 ) ;
#15680 = ORIENTED_EDGE ( 'NONE', *, *, #11465, .F. ) ;
#15681 = FACE_OUTER_BOUND ( 'NONE', #1103, .T. ) ;
#15682 = ORIENTED_EDGE ( 'NONE', *, *, #29021, .F. ) ;
#15683 = CARTESIAN_POINT ( 'NONE',  ( 7.410718339131154409, -77.40115380615291940, 5.535753629427827782 ) ) ;
#15684 = CARTESIAN_POINT ( 'NONE',  ( 10.65102452230999930, -77.76164423048498975, 2.905137941168000282 ) ) ;
#15685 = CARTESIAN_POINT ( 'NONE',  ( -9.998919412391977346, -77.38733819846200390, -5.083622679572695979 ) ) ;
#15687 = EDGE_CURVE ( 'NONE', #2822, #35616, #36231, .T. ) ;
#15686 = CARTESIAN_POINT ( 'NONE',  ( 1.272474653676000100, -78.31634434942250778, -0.6251940786299999830 ) ) ;
#15688 = FACE_OUTER_BOUND ( 'NONE', #13897, .T. ) ;
#15689 = DIRECTION ( 'NONE',  ( 0.000000000000000000, 1.000000000000000000, 0.000000000000000000 ) ) ;
#15690 = CARTESIAN_POINT ( 'NONE',  ( 1.341343219651000229, -79.03170025523999698, -0.9216622887798999741 ) ) ;
#15691 = CARTESIAN_POINT ( 'NONE',  ( -7.655555357433999397, -22.77795407709999864, 10.38646360829000059 ) ) ;
#15692 = EDGE_CURVE ( 'NONE', #20749, #13177, #1034, .T. ) ;
#15693 = CARTESIAN_POINT ( 'NONE',  ( -10.53745838584999994, -79.91191800929898648, 2.317267403318000074 ) ) ;
#15694 = DIRECTION ( 'NONE',  ( 0.000000000000000000, 0.7071067811866525998, -0.7071067811864425456 ) ) ;
#15695 = CARTESIAN_POINT ( 'NONE',  ( 2.377756013412999803, -79.29083355210798345, -11.79209151100000064 ) ) ;
#15696 = CARTESIAN_POINT ( 'NONE',  ( -12.57042253521000141, -62.90094976977999863, 0.000000000000000000 ) ) ;
#15697 = CARTESIAN_POINT ( 'NONE',  ( 1.078481765258000102, -83.66130927919799376, -3.379119232009999418 ) ) ;
#15698 = VERTEX_POINT ( 'NONE', #53699 ) ;
#15699 = LINE ( 'NONE', #37253, #15544 ) ;
#15700 = CARTESIAN_POINT ( 'NONE',  ( -0.9181250412607999678, -79.90971054856998990, -1.434176897702999831 ) ) ;
#15701 = CARTESIAN_POINT ( 'NONE',  ( 2.813892236037239591, -79.24597810272209131, -10.47065658903501451 ) ) ;
#15702 = CARTESIAN_POINT ( 'NONE',  ( -3.545645331619000196, -77.53280483666000578, 11.44309676683000099 ) ) ;
#15703 = CARTESIAN_POINT ( 'NONE',  ( -8.251806177847308632, -53.99944067039370310, 9.431051272634938698 ) ) ;
#15704 = CARTESIAN_POINT ( 'NONE',  ( -5.413816992568016850, -79.01682948708119625, 9.393189368892933544 ) ) ;
#15705 = CARTESIAN_POINT ( 'NONE',  ( -1.543989697593808330, -2.161087190870070618, 3.163786432364460666 ) ) ;
#15706 = CARTESIAN_POINT ( 'NONE',  ( 8.138661153347824140, -80.90697426621636623, 7.022889926100115865 ) ) ;
#15707 = CARTESIAN_POINT ( 'NONE',  ( -8.431119552239000114, -78.10459554355099954, 4.425675013809000191 ) ) ;
#15708 = CARTESIAN_POINT ( 'NONE',  ( 1.798944584246999989, -55.58466771687000119, -12.61116915997000021 ) ) ;
#15709 = CARTESIAN_POINT ( 'NONE',  ( -11.03167625133000129, -77.95931131755500587, -0.06207630174703999970 ) ) ;
#15710 = DIRECTION ( 'NONE',  ( 0.000000000000000000, -1.000000000000000000, 0.000000000000000000 ) ) ;
#15711 = CARTESIAN_POINT ( 'NONE',  ( 10.74691056845999881, -80.79039695949025202, 1.883480763652999990 ) ) ;
#15712 = CARTESIAN_POINT ( 'NONE',  ( 0.8181542670502196524, -80.83029637058210426, -0.9768312912188416020 ) ) ;
#15713 = VERTEX_POINT ( 'NONE', #17092 ) ;
#15714 = CARTESIAN_POINT ( 'NONE',  ( -0.9200108141794000050, -81.83007978797098758, -0.9654823929056000065 ) ) ;
#15715 = CARTESIAN_POINT ( 'NONE',  ( 1.933504092458000034, -60.20406847242999504, -12.70940235709999833 ) ) ;
#15716 = CARTESIAN_POINT ( 'NONE',  ( -14.00000000000000000, -46.09579702914000165, 3.101240652847000040E-11 ) ) ;
#15717 = CARTESIAN_POINT ( 'NONE',  ( -2.185791986076000004, -77.87549888071799842, -11.00183730042999919 ) ) ;
#15718 = CARTESIAN_POINT ( 'NONE',  ( 7.218984044805000444, -79.18772777176498323, 8.267423174273998754 ) ) ;
#15719 = CARTESIAN_POINT ( 'NONE',  ( 10.42531124903999995, -55.53514851492000304, -7.624341765436000173 ) ) ;
#15720 = CARTESIAN_POINT ( 'NONE',  ( 3.514163197055722776, -83.82604166181818073, -2.015118541338928981 ) ) ;
#15721 = CARTESIAN_POINT ( 'NONE',  ( 3.242959734088999735, -77.22308533742300085, -11.71178937074000004 ) ) ;
#15722 = CARTESIAN_POINT ( 'NONE',  ( 5.971486360289516071, -78.53205027161877183, 10.11909832258768382 ) ) ;
#15723 = CARTESIAN_POINT ( 'NONE',  ( 6.000000002940000243, -81.20000000293998710, -1.734976712879000142E-08 ) ) ;
#15724 = EDGE_LOOP ( 'NONE', ( #8458, #52015, #46842, #57916 ) ) ;
#15725 = AXIS2_PLACEMENT_3D ( 'NONE', #12084, #16517, #25363 ) ;
#15726 = DIRECTION ( 'NONE',  ( 0.000000000000000000, 1.000000000000000000, 0.000000000000000000 ) ) ;
#15727 = CARTESIAN_POINT ( 'NONE',  ( -9.250000000000000000, -78.01041666666667140, -1.210822168571064728 ) ) ;
#15728 = AXIS2_PLACEMENT_3D ( 'NONE', #9244, #8355, #40234 ) ;
#15729 = CARTESIAN_POINT ( 'NONE',  ( -0.6687410688010000381, -79.55891271007898524, 11.24641019779000040 ) ) ;
#15730 = DIRECTION ( 'NONE',  ( 0.000000000000000000, 0.000000000000000000, -1.000000000000000000 ) ) ;
#15731 = DIRECTION ( 'NONE',  ( 0.000000000000000000, 0.000000000000000000, -1.000000000000000000 ) ) ;
#15732 = DIRECTION ( 'NONE',  ( 0.000000000000000000, -1.000000000000000000, 0.000000000000000000 ) ) ;
#15733 = CONICAL_SURFACE ( 'NONE', #23274, 5.599999999950999729, 0.2449786631268792425 ) ;
#15734 = CARTESIAN_POINT ( 'NONE',  ( 1.382775425143483394, -83.06597328304708583, -0.6152231662640477161 ) ) ;
#15735 = CARTESIAN_POINT ( 'NONE',  ( -0.5441368889797353336, -79.68939737495202280, -1.127482903650173229 ) ) ;
#15736 = CARTESIAN_POINT ( 'NONE',  ( 1.460959015002474493, -78.12916666666669130, -0.3926218265389176953 ) ) ;
#15737 = VERTEX_POINT ( 'NONE', #53393 ) ;
#15738 = CARTESIAN_POINT ( 'NONE',  ( 1.930989144707000005, -21.75365779208000205, 12.80900240953000058 ) ) ;
#15739 = CARTESIAN_POINT ( 'NONE',  ( -1.980584515756000030, -55.53514849873000259, 12.76303204337999908 ) ) ;
#15740 = EDGE_LOOP ( 'NONE', ( #45454, #4108, #3404, #43780 ) ) ;
#15741 = ORIENTED_EDGE ( 'NONE', *, *, #6928, .F. ) ;
#15742 = CARTESIAN_POINT ( 'NONE',  ( -7.000000000000000000, -81.99999999999998579, 0.000000000000000000 ) ) ;
#15743 = VERTEX_POINT ( 'NONE', #25656 ) ;
#15744 = B_SPLINE_CURVE_WITH_KNOTS ( 'NONE', 3,
 ( #2434, #20721, #38431, #29562, #2725, #38720, #30344, #22377, #53090, #3784, #44820, #17660, #48669, #58396, #31209, #17958, #35647, #53675 ),
 .UNSPECIFIED., .F., .F.,
 ( 4, 2, 2, 2, 2, 2, 2, 2, 4 ),
 ( 0.000000000000000000, 0.1250000000000000000, 0.2499999999999999722, 0.3750000000000000000, 0.5000000000000000000, 0.6250000000000000000, 0.7500000000000000000, 0.8750000000000000000, 1.000000000000000000 ),
 .UNSPECIFIED. ) ;
#15745 = CARTESIAN_POINT ( 'NONE',  ( 4.926127088035904045, -79.91815483164202760, -8.184945656613731302 ) ) ;
#15746 = EDGE_LOOP ( 'NONE', ( #1937, #20307, #4426, #56340 ) ) ;
#15747 = FACE_OUTER_BOUND ( 'NONE', #36153, .T. ) ;
#15748 = FACE_OUTER_BOUND ( 'NONE', #16464, .T. ) ;
#15749 = EDGE_CURVE ( 'NONE', #49656, #34958, #7304, .T. ) ;
#15750 = CARTESIAN_POINT ( 'NONE',  ( -7.958776490640000034, -61.27699850015999772, 9.723157983991999487 ) ) ;
#15751 = CARTESIAN_POINT ( 'NONE',  ( -5.548464554217999556, -78.77021332859899871, -8.076689350464999251 ) ) ;
#15752 = EDGE_CURVE ( 'NONE', #43416, #17252, #34633, .T. ) ;
#15753 = CARTESIAN_POINT ( 'NONE',  ( -1.664588014272184502, -78.21069673449349580, -9.099086625984378784 ) ) ;
#15754 = CARTESIAN_POINT ( 'NONE',  ( 2.407803015296000382, -80.05575617674540467, 10.73324203768999929 ) ) ;
#15755 = EDGE_LOOP ( 'NONE', ( #4850, #2263, #10522, #13916 ) ) ;
#15756 = VERTEX_POINT ( 'NONE', #22396 ) ;
#15757 = CARTESIAN_POINT ( 'NONE',  ( -8.852603344437753208, -77.57660330915794589, 2.682567943804467614 ) ) ;
#15758 = VECTOR ( 'NONE', #49160, 1000.000000000000000 ) ;
#15759 = CARTESIAN_POINT ( 'NONE',  ( -12.72397319118000070, -60.02144180272999563, -1.930910316632999946 ) ) ;
#15760 = CARTESIAN_POINT ( 'NONE',  ( -6.473047519705999342, -78.20295812197798568, 7.229824698717000508 ) ) ;
#15761 = DIRECTION ( 'NONE',  ( 0.000000000000000000, 0.000000000000000000, 1.000000000000000000 ) ) ;
#15762 = CARTESIAN_POINT ( 'NONE',  ( 8.596418555780450887, -76.69791666666668561, -6.606377239730321982 ) ) ;
#15763 = CIRCLE ( 'NONE', #47727, 0.5999999999999999778 ) ;
#15764 = CARTESIAN_POINT ( 'NONE',  ( -7.223234266881707555, -77.37379502737748282, -9.635782272404652460 ) ) ;
#15765 = EDGE_CURVE ( 'NONE', #51480, #14133, #31230, .T. ) ;
#15766 = CARTESIAN_POINT ( 'NONE',  ( 0.3526082373300999939, -79.84950314121999781, -1.545983222067000007 ) ) ;
#15767 = CARTESIAN_POINT ( 'NONE',  ( -0.4779922839590000083, -82.25159812202299747, -1.146319568230000030 ) ) ;
#15768 = CIRCLE ( 'NONE', #42155, 11.19999999999999929 ) ;
#15769 = CARTESIAN_POINT ( 'NONE',  ( 0.6656542303264000315, -82.10069402096399926, -4.119090728389999789 ) ) ;
#15770 = CIRCLE ( 'NONE', #26127, 9.199999999999999289 ) ;
#15771 = CARTESIAN_POINT ( 'NONE',  ( -9.636775127258999873, -54.35967715709000458, 7.948072248856999700 ) ) ;
#15772 = CARTESIAN_POINT ( 'NONE',  ( -3.255457669676000254, -78.10493667140100627, -9.242313942619999168 ) ) ;
#15773 = CARTESIAN_POINT ( 'NONE',  ( 6.606800074109491661, -76.77723522011874024, -8.596815025920347964 ) ) ;
#15774 = CARTESIAN_POINT ( 'NONE',  ( -7.631896578932000352, -18.77877526479000281, -10.36221705164000184 ) ) ;
#15776 = CARTESIAN_POINT ( 'NONE',  ( 2.061613410425999771, -18.79429985524000202, -12.83797036855999885 ) ) ;
#15775 = DIRECTION ( 'NONE',  ( 0.000000000000000000, 1.000000000000000000, 0.000000000000000000 ) ) ;
#15777 = CARTESIAN_POINT ( 'NONE',  ( -9.010394027838918518, -79.57955026341325322, 2.421758550787145303 ) ) ;
#15778 = CARTESIAN_POINT ( 'NONE',  ( -4.999715220074000044, -80.01690199409698323, -9.878567298617999981 ) ) ;
#15779 = CARTESIAN_POINT ( 'NONE',  ( 1.750000000000000000, -18.75000000310999937, 12.50000000000000000 ) ) ;
#15780 = ADVANCED_FACE ( 'NONE', ( #48688 ), #43969, .F. ) ;
#15781 = CARTESIAN_POINT ( 'NONE',  ( -3.268529449828999844, -2.394807261822999855, -1.950076325099000085 ) ) ;
#15782 = CARTESIAN_POINT ( 'NONE',  ( 1.845086187428521374, -0.9188386717781817925, -3.011634086822836398 ) ) ;
#15783 = B_SPLINE_CURVE_WITH_KNOTS ( 'NONE', 3,
 ( #27428, #32143, #45463, #23010, #896, #41021, #54883, #18594, #36584, #14433, #32428, #43066, #24472, #56638, #2902 ),
 .UNSPECIFIED., .F., .F.,
 ( 4, 1, 1, 1, 1, 1, 1, 1, 1, 1, 1, 1, 4 ),
 ( 0.000000000000000000, 0.08333611588665000569, 0.1666676715620999949, 0.2500039875833999781, 0.3333306964953999807, 0.4166666792817999565, 0.4999999999924999994, 0.5833333197091999933, 0.6666692694150000431, 0.7499959719902999922, 0.8333323089881000678, 0.9166638425153998959, 1.000000000000000000 ),
 .UNSPECIFIED. ) ;
#15784 = ORIENTED_EDGE ( 'NONE', *, *, #25263, .T. ) ;
#15785 = CARTESIAN_POINT ( 'NONE',  ( -9.250000000000000000, -78.49999999999998579, 0.000000000000000000 ) ) ;
#15786 = CARTESIAN_POINT ( 'NONE',  ( -12.50000000000000000, -65.72928575305999743, 0.000000000000000000 ) ) ;
#15787 = EDGE_CURVE ( 'NONE', #4635, #22997, #30576, .T. ) ;
#15788 = CARTESIAN_POINT ( 'NONE',  ( -1.333333333333333259, -77.60000000000000853, 0.000000000000000000 ) ) ;
#15789 = CARTESIAN_POINT ( 'NONE',  ( -0.0009180708875000889333, -78.47527983758934056, 1.249867243019089358 ) ) ;
#15790 = CARTESIAN_POINT ( 'NONE',  ( 9.563799579366000003, -79.07178538496899023, -0.8978884989661999327 ) ) ;
#15791 = CARTESIAN_POINT ( 'NONE',  ( -12.66008925480999814, -54.17289997881999852, 1.387046028394999908 ) ) ;
#15792 = CARTESIAN_POINT ( 'NONE',  ( 9.494736565810956819, -79.10440807414381936, 0.5477041750795209607 ) ) ;
#15793 = CARTESIAN_POINT ( 'NONE',  ( 1.477284502223000118, -61.52631500263999698, 12.77254812472999923 ) ) ;
#15794 = CARTESIAN_POINT ( 'NONE',  ( -0.003822974957334815405, -79.47514570661689959, 10.74992904790657455 ) ) ;
#15795 = CARTESIAN_POINT ( 'NONE',  ( -2.600000000000000089, -78.49999999999998579, 0.000000000000000000 ) ) ;
#15796 = CARTESIAN_POINT ( 'NONE',  ( -3.000000000000000000, -86.20000000000000284, 0.000000000000000000 ) ) ;
#15797 = CARTESIAN_POINT ( 'NONE',  ( 3.837643902511000071, -77.71731316181897853, 10.25315621143999856 ) ) ;
#15798 = CARTESIAN_POINT ( 'NONE',  ( 9.014444551600488964, -76.39432718886233431, -7.542217132489586362 ) ) ;
#15799 = CARTESIAN_POINT ( 'NONE',  ( 8.993546968190999635, -77.34198448012199378, -6.388884668894999841 ) ) ;
#15800 = CARTESIAN_POINT ( 'NONE',  ( -1.218115782252727985, -82.07993943974406648, 0.3280300537313449727 ) ) ;
#15801 = CARTESIAN_POINT ( 'NONE',  ( 1.750000000000000000, -58.55064714144999982, -12.65372179280999987 ) ) ;
#15802 = CARTESIAN_POINT ( 'NONE',  ( -3.250000000000000000, -3.000000000000000000, 0.000000000000000000 ) ) ;
#15803 = CARTESIAN_POINT ( 'NONE',  ( 8.395992668097999712, -79.41965194988499377, 4.560928606276999808 ) ) ;
#15804 = CARTESIAN_POINT ( 'NONE',  ( 6.760013919724039866, -77.42291666666667993, 8.796335266379998075 ) ) ;
#15805 = CARTESIAN_POINT ( 'NONE',  ( 7.807646140253542200, -80.28969248854734531, -7.390132470684190658 ) ) ;
#15806 = CIRCLE ( 'NONE', #42190, 1.750000000000001332 ) ;
#15807 = CARTESIAN_POINT ( 'NONE',  ( 7.919595949288999570, -55.64999999965999677, -8.768124086712999699 ) ) ;
#15808 = CARTESIAN_POINT ( 'NONE',  ( 9.500000000000000000, -77.14999999999999147, 0.000000000000000000 ) ) ;
#15809 = CARTESIAN_POINT ( 'NONE',  ( -7.858171174022000827, -79.06554253958299228, 9.108036400545000077 ) ) ;
#15810 = CARTESIAN_POINT ( 'NONE',  ( 0.000000000000000000, -18.84999999999999787, -11.89999999977000122 ) ) ;
#15811 = CARTESIAN_POINT ( 'NONE',  ( 0.000000000000000000, -9.295797029142999435, 0.000000000000000000 ) ) ;
#15812 = AXIS2_PLACEMENT_3D ( 'NONE', #16614, #7173, #3324 ) ;
#15813 = ORIENTED_EDGE ( 'NONE', *, *, #24591, .T. ) ;
#15814 = CARTESIAN_POINT ( 'NONE',  ( -11.44451898095999987, -78.14629421814900923, -3.385038809382000302 ) ) ;
#15815 = AXIS2_PLACEMENT_3D ( 'NONE', #14022, #13138, #32020 ) ;
#15816 = EDGE_LOOP ( 'NONE', ( #5289, #52840, #20599, #33518 ) ) ;
#15817 = VERTEX_POINT ( 'NONE', #35971 ) ;
#15818 = VECTOR ( 'NONE', #17680, 1000.000000000000000 ) ;
#15819 =( BOUNDED_SURFACE ( )  B_SPLINE_SURFACE ( 3, 3, ( 
 ( #33311, #19752, #37748, #10904, #46927, #6454, #24469 ),
 ( #56062, #42482, #15608, #48645, #35619, #39186, #16479 ),
 ( #8189, #22046, #17331, #43632, #30028, #4042, #40053 ),
 ( #26468, #47791, #44491, #35320, #30896, #3195, #53062 ),
 ( #30317, #58070, #8471, #7322, #26190, #21185, #56921 ),
 ( #53646, #48358, #25611, #7898, #17630, #13186, #48929 ),
 ( #39763, #25324, #52777, #7611, #53349, #12895, #57201 ),
 ( #43341, #25900, #2898, #21477, #20898, #38901, #34459 ),
 ( #16769, #21758, #52490, #12047, #12614, #48081, #34748 ),
 ( #12331, #43924, #44208, #3471, #17050, #39484, #57486 ),
 ( #35030, #30611, #3758, #57776, #9656, #45981, #45685 ),
 ( #58367, #9365, #19097, #32070, #41527, #36510, #40657 ),
 ( #22344, #50111, #35919, #27931, #1112, #247, #23517 ),
 ( #18231, #53950, #27355, #5225, #40359, #36220, #22647 ),
 ( #13486, #37087, #55105, #22937, #54534, #40949, #540 ) ),
 .UNSPECIFIED., .F., .F., .T. ) 
 B_SPLINE_SURFACE_WITH_KNOTS ( ( 4, 1, 1, 1, 1, 1, 1, 1, 1, 1, 1, 1, 4 ),
 ( 4, 3, 4 ),
 ( 0.009836338020448129327, 0.09153385889397000486, 0.1732268882812000033, 0.2549245844128000260, 0.3366128623372000028, 0.4183102317861999708, 0.5000049915032999115, 0.5816997502458999270, 0.6633970872647999562, 0.7450853589770999319, 0.8267830756728000718, 0.9084760833474000430, 0.9901736249421290159 ),
 ( 0.000000000000000000, 0.5000000000000000000, 1.000000000000000000 ),
 .UNSPECIFIED. ) 
 GEOMETRIC_REPRESENTATION_ITEM ( )  RATIONAL_B_SPLINE_SURFACE ( (
 ( 1.000000000000000000, 0.8025111667134329219, 0.8025111667134329219, 1.000000000000000000, 0.8025111667134329219, 0.8025111667134329219, 1.000000000000000000),
 ( 1.000000000000000000, 0.8025111667134329219, 0.8025111667134329219, 1.000000000000000000, 0.8025111667134329219, 0.8025111667134329219, 1.000000000000000000),
 ( 1.000000000000000000, 0.8025111667134329219, 0.8025111667134329219, 1.000000000000000000, 0.8025111667134329219, 0.8025111667134329219, 1.000000000000000000),
 ( 1.000000000000000000, 0.8025111667134329219, 0.8025111667134329219, 1.000000000000000000, 0.8025111667134329219, 0.8025111667134329219, 1.000000000000000000),
 ( 1.000000000000000000, 0.8025111667134329219, 0.8025111667134329219, 1.000000000000000000, 0.8025111667134329219, 0.8025111667134329219, 1.000000000000000000),
 ( 1.000000000000000000, 0.8025111667134329219, 0.8025111667134329219, 1.000000000000000000, 0.8025111667134329219, 0.8025111667134329219, 1.000000000000000000),
 ( 1.000000000000000000, 0.8025111667134329219, 0.8025111667134329219, 1.000000000000000000, 0.8025111667134329219, 0.8025111667134329219, 1.000000000000000000),
 ( 1.000000000000000000, 0.8025111667134329219, 0.8025111667134329219, 1.000000000000000000, 0.8025111667134329219, 0.8025111667134329219, 1.000000000000000000),
 ( 1.000000000000000000, 0.8025111667134329219, 0.8025111667134329219, 1.000000000000000000, 0.8025111667134329219, 0.8025111667134329219, 1.000000000000000000),
 ( 1.000000000000000000, 0.8025111667134329219, 0.8025111667134329219, 1.000000000000000000, 0.8025111667134329219, 0.8025111667134329219, 1.000000000000000000),
 ( 1.000000000000000000, 0.8025111667134329219, 0.8025111667134329219, 1.000000000000000000, 0.8025111667134329219, 0.8025111667134329219, 1.000000000000000000),
 ( 1.000000000000000000, 0.8025111667134329219, 0.8025111667134329219, 1.000000000000000000, 0.8025111667134329219, 0.8025111667134329219, 1.000000000000000000),
 ( 1.000000000000000000, 0.8025111667134329219, 0.8025111667134329219, 1.000000000000000000, 0.8025111667134329219, 0.8025111667134329219, 1.000000000000000000),
 ( 1.000000000000000000, 0.8025111667134329219, 0.8025111667134329219, 1.000000000000000000, 0.8025111667134329219, 0.8025111667134329219, 1.000000000000000000),
 ( 1.000000000000000000, 0.8025111667134329219, 0.8025111667134329219, 1.000000000000000000, 0.8025111667134329219, 0.8025111667134329219, 1.000000000000000000) ) ) 
 REPRESENTATION_ITEM ( '' )  SURFACE ( )  );
#15820 = CARTESIAN_POINT ( 'NONE',  ( -9.396085398178614767, -77.35208333333333997, -7.220923959705254802 ) ) ;
#15821 = CARTESIAN_POINT ( 'NONE',  ( -3.218446570455000266, -80.49781712273099288, -1.589134001521000039 ) ) ;
#15822 = CARTESIAN_POINT ( 'NONE',  ( 8.491818810844479870, -79.18689644516919657, 4.277273810732789450 ) ) ;
#15823 = ORIENTED_EDGE ( 'NONE', *, *, #33081, .F. ) ;
#15824 = CARTESIAN_POINT ( 'NONE',  ( -1.093100964505588690, -82.64204610221628400, -0.6296463513202182893 ) ) ;
#15825 = ORIENTED_EDGE ( 'NONE', *, *, #19782, .F. ) ;
#15826 = CARTESIAN_POINT ( 'NONE',  ( 2.764245102654999897, -2.355122700497000121, 1.982000095699999909 ) ) ;
#15827 = EDGE_LOOP ( 'NONE', ( #51197, #1680 ) ) ;
#15828 = CARTESIAN_POINT ( 'NONE',  ( -1.250000000000000000, -80.00000000000000000, 0.000000000000000000 ) ) ;
#15829 = CARTESIAN_POINT ( 'NONE',  ( -0.3042520966058857579, -78.64066448665755615, 1.500984266365883446 ) ) ;
#15830 = CARTESIAN_POINT ( 'NONE',  ( -2.414913865112868763, -79.79999999999999716, -11.57229497112463612 ) ) ;
#15831 = B_SPLINE_SURFACE_WITH_KNOTS ( 'NONE', 3, 3, ( 
 ( #20237, #33790, #24945, #56251, #42965, #38522, #56537, #52684, #30230, #34368, #52114, #57401, #16098, #7230, #25234, #16959, #12239, #43254, #2810, #20804, #38811, #31384, #49124, #31678, #35224, #8378, #39673, #40259, #49425, #22248, #40851, #44991, #27252, #53551, #31971 ),
 ( #36412, #53254, #57975, #44395, #18421, #54440, #21950, #443, #3667, #13976, #49724, #45292, #17531, #8975, #57679, #44696, #50014, #22838, #21667, #40560, #35522, #12804, #13090, #9560, #4251, #39962, #58272, #27544, #17237, #4842, #30803, #54140, #48836, #8674, #31087 ),
 ( #26663, #3947, #26376, #17835, #9267, #35823, #53852, #13384, #26961, #4547, #22549, #36124, #153, #18129, #13680, #28713, #45881, #33137, #24302, #50598, #46465, #46765, #14846, #32549, #33437, #5993, #51473, #42316, #55891, #23999, #42017, #1884, #1587, #41433, #19577 ),
 ( #15142, #1019, #41139, #19878, #32258, #37871, #15443, #10737, #23711, #18710, #10147, #54719, #11030, #5133, #6287, #19000, #50887, #730, #28124, #45588, #23130, #36704, #37576, #36992, #14262, #55008, #50304, #46174, #23421, #5700, #9854, #27835, #5413, #14556, #55593 ) ),
 .UNSPECIFIED., .F., .F., .F.,
 ( 4, 4 ),
 ( 4, 1, 1, 1, 1, 1, 1, 1, 1, 1, 1, 1, 1, 1, 1, 1, 1, 1, 1, 1, 1, 1, 1, 1, 1, 1, 1, 1, 1, 1, 1, 1, 4 ),
 ( -0.1331668876848000060, 1.133166887685000068 ),
 ( -0.01763212848115999765, 0.01102008030072000079, 0.03967228908261000164, 0.06832449786448999141, 0.09697670664638000093, 0.1256289154283000142, 0.1542811242101000124, 0.1829333329919999862, 0.2115855417738999877, 0.2402377505557999893, 0.2688899593376999908, 0.2975421681195999923, 0.3261943769014999939, 0.3548465856833000198, 0.3834987944651999658, 0.4121510032471000229, 0.4408032120290000244, 0.4694554208109000260, 0.4981076295927999720, 0.5267598383746000534, 0.5554120471565000550, 0.5840642559384000565, 0.6127164647203000580, 0.6413686735021999485, 0.6700208822840999501, 0.6986730910659999516, 0.7273252998478000331, 0.7559775086296999236, 0.7846297174115999251, 0.8132819261935000377, 0.8419341349753999282, 0.8705863437573000407, 0.8992385525391000112 ),
 .UNSPECIFIED. ) ;
#15832 = CARTESIAN_POINT ( 'NONE',  ( -10.58481073984209786, -80.08630942833664790, 1.876888235204818622 ) ) ;
#15833 = CARTESIAN_POINT ( 'NONE',  ( -11.55452283565012728, -78.92300996100392751, 4.111075736105198608 ) ) ;
#15834 = CARTESIAN_POINT ( 'NONE',  ( -3.237453996416787216, -86.09999999999998010, -2.259489515356280620 ) ) ;
#15835 = CARTESIAN_POINT ( 'NONE',  ( -7.695020077040999773, -76.33706720858099004, 8.115451295621999961 ) ) ;
#15836 = DIRECTION ( 'NONE',  ( 0.000000000000000000, -1.000000000000000000, 0.000000000000000000 ) ) ;
#15837 = ADVANCED_FACE ( 'NONE', ( #39528 ), #58246, .F. ) ;
#15838 = CARTESIAN_POINT ( 'NONE',  ( 10.71369944335147117, -78.47083333333331723, 2.879226727952105769 ) ) ;
#15839 = CARTESIAN_POINT ( 'NONE',  ( -9.770426151684000970, -76.35160278844999482, 5.297017541237999616 ) ) ;
#15840 = CARTESIAN_POINT ( 'NONE',  ( -6.523492958078782600, -78.66275140589766579, -6.557889900168049735 ) ) ;
#15841 = CARTESIAN_POINT ( 'NONE',  ( -9.517358746150001991, -77.50498667140099940, 0.2272806389514000214 ) ) ;
#15842 = CARTESIAN_POINT ( 'NONE',  ( -1.248430190247999949, -79.17412440393199802, 0.06262635289305999720 ) ) ;
#15843 = CYLINDRICAL_SURFACE ( 'NONE', #50673, 9.500000000000000000 ) ;
#15844 = CARTESIAN_POINT ( 'NONE',  ( -3.210881389860447577, -3.087896390847898243, 0.5389748725432149667 ) ) ;
#15845 = CARTESIAN_POINT ( 'NONE',  ( -1.265066673746999770, -81.68828455456798565, -3.537086639947999878 ) ) ;
#15846 = CARTESIAN_POINT ( 'NONE',  ( -5.021054719342000539, -79.98639431301229763, 10.71058697011000049 ) ) ;
#15847 = DIRECTION ( 'NONE',  ( 1.000000000000000000, 0.000000000000000000, 0.000000000000000000 ) ) ;
#15848 = CARTESIAN_POINT ( 'NONE',  ( -0.4784572937601109799, -83.00632309593854075, 1.154759755059053150 ) ) ;
#15849 = PRESENTATION_STYLE_ASSIGNMENT (( #46585 ) ) ;
#15850 = CARTESIAN_POINT ( 'NONE',  ( -3.302049379960999786, -84.59819503318799150, 1.295388840129999997 ) ) ;
#15851 = CARTESIAN_POINT ( 'NONE',  ( -8.308486710064240555, -76.26191577339538696, -8.308010501594221608 ) ) ;
#15852 = CARTESIAN_POINT ( 'NONE',  ( 10.59548767699999949, -20.24263462181000151, 7.678667886068000215 ) ) ;
#15853 = B_SPLINE_SURFACE_WITH_KNOTS ( 'NONE', 3, 3, ( 
 ( #7012, #2026, #20024, #38878, #21161, #29718, #29147, #25014, #56898, #39167, #33282, #3171, #56607, #25303, #51323, #46903, #11172, #16455, #2597, #7301, #6429, #16167, #34437, #12025, #34145, #52185, #38008, #15582, #30005, #24733, #33577, #51616, #48059, #7590, #25589 ),
 ( #43611, #47766, #47193, #6725, #42747, #20306, #38301, #12590, #12870, #4319, #22622, #40633, #45070, #22023, #8747, #4622, #16743, #53043, #27033, #26738, #53928, #21735, #35010, #44769, #22318, #26169, #17309, #30297, #34723, #48336, #21454, #35295, #17605, #12307, #40335 ),
 ( #4017, #52753, #39742, #44466, #30589, #7875, #35594, #13460, #53622, #53325, #44188, #58344, #48620, #58045, #30873, #48908, #8167, #17907, #35896, #25877, #3734, #57752, #43904, #13160, #8449, #49498, #26444, #3448, #9047, #39461, #40031, #57465, #31157, #49195, #17026 ),
 ( #27331, #9342, #14334, #514, #1368, #55081, #14918, #54216, #49796, #50378, #228, #23490, #32913, #19364, #36198, #32620, #36483, #23204, #23781, #37063, #41796, #40927, #10214, #28193, #45953, #9925, #41503, #54791, #45365, #46246, #37357, #4914, #41209, #14049, #5774 ) ),
 .UNSPECIFIED., .F., .F., .F.,
 ( 4, 4 ),
 ( 4, 1, 1, 1, 1, 1, 1, 1, 1, 1, 1, 1, 1, 1, 1, 1, 1, 1, 1, 1, 1, 1, 1, 1, 1, 1, 1, 1, 1, 1, 1, 1, 4 ),
 ( -0.05371687727927999811, 1.053716877278999986 ),
 ( -0.02000000000000000042, 0.01250000000000000069, 0.04499999999999999833, 0.07749999999999999944, 0.1100000000000000006, 0.1424999999999999878, 0.1749999999999999889, 0.2074999999999999900, 0.2399999999999999911, 0.2725000000000000200, 0.3049999999999999933, 0.3375000000000000222, 0.3699999999999999956, 0.4025000000000000244, 0.4349999999999999978, 0.4675000000000000266, 0.5000000000000000000, 0.5324999999999999734, 0.5649999999999999467, 0.5975000000000000311, 0.6300000000000000044, 0.6624999999999999778, 0.6949999999999999512, 0.7275000000000000355, 0.7600000000000000089, 0.7924999999999999822, 0.8249999999999999556, 0.8575000000000000400, 0.8900000000000000133, 0.9224999999999999867, 0.9549999999999999600, 0.9875000000000000444, 1.020000000000000018 ),
 .UNSPECIFIED. ) ;
#15854 = CARTESIAN_POINT ( 'NONE',  ( 1.103931348482591668, -24.62083748120022264, 12.50298439259066363 ) ) ;
#15855 = EDGE_CURVE ( 'NONE', #313, #26598, #20542, .T. ) ;
#15856 = CARTESIAN_POINT ( 'NONE',  ( 8.300970689365442468, -78.19166666666667709, 4.784380313523563188 ) ) ;
#15857 = CARTESIAN_POINT ( 'NONE',  ( 1.316231252753000014, -81.89720822875999318, 0.2147359707272000207 ) ) ;
#15858 = CARTESIAN_POINT ( 'NONE',  ( -12.83836748062999966, -18.79372227161000097, -2.062147040910000229 ) ) ;
#15859 = CARTESIAN_POINT ( 'NONE',  ( 12.65987830573000039, -24.93692962305999927, 0.9847759095506000149 ) ) ;
#15860 = CARTESIAN_POINT ( 'NONE',  ( 9.469096744587201187, -77.74081920503226684, 5.269811678343041095 ) ) ;
#15861 = CARTESIAN_POINT ( 'NONE',  ( -3.044763360077934689, -78.30249503962149049, -11.37362071366816352 ) ) ;
#15862 = AXIS2_PLACEMENT_3D ( 'NONE', #22989, #592, #14124 ) ;
#15863 = CARTESIAN_POINT ( 'NONE',  ( 10.74341457190999982, -79.08360172330206694, -2.245675826504000216 ) ) ;
#15864 = CARTESIAN_POINT ( 'NONE',  ( 3.844527461940999480, -75.64423130519999461, -11.90714177081000003 ) ) ;
#15865 = EDGE_LOOP ( 'NONE', ( #48780, #46911, #12828 ) ) ;
#15866 = FACE_OUTER_BOUND ( 'NONE', #24453, .T. ) ;
#15867 = CARTESIAN_POINT ( 'NONE',  ( 10.36746145409304987, -55.03400544981041520, 7.635225828740804133 ) ) ;
#15868 = DIRECTION ( 'NONE',  ( 0.7071067811814920612, -1.249159359038985910E-07, -0.7071067811915919821 ) ) ;
#15869 = CARTESIAN_POINT ( 'NONE',  ( -1.799501877793999949, -18.71082276572999703, -12.60552511010000032 ) ) ;
#15870 = CARTESIAN_POINT ( 'NONE',  ( 1.265244864176999995, -77.69381939105899448, 9.657062241701000360 ) ) ;
#15871 = CARTESIAN_POINT ( 'NONE',  ( -1.324613189995999862, -83.42769169510199845, -0.7038465009425000085 ) ) ;
#15872 = LINE ( 'NONE', #55742, #2950 ) ;
#15873 = CARTESIAN_POINT ( 'NONE',  ( 8.343860018000999190, -59.94999999967000548, 8.343860018000999190 ) ) ;
#15874 = EDGE_CURVE ( 'NONE', #37266, #26517, #46012, .T. ) ;
#15875 = VERTEX_POINT ( 'NONE', #57532 ) ;
#15876 = CARTESIAN_POINT ( 'NONE',  ( -3.250000000000000000, -3.000000000000000000, 0.000000000000000000 ) ) ;
#15877 = DIRECTION ( 'NONE',  ( 1.000000000000000000, 0.000000000000000000, 0.000000000000000000 ) ) ;
#15878 = CARTESIAN_POINT ( 'NONE',  ( 0.05072268191597268522, -78.88976567714485100, -3.472900191114431490 ) ) ;
#15879 = ORIENTED_EDGE ( 'NONE', *, *, #41105, .F. ) ;
#15880 = CARTESIAN_POINT ( 'NONE',  ( 1.315129997485000146, -78.44138412015038853, 0.2213803045116000123 ) ) ;
#15881 = CARTESIAN_POINT ( 'NONE',  ( 0.9151062594318000176, -78.67533943566898813, 11.01092521911999889 ) ) ;
#15882 = DIRECTION ( 'NONE',  ( -1.000000000000000000, 0.000000000000000000, 0.000000000000000000 ) ) ;
#15883 = B_SPLINE_CURVE_WITH_KNOTS ( 'NONE', 3,
 ( #24548, #37829, #18673, #55548, #32507, #28084, #41681, #36662, #19248, #37243 ),
 .UNSPECIFIED., .F., .F.,
 ( 4, 2, 2, 2, 4 ),
 ( 0.000000000000000000, 0.2500000000000000000, 0.5000000000000000000, 0.7500000000000000000, 1.000000000000000000 ),
 .UNSPECIFIED. ) ;
#15884 = FACE_OUTER_BOUND ( 'NONE', #3916, .T. ) ;
#15885 = EDGE_LOOP ( 'NONE', ( #55678, #42696, #2366, #17588 ) ) ;
#15886 = CARTESIAN_POINT ( 'NONE',  ( 12.09396573961999799, -77.56272526409898660, -2.128801122353999986 ) ) ;
#15887 = CARTESIAN_POINT ( 'NONE',  ( 11.29729853867000067, -77.85856316181899217, -1.753017772781999772 ) ) ;
#15888 = VERTEX_POINT ( 'NONE', #7657 ) ;
#15889 = EDGE_LOOP ( 'NONE', ( #55967, #1211, #44309, #32344, #9425, #24086, #18581 ) ) ;
#15890 = CARTESIAN_POINT ( 'NONE',  ( 1.021667840366504487, -80.39937480585440710, 0.7203988087165839049 ) ) ;
#15891 = CARTESIAN_POINT ( 'NONE',  ( -8.485281374238999419, -18.75000000000000000, 8.485281374238999419 ) ) ;
#15892 = CARTESIAN_POINT ( 'NONE',  ( -2.116314338179000387, -80.23777995843001065, -9.535298106756000536 ) ) ;
#15893 = ORIENTED_EDGE ( 'NONE', *, *, #57030, .T. ) ;
#15894 = CARTESIAN_POINT ( 'NONE',  ( -12.70259419118153410, -24.73882758528178982, -1.314635108445226797 ) ) ;
#15895 = CARTESIAN_POINT ( 'NONE',  ( 10.85828250482999913, -79.33164886400000171, 1.128302723381999995 ) ) ;
#15896 = VERTEX_POINT ( 'NONE', #43685 ) ;
#15897 = CARTESIAN_POINT ( 'NONE',  ( 9.889431646000000242, -78.85035427783628847, 7.252463523969000292 ) ) ;
#15898 = CARTESIAN_POINT ( 'NONE',  ( 9.243123479240180629, -24.91653773629412427, 8.441201027670452106 ) ) ;
#15899 = AXIS2_PLACEMENT_3D ( 'NONE', #46420, #5372, #41678 ) ;
#15900 = LINE ( 'NONE', #56064, #45923 ) ;
#15901 = DIRECTION ( 'NONE',  ( 0.000000000000000000, 0.7071067811866525998, -0.7071067811864425456 ) ) ;
#15902 = CARTESIAN_POINT ( 'NONE',  ( 9.347227379752075294, -78.32137913613844660, 2.683805748252192203 ) ) ;
#15903 = EDGE_CURVE ( 'NONE', #13012, #15167, #21232, .T. ) ;
#15904 = CARTESIAN_POINT ( 'NONE',  ( -6.146221368751000114, -77.09692023966638885, 7.568187592052000312 ) ) ;
#15905 = CARTESIAN_POINT ( 'NONE',  ( 10.18066396183999878, -78.44417834570113257, 6.314281093748000728 ) ) ;
#15906 = CYLINDRICAL_SURFACE ( 'NONE', #39727, 10.75000000000000000 ) ;
#15907 = EDGE_CURVE ( 'NONE', #42991, #7477, #44251, .T. ) ;
#15908 = CARTESIAN_POINT ( 'NONE',  ( -8.292771711448001071, -25.05529938523999789, 9.770424367364000773 ) ) ;
#15909 = CARTESIAN_POINT ( 'NONE',  ( -9.499653450934914645, -79.30027302004205580, 1.387647615217423080E-06 ) ) ;
#15910 = CARTESIAN_POINT ( 'NONE',  ( -8.300970689365447797, -77.94166666666667709, -4.784380313523547201 ) ) ;
#15911 = CARTESIAN_POINT ( 'NONE',  ( 10.53495260694000102, -60.02711197453000125, -7.618387230260000642 ) ) ;
#15912 = CARTESIAN_POINT ( 'NONE',  ( -11.55418265775999842, -78.95546464548999666, 4.110954701505000308 ) ) ;
#15913 = CARTESIAN_POINT ( 'NONE',  ( -7.650089724727000551, -76.63759212789700825, -9.607224057717001386 ) ) ;
#15914 = DIRECTION ( 'NONE',  ( 0.000000000000000000, 0.000000000000000000, -1.000000000000000000 ) ) ;
#15915 = CARTESIAN_POINT ( 'NONE',  ( -3.678946202636633522, -77.94976169127751575, 11.44154515669267980 ) ) ;
#15916 = DIRECTION ( 'NONE',  ( 0.000000000000000000, 1.000000000000000000, 0.000000000000000000 ) ) ;
#15917 = ADVANCED_FACE ( 'NONE', ( #34798 ), #30364, .F. ) ;
#15918 = ORIENTED_EDGE ( 'NONE', *, *, #57095, .T. ) ;
#15919 = CARTESIAN_POINT ( 'NONE',  ( 1.490312334586760157, -81.01311113150978827, 0.2476722647248059406 ) ) ;
#15920 = CARTESIAN_POINT ( 'NONE',  ( -3.716474266315000108, -77.11277995979999389, -8.432660871143999870 ) ) ;
#15921 = DIRECTION ( 'NONE',  ( 0.000000000000000000, -1.000000000000000000, 0.000000000000000000 ) ) ;
#15922 = LINE ( 'NONE', #21205, #42680 ) ;
#15923 = CARTESIAN_POINT ( 'NONE',  ( 1.027101072325000031, -2.234162460019999852, 3.569245810093000237 ) ) ;
#15924 = CARTESIAN_POINT ( 'NONE',  ( -7.733454931756999606, -78.37096101391799152, 9.390218602554998739 ) ) ;
#15925 = CARTESIAN_POINT ( 'NONE',  ( -8.711966356949998769, -77.23751300560297750, 3.874524904258000557 ) ) ;
#15926 = VECTOR ( 'NONE', #29752, 999.9999999999998863 ) ;
#15928 = CARTESIAN_POINT ( 'NONE',  ( -9.319010416924347950, -77.13098958334455801, 1.219003397386794862 ) ) ;
#15927 = CARTESIAN_POINT ( 'NONE',  ( -9.062526876912226470, -76.14485825892174375, 7.478624034300348278 ) ) ;
#15929 = CARTESIAN_POINT ( 'NONE',  ( 10.30613478042999986, -78.74984902316998614, -3.599856929194000354 ) ) ;
#15930 = CARTESIAN_POINT ( 'NONE',  ( -10.55305693674421619, -79.58487289164341405, 2.047928793955265281 ) ) ;
#15931 = ORIENTED_EDGE ( 'NONE', *, *, #10109, .F. ) ;
#15932 = CARTESIAN_POINT ( 'NONE',  ( -10.77133038181999503, -76.59021486849412952, -5.959359258312999508 ) ) ;
#15933 = CARTESIAN_POINT ( 'NONE',  ( -9.488660192930483461, -79.25397600642003226, -0.4744913388225507900 ) ) ;
#15934 = CARTESIAN_POINT ( 'NONE',  ( 10.74999999999999645, -77.26041666666667140, 1.407171709420451666 ) ) ;
#15935 = CARTESIAN_POINT ( 'NONE',  ( -7.601397897754999633, -18.75000000000000000, -9.369164850722000892 ) ) ;
#15936 = CARTESIAN_POINT ( 'NONE',  ( -10.30068234846894626, -80.07172511735936382, 3.869806167791196572 ) ) ;
#15937 = CARTESIAN_POINT ( 'NONE',  ( -3.001687856302999613, -79.54317808830998615, 9.192644655792999941 ) ) ;
#15938 = CARTESIAN_POINT ( 'NONE',  ( -12.00000000000000000, -77.89999999999999147, -2.795183092923000262E-14 ) ) ;
#15939 = CARTESIAN_POINT ( 'NONE',  ( -6.760013919724058518, -78.67291666666667993, -8.796335266379987416 ) ) ;
#15940 = ORIENTED_EDGE ( 'NONE', *, *, #51363, .F. ) ;
#15941 = CARTESIAN_POINT ( 'NONE',  ( 2.188076007269000200, -78.63603073817900224, 11.04745617521000156 ) ) ;
#15942 = CARTESIAN_POINT ( 'NONE',  ( -10.15970891481431515, -76.81842413191742480, 4.240029984634371196 ) ) ;
#15943 = CONICAL_SURFACE ( 'NONE', #20661, 12.14999999923000118, 0.7853981633972997312 ) ;
#15944 = CARTESIAN_POINT ( 'NONE',  ( -11.10694245833507310, -79.07649623643344228, -3.897797401036807496 ) ) ;
#15945 = CARTESIAN_POINT ( 'NONE',  ( -1.397634362971892807, -81.93340492005572173, -0.6272248289412739597 ) ) ;
#15946 = CARTESIAN_POINT ( 'NONE',  ( 1.118977020825177249, -81.38716913225974281, 0.5574429764450725688 ) ) ;
#15947 = CARTESIAN_POINT ( 'NONE',  ( 1.103779259214931585, -78.85851262082059066, -0.6375342514394781723 ) ) ;
#15948 = CARTESIAN_POINT ( 'NONE',  ( -1.093124704215232557, -82.14231321599577029, -0.6293855122744574926 ) ) ;
#15949 = CARTESIAN_POINT ( 'NONE',  ( -7.836764916234015388, -24.30511429678721669, -9.850487231000789379 ) ) ;
#15950 = EDGE_CURVE ( 'NONE', #38673, #37604, #300, .T. ) ;
#15951 = CARTESIAN_POINT ( 'NONE',  ( 9.559505855103624938, -76.07072051956410519, -5.521514537851864191 ) ) ;
#15952 = DIRECTION ( 'NONE',  ( 0.000000000000000000, 1.000000000000000000, 0.000000000000000000 ) ) ;
#15953 = CARTESIAN_POINT ( 'NONE',  ( 0.5999999999999999778, -5.200000000000000178, -0.5999999999999999778 ) ) ;
#15954 = EDGE_LOOP ( 'NONE', ( #41216, #21020, #25312, #1168, #16570 ) ) ;
#15955 = VERTEX_POINT ( 'NONE', #54294 ) ;
#15956 = CARTESIAN_POINT ( 'NONE',  ( -6.169654037346999687, -76.24235318827498986, 10.97285421267000061 ) ) ;
#15957 = CARTESIAN_POINT ( 'NONE',  ( 0.1192520569309659245, -78.72596489933566488, -10.74939088699284362 ) ) ;
#15958 = EDGE_LOOP ( 'NONE', ( #10881, #24755, #4264, #4412 ) ) ;
#15959 = VERTEX_POINT ( 'NONE', #14408 ) ;
#15960 = CARTESIAN_POINT ( 'NONE',  ( 10.35410226330999883, -18.59601732823000120, 7.619716344073999892 ) ) ;
#15961 = CARTESIAN_POINT ( 'NONE',  ( -9.702392362153268834, -78.85149179162094413, -0.1934172642948918386 ) ) ;
#15962 = AXIS2_PLACEMENT_3D ( 'NONE', #26427, #4895, #12853 ) ;
#15963 = CARTESIAN_POINT ( 'NONE',  ( 0.6484536763455558406, -53.67597017258059822, 12.70397497887483063 ) ) ;
#15964 = CARTESIAN_POINT ( 'NONE',  ( 11.66345872527999994, -77.95231164849001004, 5.269998857220999255 ) ) ;
#15965 = CARTESIAN_POINT ( 'NONE',  ( -6.606081245964748661, -79.67294187189699528, -8.595967819608736349 ) ) ;
#15966 = DIRECTION ( 'NONE',  ( 0.000000000000000000, 0.000000000000000000, -1.000000000000000000 ) ) ;
#15967 = CARTESIAN_POINT ( 'NONE',  ( -0.7554284705563544255, -79.91666666666667140, 1.310679582531384169 ) ) ;
#15968 = CARTESIAN_POINT ( 'NONE',  ( -6.324515969367999979, -78.91122516221300032, -9.263833350438000380 ) ) ;
#15969 = VERTEX_POINT ( 'NONE', #46322 ) ;
#15970 = LINE ( 'NONE', #11554, #17097 ) ;
#15971 = ORIENTED_EDGE ( 'NONE', *, *, #6507, .F. ) ;
#15972 = EDGE_CURVE ( 'NONE', #47577, #22104, #50729, .T. ) ;
#15973 = CARTESIAN_POINT ( 'NONE',  ( 7.486916784802780889, -77.30012800153166097, -5.432092700114928618 ) ) ;
#15974 = CARTESIAN_POINT ( 'NONE',  ( 12.50412785609288058, -61.31985834570178184, -1.235051470171430577 ) ) ;
#15975 = CARTESIAN_POINT ( 'NONE',  ( 7.919595949288999570, -59.94999999446000771, -8.768124086549999419 ) ) ;
#15976 = AXIS2_PLACEMENT_3D ( 'NONE', #17230, #3942, #18124 ) ;
#15977 = LINE ( 'NONE', #42559, #58331 ) ;
#15978 = UNCERTAINTY_MEASURE_WITH_UNIT (LENGTH_MEASURE( 1.000000000000000082E-05 ), #33736, 'distance_accuracy_value', 'NONE');
#15979 = CARTESIAN_POINT ( 'NONE',  ( -1.223493401540999947, -79.06053370013900405, 0.7163828769940999708 ) ) ;
#15980 = LINE ( 'NONE', #2128, #24750 ) ;
#15981 = CARTESIAN_POINT ( 'NONE',  ( -10.41144070832756618, -18.47453159777755261, 7.610433246107068506 ) ) ;
#15982 = CARTESIAN_POINT ( 'NONE',  ( -1.578837173282999995, -79.36932442800998899, 0.3948290484592000271 ) ) ;
#15983 = CARTESIAN_POINT ( 'NONE',  ( -9.312499999988999022, -77.13750000001088836, -2.050180145195999796E-09 ) ) ;
#15984 = CARTESIAN_POINT ( 'NONE',  ( -9.152236916771000708, -78.94574075788399625, 6.189866966782000546 ) ) ;
#15985 = CARTESIAN_POINT ( 'NONE',  ( 5.285146527633999725, -77.77108832859899223, 7.886954000319999381 ) ) ;
#15986 = SURFACE_STYLE_FILL_AREA ( #43152 ) ;
#15987 = B_SPLINE_CURVE_WITH_KNOTS ( 'NONE', 3,
 ( #50959, #10510, #3390, #42970, #34374, #33795, #20242, #12527, #20530, #21386 ),
 .UNSPECIFIED., .F., .F.,
 ( 4, 2, 2, 2, 4 ),
 ( 0.000000000000000000, 0.2500000000000001110, 0.5000000000000001110, 0.7500000000000001110, 1.000000000000000000 ),
 .UNSPECIFIED. ) ;
#15988 = DIRECTION ( 'NONE',  ( 0.000000000000000000, -1.000000000000000000, 0.000000000000000000 ) ) ;
#15989 = EDGE_CURVE ( 'NONE', #22563, #19308, #23584, .T. ) ;
#15990 = CARTESIAN_POINT ( 'NONE',  ( -2.280909059783999826, -83.42080844866399048, -2.716435822977000036 ) ) ;
#15991 = ORIENTED_EDGE ( 'NONE', *, *, #17830, .T. ) ;
#15992 = CARTESIAN_POINT ( 'NONE',  ( -0.2501781407124171741, -77.20000000000001705, 10.80171731040410243 ) ) ;
#15993 = CARTESIAN_POINT ( 'NONE',  ( -0.5553526962645999321, -81.42553171121998901, -1.429183993495000138 ) ) ;
#15994 = CARTESIAN_POINT ( 'NONE',  ( -9.393470487601941699, -79.14183230196326235, -5.414092425894560634 ) ) ;
#15995 = EDGE_CURVE ( 'NONE', #2820, #35308, #10217, .T. ) ;
#15996 = CARTESIAN_POINT ( 'NONE',  ( -6.777984382448000389, -78.07546061570199925, -9.878005474088999094 ) ) ;
#15997 = CARTESIAN_POINT ( 'NONE',  ( -9.770419344679000417, -16.94469452567000189, 8.292776877939001423 ) ) ;
#15998 = CARTESIAN_POINT ( 'NONE',  ( 1.012512968712311334, -78.05232246393418905, 0.7737093686211432564 ) ) ;
#15999 = CARTESIAN_POINT ( 'NONE',  ( -2.415176324861053825, -2.314881229756596603, -2.560669143145342996 ) ) ;
#16000 = CARTESIAN_POINT ( 'NONE',  ( 10.41713664689605245, -80.87023554807993264, 2.654027955184751431 ) ) ;
#16001 = CARTESIAN_POINT ( 'NONE',  ( 8.393017115181999444, -78.92888658829198789, 4.056188317180000169 ) ) ;
#16002 = CARTESIAN_POINT ( 'NONE',  ( 1.807051837521999937, -54.49921584723999501, -12.77977401831000037 ) ) ;
#16003 = CARTESIAN_POINT ( 'NONE',  ( 8.061453700986000115, -77.76865691654299440, 7.530916186516999566 ) ) ;
#16004 = CARTESIAN_POINT ( 'NONE',  ( 8.039723150245000838, -80.33398629742849550, 7.069263470143000383 ) ) ;
#16005 = CARTESIAN_POINT ( 'NONE',  ( 0.1532075572505490757, -81.78438528175662725, -1.264636186328577105 ) ) ;
#16006 = VERTEX_POINT ( 'NONE', #55450 ) ;
#16007 = FACE_OUTER_BOUND ( 'NONE', #27848, .T. ) ;
#16008 = CARTESIAN_POINT ( 'NONE',  ( 10.27304407731668690, -76.98877676696531580, 5.920460778062027529 ) ) ;
#16009 = CARTESIAN_POINT ( 'NONE',  ( -0.9781264271446999947, -61.74031143843999558, -12.65967462882999861 ) ) ;
#16010 = CARTESIAN_POINT ( 'NONE',  ( 1.407384697719938904, -80.46469927918771248, 10.68108411319174245 ) ) ;
#16011 = CARTESIAN_POINT ( 'NONE',  ( 0.5473670387515998659, -76.89499053265299722, -11.20350390113000039 ) ) ;
#16012 = CARTESIAN_POINT ( 'NONE',  ( -7.508490145779999736, -78.93489658277098897, -8.005410190140000992 ) ) ;
#16013 = CARTESIAN_POINT ( 'NONE',  ( 10.47840054245999930, -23.78693148451999662, -7.622763498569999463 ) ) ;
#16014 = CARTESIAN_POINT ( 'NONE',  ( 3.915023737200626908, -85.50260417986531536, 0.8776777806838870211 ) ) ;
#16015 = DIRECTION ( 'NONE',  ( 1.000000000000000000, 0.000000000000000000, 0.000000000000000000 ) ) ;
#16016 = CARTESIAN_POINT ( 'NONE',  ( 9.734666230076248539, -78.49530485907877164, 6.578030644441952290 ) ) ;
#16017 = LINE ( 'NONE', #21019, #36205 ) ;
#16018 = ORIENTED_EDGE ( 'NONE', *, *, #47840, .F. ) ;
#16019 = CYLINDRICAL_SURFACE ( 'NONE', #56914, 1.000000000000000000 ) ;
#16020 = EDGE_CURVE ( 'NONE', #17027, #42621, #13949, .T. ) ;
#16021 = CARTESIAN_POINT ( 'NONE',  ( -2.743382484896518925, -75.80000000000001137, -11.44562466199204032 ) ) ;
#16022 = B_SPLINE_CURVE_WITH_KNOTS ( 'NONE', 3,
 ( #46399, #11535, #10669, #5926, #1519, #47275 ),
 .UNSPECIFIED., .F., .F.,
 ( 4, 1, 1, 4 ),
 ( 0.000000000000000000, 0.3333333333333000081, 0.6666666666667000474, 1.000000000000000000 ),
 .UNSPECIFIED. ) ;
#16023 = CARTESIAN_POINT ( 'NONE',  ( -9.688835989853998854, -79.22180445808699290, -5.749381838710999837 ) ) ;
#16024 = CARTESIAN_POINT ( 'NONE',  ( -6.464912241513801260E-06, -79.20362641130290626, -11.95086305119197689 ) ) ;
#16025 = CARTESIAN_POINT ( 'NONE',  ( 9.396085398178598780, -77.60208333333331154, 7.220923959705271677 ) ) ;
#16026 = DIRECTION ( 'NONE',  ( 0.000000000000000000, -1.000000000000000000, 0.000000000000000000 ) ) ;
#16027 = VECTOR ( 'NONE', #57680, 1000.000000000000114 ) ;
#16028 = CARTESIAN_POINT ( 'NONE',  ( -0.7285324502130352542, -82.93438848133038732, -1.325323562101084152 ) ) ;
#16029 = CARTESIAN_POINT ( 'NONE',  ( 0.9143677338810914934, -79.79065590062214142, -0.8521684201040128359 ) ) ;
#16030 = ADVANCED_FACE ( 'NONE', ( #54862 ), #35632, .T. ) ;
#16031 = AXIS2_PLACEMENT_3D ( 'NONE', #44055, #16327, #7170 ) ;
#16032 = CARTESIAN_POINT ( 'NONE',  ( -7.770365053994759741, -54.56417299442668423, 10.20675369723379156 ) ) ;
#16033 = VERTEX_POINT ( 'NONE', #14994 ) ;
#16034 = ADVANCED_FACE ( 'NONE', ( #50161 ), #9416, .F. ) ;
#16035 = CARTESIAN_POINT ( 'NONE',  ( 1.799502287743000029, -18.69283065396999888, 12.60413652832999887 ) ) ;
#16036 =( NAMED_UNIT ( * ) PLANE_ANGLE_UNIT ( ) SI_UNIT ( $, .RADIAN. ) );
#16037 = CARTESIAN_POINT ( 'NONE',  ( -7.220923959705292994, -76.22708333333335418, 9.396085398178589898 ) ) ;
#16038 = ORIENTED_EDGE ( 'NONE', *, *, #32419, .F. ) ;
#16039 = EDGE_LOOP ( 'NONE', ( #57416, #50030, #39184, #33308 ) ) ;
#16040 = CARTESIAN_POINT ( 'NONE',  ( -12.54673279569000144, -53.97202488745999460, -0.9078290272348999990 ) ) ;
#16041 = VERTEX_POINT ( 'NONE', #49575 ) ;
#16042 = VERTEX_POINT ( 'NONE', #27108 ) ;
#16043 = CARTESIAN_POINT ( 'NONE',  ( -10.50414906643726987, -81.00000000000000000, -2.423834968728446615 ) ) ;
#16044 = CARTESIAN_POINT ( 'NONE',  ( 7.307192483546000261, -76.75676689867499647, -8.110505779365999146 ) ) ;
#16045 = FACE_BOUND ( 'NONE', #37077, .T. ) ;
#16046 = CARTESIAN_POINT ( 'NONE',  ( 4.582566119076999733, -78.09363667140100063, 8.787281441338999244 ) ) ;
#16047 = CARTESIAN_POINT ( 'NONE',  ( -1.966495496757295847, -78.20800177901919881, -9.040030525289719066 ) ) ;
#16048 = CARTESIAN_POINT ( 'NONE',  ( 4.601194894417628412, -79.33389418958066130, 8.114662363814824531 ) ) ;
#16049 = ORIENTED_EDGE ( 'NONE', *, *, #36427, .F. ) ;
#16050 = CIRCLE ( 'NONE', #43390, 1.750000000000002887 ) ;
#16051 = ORIENTED_EDGE ( 'NONE', *, *, #41797, .F. ) ;
#16052 = CARTESIAN_POINT ( 'NONE',  ( -6.677150611632656663, -77.53932992427476734, 6.401716840538735021 ) ) ;
#16053 = FACE_OUTER_BOUND ( 'NONE', #55100, .T. ) ;
#16054 = FACE_OUTER_BOUND ( 'NONE', #20546, .T. ) ;
#16055 = CARTESIAN_POINT ( 'NONE',  ( 9.259046916275000427, -78.60434699719698415, 2.905298533503999803 ) ) ;
#16056 = CARTESIAN_POINT ( 'NONE',  ( 3.654181830570521594, -86.09999999999978115, -1.626946572303536120 ) ) ;
#16057 = CARTESIAN_POINT ( 'NONE',  ( 9.841120606634161661, -61.63627250028590510, 8.121699444636400145 ) ) ;
#16058 = CARTESIAN_POINT ( 'NONE',  ( -5.413904038987160661, -76.58333333333330017, -9.393203674808278336 ) ) ;
#16059 = CARTESIAN_POINT ( 'NONE',  ( -9.596002108778193929, -76.84791666666663446, 7.374560639698937159 ) ) ;
#16060 = CARTESIAN_POINT ( 'NONE',  ( -1.576937714420000081, -81.23916334729999278, 0.6430338560479000876 ) ) ;
#16061 = CARTESIAN_POINT ( 'NONE',  ( -0.7089775319598999870, -82.20557270575599773, -1.075828666865999983 ) ) ;
#16062 = CARTESIAN_POINT ( 'NONE',  ( -9.752024281374076509, -76.65249643834691540, 6.553952695904345482 ) ) ;
#16063 = APPLICATION_CONTEXT ( 'automotive_design' ) ;
#16064 = CARTESIAN_POINT ( 'NONE',  ( -0.1057940869841550030, -79.86936252454921714, -1.506682504695135982 ) ) ;
#16066 = ADVANCED_FACE ( 'NONE', ( #19147 ), #37142, .F. ) ;
#16065 = CARTESIAN_POINT ( 'NONE',  ( -7.589275504201999922, -78.06138667140099585, -6.198488971763000066 ) ) ;
#16067 = CARTESIAN_POINT ( 'NONE',  ( -10.69999999999999929, -77.19999999999998863, 0.000000000000000000 ) ) ;
#16068 = CARTESIAN_POINT ( 'NONE',  ( 1.931086388455000025, -18.70221404512000163, -12.71798280854999952 ) ) ;
#16069 = B_SPLINE_CURVE_WITH_KNOTS ( 'NONE', 3,
 ( #14964, #24711, #11149, #9969, #45999, #32961, #1704, #51006, #10555, #28538, #46586, #6111, #42137, #19999, #56009 ),
 .UNSPECIFIED., .F., .F.,
 ( 4, 1, 1, 1, 1, 1, 1, 1, 1, 1, 1, 1, 4 ),
 ( 0.000000000000000000, 0.08333615652962080012, 0.1666676882018690575, 0.2500040233444769111, 0.3333307240648036851, 0.4166666719153997445, 0.4999999897769762947, 0.5833333086325983574, 0.6666692895637478244, 0.7499959966207713213, 0.8333323107868229052, 0.9166638646071934016, 1.000000000000000000 ),
 .UNSPECIFIED. ) ;
#16070 = VECTOR ( 'NONE', #48213, 1000.000000000000114 ) ;
#16072 = CARTESIAN_POINT ( 'NONE',  ( 1.000000000000000000, -75.20000000000000284, -7.200000000000000178 ) ) ;
#16071 = CYLINDRICAL_SURFACE ( 'NONE', #45749, 0.5000000000000006661 ) ;
#16073 = CIRCLE ( 'NONE', #56611, 0.5000000000000001110 ) ;
#16074 = CARTESIAN_POINT ( 'NONE',  ( -1.639137479228926164, -1.184957622258020926, -2.839660048845916052 ) ) ;
#16075 = CARTESIAN_POINT ( 'NONE',  ( 8.396295933391000332, -80.12268549011298546, -7.217020962015999963 ) ) ;
#16076 = CARTESIAN_POINT ( 'NONE',  ( -0.4831833036036000117, -82.22787956406298804, -1.158768654956999988 ) ) ;
#16077 = DIRECTION ( 'NONE',  ( -1.000000000000000000, 0.000000000000000000, 0.000000000000000000 ) ) ;
#16078 = LINE ( 'NONE', #47967, #48666 ) ;
#16079 = ORIENTED_EDGE ( 'NONE', *, *, #38706, .F. ) ;
#16080 = CARTESIAN_POINT ( 'NONE',  ( -3.248956906310343395, -1.591438635919541156, 0.4262020595363264497 ) ) ;
#16081 = FACE_OUTER_BOUND ( 'NONE', #23158, .T. ) ;
#16082 = DIRECTION ( 'NONE',  ( 0.000000000000000000, 1.000000000000000000, 0.000000000000000000 ) ) ;
#16083 = CARTESIAN_POINT ( 'NONE',  ( 0.8124100789227103325, -78.41886625915758202, 0.9503163788704104276 ) ) ;
#16084 = CARTESIAN_POINT ( 'NONE',  ( -5.076456076831999731, -80.03725306992998867, -8.069692061488998647 ) ) ;
#16085 = CARTESIAN_POINT ( 'NONE',  ( -12.66761570926000147, -54.57632520071999949, 1.696752301450999978 ) ) ;
#16086 = DIRECTION ( 'NONE',  ( 0.000000000000000000, -1.000000000000000000, 0.000000000000000000 ) ) ;
#16087 = CARTESIAN_POINT ( 'NONE',  ( 1.460959015002474048, -80.22916666666668561, -0.3926218265389178064 ) ) ;
#16088 = DIRECTION ( 'NONE',  ( 0.7071067811865474617, -0.7071067811865474617, 7.724133980720514139E-12 ) ) ;
#16089 = EDGE_CURVE ( 'NONE', #5425, #34724, #45439, .T. ) ;
#16090 = DIRECTION ( 'NONE',  ( -1.000000000000000000, 0.000000000000000000, 0.000000000000000000 ) ) ;
#16091 = CARTESIAN_POINT ( 'NONE',  ( -3.999289405514205864, -78.67389998729011324, -0.07539397150087834287 ) ) ;
#16092 = ADVANCED_FACE ( 'NONE', ( #55151 ), #53571, .F. ) ;
#16093 = CARTESIAN_POINT ( 'NONE',  ( -2.917097991912000143, -77.97435053980699138, -10.55202616546000094 ) ) ;
#16094 = VECTOR ( 'NONE', #8097, 1000.000000000000000 ) ;
#16095 = CARTESIAN_POINT ( 'NONE',  ( 2.381202143020299644, -76.34051971754411170, -11.52415263934972245 ) ) ;
#16096 = CARTESIAN_POINT ( 'NONE',  ( -9.149418163674001292, -76.68831224807900071, -6.163594735446999984 ) ) ;
#16097 = CARTESIAN_POINT ( 'NONE',  ( 5.896171905175000560, -77.96999999999999886, 7.127247495676000355 ) ) ;
#16098 = CARTESIAN_POINT ( 'NONE',  ( -1.504841238612000032, -78.86507235081998601, -0.7092193051005999394 ) ) ;
#16099 = CARTESIAN_POINT ( 'NONE',  ( -9.555818165766000405, -77.27086163495798132, -0.1257991660602000017 ) ) ;
#16100 = CARTESIAN_POINT ( 'NONE',  ( 0.3926218265389159190, -78.85416666666667140, 1.460959015002474715 ) ) ;
#16101 = CARTESIAN_POINT ( 'NONE',  ( -1.004305231718999991, -3.500000000000000000, 3.090933677959000203 ) ) ;
#16102 = CARTESIAN_POINT ( 'NONE',  ( 5.994180301456028204, -80.27253328818157740, -8.923361141312334155 ) ) ;
#16103 = DIRECTION ( 'NONE',  ( 0.9999380042107527400, 0.000000000000000000, -0.01113497799803945566 ) ) ;
#16104 = CARTESIAN_POINT ( 'NONE',  ( 4.914100338553271996, -75.80000000000001137, 11.02085870159172032 ) ) ;
#16105 = EDGE_CURVE ( 'NONE', #18787, #54024, #13015, .T. ) ;
#16106 = CARTESIAN_POINT ( 'NONE',  ( -0.9103933733443999587, -79.61728894252300393, -11.99492895764000089 ) ) ;
#16107 = CARTESIAN_POINT ( 'NONE',  ( -1.249634766890562743, -78.11054148323580648, -0.1635212922017194592 ) ) ;
#16108 = CARTESIAN_POINT ( 'NONE',  ( 10.16136252780999882, -79.60888520700200388, 4.855993836148999598 ) ) ;
#16109 = ORIENTED_EDGE ( 'NONE', *, *, #38593, .F. ) ;
#16110 = CARTESIAN_POINT ( 'NONE',  ( 7.648026768036999989, -60.04999998387000204, 10.12290050219000115 ) ) ;
#16111 = EDGE_LOOP ( 'NONE', ( #53501, #35913, #29719, #9805, #47510 ) ) ;
#16112 = VERTEX_POINT ( 'NONE', #32699 ) ;
#16113 = CARTESIAN_POINT ( 'NONE',  ( -1.636761686205434385, -1.416666666666666297, 2.839805762151331958 ) ) ;
#16114 = ORIENTED_EDGE ( 'NONE', *, *, #55399, .T. ) ;
#16115 = CARTESIAN_POINT ( 'NONE',  ( 0.5654955014232999622, -82.16974633842799847, -3.499305150839000067 ) ) ;
#16116 = CARTESIAN_POINT ( 'NONE',  ( 5.732671476984768866, -79.22339475712911394, 7.582784944364554747 ) ) ;
#16117 = EDGE_CURVE ( 'NONE', #13664, #11409, #50747, .T. ) ;
#16118 = ORIENTED_EDGE ( 'NONE', *, *, #47396, .T. ) ;
#16119 = CARTESIAN_POINT ( 'NONE',  ( -3.444266691755999865, -78.40360489188999793, 11.59182779477000125 ) ) ;
#16120 = CARTESIAN_POINT ( 'NONE',  ( 0.6330385443858000949, -2.195518323557999807, -3.341926243291000187 ) ) ;
#16121 = ORIENTED_EDGE ( 'NONE', *, *, #2763, .T. ) ;
#16122 = CARTESIAN_POINT ( 'NONE',  ( 0.4024786306066807651, -79.44944984597937321, 1.183223541616218011 ) ) ;
#16123 = CARTESIAN_POINT ( 'NONE',  ( -0.9504519148020524888, -79.17842417668877886, 1.203406266442021977 ) ) ;
#16124 = LINE ( 'NONE', #49673, #28387 ) ;
#16125 = CARTESIAN_POINT ( 'NONE',  ( -10.54604950822804454, -80.08464066063081077, 2.090755568749749216 ) ) ;
#16126 = DIRECTION ( 'NONE',  ( 0.000000000000000000, -1.000000000000000000, 0.000000000000000000 ) ) ;
#16127 = B_SPLINE_CURVE_WITH_KNOTS ( 'NONE', 3,
 ( #31611, #22478, #10080, #45222, #32775, #49652, #9199, #951, #40489, #50820, #36344, #54371, #14489, #22770, #50526, #18935, #27771, #5632 ),
 .UNSPECIFIED., .F., .F.,
 ( 4, 2, 2, 2, 2, 2, 2, 2, 4 ),
 ( 0.000000000000000000, 0.1250000000000000555, 0.2500000000000001110, 0.3750000000000001665, 0.5000000000000001110, 0.6250000000000001110, 0.7500000000000002220, 0.8750000000000001110, 1.000000000000000000 ),
 .UNSPECIFIED. ) ;
#16128 = CARTESIAN_POINT ( 'NONE',  ( 3.106054555984424148, -86.12609999968211127, -1.382904586457713858 ) ) ;
#16129 = CARTESIAN_POINT ( 'NONE',  ( 7.778176538613999824, -76.58788662847199191, -8.035785801754000701 ) ) ;
#16130 = CARTESIAN_POINT ( 'NONE',  ( -9.674786689060324463, -79.84246777690499641, 0.8964806179170247136 ) ) ;
#16131 = CARTESIAN_POINT ( 'NONE',  ( -0.7271731550489020091, -81.26431952766002098, 1.327098488219002004 ) ) ;
#16132 = CARTESIAN_POINT ( 'NONE',  ( -4.924589481749999997, -76.87080480866698906, 9.835153137904999454 ) ) ;
#16133 = CARTESIAN_POINT ( 'NONE',  ( -5.884541003006559912, -78.67027905328879456, -7.138263159130112889 ) ) ;
#16134 = AXIS2_PLACEMENT_3D ( 'NONE', #56615, #57760, #8177 ) ;
#16135 = CARTESIAN_POINT ( 'NONE',  ( 0.5765222740522000233, -80.01753900141099507, 1.202579817323000233 ) ) ;
#16136 = B_SPLINE_CURVE_WITH_KNOTS ( 'NONE', 3,
 ( #5996, #46178, #42319, #733, #19881, #24002, #33440, #37874, #51476, #5703, #32843, #54722, #14265, #32262, #50307, #9857, #27839, #52052, #15734, #34594, #2174, #21030, #25169, #51765, #29872, #2458, #12174, #16028, #11609, #57331, #43476, #34306, #47640, #7164, #29583, #43192, #52337, #52906, #52622, #11317, #30161, #47925, #2745, #7458, #48210, #7743, #33730, #24596, #25742, #6874, #43769, #34877, #16894, #11893, #42610, #20746, #25457, #24883, #38744, #56186, #56764, #16324, #3319, #38162, #12455, #3033, #20463, #39036, #42899, #30451, #6585, #57047, #16606, #29297, #47346, #21313, #39324, #34016, #20174, #38455, #56472, #35448, #54074, #371, #18352, #45219, #4181, #22475, #8026, #22177, #30733, #26313, #26022, #22769, #26894, #27181, #36342, #58200, #4768, #54368, #40486, #35750, #57612, #53480, #17172, #18059, #44051, #31019 ),
 .UNSPECIFIED., .F., .F.,
 ( 4, 2, 2, 2, 2, 2, 1, 2, 2, 2, 2, 2, 2, 2, 2, 2, 2, 2, 2, 2, 2, 2, 2, 2, 2, 2, 2, 2, 2, 2, 2, 2, 2, 2, 2, 2, 2, 2, 2, 2, 2, 2, 2, 2, 2, 2, 2, 2, 1, 2, 2, 2, 2, 2, 4 ),
 ( 0.000000000000000000, 0.01562500000000003469, 0.03125000000000006939, 0.04687500000000011796, 0.06250000000000016653, 0.07812500000000022204, 0.09375000000000024980, 0.1093750000000002914, 0.1250000000000003331, 0.1406250000000003608, 0.1562500000000004163, 0.1718750000000004441, 0.1875000000000004718, 0.2031250000000004996, 0.2187500000000005274, 0.2343750000000005274, 0.2500000000000004996, 0.2656250000000005551, 0.2812500000000005551, 0.2968750000000006106, 0.3125000000000006106, 0.3281250000000006661, 0.3437500000000007216, 0.3750000000000007216, 0.4062500000000007216, 0.4375000000000007216, 0.4687500000000007772, 0.5000000000000007772, 0.5312500000000007772, 0.5625000000000006661, 0.5937500000000006661, 0.6250000000000005551, 0.6562500000000005551, 0.6718750000000005551, 0.6875000000000006661, 0.7031250000000005551, 0.7187500000000004441, 0.7343750000000004441, 0.7500000000000003331, 0.7656250000000002220, 0.7812500000000002220, 0.7968750000000001110, 0.8125000000000000000, 0.8281250000000001110, 0.8437500000000001110, 0.8593750000000001110, 0.8750000000000001110, 0.8906250000000002220, 0.9062500000000002220, 0.9218750000000002220, 0.9375000000000003331, 0.9531250000000002220, 0.9687500000000001110, 0.9843750000000001110, 1.000000000000000000 ),
 .UNSPECIFIED. ) ;
#16137 = CARTESIAN_POINT ( 'NONE',  ( -10.34820832961891490, -80.12787718711169305, -3.730169475059172957 ) ) ;
#16138 = CARTESIAN_POINT ( 'NONE',  ( -2.486604901413195456, -77.19583333333333997, 9.252740428348991131 ) ) ;
#16139 = CARTESIAN_POINT ( 'NONE',  ( 3.843843246054999607, -82.12920122123499311, -0.2533605254773000359 ) ) ;
#16140 = CARTESIAN_POINT ( 'NONE',  ( -9.963109346188520732, -78.06943961487655770, 4.037170563993010219 ) ) ;
#16141 = CARTESIAN_POINT ( 'NONE',  ( 9.000000000000000000, -0.2000000000000000111, 0.000000000000000000 ) ) ;
#16142 =( NAMED_UNIT ( * ) SI_UNIT ( $, .STERADIAN. ) SOLID_ANGLE_UNIT ( ) );
#16143 = CARTESIAN_POINT ( 'NONE',  ( -2.847633505915000196, -83.03494503318799502, 2.114839446580000004 ) ) ;
#16144 = CARTESIAN_POINT ( 'NONE',  ( -6.767262360081500283, -76.27600367820089389, -9.605998308841860123 ) ) ;
#16145 = CARTESIAN_POINT ( 'NONE',  ( 10.21381326472000062, -22.77129148951999937, 7.668949790003000366 ) ) ;
#16146 = CARTESIAN_POINT ( 'NONE',  ( -7.622785526051999661, -60.58712283452999259, -10.47836401508999948 ) ) ;
#16147 = CARTESIAN_POINT ( 'NONE',  ( -6.745911349169843696, -79.22231418035541139, 9.981325353439961745 ) ) ;
#16148 = CARTESIAN_POINT ( 'NONE',  ( -5.500000000000000000, -80.99999999999998579, 0.000000000000000000 ) ) ;
#16149 = AXIS2_PLACEMENT_3D ( 'NONE', #18517, #31477, #49221 ) ;
#16150 = CARTESIAN_POINT ( 'NONE',  ( 9.249483092228999226, -79.25084128437099196, 0.09778817195952001218 ) ) ;
#16151 = CARTESIAN_POINT ( 'NONE',  ( -12.97861384075000046, -78.05778978748000441, -0.9459496016724999734 ) ) ;
#16152 = VECTOR ( 'NONE', #3103, 1000.000000000000000 ) ;
#16153 = CARTESIAN_POINT ( 'NONE',  ( -10.75519713130186261, -77.95494529858517296, -0.6025658906798456727 ) ) ;
#16154 = CARTESIAN_POINT ( 'NONE',  ( -10.26030881462940947, -78.24069963102668623, -5.914557015925677952 ) ) ;
#16155 = ADVANCED_FACE ( 'NONE', ( #2314 ), #20309, .T. ) ;
#16156 = CARTESIAN_POINT ( 'NONE',  ( -0.5999999999999999778, -18.84999999999999787, -10.98362417419999915 ) ) ;
#16157 = CARTESIAN_POINT ( 'NONE',  ( -12.26667365293000067, -76.09135856455000635, -1.533824757711000020 ) ) ;
#16158 = EDGE_LOOP ( 'NONE', ( #40316, #50178, #1733, #53932 ) ) ;
#16159 = CARTESIAN_POINT ( 'NONE',  ( 7.496935112050000072, -80.56705559776401060, 8.408636027568000770 ) ) ;
#16160 = DIRECTION ( 'NONE',  ( 0.7071067811865474617, -0.7071067811865474617, -3.205711300058212616E-10 ) ) ;
#16161 = CARTESIAN_POINT ( 'NONE',  ( 12.54715528154999937, -61.33180535358000185, 1.292252957172000061 ) ) ;
#16162 = CARTESIAN_POINT ( 'NONE',  ( -5.286038998608000306, -79.16541925342001207, 11.30782674599000082 ) ) ;
#16163 = CARTESIAN_POINT ( 'NONE',  ( -12.50000000000000000, -18.75000000000000000, -1.250000000000000000 ) ) ;
#16164 = CARTESIAN_POINT ( 'NONE',  ( 3.223804565277000211, -78.24090022703498448, 9.075257246486000184 ) ) ;
#16165 = CARTESIAN_POINT ( 'NONE',  ( -4.134529906664000443, -83.18030761812998719, 0.5619030602642999250 ) ) ;
#16166 = CARTESIAN_POINT ( 'NONE',  ( 6.436424241555000592, -79.92391735373439587, 8.610165096135999008 ) ) ;
#16167 = CARTESIAN_POINT ( 'NONE',  ( -1.597158643424000157, -79.98020634875099688, 0.2372724044997999993 ) ) ;
#16168 = VERTEX_POINT ( 'NONE', #33581 ) ;
#16169 = DIRECTION ( 'NONE',  ( 0.000000000000000000, 0.000000000000000000, -1.000000000000000000 ) ) ;
#16170 = CARTESIAN_POINT ( 'NONE',  ( 1.550761107483941137, -78.94176543215372988, -3.175578139143914846 ) ) ;
#16171 = VERTEX_POINT ( 'NONE', #33863 ) ;
#16172 = EDGE_CURVE ( 'NONE', #313, #35853, #28375, .T. ) ;
#16173 = CARTESIAN_POINT ( 'NONE',  ( 10.78711022396000097, -79.57429477431499265, 2.390846439793999689 ) ) ;
#16174 = CARTESIAN_POINT ( 'NONE',  ( -8.190836719257346132, -55.61035107871763472, -7.342356150419313998 ) ) ;
#16175 = CARTESIAN_POINT ( 'NONE',  ( -1.171666301184231207, -80.63007484519644663, -0.4570117860640778851 ) ) ;
#16176 = EDGE_LOOP ( 'NONE', ( #11742, #54875, #24003, #45381, #4263 ) ) ;
#16177 = CARTESIAN_POINT ( 'NONE',  ( 8.821626479137000487, -79.00077142985099954, 8.208219718620000549 ) ) ;
#16178 = CARTESIAN_POINT ( 'NONE',  ( 10.22337536533999902, -78.27158863368499908, -4.865471675980000299 ) ) ;
#16179 = ORIENTED_EDGE ( 'NONE', *, *, #57168, .T. ) ;
#16180 = B_SPLINE_CURVE_WITH_KNOTS ( 'NONE', 3,
 ( #4432, #21841, #39848, #30406 ),
 .UNSPECIFIED., .F., .F.,
 ( 4, 4 ),
 ( 0.000000000000000000, 1.000000000000000000 ),
 .UNSPECIFIED. ) ;
#16181 = ORIENTED_EDGE ( 'NONE', *, *, #1537, .F. ) ;
#16182 = EDGE_CURVE ( 'NONE', #42830, #40288, #57326, .T. ) ;
#16183 = CARTESIAN_POINT ( 'NONE',  ( 0.3529067879003955910, -80.45250755409055898, 1.199236710938469397 ) ) ;
#16184 = CARTESIAN_POINT ( 'NONE',  ( 11.74527629117004857, -77.95727216427877693, 1.539259998173173827 ) ) ;
#16185 = CARTESIAN_POINT ( 'NONE',  ( -2.217000330786000450, -79.40352863330448940, 9.512392227823999846 ) ) ;
#16186 = ADVANCED_FACE ( 'NONE', ( #48624 ), #19506, .T. ) ;
#16187 = ORIENTED_EDGE ( 'NONE', *, *, #2907, .F. ) ;
#16188 = CARTESIAN_POINT ( 'NONE',  ( -2.599682250000723727, -2.548992540563667752, 1.997718607485681863 ) ) ;
#16189 = ORIENTED_EDGE ( 'NONE', *, *, #5513, .T. ) ;
#16190 = AXIS2_PLACEMENT_3D ( 'NONE', #55250, #50838, #12119 ) ;
#16191 = CARTESIAN_POINT ( 'NONE',  ( 1.274386203284063823, -79.39916300381975134, -0.01037360266173210400 ) ) ;
#16192 = CARTESIAN_POINT ( 'NONE',  ( 9.502896617881404495, -24.74094210335991662, 8.179425869167879171 ) ) ;
#16193 = CIRCLE ( 'NONE', #7712, 1.750000000000001332 ) ;
#16194 = CARTESIAN_POINT ( 'NONE',  ( 8.194873807802000698, -54.08956116737999764, 9.389185139509999445 ) ) ;
#16195 = CARTESIAN_POINT ( 'NONE',  ( 7.610717068332717439, -18.47984996834297888, -10.41172376763008245 ) ) ;
#16196 = CARTESIAN_POINT ( 'NONE',  ( 1.199500263597268246, -81.20208333333334849, 0.9218200799623752495 ) ) ;
#16197 = CARTESIAN_POINT ( 'NONE',  ( 3.350976038670510970, -79.20354908895222934, -8.646094610806894565 ) ) ;
#16198 = CARTESIAN_POINT ( 'NONE',  ( -3.201374924283697521, -80.74789697147706136, 10.74410602307857765 ) ) ;
#16199 = CARTESIAN_POINT ( 'NONE',  ( -3.085175050843000477, -78.25427313773511173, -11.57574012064000435 ) ) ;
#16200 = CARTESIAN_POINT ( 'NONE',  ( -3.300976773589475499, -81.55208334408089854, 2.347730810921812239 ) ) ;
#16201 = CARTESIAN_POINT ( 'NONE',  ( -11.84062247810999935, -76.42595468096000388, 3.366775603358000080 ) ) ;
#16202 = ADVANCED_FACE ( 'NONE', ( #36487 ), #49502, .F. ) ;
#16203 = CARTESIAN_POINT ( 'NONE',  ( -2.943945732315000008, -81.53082046129100036, 2.956303192671000168 ) ) ;
#16204 = CARTESIAN_POINT ( 'NONE',  ( 9.250000000000000000, -77.74999999999998579, 0.000000000000000000 ) ) ;
#16205 = CARTESIAN_POINT ( 'NONE',  ( 10.31986335556999990, -61.08918510704999960, -7.753844818055000587 ) ) ;
#16206 = CARTESIAN_POINT ( 'NONE',  ( 12.16303714866999997, -79.20820515958999408, 1.568404430622000190 ) ) ;
#16207 = DIRECTION ( 'NONE',  ( -1.000000000000000000, 0.000000000000000000, 0.000000000000000000 ) ) ;
#16208 = CARTESIAN_POINT ( 'NONE',  ( -7.342356150419245608, -59.98964892062633680, -8.190836719257406529 ) ) ;
#16209 = CARTESIAN_POINT ( 'NONE',  ( 12.00000000000000888, -78.03958333333333997, -1.570796326794872577 ) ) ;
#16210 = ORIENTED_EDGE ( 'NONE', *, *, #38865, .F. ) ;
#16211 = CARTESIAN_POINT ( 'NONE',  ( -0.3722592371509435560, -81.14469282965922048, 1.465311301645253916 ) ) ;
#16212 = CARTESIAN_POINT ( 'NONE',  ( 2.554064167922000195, -77.37387362948199154, 9.027803880580000495 ) ) ;
#16213 = CYLINDRICAL_SURFACE ( 'NONE', #27631, 0.5000000000000004441 ) ;
#16214 = CARTESIAN_POINT ( 'NONE',  ( 11.99999999999999822, -78.65670863885249275, 1.011638905658234666 ) ) ;
#16215 = CARTESIAN_POINT ( 'NONE',  ( 3.553889031728000081, -2.214840391789000051, -0.1653587369246999894 ) ) ;
#16216 = CARTESIAN_POINT ( 'NONE',  ( 3.985687926398000069, -78.28957306764699808, 11.49333817212000142 ) ) ;
#16217 = DIRECTION ( 'NONE',  ( -0.7071067811865474617, -0.7071067811865474617, 8.526560539801564177E-11 ) ) ;
#16219 = CARTESIAN_POINT ( 'NONE',  ( -4.000000000000000000, -74.80000000000001137, -0.5999999999999999778 ) ) ;
#16218 = CARTESIAN_POINT ( 'NONE',  ( 0.000000000000000000, -6.100000000000000533, 0.000000000000000000 ) ) ;
#16220 = CARTESIAN_POINT ( 'NONE',  ( -1.115197308773999918, -81.11885036431999652, -0.5833774300368999022 ) ) ;
#16221 = CARTESIAN_POINT ( 'NONE',  ( -10.22017084124837005, -79.57491545742729500, 3.338102352714737986 ) ) ;
#16222 = ORIENTED_EDGE ( 'NONE', *, *, #35956, .T. ) ;
#16223 = CARTESIAN_POINT ( 'NONE',  ( 0.1988171392200138166, -81.03513263419276313, -1.518600332402399999 ) ) ;
#16224 = CARTESIAN_POINT ( 'NONE',  ( 5.224348721355000613, -79.41921447277900370, -10.97639677120000101 ) ) ;
#16225 = CARTESIAN_POINT ( 'NONE',  ( 8.195846875379992014, -79.04247058337611520, 4.844231267137363517 ) ) ;
#16226 = CARTESIAN_POINT ( 'NONE',  ( 2.935661446561999899, -79.99999999999998579, -9.035036904803998681 ) ) ;
#16227 = CARTESIAN_POINT ( 'NONE',  ( -0.3862712429687000237, -82.25000000000000000, -1.188820645369000006 ) ) ;
#16228 = CIRCLE ( 'NONE', #20981, 9.549999999999998934 ) ;
#16229 = CARTESIAN_POINT ( 'NONE',  ( 1.025029370886000101E-14, -0.2000000000000005107, 0.000000000000000000 ) ) ;
#16230 = CARTESIAN_POINT ( 'NONE',  ( -6.785595605124000507, -79.27092490477099318, -7.044055193142999549 ) ) ;
#16231 = CARTESIAN_POINT ( 'NONE',  ( 12.00000000000000000, -78.14999999999999147, 0.000000000000000000 ) ) ;
#16232 = CARTESIAN_POINT ( 'NONE',  ( -12.70556836343000029, -53.57227722738999631, 1.774192865971000122E-09 ) ) ;
#16233 = ORIENTED_EDGE ( 'NONE', *, *, #5924, .F. ) ;
#16234 = AXIS2_PLACEMENT_3D ( 'NONE', #20295, #37710, #46015 ) ;
#16235 = DIRECTION ( 'NONE',  ( 0.000000000000000000, -1.000000000000000000, 0.000000000000000000 ) ) ;
#16236 = CARTESIAN_POINT ( 'NONE',  ( 11.17338741157130322, -79.27293521690316425, -3.903988906372769296 ) ) ;
#16237 = CARTESIAN_POINT ( 'NONE',  ( -3.406490280106461377, -78.62148120184446043, -0.06421861612271693998 ) ) ;
#16238 = EDGE_CURVE ( 'NONE', #41814, #23790, #48856, .T. ) ;
#16239 = CARTESIAN_POINT ( 'NONE',  ( -0.4457402708948181580, -81.50411655302407610, 1.168277140437457895 ) ) ;
#16240 = CARTESIAN_POINT ( 'NONE',  ( -0.8981901762082999952, -79.90929374366000104, -1.403037214508999986 ) ) ;
#16241 = VERTEX_POINT ( 'NONE', #55671 ) ;
#16242 = EDGE_CURVE ( 'NONE', #52133, #9420, #1372, .T. ) ;
#16243 = CARTESIAN_POINT ( 'NONE',  ( 1.073551389641718368, -78.44507409264528519, 0.6868635585880937811 ) ) ;
#16244 = CARTESIAN_POINT ( 'NONE',  ( 10.18496935386000146, -58.55064714674999493, -7.710095619709000481 ) ) ;
#16245 = CARTESIAN_POINT ( 'NONE',  ( 3.325701842495000005, -82.39999999999999147, -0.7068997487804000723 ) ) ;
#16246 = AXIS2_PLACEMENT_3D ( 'NONE', #2600, #20597, #11458 ) ;
#16247 = CARTESIAN_POINT ( 'NONE',  ( 1.532229594833856012, -17.87701036868171300, -12.51228690880882688 ) ) ;
#16248 = DIRECTION ( 'NONE',  ( 0.000000000000000000, -1.000000000000000000, 0.000000000000000000 ) ) ;
#16249 = DIRECTION ( 'NONE',  ( -1.000000000000000000, 0.000000000000000000, 0.000000000000000000 ) ) ;
#16250 = VERTEX_POINT ( 'NONE', #33512 ) ;
#16251 = EDGE_CURVE ( 'NONE', #9948, #37958, #47457, .T. ) ;
#16252 = ORIENTED_EDGE ( 'NONE', *, *, #49181, .F. ) ;
#16253 = CARTESIAN_POINT ( 'NONE',  ( -12.46551533733999939, -76.25659160047199236, 0.3559871039980000429 ) ) ;
#16254 = CARTESIAN_POINT ( 'NONE',  ( 5.898677060894324420, -78.77139060450180352, -8.987420904564112689 ) ) ;
#16255 = CARTESIAN_POINT ( 'NONE',  ( -1.277911487367000110, -78.60727590003000387, 0.6223777146390999659 ) ) ;
#16256 = ORIENTED_EDGE ( 'NONE', *, *, #47997, .T. ) ;
#16257 = CARTESIAN_POINT ( 'NONE',  ( 7.974020021247000933, -17.36898233693000293, 9.929669236791999865 ) ) ;
#16258 = CARTESIAN_POINT ( 'NONE',  ( -10.71369944335148361, -77.67916666666667425, 2.879226727952040044 ) ) ;
#16259 = CARTESIAN_POINT ( 'NONE',  ( 1.980584515752000119, -55.53514853344000102, 12.76303204600000107 ) ) ;
#16260 = CARTESIAN_POINT ( 'NONE',  ( 9.135190432272999317, -76.77363952651001000, -8.185884657762999339 ) ) ;
#16261 = CARTESIAN_POINT ( 'NONE',  ( -10.75037226435630267, -79.61044805530501378, -1.407100289909882118 ) ) ;
#16262 = CARTESIAN_POINT ( 'NONE',  ( -11.79999999999999893, -18.84999999999000053, 0.5999999999999999778 ) ) ;
#16263 = CARTESIAN_POINT ( 'NONE',  ( 3.106054555984939736, -86.09999999999998010, -1.382904586457970986 ) ) ;
#16264 = CARTESIAN_POINT ( 'NONE',  ( -8.982117338527000783, -79.78278813827100180, 6.718606902359000266 ) ) ;
#16265 = CARTESIAN_POINT ( 'NONE',  ( 3.537828989635279697, -79.94386011961954353, 8.546646707163249701 ) ) ;
#16266 = EDGE_LOOP ( 'NONE', ( #47534, #17040, #48354, #11, #7765 ) ) ;
#16267 = CARTESIAN_POINT ( 'NONE',  ( 7.644092900757153863, -55.27619833568790142, -10.09634159697595912 ) ) ;
#16268 = ORIENTED_EDGE ( 'NONE', *, *, #42939, .T. ) ;
#16269 = CARTESIAN_POINT ( 'NONE',  ( 9.550909342165001092, -79.32632342844499362, -5.975706243058000133 ) ) ;
#16270 = CARTESIAN_POINT ( 'NONE',  ( 7.485279715301945913, -77.30010352984844246, -5.434349560424259096 ) ) ;
#16271 = CARTESIAN_POINT ( 'NONE',  ( -1.172662378873000177, -80.27981897213200568, -0.6045068694098000295 ) ) ;
#16272 = LINE ( 'NONE', #15975, #8805 ) ;
#16273 = AXIS2_PLACEMENT_3D ( 'NONE', #29263, #30128, #25425 ) ;
#16274 = CARTESIAN_POINT ( 'NONE',  ( -9.524907056233788083, -77.30562916945632423, 5.924335788417241844 ) ) ;
#16275 = CARTESIAN_POINT ( 'NONE',  ( -1.411465571349000081, -79.11014632351999865, -0.1328074485833999896 ) ) ;
#16276 = DIRECTION ( 'NONE',  ( -1.000000000000000000, 0.000000000000000000, 0.000000000000000000 ) ) ;
#16277 = CARTESIAN_POINT ( 'NONE',  ( 1.407171709420391936, -80.86458333333331439, 10.75000000000000178 ) ) ;
#16278 = CARTESIAN_POINT ( 'NONE',  ( 0.3877229342594999961, -77.97375042942999812, -1.580612325761999948 ) ) ;
#16279 = CARTESIAN_POINT ( 'NONE',  ( -12.49306764015999960, -18.71943464842000182, -1.667917367065999912 ) ) ;
#16280 = DIRECTION ( 'NONE',  ( 0.000000000000000000, 1.000000000000000000, 0.000000000000000000 ) ) ;
#16281 = CARTESIAN_POINT ( 'NONE',  ( -6.966543547089000477, -79.56377255320299469, -8.575847751312000611 ) ) ;
#16282 = CARTESIAN_POINT ( 'NONE',  ( 10.75000000000000000, -79.35000000000000853, 0.000000000000000000 ) ) ;
#16283 = DIRECTION ( 'NONE',  ( -1.000000000000000000, 0.000000000000000000, 0.000000000000000000 ) ) ;
#16284 = AXIS2_PLACEMENT_3D ( 'NONE', #54573, #4968, #31818 ) ;
#16285 = B_SPLINE_CURVE_WITH_KNOTS ( 'NONE', 3,
 ( #12173, #34015, #42898, #20461, #7163, #2744 ),
 .UNSPECIFIED., .F., .F.,
 ( 4, 1, 1, 4 ),
 ( 0.000000000000000000, 0.3333333333333000081, 0.6666666666667000474, 1.000000000000000000 ),
 .UNSPECIFIED. ) ;
#16286 = CARTESIAN_POINT ( 'NONE',  ( -7.710095619827000313, -58.55064714318000085, -10.18496935397999970 ) ) ;
#16287 = DIRECTION ( 'NONE',  ( 0.000000000000000000, 1.000000000000000000, 0.000000000000000000 ) ) ;
#16288 = ORIENTED_EDGE ( 'NONE', *, *, #39828, .F. ) ;
#16289 = CARTESIAN_POINT ( 'NONE',  ( -0.7740797122817000275, -83.24257374592500014, 1.516913212488000040 ) ) ;
#16290 = CARTESIAN_POINT ( 'NONE',  ( -0.5437916395094000155, -79.48880658815998856, -1.373128015768000143 ) ) ;
#16291 = CARTESIAN_POINT ( 'NONE',  ( 10.12290050126000196, -60.04999999958999979, 7.648026767103999646 ) ) ;
#16292 = CARTESIAN_POINT ( 'NONE',  ( 11.20799393363000007, -77.84482669931600185, 4.230477091134000389 ) ) ;
#16293 = DIRECTION ( 'NONE',  ( 0.000000000000000000, 0.7071067811866525998, -0.7071067811864425456 ) ) ;
#16294 = EDGE_CURVE ( 'NONE', #51331, #3286, #160, .T. ) ;
#16295 = AXIS2_PLACEMENT_3D ( 'NONE', #15640, #42514, #33919 ) ;
#16296 = CARTESIAN_POINT ( 'NONE',  ( -0.3807657621149953542, -79.14953454632663465, 1.216325176385994355 ) ) ;
#16297 = CARTESIAN_POINT ( 'NONE',  ( 0.1434218413062385844, -2.378208186945148572, -3.516600075276243409 ) ) ;
#16298 = CARTESIAN_POINT ( 'NONE',  ( 4.598371993787000456, -78.79425194988499470, -8.567308531191999421 ) ) ;
#16299 = CARTESIAN_POINT ( 'NONE',  ( -10.62516247904072486, -76.58790361868092589, 1.636441214579218650 ) ) ;
#16300 = CARTESIAN_POINT ( 'NONE',  ( -0.9257816722924000485, -78.40834718399401027, 10.87742130684000053 ) ) ;
#16301 = CARTESIAN_POINT ( 'NONE',  ( 8.343860018000999190, -59.94999999967000548, 8.343860018000999190 ) ) ;
#16302 = CARTESIAN_POINT ( 'NONE',  ( -0.6696908800640647419, -81.06881859837598370, 1.084700732491975517 ) ) ;
#16303 = EDGE_LOOP ( 'NONE', ( #12043, #56744, #56261, #45968 ) ) ;
#16304 = VECTOR ( 'NONE', #5892, 1000.000000000000000 ) ;
#16305 = CARTESIAN_POINT ( 'NONE',  ( -8.082524092276901939, -78.95833333333332860, 4.658475568430788805 ) ) ;
#16306 = CARTESIAN_POINT ( 'NONE',  ( 1.582498447116000184, -60.95086122444999432, -12.55493832976000057 ) ) ;
#16307 = CARTESIAN_POINT ( 'NONE',  ( -2.398287624620491609, -78.67389998729009903, -3.977573462190680420 ) ) ;
#16308 = CARTESIAN_POINT ( 'NONE',  ( -9.871730464199000465, -79.83385192141699349, 4.797141237513000256 ) ) ;
#16309 = CARTESIAN_POINT ( 'NONE',  ( 0.000000000000000000, -74.64999999999999147, 0.000000000000000000 ) ) ;
#16310 = CARTESIAN_POINT ( 'NONE',  ( 3.541116439658829496, -85.32916667799834443, -1.969010436737064662 ) ) ;
#16311 = CARTESIAN_POINT ( 'NONE',  ( 11.37390407689999883, -76.35523235640999928, 4.280169657041000164 ) ) ;
#16312 = CARTESIAN_POINT ( 'NONE',  ( 11.53783733622431917, -78.46305301807434773, 2.299832388111439307 ) ) ;
#16313 = CARTESIAN_POINT ( 'NONE',  ( -8.532660243106189313, -61.92798380497763588, 9.433531203738310111 ) ) ;
#16314 = EDGE_LOOP ( 'NONE', ( #40350, #54490, #22645, #42104 ) ) ;
#16315 = CARTESIAN_POINT ( 'NONE',  ( -8.329953570067999635, -79.76670276584599151, -7.407190701775999919 ) ) ;
#16316 = CARTESIAN_POINT ( 'NONE',  ( 12.56594317982999875, -55.55000000504000468, -1.750000000000000000 ) ) ;
#16317 = CARTESIAN_POINT ( 'NONE',  ( 0.000000000000000000, -75.19999999999998863, -4.100000000000000533 ) ) ;
#16318 = CARTESIAN_POINT ( 'NONE',  ( 2.592785862636999727, -78.38672486022498731, -10.85214546196000107 ) ) ;
#16319 = ADVANCED_FACE ( 'NONE', ( #51187 ), #803, .F. ) ;
#16320 = FACE_OUTER_BOUND ( 'NONE', #4806, .T. ) ;
#16321 = FACE_OUTER_BOUND ( 'NONE', #33374, .T. ) ;
#16322 = LINE ( 'NONE', #16605, #33112 ) ;
#16323 = AXIS2_PLACEMENT_3D ( 'NONE', #46291, #6404, #1417 ) ;
#16324 = CARTESIAN_POINT ( 'NONE',  ( 1.189282163301631279, -82.15500157885483645, 0.9888244770500705938 ) ) ;
#16325 = B_SPLINE_SURFACE_WITH_KNOTS ( 'NONE', 3, 3, ( 
 ( #15858, #33844, #51882, #56591 ),
 ( #11438, #29418, #34127, #13443 ),
 ( #48606, #25861, #17295, #53608 ),
 ( #8153, #21437, #31443, #17893 ),
 ( #9033, #53313, #44453, #12856 ),
 ( #30574, #17012, #13147, #48895 ),
 ( #43890, #48322, #31141, #26152 ),
 ( #49180, #3436, #49484, #12577 ),
 ( #44172, #58329, #3720, #39446 ),
 ( #27020, #21723, #7862, #39728 ),
 ( #35882, #21145, #53912, #8732 ) ),
 .UNSPECIFIED., .F., .F., .F.,
 ( 4, 1, 1, 1, 1, 1, 1, 1, 4 ),
 ( 4, 4 ),
 ( -0.02001211456244999728, 0.000000000000000000, 0.1666666666667000196, 0.3333333333333000081, 0.5000000000000000000, 0.6666666666667000474, 0.8333333333333000637, 1.000000000000000000, 1.020273719995999917 ),
 ( -0.3582002740325999635, 1.358863140973999961 ),
 .UNSPECIFIED. ) ;
#16326 = CARTESIAN_POINT ( 'NONE',  ( 0.02451244981669795098, -79.72693319877517126, -1.249557414888817997 ) ) ;
#16327 = DIRECTION ( 'NONE',  ( 0.000000000000000000, -1.000000000000000000, 0.000000000000000000 ) ) ;
#16328 = CIRCLE ( 'NONE', #23856, 0.2000000000000005107 ) ;
#16329 =( NAMED_UNIT ( * ) SI_UNIT ( $, .STERADIAN. ) SOLID_ANGLE_UNIT ( ) );
#16330 = CARTESIAN_POINT ( 'NONE',  ( 11.74999999999999289, -76.06041666666665435, 1.538071403320028452 ) ) ;
#16331 = ORIENTED_EDGE ( 'NONE', *, *, #24179, .F. ) ;
#16332 = EDGE_CURVE ( 'NONE', #13233, #23510, #12896, .T. ) ;
#16333 = ORIENTED_EDGE ( 'NONE', *, *, #33569, .T. ) ;
#16334 = CARTESIAN_POINT ( 'NONE',  ( -12.46083735077000121, -55.11664398755999628, -1.628985986890000071 ) ) ;
#16335 = ORIENTED_EDGE ( 'NONE', *, *, #25379, .T. ) ;
#16336 = VERTEX_POINT ( 'NONE', #32847 ) ;
#16337 = CARTESIAN_POINT ( 'NONE',  ( -7.753620043410437646, -81.00000000000002842, -7.606346643182852141 ) ) ;
#16338 = AXIS2_PLACEMENT_3D ( 'NONE', #2655, #20366, #56095 ) ;
#16339 = CARTESIAN_POINT ( 'NONE',  ( 10.06402303786000196, -77.79174793274400201, -4.229752508564000202 ) ) ;
#16340 = CARTESIAN_POINT ( 'NONE',  ( 1.500000000000000000, -78.25000000000000000, 0.000000000000000000 ) ) ;
#16341 = AXIS2_PLACEMENT_3D ( 'NONE', #19721, #7297, #46898 ) ;
#16342 = CARTESIAN_POINT ( 'NONE',  ( -7.544159220956999867, -79.31303667140099378, -6.426939800899999611 ) ) ;
#16343 = CARTESIAN_POINT ( 'NONE',  ( 8.203824050184531202, -76.29609375003914806, -7.004042987541993170 ) ) ;
#16344 = EDGE_LOOP ( 'NONE', ( #36208, #21694, #44775, #55376 ) ) ;
#16345 = ORIENTED_EDGE ( 'NONE', *, *, #5454, .T. ) ;
#16346 = CARTESIAN_POINT ( 'NONE',  ( -3.357666854334504514, -77.50471486696052636, 8.619924559119072072 ) ) ;
#16347 = FACE_OUTER_BOUND ( 'NONE', #804, .T. ) ;
#16348 = CARTESIAN_POINT ( 'NONE',  ( 10.61050599188999932, -78.32876026662599145, -2.901234667509999809 ) ) ;
#16349 = CARTESIAN_POINT ( 'NONE',  ( -2.572125540837000290, -78.43380402242298999, -9.357076443458000270 ) ) ;
#16350 = CARTESIAN_POINT ( 'NONE',  ( 7.718346056094000041, -21.74888345808999901, 10.07719973192000040 ) ) ;
#16351 = DIRECTION ( 'NONE',  ( 0.000000000000000000, 1.000000000000000000, -1.243449787580000135E-13 ) ) ;
#16352 = CARTESIAN_POINT ( 'NONE',  ( -10.75000000000000000, -76.51041666666665719, -1.407171709420429018 ) ) ;
#16353 = CARTESIAN_POINT ( 'NONE',  ( 8.693423296916000353, -80.12538939878398025, -7.148151291522000683 ) ) ;
#16354 = CARTESIAN_POINT ( 'NONE',  ( 0.2491193812340000147, -79.34422942033999959, -1.565693046525999943 ) ) ;
#16355 = FACE_OUTER_BOUND ( 'NONE', #6340, .T. ) ;
#16356 = CARTESIAN_POINT ( 'NONE',  ( -7.956418361354000268, -54.27110680110000374, 9.787952249823998585 ) ) ;
#16357 = CARTESIAN_POINT ( 'NONE',  ( 6.607804308078000233, -79.12991332859898819, -6.725089593472000082 ) ) ;
#16358 = CARTESIAN_POINT ( 'NONE',  ( -3.085175050843000477, -78.30595559095398528, -11.57574012064000080 ) ) ;
#16359 = CARTESIAN_POINT ( 'NONE',  ( -9.650965486090999690, -17.06598967526999999, -8.252456812006998987 ) ) ;
#16360 = EDGE_CURVE ( 'NONE', #56978, #20349, #52349, .T. ) ;
#16362 = CARTESIAN_POINT ( 'NONE',  ( 0.9113424693944999211, -17.17464206440000041, -12.54674099557999867 ) ) ;
#16361 = CARTESIAN_POINT ( 'NONE',  ( -7.397096502814789254, -78.54793235670427975, 5.684705351741184742 ) ) ;
#16363 = CARTESIAN_POINT ( 'NONE',  ( 5.642647961229684483, -79.42304073986576896, 7.355092408208053989 ) ) ;
#16364 = CARTESIAN_POINT ( 'NONE',  ( -10.21813353151999948, -76.78887615466000227, 4.735332084273999875 ) ) ;
#16365 = CARTESIAN_POINT ( 'NONE',  ( 0.1739064196789271433, -3.499999999999999556, 3.294261630741291746 ) ) ;
#16366 = CARTESIAN_POINT ( 'NONE',  ( 3.493916750265503524, -1.488669189522607184, -0.5022341488964027212 ) ) ;
#16367 = EDGE_CURVE ( 'NONE', #38753, #14405, #53063, .T. ) ;
#16368 = ORIENTED_EDGE ( 'NONE', *, *, #5835, .F. ) ;
#16369 = DIRECTION ( 'NONE',  ( 1.000000000000000000, 0.000000000000000000, 0.000000000000000000 ) ) ;
#16370 = DIRECTION ( 'NONE',  ( 1.000000000000000000, 0.000000000000000000, 0.000000000000000000 ) ) ;
#16371 = CARTESIAN_POINT ( 'NONE',  ( 0.7572423792512895657, -78.42344112683323942, 0.9945924809264382604 ) ) ;
#16372 = CARTESIAN_POINT ( 'NONE',  ( -3.144532066837999906, -1.606752247163000025, 1.008949614594999877 ) ) ;
#16373 = CARTESIAN_POINT ( 'NONE',  ( -0.4810211636624999731, -79.27203353095599425, 9.630519408955999339 ) ) ;
#16374 = CARTESIAN_POINT ( 'NONE',  ( -12.55485633992000061, -54.64594908747999824, 1.580761757393000178 ) ) ;
#16375 = CARTESIAN_POINT ( 'NONE',  ( 1.666698456695999919, -59.99181739808000202, 12.50018138922999889 ) ) ;
#16376 = DIRECTION ( 'NONE',  ( 0.000000000000000000, 1.000000000000000000, 0.000000000000000000 ) ) ;
#16377 = AXIS2_PLACEMENT_3D ( 'NONE', #50287, #36397, #13961 ) ;
#16378 = CARTESIAN_POINT ( 'NONE',  ( 9.549999999999998934, -76.89999999999999147, 0.000000000000000000 ) ) ;
#16379 = CARTESIAN_POINT ( 'NONE',  ( 3.999999999999884537, -78.69999999999998863, -4.898587196589271820E-16 ) ) ;
#16380 = CARTESIAN_POINT ( 'NONE',  ( -9.737968063966999210, -77.76767625569698339, 5.236421613506999861 ) ) ;
#16381 = CARTESIAN_POINT ( 'NONE',  ( -2.295071999339000079, -77.60036594554799194, 10.90812747857000176 ) ) ;
#16382 = EDGE_CURVE ( 'NONE', #24385, #10331, #10849, .T. ) ;
#16383 = CARTESIAN_POINT ( 'NONE',  ( -0.2929820310045200271, -81.99426728663597430, 1.218107854444346216 ) ) ;
#16384 = CARTESIAN_POINT ( 'NONE',  ( -1.635567090190121142, -1.018497397474406929, 2.827602005665806661 ) ) ;
#16385 = CARTESIAN_POINT ( 'NONE',  ( -3.591972190522999764, -77.23543021507899198, 8.980252640667000463 ) ) ;
#16386 = CARTESIAN_POINT ( 'NONE',  ( 1.500000000000000000, -78.76041666666668561, 0.1963495408493652339 ) ) ;
#16387 = CARTESIAN_POINT ( 'NONE',  ( 0.000000000000000000, -78.79999999980499581, 0.000000000000000000 ) ) ;
#16388 = CARTESIAN_POINT ( 'NONE',  ( 6.639710140890153767, -80.27824733682197689, -8.457367011817090940 ) ) ;
#16389 = CARTESIAN_POINT ( 'NONE',  ( 10.27001848845763021, -79.87467406915122581, 3.283795101429460850 ) ) ;
#16390 = CARTESIAN_POINT ( 'NONE',  ( -10.25203062050054470, -17.87822876372841208, -7.730397977282122746 ) ) ;
#16391 = CARTESIAN_POINT ( 'NONE',  ( -10.65106809510000119, -78.95984906387799640, 5.591232889670999739 ) ) ;
#16392 = CARTESIAN_POINT ( 'NONE',  ( -8.300970689365472666, -78.75833333333335418, 4.784380313523514339 ) ) ;
#16393 = B_SPLINE_CURVE_WITH_KNOTS ( 'NONE', 3,
 ( #30713, #48750, #8293, #53458, #22159, #17745 ),
 .UNSPECIFIED., .F., .F.,
 ( 4, 2, 4 ),
 ( 0.000000000000000000, 0.5000000000000000000, 1.000000000000000000 ),
 .UNSPECIFIED. ) ;
#16394 = DIRECTION ( 'NONE',  ( 0.000000000000000000, 0.000000000000000000, -1.000000000000000000 ) ) ;
#16395 = ORIENTED_EDGE ( 'NONE', *, *, #15556, .T. ) ;
#16396 = EDGE_CURVE ( 'NONE', #24848, #1462, #38943, .T. ) ;
#16397 = CARTESIAN_POINT ( 'NONE',  ( 0.000000000000000000, -23.15000000000000213, 11.89999999977000122 ) ) ;
#16398 = ADVANCED_FACE ( 'NONE', ( #23691 ), #45567, .T. ) ;
#16399 = EDGE_LOOP ( 'NONE', ( #9946, #13165, #30601, #36834 ) ) ;
#16400 = ORIENTED_EDGE ( 'NONE', *, *, #49929, .T. ) ;
#16401 = CARTESIAN_POINT ( 'NONE',  ( -0.8506806241676722058, -1.395833333333332815, 3.165411199172021739 ) ) ;
#16402 = ORIENTED_EDGE ( 'NONE', *, *, #46126, .T. ) ;
#16403 = CIRCLE ( 'NONE', #49410, 1.749999999999997335 ) ;
#16404 = CARTESIAN_POINT ( 'NONE',  ( -0.9781931330616999709, -81.44824379153999416, 3.407067580805999807 ) ) ;
#16405 = CARTESIAN_POINT ( 'NONE',  ( 7.762291303765522343, -79.19863279546440538, 5.476889886169479915 ) ) ;
#16406 = B_SPLINE_SURFACE_WITH_KNOTS ( 'NONE', 3, 3, ( 
 ( #26701, #14008, #49463, #3984, #45325, #27288, #763, #54472, #32005, #31420, #45029, #18741, #36734, #22581, #54750, #13715, #35559, #13419, #53585, #50047, #21986, #9009, #14295, #45621, #26409, #4876, #22280, #13123, #53888, #32289, #26994, #4283, #31118, #9593, #4581, #40297, #50335, #5162, #22872, #49158, #23162, #18453, #41170, #31710, #18165, #9299, #40595, #40882, #189, #8710, #36158, #44431, #39995, #58008, #17567, #44732, #54178, #58308, #17869, #49759, #474, #36443, #42635, #10179, #42349, #50918, #6320 ),
 ( #20201, #55625, #19033, #55332, #37026, #37901, #5446, #10467, #2202, #29043, #9885, #46795, #5735, #55040, #19325, #56212, #28453, #46208, #14589, #55925, #46501, #23742, #38193, #1916, #47084, #14877, #28157, #15476, #33467, #37317, #50629, #15760, #6025, #51504, #42048, #11062, #6613, #24624, #33755, #24337, #41756, #19910, #27865, #45912, #1331, #24035, #23451, #10766, #51214, #41463, #28744, #19610, #1049, #32580, #1620, #37610, #32874, #15176, #33169, #30185, #8054, #7770, #34040, #6902, #17195, #3060, #39633 ),
 ( #38482, #48507, #3622, #16922, #38771, #26049, #29325, #12480, #47666, #16632, #24911, #7192, #52932, #48234, #44075, #47372, #25194, #7482, #21628, #16055, #56788, #47951, #2483, #30481, #29611, #16349, #43212, #25480, #57641, #52077, #34329, #43500, #20487, #51794, #2771, #52364, #34901, #25773, #56500, #11347, #43797, #39352, #39057, #21056, #34618, #57072, #3344, #52645, #11636, #11916, #57359, #42928, #20770, #29894, #12200, #21340, #17489, #690, #35476, #13047, #12764, #9516, #53507, #9224, #17791, #31636, #13933 ),
 ( #22798, #26618, #22505, #27503, #31046, #31928, #49678, #53807, #40806, #4797, #36370, #49081, #44655, #40216, #45543, #13641, #4504, #35778, #13343, #22205, #31339, #40516, #23085, #399, #39918, #18377, #54396, #18087, #5089, #49382, #49973, #8633, #44354, #53216, #41098, #4208, #35184, #48793, #8339, #36079, #58227, #8930, #26336, #54099, #26918, #27209, #44949, #45248, #3908, #21909, #37242, #32219, #1544, #19247, #50843, #54963, #10691, #28670, #18672, #50551, #28083, #14221, #55547, #41680, #46723, #14514, #50260 ) ),
 .UNSPECIFIED., .F., .F., .F.,
 ( 4, 4 ),
 ( 4, 1, 1, 1, 1, 1, 1, 1, 1, 1, 1, 1, 1, 1, 1, 1, 1, 1, 1, 1, 1, 1, 1, 1, 1, 1, 1, 1, 1, 1, 1, 1, 1, 1, 1, 1, 1, 1, 1, 1, 1, 1, 1, 1, 1, 1, 1, 1, 1, 1, 1, 1, 1, 1, 1, 1, 1, 1, 1, 1, 1, 1, 1, 1, 4 ),
 ( -0.4045438850609999748, 1.404543885061000141 ),
 ( -0.02000000000000000042, -0.003749999999999999861, 0.01250000000000000069, 0.02875000000000000125, 0.04499999999999999833, 0.06124999999999999889, 0.07749999999999999944, 0.09375000000000000000, 0.1100000000000000006, 0.1262500000000000011, 0.1424999999999999878, 0.1587500000000000022, 0.1749999999999999889, 0.1912500000000000033, 0.2074999999999999900, 0.2237500000000000044, 0.2399999999999999911, 0.2562499999999999778, 0.2725000000000000200, 0.2887500000000000067, 0.3049999999999999933, 0.3212499999999999800, 0.3375000000000000222, 0.3537500000000000089, 0.3699999999999999956, 0.3862499999999999822, 0.4025000000000000244, 0.4187500000000000111, 0.4349999999999999978, 0.4512499999999999845, 0.4675000000000000266, 0.4837500000000000133, 0.5000000000000000000, 0.5162499999999999867, 0.5324999999999999734, 0.5487499999999999600, 0.5649999999999999467, 0.5812500000000000444, 0.5975000000000000311, 0.6137500000000000178, 0.6300000000000000044, 0.6462499999999999911, 0.6624999999999999778, 0.6787499999999999645, 0.6949999999999999512, 0.7112500000000000488, 0.7275000000000000355, 0.7437500000000000222, 0.7600000000000000089, 0.7762499999999999956, 0.7924999999999999822, 0.8087499999999999689, 0.8249999999999999556, 0.8412500000000000533, 0.8575000000000000400, 0.8737500000000000266, 0.8900000000000000133, 0.9062500000000000000, 0.9224999999999999867, 0.9387499999999999734, 0.9549999999999999600, 0.9712499999999999467, 0.9875000000000000444, 1.003749999999999920, 1.020000000000000018 ),
 .UNSPECIFIED. ) ;
#16407 = ORIENTED_EDGE ( 'NONE', *, *, #28903, .T. ) ;
#16408 = CARTESIAN_POINT ( 'NONE',  ( -10.47313876284000145, -78.46108632805000127, 6.560901509735000303 ) ) ;
#16409 = CARTESIAN_POINT ( 'NONE',  ( 10.53559655518999882, -60.00569178284000316, 7.620036226177999694 ) ) ;
#16410 = EDGE_LOOP ( 'NONE', ( #18599, #38691, #2258, #28798 ) ) ;
#16411 = CARTESIAN_POINT ( 'NONE',  ( -0.08250089784128371295, -79.48042012904160458, 1.249901427480934135 ) ) ;
#16412 = CARTESIAN_POINT ( 'NONE',  ( -0.8863621734748006187, -78.67427446728444806, 1.251082152859870344 ) ) ;
#16413 = CARTESIAN_POINT ( 'NONE',  ( 9.964806208336344895, -79.79999999999999716, 6.397882358273444758 ) ) ;
#16414 = CLOSED_SHELL ( 'NONE', ( #35860, #10041, #49518, #53924, #30087, #49142, #20509, #11817, #57174, #43696, #3778, #49788, #23462, #52452, #40848, #12379, #56369, #30777, #54652, #7517, #53597, #47928, #53402, #12953, #29665, #18163, #50780, #56460, #32899, #52127, #42329, #36052, #3802, #29457, #1386, #23445, #48871, #53408, #601, #1991, #35725, #33882, #22477, #32803, #18515, #58351, #50703, #14843, #22707, #37739, #47167, #51314, #51617, #35455, #5517, #31528, #19845, #37031, #24678, #30337 ) ) ;
#16415 = CARTESIAN_POINT ( 'NONE',  ( -6.940450258154920782, -80.03122518745470870, 8.209008405819576026 ) ) ;
#16416 = DIRECTION ( 'NONE',  ( 0.000000000000000000, -1.000000000000000000, 0.000000000000000000 ) ) ;
#16417 = ADVANCED_FACE ( 'NONE', ( #6264 ), #23111, .F. ) ;
#16418 = CARTESIAN_POINT ( 'NONE',  ( 2.289901096215520404, -86.12609999968211127, -3.216015270247588820 ) ) ;
#16419 = CARTESIAN_POINT ( 'NONE',  ( 10.97835188747000146, -76.06862311939200083, -2.133021021907000048 ) ) ;
#16420 = DIRECTION ( 'NONE',  ( -1.000000000000000000, 0.000000000000000000, 0.000000000000000000 ) ) ;
#16421 = CARTESIAN_POINT ( 'NONE',  ( -9.350444020985786864, -77.33083626513527520, 2.280479404982021840 ) ) ;
#16422 = CARTESIAN_POINT ( 'NONE',  ( 8.280908091976000307, -76.08406207389899123, -7.227859519978000691 ) ) ;
#16423 = DIRECTION ( 'NONE',  ( 0.7071067811865475727, 0.000000000000000000, 0.7071067811865475727 ) ) ;
#16424 = CARTESIAN_POINT ( 'NONE',  ( -4.404426062549000598, -77.42016167140099014, 8.439952905775999881 ) ) ;
#16425 = CARTESIAN_POINT ( 'NONE',  ( -1.120379678216000041, -79.26751104489200372, -0.7232983489183999470 ) ) ;
#16426 = DIRECTION ( 'NONE',  ( -1.000000000000000000, 0.000000000000000000, 0.000000000000000000 ) ) ;
#16427 = CARTESIAN_POINT ( 'NONE',  ( 2.291577237701493353, -2.913270536965290702, 2.304101226941956515 ) ) ;
#16428 = CARTESIAN_POINT ( 'NONE',  ( -3.205004355390999926, -79.76428455456799327, 1.959415517562000053 ) ) ;
#16429 = CARTESIAN_POINT ( 'NONE',  ( -4.484732399288205329, -78.00924820851443542, 9.770240355338039251 ) ) ;
#16430 = CARTESIAN_POINT ( 'NONE',  ( 12.00000000000000000, -55.54999999966999980, 0.000000000000000000 ) ) ;
#16431 = CARTESIAN_POINT ( 'NONE',  ( -7.714303428875997959, -52.49705297113997204, 12.53545825868000385 ) ) ;
#16432 = CARTESIAN_POINT ( 'NONE',  ( -3.514866375491000117, -84.78749735065200355, -0.4589968959933000137 ) ) ;
#16433 = CARTESIAN_POINT ( 'NONE',  ( 10.38646360829000059, -22.77795407709999864, 7.655555357433999397 ) ) ;
#16434 = EDGE_CURVE ( 'NONE', #11513, #19894, #31848, .T. ) ;
#16435 = CARTESIAN_POINT ( 'NONE',  ( -7.956422463042999382, -61.32889896150999931, -9.787948076380001083 ) ) ;
#16436 = CARTESIAN_POINT ( 'NONE',  ( 9.252740428348992907, -78.17083333333334849, 2.486604901413179025 ) ) ;
#16437 = AXIS2_PLACEMENT_3D ( 'NONE', #42997, #16416, #52717 ) ;
#16438 = CARTESIAN_POINT ( 'NONE',  ( 0.3926218265389220807, -77.64583333333334281, -1.460959015002473382 ) ) ;
#16439 = CARTESIAN_POINT ( 'NONE',  ( -1.302418038466583106, -79.04516373638908533, -0.8227471584171217600 ) ) ;
#16440 = CARTESIAN_POINT ( 'NONE',  ( 6.891227191158999510, -76.72567840438999553, -9.824000600561999974 ) ) ;
#16441 = CARTESIAN_POINT ( 'NONE',  ( 12.50000000000000000, -23.24999999758999536, -1.750000000000000000 ) ) ;
#16442 = CARTESIAN_POINT ( 'NONE',  ( 1.583004792607182853, -24.45209241162641334, -12.70616254410850665 ) ) ;
#16443 = CARTESIAN_POINT ( 'NONE',  ( -11.84510048553000061, -75.96827307386000427, 4.031494313132999885 ) ) ;
#16444 = ORIENTED_EDGE ( 'NONE', *, *, #7321, .T. ) ;
#16445 = AXIS2_PLACEMENT_3D ( 'NONE', #13253, #8537, #53128 ) ;
#16446 = CARTESIAN_POINT ( 'NONE',  ( 1.328862289696999932, -80.11559030770953882, 11.18676134159000135 ) ) ;
#16447 = PLANE ( 'NONE',  #53109 ) ;
#16448 = B_SPLINE_CURVE_WITH_KNOTS ( 'NONE', 3,
 ( #35419, #53449, #21855, #56734 ),
 .UNSPECIFIED., .F., .F.,
 ( 4, 4 ),
 ( 0.000000000000000000, 1.000000000000000000 ),
 .UNSPECIFIED. ) ;
#16449 = CARTESIAN_POINT ( 'NONE',  ( -10.98449626305583138, -18.69382183571932643, -0.5845794248139971616 ) ) ;
#16450 = CARTESIAN_POINT ( 'NONE',  ( -11.13365145556000080, -79.12931983984000794, 5.979534326088000284 ) ) ;
#16451 = CARTESIAN_POINT ( 'NONE',  ( 12.61117324687999997, -55.58448536084999603, -1.798979683803999974 ) ) ;
#16452 = CARTESIAN_POINT ( 'NONE',  ( 9.440269692223999698, -78.12720491051898364, -1.906441214165000009 ) ) ;
#16453 = CARTESIAN_POINT ( 'NONE',  ( -3.413555124258999651, -86.07258307901300043, 2.398694242656000064 ) ) ;
#16454 = CARTESIAN_POINT ( 'NONE',  ( 2.194504958346340739, -79.95907396938338252, 10.52387239888080828 ) ) ;
#16455 = CARTESIAN_POINT ( 'NONE',  ( 1.416781233620999947, -79.78175585522699009, 0.7745610770380000343 ) ) ;
#16456 = ORIENTED_EDGE ( 'NONE', *, *, #42515, .F. ) ;
#16457 = CARTESIAN_POINT ( 'NONE',  ( 8.660139315840918783, -77.29964975416137918, -6.376535095569426659 ) ) ;
#16458 = CARTESIAN_POINT ( 'NONE',  ( 7.986185577601829344, -78.89281710089944966, 4.706103088835384973 ) ) ;
#16459 = CARTESIAN_POINT ( 'NONE',  ( -3.399999999999725020, -78.69999999999998863, -1.426627331148077631E-14 ) ) ;
#16460 = VERTEX_POINT ( 'NONE', #41414 ) ;
#16461 = CARTESIAN_POINT ( 'NONE',  ( 10.94849663375999960, -79.54620241998199504, -1.486040076422999956 ) ) ;
#16462 = CARTESIAN_POINT ( 'NONE',  ( -10.48771805367000098, -58.55560171494000343, 7.686918321054999836 ) ) ;
#16463 = CARTESIAN_POINT ( 'NONE',  ( -8.715923958271998728, -80.31661853915498739, 7.063164134645999681 ) ) ;
#16464 = EDGE_LOOP ( 'NONE', ( #34381, #42544, #52350, #42751 ) ) ;
#16465 = CARTESIAN_POINT ( 'NONE',  ( 1.644133925033999910, -79.05503006069899641, 11.70364056775000172 ) ) ;
#16466 = ADVANCED_FACE ( 'NONE', ( #997 ), #36975, .T. ) ;
#16467 = ORIENTED_EDGE ( 'NONE', *, *, #3026, .T. ) ;
#16468 = ORIENTED_EDGE ( 'NONE', *, *, #47801, .T. ) ;
#16469 = CARTESIAN_POINT ( 'NONE',  ( -0.5354806933557879622, -80.51039173408095451, 1.129579107287216777 ) ) ;
#16470 = B_SPLINE_CURVE_WITH_KNOTS ( 'NONE', 3,
 ( #19570, #28410, #36695, #5692, #50294, #18993, #15435, #45873, #54999, #14548, #32540, #46457, #50586, #10141, #46167, #23702, #37570, #55585, #33131, #10727, #51173, #12447, #38446, #57322 ),
 .UNSPECIFIED., .F., .F.,
 ( 4, 2, 2, 2, 2, 2, 2, 2, 2, 2, 2, 4 ),
 ( 0.000000000000000000, 0.1249999999999980294, 0.2499999999999960587, 0.3749999999999941158, 0.4374999999999937272, 0.4999999999999933387, 0.6249999999999925615, 0.7499999999999917843, 0.8124999999999926725, 0.8437499999999944489, 0.8749999999999963363, 1.000000000000000000 ),
 .UNSPECIFIED. ) ;
#16471 = CARTESIAN_POINT ( 'NONE',  ( 11.79999999999999893, -18.84999999999000053, -0.5999999999999999778 ) ) ;
#16472 = CARTESIAN_POINT ( 'NONE',  ( -5.726462542197000793, -80.20530730017200938, -7.912542777261000637 ) ) ;
#16473 = AXIS2_PLACEMENT_3D ( 'NONE', #36890, #51368, #10924 ) ;
#16474 = ORIENTED_EDGE ( 'NONE', *, *, #13710, .T. ) ;
#16475 = CARTESIAN_POINT ( 'NONE',  ( -3.250000000000000000, -2.600000000000000089, 0.000000000000000000 ) ) ;
#16476 = VERTEX_POINT ( 'NONE', #34566 ) ;
#16477 = CARTESIAN_POINT ( 'NONE',  ( -10.39285214024000048, -78.50546566091685463, 6.510605926401999533 ) ) ;
#16478 = CONICAL_SURFACE ( 'NONE', #20319, 2.949999999500999781, 0.7853981633972997312 ) ;
#16479 = CARTESIAN_POINT ( 'NONE',  ( 3.399999999999690381, -78.72609999968184979, -1.260385025514398905E-15 ) ) ;
#16480 = CARTESIAN_POINT ( 'NONE',  ( 7.619389775666999931, -55.39213701549999769, 10.35398629634000045 ) ) ;
#16481 = EDGE_CURVE ( 'NONE', #18065, #42621, #25143, .T. ) ;
#16482 = CARTESIAN_POINT ( 'NONE',  ( 7.792421629684946005, -17.70899070367055472, -10.18245656324600290 ) ) ;
#16483 = DIRECTION ( 'NONE',  ( -0.7071067811865475727, 0.000000000000000000, 0.7071067811865475727 ) ) ;
#16484 = CARTESIAN_POINT ( 'NONE',  ( -3.340139707862435969, -78.45202913613843521, 9.133287453676040002 ) ) ;
#16485 = AXIS2_PLACEMENT_3D ( 'NONE', #35537, #31987, #5146 ) ;
#16486 = CARTESIAN_POINT ( 'NONE',  ( 12.71466317168506066, -60.93795986706761170, -1.778778223978346285 ) ) ;
#16487 = CARTESIAN_POINT ( 'NONE',  ( -0.3707198704570134340, -77.95484660748586236, -1.462871543653826656 ) ) ;
#16488 = CARTESIAN_POINT ( 'NONE',  ( 9.250000000000000000, -78.84999999999999432, 1.340711541092999922E-14 ) ) ;
#16489 = CARTESIAN_POINT ( 'NONE',  ( 3.007117222848000093, -75.80336186172000623, 11.93703523519999976 ) ) ;
#16490 = LINE ( 'NONE', #25050, #45993 ) ;
#16491 = CARTESIAN_POINT ( 'NONE',  ( 9.009247259181915268, -77.77083333333335702, 2.421167930323361972 ) ) ;
#16492 = CARTESIAN_POINT ( 'NONE',  ( 10.13694968399000018, -60.50834319308000175, -7.646073915548999622 ) ) ;
#16493 = CARTESIAN_POINT ( 'NONE',  ( 9.889431646000000242, -78.78302033703000973, 7.252463523969000292 ) ) ;
#16494 = DIRECTION ( 'NONE',  ( 0.000000000000000000, -1.000000000000000000, 0.000000000000000000 ) ) ;
#16495 = CARTESIAN_POINT ( 'NONE',  ( -7.429974109835268514, -60.31614597266563749, -8.111636311568133806 ) ) ;
#16496 = ADVANCED_FACE ( 'NONE', ( #57019 ), #21290, .F. ) ;
#16497 = CARTESIAN_POINT ( 'NONE',  ( -26.50000000000000000, -39.30476017083000073, -1.122808443442999720E-13 ) ) ;
#16498 = CARTESIAN_POINT ( 'NONE',  ( 0.5212184487221598328, -80.59812269889569336, 1.458433989672604625 ) ) ;
#16499 = CARTESIAN_POINT ( 'NONE',  ( 1.092232985442820992, -79.29166666666664298, 0.6295237254636267821 ) ) ;
#16500 = CARTESIAN_POINT ( 'NONE',  ( 1.247385801072999900, -24.47722256257999973, 12.50301438876999960 ) ) ;
#16501 = CARTESIAN_POINT ( 'NONE',  ( 2.977898218353999926, -3.172466653419999894, -1.946686942756000072 ) ) ;
#16502 = CARTESIAN_POINT ( 'NONE',  ( -9.840265838668001308, -77.99115059798600669, -7.152041583326999685 ) ) ;
#16503 = CARTESIAN_POINT ( 'NONE',  ( -8.623695280723000067, -78.23234702511798844, 4.526762133323999571 ) ) ;
#16504 = EDGE_CURVE ( 'NONE', #31705, #57022, #39297, .T. ) ;
#16506 = CARTESIAN_POINT ( 'NONE',  ( 10.75000000000000000, -80.34999999999999432, 0.000000000000000000 ) ) ;
#16505 = CARTESIAN_POINT ( 'NONE',  ( -2.787965030838566616, -75.80000000000003979, 11.63553696988441466 ) ) ;
#16507 = CARTESIAN_POINT ( 'NONE',  ( -1.438065998794000100, -83.22447248197899228, -0.3363867981957999742 ) ) ;
#16508 = CARTESIAN_POINT ( 'NONE',  ( -10.71852045160081168, -79.59351931985985118, 0.8923418771536563154 ) ) ;
#16509 = EDGE_LOOP ( 'NONE', ( #7957, #31040, #48631, #41663, #47499, #29517 ) ) ;
#16510 = CARTESIAN_POINT ( 'NONE',  ( -11.85739648576925553, -78.88587530551917837, 2.129864859879341932 ) ) ;
#16511 = CARTESIAN_POINT ( 'NONE',  ( -2.849897923499999930, -79.08515109989099301, 11.69915687793999837 ) ) ;
#16512 = EDGE_CURVE ( 'NONE', #35685, #42541, #57308, .T. ) ;
#16513 = CARTESIAN_POINT ( 'NONE',  ( -7.586433418133593065, -79.30182515582218628, -5.779326228052479308 ) ) ;
#16514 = CARTESIAN_POINT ( 'NONE',  ( -5.793906668835271390, -79.99999999999998579, -7.373316236663074008 ) ) ;
#16515 = CARTESIAN_POINT ( 'NONE',  ( -7.974014308154000474, -61.43100890296999950, 9.929675091768999096 ) ) ;
#16516 = AXIS2_PLACEMENT_3D ( 'NONE', #32207, #15388, #9799 ) ;
#16517 = DIRECTION ( 'NONE',  ( 0.000000000000000000, 1.000000000000000000, 0.000000000000000000 ) ) ;
#16518 = CARTESIAN_POINT ( 'NONE',  ( -9.294849547870001061, -79.68174914560898969, 3.044469259936000149 ) ) ;
#16519 = CARTESIAN_POINT ( 'NONE',  ( -1.417334032777999964, -79.42654225787899236, -0.4910847579886000736 ) ) ;
#16520 = CARTESIAN_POINT ( 'NONE',  ( 8.796335266379994522, -78.79791666666666572, -6.760013919724047859 ) ) ;
#16521 = ORIENTED_EDGE ( 'NONE', *, *, #890, .F. ) ;
#16522 = CARTESIAN_POINT ( 'NONE',  ( -12.70259395223330756, -54.06112126474956625, 1.314575638834851512 ) ) ;
#16523 = CONICAL_SURFACE ( 'NONE', #51431, 9.400000000000000355, 0.7853981633972997312 ) ;
#16524 = CARTESIAN_POINT ( 'NONE',  ( 5.633582509268093119, -78.88484845060878570, 10.33564305875573730 ) ) ;
#16525 = CARTESIAN_POINT ( 'NONE',  ( -12.65375411747000101, -58.54977139013999476, 1.750000000000000000 ) ) ;
#16527 = CARTESIAN_POINT ( 'NONE',  ( 3.548349909811000291, -78.43735717367049176, 0.000000000000000000 ) ) ;
#16526 = CIRCLE ( 'NONE', #11810, 14.00000000000000000 ) ;
#16528 = CARTESIAN_POINT ( 'NONE',  ( -0.8906226101088000613, -79.40402002277998861, -1.206976125017999779 ) ) ;
#16529 = VERTEX_POINT ( 'NONE', #47900 ) ;
#16530 = CARTESIAN_POINT ( 'NONE',  ( -1.244347653747824634, -78.66769483858584522, -0.2779331296326563172 ) ) ;
#16531 = CARTESIAN_POINT ( 'NONE',  ( 2.858407197969000002, -77.00000000000000000, 8.797272775729998884 ) ) ;
#16532 = CARTESIAN_POINT ( 'NONE',  ( -11.59999999999999964, -87.70000000000000284, 0.000000000000000000 ) ) ;
#16533 = EDGE_CURVE ( 'NONE', #37604, #44143, #24217, .T. ) ;
#16534 = CARTESIAN_POINT ( 'NONE',  ( 0.7035754441837855921, -78.46981644582842819, 10.74957883124878499 ) ) ;
#16535 = CARTESIAN_POINT ( 'NONE',  ( 8.193575559979001000, -79.00534903806799036, 5.316613930189999948 ) ) ;
#16536 = VERTEX_POINT ( 'NONE', #12150 ) ;
#16537 = ORIENTED_EDGE ( 'NONE', *, *, #31016, .T. ) ;
#16538 = CARTESIAN_POINT ( 'NONE',  ( -9.212468050143000298, -77.26692164589900358, 8.579241990457999734 ) ) ;
#16539 = CARTESIAN_POINT ( 'NONE',  ( 4.117740896665462280, -78.75630124736080973, -9.930072027249686073 ) ) ;
#16540 = CARTESIAN_POINT ( 'NONE',  ( -1.031488621067000011, -78.08296020222998379, 0.9779790477098000423 ) ) ;
#16541 = ORIENTED_EDGE ( 'NONE', *, *, #51767, .F. ) ;
#16542 = CARTESIAN_POINT ( 'NONE',  ( 1.529609450199000076, -77.05228084965399660, 9.371081266747001592 ) ) ;
#16543 = FACE_OUTER_BOUND ( 'NONE', #25116, .T. ) ;
#16544 = CARTESIAN_POINT ( 'NONE',  ( -1.718598680027600967, -54.55037066937041601, 12.71111582765235681 ) ) ;
#16545 = CARTESIAN_POINT ( 'NONE',  ( -1.300465888139999970, -78.37242034399000090, -12.57433635189999954 ) ) ;
#16546 = DIRECTION ( 'NONE',  ( -1.000000000000000000, 0.000000000000000000, 0.000000000000000000 ) ) ;
#16547 = CARTESIAN_POINT ( 'NONE',  ( 10.75000000000000000, -78.75000000000000000, 0.000000000000000000 ) ) ;
#16548 = CARTESIAN_POINT ( 'NONE',  ( 3.922208058606298842, -86.12609999968211127, 0.4502061935811673132 ) ) ;
#16549 = CARTESIAN_POINT ( 'NONE',  ( -10.75729140709000120, -78.92454102948499894, -3.177859684493999914 ) ) ;
#16550 = CARTESIAN_POINT ( 'NONE',  ( 4.445228475228653942, -79.93551855130198192, 8.119495521249815440 ) ) ;
#16551 = ORIENTED_EDGE ( 'NONE', *, *, #22643, .T. ) ;
#16552 = CARTESIAN_POINT ( 'NONE',  ( -5.747123378374999980, -78.21567021303999923, 10.24856442990000005 ) ) ;
#16553 = ORIENTED_EDGE ( 'NONE', *, *, #45383, .F. ) ;
#16554 = CARTESIAN_POINT ( 'NONE',  ( 11.16390912141999792, -79.86007816076597976, -1.515278025736000123 ) ) ;
#16555 = CARTESIAN_POINT ( 'NONE',  ( 6.898510738327106928, -77.29199995586373007, -6.163577416694886679 ) ) ;
#16556 = CARTESIAN_POINT ( 'NONE',  ( -0.1806087918925000091, -80.68247902352800338, 1.406216040666999900 ) ) ;
#16557 = CARTESIAN_POINT ( 'NONE',  ( 0.6295237254636258939, -83.16666666666667140, -1.092232985442821658 ) ) ;
#16558 = CARTESIAN_POINT ( 'NONE',  ( 10.78724245695320505, -76.48279647566602080, 4.717496507233430947 ) ) ;
#16559 = CARTESIAN_POINT ( 'NONE',  ( 0.1641065589886999965, -77.91368429802710693, 1.507319194642999793 ) ) ;
#16560 = CARTESIAN_POINT ( 'NONE',  ( -10.75000000000000000, -78.00000000000000000, 2.252154972635999871E-14 ) ) ;
#16561 = CARTESIAN_POINT ( 'NONE',  ( 0.000000000000000000, -80.69999999999998863, 0.000000000000000000 ) ) ;
#16562 = CARTESIAN_POINT ( 'NONE',  ( -11.00000000000000000, -78.59999999999999432, 0.000000000000000000 ) ) ;
#16563 = CARTESIAN_POINT ( 'NONE',  ( -1.750000000001000089, -23.24999998674999802, 12.56594318051000059 ) ) ;
#16564 = FACE_OUTER_BOUND ( 'NONE', #54235, .T. ) ;
#16565 = CARTESIAN_POINT ( 'NONE',  ( 3.980415848809999879, -79.40290945932498801, 10.42342982551999953 ) ) ;
#16566 = ADVANCED_FACE ( 'NONE', ( #34852 ), #11159, .T. ) ;
#16567 = CARTESIAN_POINT ( 'NONE',  ( 10.01234990228999955, -23.29849137228000444, -7.653559502275999016 ) ) ;
#16568 = FILL_AREA_STYLE_COLOUR ( '', #20404 ) ;
#16569 = CARTESIAN_POINT ( 'NONE',  ( 0.000000000000000000, -90.35000000009100063, 0.000000000000000000 ) ) ;
#16570 = ORIENTED_EDGE ( 'NONE', *, *, #52416, .F. ) ;
#16571 = CARTESIAN_POINT ( 'NONE',  ( -1.495211702480000016, -81.34779729262000103, -0.3395960383748000133 ) ) ;
#16572 = CARTESIAN_POINT ( 'NONE',  ( -1.376297233339999870, -80.35198252799999352, 0.7875294559552000750 ) ) ;
#16573 = CARTESIAN_POINT ( 'NONE',  ( -8.190859204290999784, -59.94999999967000548, -7.342331066867000544 ) ) ;
#16574 = CARTESIAN_POINT ( 'NONE',  ( 9.148490208346998998, -77.87195601473999318, 7.734416031130999514 ) ) ;
#16575 = CARTESIAN_POINT ( 'NONE',  ( -1.250000000000000000, -79.50000000000000000, 0.000000000000000000 ) ) ;
#16576 = DIRECTION ( 'NONE',  ( 1.000000000000000000, 0.000000000000000000, 0.000000000000000000 ) ) ;
#16577 = DIRECTION ( 'NONE',  ( -0.9936845293270585300, 0.1122098755727947705, 0.000000000000000000 ) ) ;
#16578 = CARTESIAN_POINT ( 'NONE',  ( 2.210712544800999879, -79.27330194988499557, -9.468498208576999531 ) ) ;
#16579 = CARTESIAN_POINT ( 'NONE',  ( -7.316919381717999826, -78.58780063874398536, 6.093690752987000359 ) ) ;
#16580 = CARTESIAN_POINT ( 'NONE',  ( -10.64192559734432031, -76.58874692010783747, 1.522398744522916125 ) ) ;
#16581 = CARTESIAN_POINT ( 'NONE',  ( 10.88122807191786023, -75.98028698031052386, 4.433341873219495355 ) ) ;
#16582 = CARTESIAN_POINT ( 'NONE',  ( -1.248018900756835192, -82.16602084622610391, -0.2580508266247266147 ) ) ;
#16583 = ORIENTED_EDGE ( 'NONE', *, *, #1310, .F. ) ;
#16584 = DIRECTION ( 'NONE',  ( -1.000000000000000000, 0.000000000000000000, 0.000000000000000000 ) ) ;
#16585 = CARTESIAN_POINT ( 'NONE',  ( -7.217308068640586605, -77.12565399570821967, 9.390397901522751667 ) ) ;
#16586 = CARTESIAN_POINT ( 'NONE',  ( 1.173088849732999872, -79.19397159786899465, 12.21509120978000063 ) ) ;
#16587 = ADVANCED_FACE ( 'NONE', ( #28990 ), #42586, .F. ) ;
#16588 = CARTESIAN_POINT ( 'NONE',  ( 2.322889840689294161, -78.67389998729009903, -4.022071228304369583 ) ) ;
#16589 = CARTESIAN_POINT ( 'NONE',  ( -1.596536837631000072, -81.85265420858999619, -0.4757406268331999533 ) ) ;
#16590 = CARTESIAN_POINT ( 'NONE',  ( -2.309466437479000156, -77.72539668997998774, 10.97654204954999990 ) ) ;
#16591 = CARTESIAN_POINT ( 'NONE',  ( -10.69701368780000017, -79.86194427574999111, 1.066019776055000090 ) ) ;
#16592 = CARTESIAN_POINT ( 'NONE',  ( 10.01752098897000032, -23.19172009652000099, -7.660412494176999765 ) ) ;
#16593 = CARTESIAN_POINT ( 'NONE',  ( 1.980584515752000119, -18.73514853375999678, 12.76303204602000108 ) ) ;
#16594 = CARTESIAN_POINT ( 'NONE',  ( -2.601777299206000205, -76.33297644249898894, 12.11064771572999987 ) ) ;
#16595 = LINE ( 'NONE', #13306, #3822 ) ;
#16596 = CARTESIAN_POINT ( 'NONE',  ( -1.250000000000000000, -77.75000000000000000, 0.000000000000000000 ) ) ;
#16597 = EDGE_LOOP ( 'NONE', ( #305, #55136, #29590, #41162 ) ) ;
#16598 = CARTESIAN_POINT ( 'NONE',  ( 8.589798209762999903, -78.33715855134300909, -6.922213596449000583 ) ) ;
#16599 = CARTESIAN_POINT ( 'NONE',  ( -1.216847505586732492, -80.08203192589257924, 0.2879019704867851193 ) ) ;
#16600 = CARTESIAN_POINT ( 'NONE',  ( 10.12290050255000118, -55.55000002206000431, 7.648026768392999664 ) ) ;
#16601 = MECHANICAL_DESIGN_GEOMETRIC_PRESENTATION_REPRESENTATION (  '', ( #24135 ), #5957 ) ;
#16602 = CARTESIAN_POINT ( 'NONE',  ( -11.10294551207000069, -79.16561974942199242, 1.911422329490000127 ) ) ;
#16603 = CARTESIAN_POINT ( 'NONE',  ( -12.50000000000000000, -23.44678171330999916, -1.250000000000000000 ) ) ;
#16604 = CARTESIAN_POINT ( 'NONE',  ( 9.050966798898000931, -59.94999999040999938, 7.919595949288999570 ) ) ;
#16605 = CARTESIAN_POINT ( 'NONE',  ( -1.249999986291000065, -76.30000000051599329, 0.6999999994844999796 ) ) ;
#16606 = CARTESIAN_POINT ( 'NONE',  ( -0.5901797316841597141, -81.94244151454432767, -1.393023506703266357 ) ) ;
#16607 = EDGE_CURVE ( 'NONE', #40109, #15092, #15744, .T. ) ;
#16608 = CARTESIAN_POINT ( 'NONE',  ( -0.1504192046052299503, -79.71605312332511062, -1.243133251493206304 ) ) ;
#16609 = AXIS2_PLACEMENT_3D ( 'NONE', #30636, #43663, #21502 ) ;
#16610 = CIRCLE ( 'NONE', #46812, 10.69999999999999929 ) ;
#16611 = CARTESIAN_POINT ( 'NONE',  ( 0.000000000000000000, -75.00000000000000000, 7.200000000000000178 ) ) ;
#16612 = CARTESIAN_POINT ( 'NONE',  ( -12.70451681032499991, -61.97641660171719735, -0.5206746370656520906 ) ) ;
#16613 = SURFACE_STYLE_USAGE ( .BOTH. , #21319 ) ;
#16614 = CARTESIAN_POINT ( 'NONE',  ( 8.485281374238999419, -55.64999999967000122, 8.485281374238999419 ) ) ;
#16615 = ORIENTED_EDGE ( 'NONE', *, *, #44273, .F. ) ;
#16616 = ORIENTED_EDGE ( 'NONE', *, *, #46750, .F. ) ;
#16617 = CARTESIAN_POINT ( 'NONE',  ( -12.72394144133999916, -55.57839271467000231, -1.930881231431999856 ) ) ;
#16618 = EDGE_LOOP ( 'NONE', ( #24432, #41817, #3647 ) ) ;
#16620 = ORIENTED_EDGE ( 'NONE', *, *, #34464, .F. ) ;
#16619 = EDGE_CURVE ( 'NONE', #41582, #44945, #25289, .T. ) ;
#16621 = CARTESIAN_POINT ( 'NONE',  ( -7.247844507162001015, -55.54999999966999980, -9.722718241315000398 ) ) ;
#16622 = CARTESIAN_POINT ( 'NONE',  ( -0.8932107854388791068, -77.79557291679432751, -1.163659720379709883 ) ) ;
#16623 = CARTESIAN_POINT ( 'NONE',  ( 5.381001269034999979, -79.42917000473400435, -7.930497238065998822 ) ) ;
#16624 = CARTESIAN_POINT ( 'NONE',  ( 0.1144858057291637116, -78.22606344178616666, -9.249342975308575632 ) ) ;
#16625 = CARTESIAN_POINT ( 'NONE',  ( -11.20683111097000051, -79.70168371772200544, -0.4743912329535999728 ) ) ;
#16626 = ORIENTED_EDGE ( 'NONE', *, *, #3805, .T. ) ;
#16627 = ORIENTED_EDGE ( 'NONE', *, *, #11674, .F. ) ;
#16628 = CARTESIAN_POINT ( 'NONE',  ( -2.333868897602956238, -77.49531809838757113, 8.954045959266851540 ) ) ;
#16629 = CARTESIAN_POINT ( 'NONE',  ( -8.283402485401001769, -77.86702283146098580, -7.298588567667000149 ) ) ;
#16630 = MANIFOLD_SOLID_BREP ( 'Stock-MAS-694-1', #28656 ) ;
#16631 = CARTESIAN_POINT ( 'NONE',  ( -12.66315196852000113, -61.97802884675999735, 0.06065366946605000448 ) ) ;
#16632 = CARTESIAN_POINT ( 'NONE',  ( -7.203390125892000562, -78.88858528848699336, -6.502451851937000704 ) ) ;
#16633 = CARTESIAN_POINT ( 'NONE',  ( 7.682331425175999762, -22.76486430425999785, 10.04115011118000211 ) ) ;
#16634 = B_SPLINE_CURVE_WITH_KNOTS ( 'NONE', 3,
 ( #873, #41290, #9418, #27407, #23567, #45442 ),
 .UNSPECIFIED., .F., .F.,
 ( 4, 2, 4 ),
 ( 0.000000000000000000, 0.5000000000000000000, 1.000000000000000000 ),
 .UNSPECIFIED. ) ;
#16635 = CARTESIAN_POINT ( 'NONE',  ( 9.689272046963719021, -61.77888144132615622, 8.274769670150060819 ) ) ;
#16636 = CARTESIAN_POINT ( 'NONE',  ( -1.407171709420418138, -76.61458333333330017, -10.75000000000000000 ) ) ;
#16637 = CARTESIAN_POINT ( 'NONE',  ( -11.11771682179999843, -80.41771755615498307, 1.751409206030000165 ) ) ;
#16638 = CARTESIAN_POINT ( 'NONE',  ( -1.478021081765000133, -80.22861590553999633, 0.8457367421919999018 ) ) ;
#16639 = EDGE_CURVE ( 'NONE', #36944, #5427, #27127, .T. ) ;
#16640 = CARTESIAN_POINT ( 'NONE',  ( 0.000000000000000000, -78.69999999999998863, 0.000000000000000000 ) ) ;
#16641 = ORIENTED_EDGE ( 'NONE', *, *, #531, .T. ) ;
#16642 = ADVANCED_FACE ( 'NONE', ( #25771 ), #16781, .F. ) ;
#16643 = CARTESIAN_POINT ( 'NONE',  ( -3.189212937810000259, -76.47126873785200019, 10.79536088457000176 ) ) ;
#16644 = CARTESIAN_POINT ( 'NONE',  ( 11.20799393363000007, -77.98040380586900255, 4.230477091134000389 ) ) ;
#16645 = CARTESIAN_POINT ( 'NONE',  ( -7.948094694409999050, -17.55965255610999876, -9.636752590488001147 ) ) ;
#16646 = VECTOR ( 'NONE', #34208, 1000.000000000000000 ) ;
#16648 = CARTESIAN_POINT ( 'NONE',  ( -1.466594960159999905, -17.91841800947999985, -12.44238958332999800 ) ) ;
#16647 = CARTESIAN_POINT ( 'NONE',  ( -9.009538955111615621, -78.57917760043629585, 2.421331503275422126 ) ) ;
#16649 = CARTESIAN_POINT ( 'NONE',  ( 9.252740428349003565, -79.02916666666671119, -2.486604901413146607 ) ) ;
#16650 =( LENGTH_UNIT ( ) NAMED_UNIT ( * ) SI_UNIT ( .MILLI., .METRE. ) );
#16651 = CARTESIAN_POINT ( 'NONE',  ( 12.80090744921000123, -19.23767312576000066, 1.980532734072999901 ) ) ;
#16652 = CARTESIAN_POINT ( 'NONE',  ( -7.880862184694999328, -76.76163981165899486, 7.737503720428000165 ) ) ;
#16653 = CARTESIAN_POINT ( 'NONE',  ( 0.9372783843427989758, -3.499999999999999112, 3.216071100383696368 ) ) ;
#16654 = CARTESIAN_POINT ( 'NONE',  ( -3.408105548625404158, -0.7711048338445120054, -0.9268356498114088682 ) ) ;
#16655 = VECTOR ( 'NONE', #434, 1000.000000000000000 ) ;
#16656 = ORIENTED_EDGE ( 'NONE', *, *, #40352, .F. ) ;
#16657 = DIRECTION ( 'NONE',  ( 0.000000000000000000, 0.000000000000000000, 1.000000000000000000 ) ) ;
#16658 = CARTESIAN_POINT ( 'NONE',  ( -1.416666666666666741, -77.54999999999999716, 0.000000000000000000 ) ) ;
#16659 = CARTESIAN_POINT ( 'NONE',  ( -12.69619287811000063, -21.75083378359999742, 1.799475295154000065 ) ) ;
#16660 = EDGE_CURVE ( 'NONE', #45569, #18184, #8929, .T. ) ;
#16661 = VECTOR ( 'NONE', #10482, 1000.000000000000114 ) ;
#16662 = CARTESIAN_POINT ( 'NONE',  ( 1.121545512341999951, -2.281343295938000004, -3.469001545188000524 ) ) ;
#16663 = CARTESIAN_POINT ( 'NONE',  ( -10.93308570624999909, -78.21625547246898691, -2.507139558745000052 ) ) ;
#16664 = CARTESIAN_POINT ( 'NONE',  ( -12.77301916222999800, -53.74808379519999590, 1.052060437763999934 ) ) ;
#16665 = LINE ( 'NONE', #52963, #16740 ) ;
#16666 = CYLINDRICAL_SURFACE ( 'NONE', #56226, 3.250000000000000000 ) ;
#16667 = CARTESIAN_POINT ( 'NONE',  ( 0.000000000000000000, -80.74999999986198418, -5.249999999862000166 ) ) ;
#16668 = CARTESIAN_POINT ( 'NONE',  ( -0.7670514813460999060, -83.83321544543098014, -3.888137449123000078 ) ) ;
#16669 = CARTESIAN_POINT ( 'NONE',  ( -10.71369944335147117, -77.22083333333334565, -2.879226727952084453 ) ) ;
#16670 = DIRECTION ( 'NONE',  ( 1.000000000000000000, 0.000000000000000000, 0.000000000000000000 ) ) ;
#16671 = CARTESIAN_POINT ( 'NONE',  ( -7.278304428485000699, -77.73911654703098861, 8.323125493531998487 ) ) ;
#16672 = CARTESIAN_POINT ( 'NONE',  ( 10.62752749630825377, -76.41453037466249043, -5.012216836189437252 ) ) ;
#16673 = CARTESIAN_POINT ( 'NONE',  ( -5.715586620248999772, -77.79102034656098397, -9.570092484259999921 ) ) ;
#16674 = CARTESIAN_POINT ( 'NONE',  ( 0.3246040448838053982, -81.95449045088716389, 1.207607888008069619 ) ) ;
#16675 = CARTESIAN_POINT ( 'NONE',  ( 1.750000000001000089, -60.04999998641999781, -12.56594318054000148 ) ) ;
#16676 = CARTESIAN_POINT ( 'NONE',  ( 5.212684961665999595, -76.87984006102360013, -8.147089634514999901 ) ) ;
#16677 = CARTESIAN_POINT ( 'NONE',  ( 2.769824414688999870, -79.21914805011499539, -8.825563591736999669 ) ) ;
#16678 = CARTESIAN_POINT ( 'NONE',  ( -1.997276839918471714, -2.572916666666666519, -2.598917237794086788 ) ) ;
#16679 = CARTESIAN_POINT ( 'NONE',  ( 2.419489426094433515, -80.24335428146707727, -10.47420677764779029 ) ) ;
#16680 = CARTESIAN_POINT ( 'NONE',  ( -11.79999999999999893, -23.15000000000000213, 0.000000000000000000 ) ) ;
#16681 = CARTESIAN_POINT ( 'NONE',  ( -9.175589924978867273, -16.77304466868007538, -8.792768277111136399 ) ) ;
#16682 = CARTESIAN_POINT ( 'NONE',  ( 11.77452260639999970, -79.75674588647899554, 1.259536412044000020 ) ) ;
#16683 = CARTESIAN_POINT ( 'NONE',  ( 9.252740428348991131, -78.57083333333333997, 2.486604901413179913 ) ) ;
#16684 = CARTESIAN_POINT ( 'NONE',  ( 10.94267788024999888, -79.55441252099899430, -2.663036869319000299 ) ) ;
#16685 = CARTESIAN_POINT ( 'NONE',  ( -10.98960559191257147, -23.51693928699113911, -0.4813395862331206199 ) ) ;
#16686 = ORIENTED_EDGE ( 'NONE', *, *, #39527, .F. ) ;
#16687 = CARTESIAN_POINT ( 'NONE',  ( -1.760728164551675023, -0.7500000000000000000, 3.046994028780342312 ) ) ;
#16688 = ORIENTED_EDGE ( 'NONE', *, *, #55984, .T. ) ;
#16689 = AXIS2_PLACEMENT_3D ( 'NONE', #1918, #19912, #47375 ) ;
#16691 = EDGE_CURVE ( 'NONE', #16476, #8049, #44353, .T. ) ;
#16690 = ORIENTED_EDGE ( 'NONE', *, *, #39130, .F. ) ;
#16692 = DIRECTION ( 'NONE',  ( 0.7026410690473252618, 0.1122098755728027641, 0.7026410690473252618 ) ) ;
#16693 = ORIENTED_EDGE ( 'NONE', *, *, #25230, .T. ) ;
#16694 = CIRCLE ( 'NONE', #26072, 12.80000000000000071 ) ;
#16695 = CARTESIAN_POINT ( 'NONE',  ( 2.184286877926000070, -82.28999676290898435, -2.791777007933000210 ) ) ;
#16696 = CARTESIAN_POINT ( 'NONE',  ( -5.070101917245042777, -79.31948482625490726, 8.043791529919085193 ) ) ;
#16697 = VERTEX_POINT ( 'NONE', #39349 ) ;
#16698 = CARTESIAN_POINT ( 'NONE',  ( -7.389227917444999960, -78.34526476023999919, 9.720412100329001603 ) ) ;
#16699 = AXIS2_PLACEMENT_3D ( 'NONE', #34805, #21527, #39535 ) ;
#16700 = CARTESIAN_POINT ( 'NONE',  ( -7.654537165486999584, -60.08056535122999975, 10.01332852690999964 ) ) ;
#16701 = ORIENTED_EDGE ( 'NONE', *, *, #29008, .T. ) ;
#16702 = CARTESIAN_POINT ( 'NONE',  ( -1.020136227765584547, -77.81721996128494823, -1.142300944648168670 ) ) ;
#16703 = CIRCLE ( 'NONE', #28949, 9.549999999999998934 ) ;
#16704 = CARTESIAN_POINT ( 'NONE',  ( -10.99999999999999822, -18.24999999999999645, 0.1600933372533455690 ) ) ;
#16705 = CARTESIAN_POINT ( 'NONE',  ( -10.21718853249328518, -80.07487106893638895, 3.342320372008775742 ) ) ;
#16706 = CARTESIAN_POINT ( 'NONE',  ( -10.42531124905999995, -23.26485148473999942, -7.624341765453999997 ) ) ;
#16707 = CARTESIAN_POINT ( 'NONE',  ( 0.4132205903735213237, -86.12609999968209706, -3.926276861430695320 ) ) ;
#16708 = CARTESIAN_POINT ( 'NONE',  ( -4.800187936532999800, -76.24419671331600057, 10.10109298474000106 ) ) ;
#16709 = CARTESIAN_POINT ( 'NONE',  ( 7.468771752218000159, -77.17884144764001064, -10.77882862479000003 ) ) ;
#16710 = CARTESIAN_POINT ( 'NONE',  ( 5.491641493159680643, -77.17685792801958655, 7.961916067739349678 ) ) ;
#16711 = CARTESIAN_POINT ( 'NONE',  ( 10.83817488108000227, -76.69523121474300353, -1.875052409207000004 ) ) ;
#16712 = CARTESIAN_POINT ( 'NONE',  ( -9.217496754025233940, -78.60672666432962785, -0.7743134236860684805 ) ) ;
#16713 = EDGE_CURVE ( 'NONE', #9880, #35206, #45352, .T. ) ;
#16714 = CARTESIAN_POINT ( 'NONE',  ( -0.2976639488673999967, -79.57102539098100635, 1.299989344602000108 ) ) ;
#16715 = CARTESIAN_POINT ( 'NONE',  ( -10.44884804545204382, -80.12557790367317523, -3.439072401377349486 ) ) ;
#16716 = CARTESIAN_POINT ( 'NONE',  ( 2.786504344070804606, -2.894472130040342872, 1.673888437967501641 ) ) ;
#16717 = CARTESIAN_POINT ( 'NONE',  ( -0.05196629067518999945, -79.77200264934798213, 3.544328326796999828 ) ) ;
#16718 = CARTESIAN_POINT ( 'NONE',  ( 1.233429448859959754, -82.86411798178254173, 0.2149029772794059101 ) ) ;
#16719 = CARTESIAN_POINT ( 'NONE',  ( -3.318006187736000090, -86.12136169985498668, 0.9370938149272999285 ) ) ;
#16720 = CARTESIAN_POINT ( 'NONE',  ( 3.521688171515000132, -3.548588873046000014, 0.7298424208991000084 ) ) ;
#16721 = CARTESIAN_POINT ( 'NONE',  ( 10.18491080493000212, -23.30716680861999990, 7.640030264156999706 ) ) ;
#16722 = CARTESIAN_POINT ( 'NONE',  ( -7.633478499842999199, -60.00098177563999968, -10.36292345936000103 ) ) ;
#16723 = CARTESIAN_POINT ( 'NONE',  ( -1.812920252538464227, -79.18700244415332179, 11.90997463893260644 ) ) ;
#16724 = EDGE_CURVE ( 'NONE', #41331, #31756, #16920, .T. ) ;
#16725 = CARTESIAN_POINT ( 'NONE',  ( 0.1510373474112000070, -81.54408125928999596, 1.325052402434999888 ) ) ;
#16727 = ADVANCED_FACE ( 'NONE', ( #44652 ), #29992, .T. ) ;
#16726 = FACE_OUTER_BOUND ( 'NONE', #44838, .T. ) ;
#16728 = CARTESIAN_POINT ( 'NONE',  ( -1.264141272797000060, -77.66925730074001422, -12.95149364859999963 ) ) ;
#16729 = AXIS2_PLACEMENT_3D ( 'NONE', #4597, #32301, #22594 ) ;
#16730 = CARTESIAN_POINT ( 'NONE',  ( 1.371980222863132592, -79.61275704297987943, -0.7006253647128551920 ) ) ;
#16731 = DIRECTION ( 'NONE',  ( 0.000000000000000000, -0.7071067811866525998, -0.7071067811864425456 ) ) ;
#16732 = CARTESIAN_POINT ( 'NONE',  ( -11.89104863444000060, -76.55941889705000847, 3.380364376359000111 ) ) ;
#16733 = ORIENTED_EDGE ( 'NONE', *, *, #35921, .F. ) ;
#16734 = CARTESIAN_POINT ( 'NONE',  ( -9.500000000000000000, -78.39999999999999147, 0.000000000000000000 ) ) ;
#16735 = AXIS2_PLACEMENT_3D ( 'NONE', #25173, #39614, #57619 ) ;
#16736 = CARTESIAN_POINT ( 'NONE',  ( 12.54987272481000105, -61.85113590103000547, 0.1385846084898000041 ) ) ;
#16737 = CARTESIAN_POINT ( 'NONE',  ( 10.85397020026000092, -79.29714617087998363, -4.993565566466998895 ) ) ;
#16738 = CARTESIAN_POINT ( 'NONE',  ( 7.654537085030999499, -18.71943307332999851, -10.01332844637000008 ) ) ;
#16739 = CARTESIAN_POINT ( 'NONE',  ( -8.985695946343000173, -78.93010020865598619, 3.150816496261000133 ) ) ;
#16740 = VECTOR ( 'NONE', #53245, 1000.000000000000000 ) ;
#16741 = CARTESIAN_POINT ( 'NONE',  ( 2.191142140121999926, -85.70556633873299290, 3.550913296835999766 ) ) ;
#16742 = CARTESIAN_POINT ( 'NONE',  ( -12.65372179310999989, -20.24935286375000132, 1.750000000000000000 ) ) ;
#16743 = CARTESIAN_POINT ( 'NONE',  ( 1.504745031191999871, -79.78751491957400788, -0.1862378672923999945 ) ) ;
#16744 = ORIENTED_EDGE ( 'NONE', *, *, #35296, .T. ) ;
#16745 = CARTESIAN_POINT ( 'NONE',  ( 10.34512087479159526, -77.32797947898937707, -2.955462300682764276 ) ) ;
#16746 = CARTESIAN_POINT ( 'NONE',  ( -2.879226727952095555, -78.80416666666667425, -10.71369944335146940 ) ) ;
#16747 = EDGE_CURVE ( 'NONE', #56598, #22393, #3106, .T. ) ;
#16748 = AXIS2_PLACEMENT_3D ( 'NONE', #8518, #53996, #12939 ) ;
#16749 = CARTESIAN_POINT ( 'NONE',  ( 3.621447497675000182, -78.99318692614357929, -4.434994086307880463E-16 ) ) ;
#16750 = ORIENTED_EDGE ( 'NONE', *, *, #4135, .T. ) ;
#16751 = CARTESIAN_POINT ( 'NONE',  ( 8.999546809828999017, -78.07436279057898787, -5.951127176402999375 ) ) ;
#16752 = CARTESIAN_POINT ( 'NONE',  ( -9.931052046351343421, -60.92278631065439498, -7.764003813311978419 ) ) ;
#16753 = CARTESIAN_POINT ( 'NONE',  ( -4.004180130848999930, -80.27485737381698527, 10.47959906926000073 ) ) ;
#16754 = ORIENTED_EDGE ( 'NONE', *, *, #49181, .T. ) ;
#16755 = B_SPLINE_CURVE_WITH_KNOTS ( 'NONE', 3,
 ( #31412, #13708, #52997, #48578, #49151, #57422, #22273, #31703, #183, #34966 ),
 .UNSPECIFIED., .F., .F.,
 ( 4, 2, 2, 2, 4 ),
 ( 0.000000000000000000, 0.2500000000000000000, 0.5000000000000001110, 0.7500000000000001110, 1.000000000000000000 ),
 .UNSPECIFIED. ) ;
#16756 = CARTESIAN_POINT ( 'NONE',  ( -8.196454039252000001, -78.75660759103701025, -8.832548491656998735 ) ) ;
#16757 = B_SPLINE_CURVE_WITH_KNOTS ( 'NONE', 3,
 ( #48096, #16208, #7340, #20914, #38917, #56935, #16495, #3210, #15335, #42496, #17064, #49237, #8203, #22362, #39779, #16784, #3486, #21492 ),
 .UNSPECIFIED., .F., .F.,
 ( 4, 2, 2, 2, 2, 2, 2, 2, 4 ),
 ( 0.000000000000000000, 0.06250000000000272005, 0.1250000000000054401, 0.2500000000000012768, 0.5000000000000001110, 0.7499999999999960032, 0.8124999999999945599, 0.8749999999999932276, 1.000000000000000000 ),
 .UNSPECIFIED. ) ;
#16758 = ORIENTED_EDGE ( 'NONE', *, *, #11850, .T. ) ;
#16760 = ADVANCED_FACE ( 'NONE', ( #37241 ), #5949, .F. ) ;
#16759 = ORIENTED_EDGE ( 'NONE', *, *, #11923, .F. ) ;
#16761 = DIRECTION ( 'NONE',  ( 0.000000000000000000, -1.000000000000000000, 0.000000000000000000 ) ) ;
#16762 = ADVANCED_FACE ( 'NONE', ( #54962 ), #40804, .F. ) ;
#16763 = CARTESIAN_POINT ( 'NONE',  ( -3.106054822367000146, -86.12610002267798848, 1.382903988153999952 ) ) ;
#16764 = CARTESIAN_POINT ( 'NONE',  ( 5.496668217546000434, -80.42257811839652959, -8.073860231047000013 ) ) ;
#16765 = VERTEX_POINT ( 'NONE', #32217 ) ;
#16766 = CARTESIAN_POINT ( 'NONE',  ( 3.168353074312903583, -2.372112023236606415, 0.8509228423427537269 ) ) ;
#16767 = ORIENTED_EDGE ( 'NONE', *, *, #45244, .F. ) ;
#16768 = CARTESIAN_POINT ( 'NONE',  ( 3.086017585447000222, -79.19524289474686896, -11.86910201801999953 ) ) ;
#16769 = CARTESIAN_POINT ( 'NONE',  ( -3.777881228421892335, -78.99318692756679638, 0.07122045777464609817 ) ) ;
#16770 = CARTESIAN_POINT ( 'NONE',  ( 8.227509542961000122, -53.97460508840000415, 9.516261809240999625 ) ) ;
#16771 = CARTESIAN_POINT ( 'NONE',  ( 0.7554284705563452107, -81.23333333333332007, 1.310679582531388609 ) ) ;
#16772 = CARTESIAN_POINT ( 'NONE',  ( 0.000000000000000000, -80.74999999950000529, 0.000000000000000000 ) ) ;
#16773 = CARTESIAN_POINT ( 'NONE',  ( -12.70457850620681306, -16.82128713317816349, -0.5106122238182330131 ) ) ;
#16774 = VECTOR ( 'NONE', #11537, 1000.000000000000000 ) ;
#16775 = CARTESIAN_POINT ( 'NONE',  ( -11.74098051674999965, -78.63408355366797764, 2.380218674853999961 ) ) ;
#16776 = CARTESIAN_POINT ( 'NONE',  ( 8.994028603496278862, -78.83108882679107410, -2.182395696014679309 ) ) ;
#16777 = CARTESIAN_POINT ( 'NONE',  ( -10.77133038182000035, -76.48821396288001040, -5.959359258312999508 ) ) ;
#16778 = CARTESIAN_POINT ( 'NONE',  ( -0.06120470443819999579, -79.77200264934798213, 4.174428554646000045 ) ) ;
#16779 = CARTESIAN_POINT ( 'NONE',  ( -8.082524092276901939, -77.95833333333330017, 4.658475568430788805 ) ) ;
#16780 = CARTESIAN_POINT ( 'NONE',  ( -12.54901566180999950, -16.99264670699999868, 0.4731578885120000244 ) ) ;
#16781 = CONICAL_SURFACE ( 'NONE', #49800, 9.649999999844000698, 0.7853981633972997312 ) ;
#16782 = CARTESIAN_POINT ( 'NONE',  ( 10.71369944335146762, -77.87083333333333712, 2.879226727952103548 ) ) ;
#16783 = CARTESIAN_POINT ( 'NONE',  ( 12.24159337356999977, -76.24194166818098495, -0.9828625608234000666 ) ) ;
#16784 = CARTESIAN_POINT ( 'NONE',  ( -8.180687091746206008, -60.10655143787243304, -7.353725627631181538 ) ) ;
#16785 = LINE ( 'NONE', #34186, #870 ) ;
#16786 = CARTESIAN_POINT ( 'NONE',  ( 1.250000000000000222, -78.73958333333331439, -0.1636246173744659582 ) ) ;
#16787 = CARTESIAN_POINT ( 'NONE',  ( -0.2601825140295693228, -80.86128609518755184, -1.488047444107771344 ) ) ;
#16788 = LINE ( 'NONE', #48099, #50407 ) ;
#16789 = CARTESIAN_POINT ( 'NONE',  ( -1.568439782227999846, -77.92713930981540216, -0.3833649254202000090 ) ) ;
#16790 = CARTESIAN_POINT ( 'NONE',  ( 0.000000000000000000, -23.15000000000000213, -11.79999999999999893 ) ) ;
#16791 = ADVANCED_FACE ( 'NONE', ( #28082 ), #37528, .T. ) ;
#16792 = CARTESIAN_POINT ( 'NONE',  ( 1.568694246062999786, -3.720626814303999996, -2.828919489903999995 ) ) ;
#16793 = CARTESIAN_POINT ( 'NONE',  ( 11.71313121114000033, -78.66938348357999189, -3.284064838691000077 ) ) ;
#16794 = DIRECTION ( 'NONE',  ( 2.582636882131000189E-11, 0.000000000000000000, -1.000000000000000000 ) ) ;
#16796 = CARTESIAN_POINT ( 'NONE',  ( -0.1108284043172000077, -77.86024949339380896, -1.314634435239000032 ) ) ;
#16795 = CARTESIAN_POINT ( 'NONE',  ( -8.734625278329845699, -75.80000000000001137, 8.108151766267953420 ) ) ;
#16797 = CARTESIAN_POINT ( 'NONE',  ( 1.160935205181999885, -81.28727493794998793, -0.6914862246935000734 ) ) ;
#16798 = CARTESIAN_POINT ( 'NONE',  ( -8.925400722459096770, -79.55299714917772747, 5.991630607438681366 ) ) ;
#16799 = ORIENTED_EDGE ( 'NONE', *, *, #1400, .T. ) ;
#16800 = CARTESIAN_POINT ( 'NONE',  ( -10.42274798264000069, -21.75365779208000205, -7.691916945395000482 ) ) ;
#16801 = CARTESIAN_POINT ( 'NONE',  ( 11.95103999880999979, -79.43138830090799729, -1.471358499936000097 ) ) ;
#16802 = CARTESIAN_POINT ( 'NONE',  ( -3.176479431003079057, -79.34794335332261994, -8.982299932693875277 ) ) ;
#16803 = CARTESIAN_POINT ( 'NONE',  ( -7.966098808101403250, -80.00000000000000000, -4.899225432969430472 ) ) ;
#16804 = CARTESIAN_POINT ( 'NONE',  ( -9.599999999916001059, -87.30000000008399752, 6.531558194539000517E-10 ) ) ;
#16805 = CARTESIAN_POINT ( 'NONE',  ( 1.829431482522000163, -1.554291850769000227, 3.403309575315999869 ) ) ;
#16806 = CARTESIAN_POINT ( 'NONE',  ( -3.070249596178999951, -79.67092956987599450, 9.402614426748000298 ) ) ;
#16807 = CARTESIAN_POINT ( 'NONE',  ( -8.909545442950999927, -57.79999999967000690, 7.919595949288999570 ) ) ;
#16808 = CARTESIAN_POINT ( 'NONE',  ( 8.082524092276891281, -79.20833333333335702, -4.658475568430806568 ) ) ;
#16809 = ORIENTED_EDGE ( 'NONE', *, *, #42593, .F. ) ;
#16810 = CARTESIAN_POINT ( 'NONE',  ( 4.799999999999999822, -74.99999999999998579, 0.000000000000000000 ) ) ;
#16811 = DIRECTION ( 'NONE',  ( 0.000000000000000000, -1.000000000000000000, 0.000000000000000000 ) ) ;
#16813 = ADVANCED_FACE ( 'NONE', ( #28374 ), #36369, .F. ) ;
#16812 = CIRCLE ( 'NONE', #29069, 1.749999999999999556 ) ;
#16814 = CARTESIAN_POINT ( 'NONE',  ( 11.00000000000000000, -23.75000000000000000, -1.203259120426999909E-14 ) ) ;
#16815 = CARTESIAN_POINT ( 'NONE',  ( -10.35845616728999907, -60.09778595451999905, -7.627487606627999739 ) ) ;
#16816 = EDGE_CURVE ( 'NONE', #19, #1253, #13995, .T. ) ;
#16817 = CARTESIAN_POINT ( 'NONE',  ( -1.529754383668999962, -81.36195569118999060, -0.6588408878327000062 ) ) ;
#16818 = ORIENTED_EDGE ( 'NONE', *, *, #37737, .T. ) ;
#16819 = CARTESIAN_POINT ( 'NONE',  ( 10.58237688094999918, -77.70362064813399172, 3.355437010509000118 ) ) ;
#16820 = DIRECTION ( 'NONE',  ( 1.000000000000000000, 0.000000000000000000, 0.000000000000000000 ) ) ;
#16821 = CARTESIAN_POINT ( 'NONE',  ( 1.636761686205427058, -1.166666666666666963, -2.839805762151336399 ) ) ;
#16822 = AXIS2_PLACEMENT_3D ( 'NONE', #29250, #20697, #56426 ) ;
#16823 = CARTESIAN_POINT ( 'NONE',  ( -12.53241208775999915, -59.56462890159999546, 1.667936697358999965 ) ) ;
#16824 = CARTESIAN_POINT ( 'NONE',  ( -0.7681833999686477066, -78.42708333333334281, 0.9995835529977223910 ) ) ;
#16825 = EDGE_CURVE ( 'NONE', #2252, #1677, #55546, .T. ) ;
#16826 = CARTESIAN_POINT ( 'NONE',  ( -0.6514213267380000172, -79.58985688671099012, 9.745581310452999801 ) ) ;
#16827 = ORIENTED_EDGE ( 'NONE', *, *, #7112, .F. ) ;
#16828 = ORIENTED_EDGE ( 'NONE', *, *, #47775, .F. ) ;
#16829 = CARTESIAN_POINT ( 'NONE',  ( 9.552063159248998403, -76.95329815165599996, -8.017142583401000167 ) ) ;
#16830 = CARTESIAN_POINT ( 'NONE',  ( 2.679031828523773306, -78.74517864561535418, -10.41213411323704463 ) ) ;
#16831 = ORIENTED_EDGE ( 'NONE', *, *, #16089, .T. ) ;
#16832 = CARTESIAN_POINT ( 'NONE',  ( -2.205007487985999770, -77.08380584965398441, 9.235565851336001941 ) ) ;
#16833 = CARTESIAN_POINT ( 'NONE',  ( 9.499157866768639380, -79.10080562451891240, 0.1004279358040388037 ) ) ;
#16834 = CARTESIAN_POINT ( 'NONE',  ( 9.250000000000000000, -78.24999999999998579, -1.152201742116999973E-14 ) ) ;
#16835 = CARTESIAN_POINT ( 'NONE',  ( 6.777770385731999525, -76.84221882925000102, -9.662258766526001352 ) ) ;
#16836 = PRODUCT_DEFINITION_CONTEXT ( 'detailed design', #16063, 'design' ) ;
#16837 = CARTESIAN_POINT ( 'NONE',  ( 11.19952915612999789, -77.99557525653385426, -0.6234238306063999424 ) ) ;
#16838 = CARTESIAN_POINT ( 'NONE',  ( -2.452652587122145178, -86.36264282632899381, 3.310696598561635451 ) ) ;
#16839 = LINE ( 'NONE', #30678, #49220 ) ;
#16840 = ADVANCED_FACE ( 'NONE', ( #1543 ), #54395, .F. ) ;
#16841 = CYLINDRICAL_SURFACE ( 'NONE', #2588, 14.00000000000000000 ) ;
#16842 = CARTESIAN_POINT ( 'NONE',  ( 9.045200488146255324, -80.24963439586137781, 6.447942591652251032 ) ) ;
#16843 = ORIENTED_EDGE ( 'NONE', *, *, #2878, .F. ) ;
#16844 = CARTESIAN_POINT ( 'NONE',  ( -8.859962374443000499, -78.56782986146299663, 6.959166695099000322 ) ) ;
#16845 = CARTESIAN_POINT ( 'NONE',  ( 6.702743137996565181, -77.28954671824730838, -6.375165872689311897 ) ) ;
#16846 = CARTESIAN_POINT ( 'NONE',  ( -0.9676267263329999535, -80.73209164690899797, 1.036212325607999807 ) ) ;
#16847 = CARTESIAN_POINT ( 'NONE',  ( -0.1636246173744673738, -83.11458333333330017, -1.249999999999999778 ) ) ;
#16848 = CARTESIAN_POINT ( 'NONE',  ( -1.344169958103999862, -78.50903577859999416, 0.7015335173854999606 ) ) ;
#16849 = DIRECTION ( 'NONE',  ( 0.7026410690473252618, -0.1122098755728027641, -0.7026410690473252618 ) ) ;
#16850 = CARTESIAN_POINT ( 'NONE',  ( -7.635226873550689852, -18.23391307131834438, 10.36745167322480121 ) ) ;
#16851 = DIRECTION ( 'NONE',  ( 0.000000000000000000, 1.000000000000000000, 0.000000000000000000 ) ) ;
#16852 = B_SPLINE_CURVE_WITH_KNOTS ( 'NONE', 3,
 ( #34881, #30165, #21886, #16897, #58204, #8906, #30456, #53785 ),
 .UNSPECIFIED., .F., .F.,
 ( 4, 2, 2, 4 ),
 ( 0.000000000000000000, 0.4999999999999944489, 0.7499999999999972244, 1.000000000000000000 ),
 .UNSPECIFIED. ) ;
#16853 = CARTESIAN_POINT ( 'NONE',  ( -12.64502302238000020, -19.22870851082999977, -1.799490220168999954 ) ) ;
#16854 = CARTESIAN_POINT ( 'NONE',  ( -1.104290071782900062, -79.13894817590623632, -0.5871211644529236162 ) ) ;
#16855 = CARTESIAN_POINT ( 'NONE',  ( 6.184832724006000149, -78.72869295534098910, -9.286519468188998871 ) ) ;
#16856 = CARTESIAN_POINT ( 'NONE',  ( 10.24998526317999925, -20.24916621771999914, -7.705142895619999877 ) ) ;
#16857 = CARTESIAN_POINT ( 'NONE',  ( -2.813789756862251856, -79.60416666666667140, -10.47020627418439709 ) ) ;
#16858 = CARTESIAN_POINT ( 'NONE',  ( 3.275019288765999903, -80.77167385719099002, -2.584725161986999975 ) ) ;
#16859 = FACE_OUTER_BOUND ( 'NONE', #3253, .T. ) ;
#16860 = ORIENTED_EDGE ( 'NONE', *, *, #51357, .T. ) ;
#16861 = CARTESIAN_POINT ( 'NONE',  ( -8.890092043222985296, -77.19999999999998863, 6.337337654403193632 ) ) ;
#16862 = CARTESIAN_POINT ( 'NONE',  ( -0.8549356769920000154, -79.97302723733999130, -1.335470596990000036 ) ) ;
#16863 = CARTESIAN_POINT ( 'NONE',  ( -3.250000000000000000, -2.004344010466332815, -0.1774124477927127019 ) ) ;
#16864 = CARTESIAN_POINT ( 'NONE',  ( -11.61454496413000115, -77.54640422965499624, 2.935712811417999557 ) ) ;
#16865 = LINE ( 'NONE', #11863, #15551 ) ;
#16866 = CARTESIAN_POINT ( 'NONE',  ( -1.552248384014999871, -82.68160978750299250, 0.6048007385293000526 ) ) ;
#16867 = CIRCLE ( 'NONE', #14036, 9.199999999999999289 ) ;
#16868 = CARTESIAN_POINT ( 'NONE',  ( -1.171009383518375246, -2.152040482700231294, 3.318974785780838044 ) ) ;
#16869 = CARTESIAN_POINT ( 'NONE',  ( -8.918806285220000518, -78.15755584965400260, 3.872830773119999570 ) ) ;
#16870 = CARTESIAN_POINT ( 'NONE',  ( 7.267019124662000173, -77.33715215706898505, -6.153113788875000267 ) ) ;
#16871 = CARTESIAN_POINT ( 'NONE',  ( -10.42531124905999995, -23.26485148473999942, -7.624341765453999997 ) ) ;
#16872 = CARTESIAN_POINT ( 'NONE',  ( -7.674627477105999240, -22.75077028084999853, 10.14950121126000049 ) ) ;
#16873 = LINE ( 'NONE', #34853, #5302 ) ;
#16874 = CARTESIAN_POINT ( 'NONE',  ( -0.9056407151152020552, -81.21193193505192198, -0.8974757952510434844 ) ) ;
#16875 = ORIENTED_EDGE ( 'NONE', *, *, #46865, .F. ) ;
#16876 = CARTESIAN_POINT ( 'NONE',  ( -9.616251104324094356, -78.64978193832848774, 6.835663575338875475 ) ) ;
#16877 = CARTESIAN_POINT ( 'NONE',  ( -2.598229267968284351, -2.153525790767399695, -1.995724898132848812 ) ) ;
#16878 = CARTESIAN_POINT ( 'NONE',  ( -5.709495105464999831, -79.91307963075219334, -10.86213658064000143 ) ) ;
#16879 = CARTESIAN_POINT ( 'NONE',  ( 0.000000000000000000, -39.49523982883999906, 0.000000000000000000 ) ) ;
#16880 = CARTESIAN_POINT ( 'NONE',  ( 0.7076411874954000591, -82.98952008057199237, -1.508144869335000138 ) ) ;
#16881 = CARTESIAN_POINT ( 'NONE',  ( -5.859445663532000914, -77.75263303298099515, 9.564779511708000115 ) ) ;
#16882 = CARTESIAN_POINT ( 'NONE',  ( 10.97550047727999889, -78.18052123279399268, 0.05101033830554000531 ) ) ;
#16883 = CARTESIAN_POINT ( 'NONE',  ( -5.440921534716935071, -80.39791666666549474, 9.438387255472232340 ) ) ;
#16884 = CARTESIAN_POINT ( 'NONE',  ( -6.650186219591999404, -76.86123477876799370, 10.45045725565999994 ) ) ;
#16885 = CARTESIAN_POINT ( 'NONE',  ( 1.064301949326286190, -78.56405572308268859, 11.70180493458724236 ) ) ;
#16886 = DIRECTION ( 'NONE',  ( -0.4045626180512096881, -0.8201574093740189308, -0.4045626180512096881 ) ) ;
#16887 = VERTEX_POINT ( 'NONE', #13932 ) ;
#16888 = CARTESIAN_POINT ( 'NONE',  ( 5.948804865077000237, -80.03906619586439319, 9.426875752653000262 ) ) ;
#16889 = CARTESIAN_POINT ( 'NONE',  ( 9.164177083796486656, -77.26245504524652574, 1.449973650478227682 ) ) ;
#16890 = CARTESIAN_POINT ( 'NONE',  ( 1.439896632895284911, -78.06458333333334565, 11.00000000000000355 ) ) ;
#16891 = CARTESIAN_POINT ( 'NONE',  ( -11.14855507251999889, -78.24626308856198875, -0.4486863643567999826 ) ) ;
#16892 = DIRECTION ( 'NONE',  ( 0.000000000000000000, 0.000000000000000000, 1.000000000000000000 ) ) ;
#16893 = CARTESIAN_POINT ( 'NONE',  ( -0.6531259097149988424, -79.01686433677801347, 1.115453275870143202 ) ) ;
#16894 = CARTESIAN_POINT ( 'NONE',  ( -0.9976315024470040482, -82.41817118228848926, -1.183693355290223570 ) ) ;
#16895 = CARTESIAN_POINT ( 'NONE',  ( 3.030935459916999974, -79.18144108438299611, 11.73679554811000081 ) ) ;
#16896 = VERTEX_POINT ( 'NONE', #9808 ) ;
#16897 = CARTESIAN_POINT ( 'NONE',  ( -1.618935784732014715, -60.72751168617232054, 12.52134385804453132 ) ) ;
#16898 = CARTESIAN_POINT ( 'NONE',  ( 13.94827586207000003, -45.69638659094999866, 8.082388075971999052E-06 ) ) ;
#16899 = EDGE_CURVE ( 'NONE', #9471, #15167, #14921, .T. ) ;
#16900 = CARTESIAN_POINT ( 'NONE',  ( 9.396085398178598780, -76.10208333333331154, 7.220923959705271677 ) ) ;
#16901 = VERTEX_POINT ( 'NONE', #41971 ) ;
#16902 = EDGE_LOOP ( 'NONE', ( #4188, #16733, #7687, #53531, #1818, #23390 ) ) ;
#16903 = DIRECTION ( 'NONE',  ( 0.000000000000000000, 0.000000000000000000, -1.000000000000000000 ) ) ;
#16904 = AXIS2_PLACEMENT_3D ( 'NONE', #44986, #54434, #49420 ) ;
#16905 = ORIENTED_EDGE ( 'NONE', *, *, #1527, .F. ) ;
#16906 = CARTESIAN_POINT ( 'NONE',  ( -3.417863094299999904, -78.44998361729999203, 11.50296535110000029 ) ) ;
#16907 = ORIENTED_EDGE ( 'NONE', *, *, #54145, .F. ) ;
#16908 = CARTESIAN_POINT ( 'NONE',  ( -10.34074641381923065, -80.99999999999998579, -3.089209180937224630 ) ) ;
#16909 = CARTESIAN_POINT ( 'NONE',  ( 5.013494814495999208, -77.41043913071800375, 9.697434492446999954 ) ) ;
#16910 = VECTOR ( 'NONE', #2190, 1000.000000000000227 ) ;
#16911 = ITEM_DEFINED_TRANSFORMATION ( 'NONE', 'NONE', #25386,  #43526 ) ;
#16912 = B_SPLINE_CURVE_WITH_KNOTS ( 'NONE', 3,
 ( #2739, #11309, #43184, #7450, #16599, #56757, #3025, #52331, #20166, #34009, #21023, #42603, #43470, #11886, #47338, #29864, #57040, #34585, #2166, #56177, #51758, #29290, #6867, #55887, #52616, #24876, #42893, #28708, #6278, #24295, #20453, #47047, #42310, #1877, #56466, #11024, #19872, #52044, #37866, #11601, #15437, #29007, #51468, #29577, #47634, #57899, #17166, #57606, #17756, #53473, #8020, #13014, #39602, #21597, #26016, #13310, #30727, #25735, #31013, #12733, #44323, #8894, #49051, #8599, #26888, #26585, #44042, #44619, #39316, #48762, #73, #4175, #22467, #17456, #35152, #3592, #3313, #22172, #57325, #30445, #21878, #53185, #35442, #43762, #8308, #31305 ),
 .UNSPECIFIED., .F., .F.,
 ( 4, 2, 2, 2, 1, 1, 2, 2, 2, 2, 2, 1, 1, 2, 2, 2, 2, 1, 1, 1, 2, 2, 2, 2, 2, 1, 1, 2, 2, 2, 2, 2, 1, 1, 2, 2, 2, 2, 2, 1, 1, 2, 2, 2, 2, 1, 1, 1, 2, 2, 4 ),
 ( 0.000000000000000000, 0.06250000000000065226, 0.09375000000000101308, 0.1093750000000011796, 0.1171875000000012490, 0.1210937500000010408, 0.1230468750000006661, 0.1250000000000002776, 0.1874999999999829581, 0.2187499999999746869, 0.2343749999999705791, 0.2421874999999685252, 0.2460937499999677480, 0.2480468749999675537, 0.2499999999999673872, 0.3124999999999732991, 0.3437499999999761857, 0.3593749999999776290, 0.3671874999999786282, 0.3710937499999789058, 0.3730468749999790723, 0.3749999999999792388, 0.4374999999999646394, 0.4687499999999570344, 0.4843749999999532041, 0.4921874999999515943, 0.4960937499999504841, 0.4980468749999502065, 0.4999999999999498734, 0.5624999999999505951, 0.5937499999999512612, 0.6093749999999515943, 0.6171874999999518163, 0.6210937499999518163, 0.6230468749999517053, 0.6249999999999514833, 0.6874999999999450440, 0.7187499999999413802, 0.7343749999999392708, 0.7421874999999382716, 0.7460937499999377165, 0.7480468749999377165, 0.7499999999999377165, 0.8124999999999399369, 0.8437499999999413802, 0.8593749999999421574, 0.8671874999999426015, 0.8710937499999427125, 0.8730468749999427125, 0.8749999999999427125, 1.000000000000000000 ),
 .UNSPECIFIED. ) ;
#16913 = CARTESIAN_POINT ( 'NONE',  ( -5.708830652390999738, -78.18073667140099303, 8.101181774151999804 ) ) ;
#16914 = CARTESIAN_POINT ( 'NONE',  ( -11.06493808903000087, -79.21142954368899325, -1.839906431680000010 ) ) ;
#16915 = ADVANCED_FACE ( 'NONE', ( #49972 ), #35680, .T. ) ;
#16916 = ORIENTED_EDGE ( 'NONE', *, *, #47656, .T. ) ;
#16917 = VERTEX_POINT ( 'NONE', #18671 ) ;
#16918 = CARTESIAN_POINT ( 'NONE',  ( -4.267465266896234510, -77.51327689984762515, 8.206740657596899524 ) ) ;
#16919 = CARTESIAN_POINT ( 'NONE',  ( -6.065106684382000068, -77.23082865815298703, 9.224892016835999797 ) ) ;
#16920 = LINE ( 'NONE', #26617, #26244 ) ;
#16921 = CARTESIAN_POINT ( 'NONE',  ( -12.77649732931999971, -62.10828417218999675, 0.06479631635403998446 ) ) ;
#16922 = CARTESIAN_POINT ( 'NONE',  ( 9.367484565636001292, -79.05912826326098752, -2.533990228858999938 ) ) ;
#16923 = CARTESIAN_POINT ( 'NONE',  ( 7.627487525415999947, -23.29778754190000001, 10.35845608625999859 ) ) ;
#16924 = CARTESIAN_POINT ( 'NONE',  ( -9.249310757543522499, -77.50112171249398330, -0.1303866578235779172 ) ) ;
#16925 = CARTESIAN_POINT ( 'NONE',  ( 1.750000000000000000, -18.75000000310999937, 12.50000000000000000 ) ) ;
#16926 = CARTESIAN_POINT ( 'NONE',  ( 3.942135768300999654, -80.02332530777499642, -10.54187931140000067 ) ) ;
#16927 = CARTESIAN_POINT ( 'NONE',  ( -1.217465845835394411, -81.02083333333330017, -0.3271848554491003647 ) ) ;
#16928 = EDGE_LOOP ( 'NONE', ( #13115, #50530, #50895, #5831 ) ) ;
#16929 = CARTESIAN_POINT ( 'NONE',  ( 12.08450773144999957, -79.26983947277899745, 1.677439557700999950 ) ) ;
#16930 = CARTESIAN_POINT ( 'NONE',  ( -7.619712398427999744, -55.39595871828999663, 10.35409979025000027 ) ) ;
#16931 = CARTESIAN_POINT ( 'NONE',  ( 11.95248949435000085, -78.95705916112399336, 0.8087524912306001124 ) ) ;
#16932 = ADVANCED_FACE ( 'NONE', ( #45837 ), #15097, .F. ) ;
#16933 = CARTESIAN_POINT ( 'NONE',  ( -9.317995624416001377, -16.86762134170999872, -8.588852714006002032 ) ) ;
#16935 = CARTESIAN_POINT ( 'NONE',  ( -7.483407197968000801, -77.00000000000000000, 5.437013583706000297 ) ) ;
#16934 = CARTESIAN_POINT ( 'NONE',  ( 7.648026768036999989, -60.04999998387000204, 10.12290050219000115 ) ) ;
#16936 = VECTOR ( 'NONE', #17507, 1000.000000000000227 ) ;
#16937 = CARTESIAN_POINT ( 'NONE',  ( -5.838193839761688153, -78.87291666666669698, -7.596835002782716728 ) ) ;
#16938 = DIRECTION ( 'NONE',  ( 0.000000000000000000, -1.000000000000000000, 0.000000000000000000 ) ) ;
#16939 = CARTESIAN_POINT ( 'NONE',  ( 0.2638252682410999750, -78.51802014218399961, -11.14383981435000059 ) ) ;
#16940 = CARTESIAN_POINT ( 'NONE',  ( 3.477442601125609656, -3.499999999999999556, 0.5952757321258587142 ) ) ;
#16941 = CARTESIAN_POINT ( 'NONE',  ( -3.045222912875851673, -0.7922096678350301069, -1.778097659094616700 ) ) ;
#16942 = ORIENTED_EDGE ( 'NONE', *, *, #44317, .T. ) ;
#16943 = CARTESIAN_POINT ( 'NONE',  ( 10.07627163191000008, -18.75000000310999937, 7.601397897754999633 ) ) ;
#16944 = CARTESIAN_POINT ( 'NONE',  ( -1.758095523371000057, -55.07708336086999878, 12.57362173513000059 ) ) ;
#16945 = CARTESIAN_POINT ( 'NONE',  ( -12.71658889741999943, -23.31584477285000290, 1.931087888049999979 ) ) ;
#16946 = CARTESIAN_POINT ( 'NONE',  ( 0.7364373216886999085, -2.859035817501999865, -3.734094651500999618 ) ) ;
#16947 = CARTESIAN_POINT ( 'NONE',  ( -10.05535668103000191, -78.16178278646499678, 4.970705447719999448 ) ) ;
#16948 = AXIS2_PLACEMENT_3D ( 'NONE', #49118, #53844, #17829 ) ;
#16949 = CARTESIAN_POINT ( 'NONE',  ( -12.61117324687999997, -55.58448536084999603, 1.798979683803999974 ) ) ;
#16950 = CARTESIAN_POINT ( 'NONE',  ( 0.8445585116414999760, -61.51040443210000319, 12.43380736240999873 ) ) ;
#16951 = CARTESIAN_POINT ( 'NONE',  ( 2.598917237794088564, -3.197916666666666519, -1.997276839918468605 ) ) ;
#16952 = VECTOR ( 'NONE', #52625, 1000.000000000000000 ) ;
#16953 = CARTESIAN_POINT ( 'NONE',  ( 2.192539838120000084, -85.74949735065199263, 3.552799672304999934 ) ) ;
#16954 = DIRECTION ( 'NONE',  ( -1.000000000000000000, 0.000000000000000000, 0.000000000000000000 ) ) ;
#16955 = CARTESIAN_POINT ( 'NONE',  ( -12.02231848918561319, -76.94547861865662242, 1.134278802166899025 ) ) ;
#16956 = CARTESIAN_POINT ( 'NONE',  ( 11.12264838851901771, -76.42369462702311012, -3.807881462539005391 ) ) ;
#16957 = CARTESIAN_POINT ( 'NONE',  ( -11.14677829112999952, -77.70931131755500587, -0.06272399197938000048 ) ) ;
#16958 = CARTESIAN_POINT ( 'NONE',  ( 0.2007160378926907962, -81.96275121485238913, 1.233601532853040750 ) ) ;
#16959 = CARTESIAN_POINT ( 'NONE',  ( 0.1460928719284999844, -78.69802764147999596, 1.657165064314999992 ) ) ;
#16960 = CARTESIAN_POINT ( 'NONE',  ( 9.100722152916000951, -76.93205879495988597, -3.274758550341999808 ) ) ;
#16961 = CARTESIAN_POINT ( 'NONE',  ( 8.395992668097999712, -79.29944415034599103, 4.560928606276999808 ) ) ;
#16962 = CARTESIAN_POINT ( 'NONE',  ( 3.124639411803366240, -3.375269249970192842, 1.018784870465328618 ) ) ;
#16963 = CARTESIAN_POINT ( 'NONE',  ( -2.085031794558877660, -80.20968772933238711, -10.54572087693944837 ) ) ;
#16964 = CARTESIAN_POINT ( 'NONE',  ( -1.335477334469999862E-14, -72.70000000000000284, 0.000000000000000000 ) ) ;
#16965 = CARTESIAN_POINT ( 'NONE',  ( 11.15695051371543833, -79.60814770476476099, 1.159337827475353189 ) ) ;
#16966 = CARTESIAN_POINT ( 'NONE',  ( -12.02912753549999891, -79.56554297241000029, 0.08506824670321999626 ) ) ;
#16967 = EDGE_CURVE ( 'NONE', #31041, #5144, #55163, .T. ) ;
#16968 = DIRECTION ( 'NONE',  ( -0.7071067811865475727, 0.000000000000000000, 0.7071067811865475727 ) ) ;
#16969 = CARTESIAN_POINT ( 'NONE',  ( 3.646964122112999807, -80.17176962903970150, 10.50067842184000000 ) ) ;
#16970 = PLANE ( 'NONE',  #56353 ) ;
#16971 = ORIENTED_EDGE ( 'NONE', *, *, #16434, .T. ) ;
#16972 = CONICAL_SURFACE ( 'NONE', #29219, 3.399999999997999733, 0.9827937232471395390 ) ;
#16973 = EDGE_CURVE ( 'NONE', #52539, #8827, #36950, .T. ) ;
#16974 = CARTESIAN_POINT ( 'NONE',  ( 1.575772165398017455, -24.46154542799817122, 12.70597445617727317 ) ) ;
#16975 = ORIENTED_EDGE ( 'NONE', *, *, #49961, .T. ) ;
#16976 = ORIENTED_EDGE ( 'NONE', *, *, #47448, .T. ) ;
#16977 = CARTESIAN_POINT ( 'NONE',  ( 2.598917237794080570, -1.302083333333333703, 1.997276839918479485 ) ) ;
#16978 = CARTESIAN_POINT ( 'NONE',  ( -3.399999999999999911, -78.69999997992952956, 5.715921273723000819E-07 ) ) ;
#16979 = CARTESIAN_POINT ( 'NONE',  ( 5.708176239699000121, -78.24219514392800079, -9.305495801267001710 ) ) ;
#16980 = B_SPLINE_CURVE_WITH_KNOTS ( 'NONE', 3,
 ( #43391, #1810, #2949, #37798, #39533, #44255, #22099, #39240 ),
 .UNSPECIFIED., .F., .F.,
 ( 4, 2, 2, 4 ),
 ( 0.000000000000000000, 0.5000000000000000000, 0.7500000000000000000, 1.000000000000000000 ),
 .UNSPECIFIED. ) ;
#16981 = CARTESIAN_POINT ( 'NONE',  ( -2.051686749538000232, -80.61806754721197876, -2.945220990589999754 ) ) ;
#16982 = CARTESIAN_POINT ( 'NONE',  ( -6.834826231162627330, -79.33866059855550645, 6.598048657260681793 ) ) ;
#16983 = EDGE_LOOP ( 'NONE', ( #54155, #52480, #631, #42989 ) ) ;
#16984 = CARTESIAN_POINT ( 'NONE',  ( 3.321932689531000182, -77.19999999999998863, 10.22385755016999909 ) ) ;
#16986 = ADVANCED_FACE ( 'NONE', ( #11844 ), #28964, .F. ) ;
#16985 = CARTESIAN_POINT ( 'NONE',  ( -3.941558004887999900, -78.60478991842998653, -11.71306536694000044 ) ) ;
#16987 = ORIENTED_EDGE ( 'NONE', *, *, #4965, .T. ) ;
#16988 = VERTEX_POINT ( 'NONE', #20411 ) ;
#16989 = DIRECTION ( 'NONE',  ( 0.7071067811865473507, 1.433669009702094715E-08, -0.7071067811865473507 ) ) ;
#16990 = CARTESIAN_POINT ( 'NONE',  ( -1.887341892627375062, -79.79999999999998295, 11.86718873371815519 ) ) ;
#16991 = CARTESIAN_POINT ( 'NONE',  ( -6.927833380277669484, -80.03110721467722044, 8.219656879950077766 ) ) ;
#16992 = AXIS2_PLACEMENT_3D ( 'NONE', #28845, #10874, #42740 ) ;
#16993 = CARTESIAN_POINT ( 'NONE',  ( -9.309367086190000862, -77.13855160546319212, -0.1968645694141999969 ) ) ;
#16994 = CARTESIAN_POINT ( 'NONE',  ( 2.289901096216106158, -86.09999999999999432, -3.216015270247992497 ) ) ;
#16995 = CARTESIAN_POINT ( 'NONE',  ( -2.951654015434272971, -86.08669351303142037, 1.729693878444511501 ) ) ;
#16996 = CARTESIAN_POINT ( 'NONE',  ( 17.50000000000000000, -57.79999999999999716, 0.000000000000000000 ) ) ;
#16997 = CARTESIAN_POINT ( 'NONE',  ( 7.199854605362999926, -76.91759889844999520, -10.39073109867000078 ) ) ;
#16998 = CARTESIAN_POINT ( 'NONE',  ( 5.292034929522999143, -76.29392014291700264, 9.642417924923000427 ) ) ;
#16999 = DIRECTION ( 'NONE',  ( 0.000000000000000000, -1.000000000000000000, 0.000000000000000000 ) ) ;
#17000 = CARTESIAN_POINT ( 'NONE',  ( 2.636414666285999964, -81.45596103735698534, 2.958936952162999567 ) ) ;
#17001 = DIRECTION ( 'NONE',  ( 0.000000000000000000, -1.000000000000000000, 0.000000000000000000 ) ) ;
#17002 = CARTESIAN_POINT ( 'NONE',  ( -1.635769836470996941, -3.018359365201534139, 2.808997201014398204 ) ) ;
#17003 = CARTESIAN_POINT ( 'NONE',  ( -1.757416575686000071, -79.96130496681199418, 3.081079248453999941 ) ) ;
#17004 = CARTESIAN_POINT ( 'NONE',  ( 1.250000000000000000, -82.84999999999999432, 0.000000000000000000 ) ) ;
#17005 = CARTESIAN_POINT ( 'NONE',  ( -2.279442914376999862, -83.46474735065199013, -2.714609328494999474 ) ) ;
#17006 = CARTESIAN_POINT ( 'NONE',  ( 3.665025684363000025, -3.545621233726000021, -1.025097465345000236 ) ) ;
#17007 = CARTESIAN_POINT ( 'NONE',  ( -1.229805502134054151, -80.77148655050061166, -0.3338661523633573713 ) ) ;
#17008 = CARTESIAN_POINT ( 'NONE',  ( -7.618386461959000044, -60.02712559312999474, -10.53495196325000016 ) ) ;
#17009 = CARTESIAN_POINT ( 'NONE',  ( -12.00000000000000711, -79.29293765275959061, 1.064976873965741921 ) ) ;
#17010 = CARTESIAN_POINT ( 'NONE',  ( -0.6509962010243000030, -81.59369388267100476, 1.163950211895000031 ) ) ;
#17011 = CIRCLE ( 'NONE', #55705, 9.760776772971999193 ) ;
#17012 = CARTESIAN_POINT ( 'NONE',  ( -12.66001647286000065, -17.36746073369999621, -1.381678996660999914 ) ) ;
#17013 = CARTESIAN_POINT ( 'NONE',  ( -1.250000000000000000, -23.25000000000000000, -12.00000000000000000 ) ) ;
#17014 = EDGE_CURVE ( 'NONE', #47018, #17785, #15977, .T. ) ;
#17015 = CARTESIAN_POINT ( 'NONE',  ( -1.302418038466582884, -79.44516373638910522, -0.8227471584171216490 ) ) ;
#17016 = CARTESIAN_POINT ( 'NONE',  ( 1.689459950949288913, -24.29188253905320849, -12.71013585610226926 ) ) ;
#17017 = CARTESIAN_POINT ( 'NONE',  ( 11.73828326341999961, -75.71624058713000238, -4.332684199240000034 ) ) ;
#17018 = ORIENTED_EDGE ( 'NONE', *, *, #31581, .F. ) ;
#17019 = CARTESIAN_POINT ( 'NONE',  ( 0.000000000000000000, -9.295797029142999435, 0.000000000000000000 ) ) ;
#17020 = CARTESIAN_POINT ( 'NONE',  ( -14.00000000000000000, -45.91785611817000046, 0.000000000000000000 ) ) ;
#17021 = CARTESIAN_POINT ( 'NONE',  ( -10.99999999999999822, -18.25000000000001066, -0.1607611550118174248 ) ) ;
#17022 = CARTESIAN_POINT ( 'NONE',  ( 12.00000000000000000, -79.14999999999999147, 0.000000000000000000 ) ) ;
#17023 = CARTESIAN_POINT ( 'NONE',  ( -1.944889849486000077, -77.50188066968198086, -9.432423272878001086 ) ) ;
#17024 = CARTESIAN_POINT ( 'NONE',  ( 3.687576869571000060, -82.51000322433299061, 1.957448392864999720 ) ) ;
#17025 = CARTESIAN_POINT ( 'NONE',  ( 1.830902252650064010, -79.96174285384452673, 10.59271595565334678 ) ) ;
#17026 = CARTESIAN_POINT ( 'NONE',  ( -0.6603457068528999496, -80.68630120477999412, -1.153171400786999978 ) ) ;
#17027 = VERTEX_POINT ( 'NONE', #33094 ) ;
#17028 = CARTESIAN_POINT ( 'NONE',  ( 10.75000000000000000, -77.35000000000000853, 0.000000000000000000 ) ) ;
#17029 = CARTESIAN_POINT ( 'NONE',  ( 1.406250000003000045, -82.09374999999700151, -9.314605757769000352E-11 ) ) ;
#17030 = AXIS2_PLACEMENT_3D ( 'NONE', #3601, #8028, #21605 ) ;
#17031 = DIRECTION ( 'NONE',  ( 0.000000000000000000, 1.000000000000000000, 0.000000000000000000 ) ) ;
#17032 = VERTEX_POINT ( 'NONE', #2983 ) ;
#17033 = CARTESIAN_POINT ( 'NONE',  ( -7.484260875330000395, -78.93586165678098610, -7.979577400219000083 ) ) ;
#17034 = CARTESIAN_POINT ( 'NONE',  ( -9.723174507563001612, -61.27697503937000079, -7.958760295438001009 ) ) ;
#17035 = CARTESIAN_POINT ( 'NONE',  ( -7.298083752484999742, -79.81301656954198620, -8.811591453050999334 ) ) ;
#17036 = ORIENTED_EDGE ( 'NONE', *, *, #19287, .T. ) ;
#17037 = EDGE_CURVE ( 'NONE', #8440, #45906, #12188, .T. ) ;
#17038 = CARTESIAN_POINT ( 'NONE',  ( 1.747513281931999840, -77.39552404313198508, -11.88039736288000014 ) ) ;
#17039 = EDGE_LOOP ( 'NONE', ( #35255, #38963, #38081, #9578 ) ) ;
#17040 = ORIENTED_EDGE ( 'NONE', *, *, #39759, .F. ) ;
#17041 = CARTESIAN_POINT ( 'NONE',  ( -3.241578944612999891, -86.36264282653499436, 1.443243925434000152 ) ) ;
#17042 = CARTESIAN_POINT ( 'NONE',  ( 9.226480760116999136, -79.48087102891551581, -2.263195259622999611 ) ) ;
#17043 = VERTEX_POINT ( 'NONE', #39273 ) ;
#17045 = EDGE_CURVE ( 'NONE', #38125, #56550, #37593, .T. ) ;
#17044 = CARTESIAN_POINT ( 'NONE',  ( 10.98675469975087182, -18.58582062461607620, 0.5398555193318163026 ) ) ;
#17046 = AXIS2_PLACEMENT_3D ( 'NONE', #49204, #53935, #18499 ) ;
#17047 = ORIENTED_EDGE ( 'NONE', *, *, #45440, .F. ) ;
#17048 = CARTESIAN_POINT ( 'NONE',  ( 1.026866341085000007E-14, -0.1000000000000002554, 0.000000000000000000 ) ) ;
#17049 = EDGE_CURVE ( 'NONE', #34794, #45142, #7999, .T. ) ;
#17050 = CARTESIAN_POINT ( 'NONE',  ( 2.236739703425203896, -78.96264283715740362, -3.872902730369248925 ) ) ;
#17051 = CARTESIAN_POINT ( 'NONE',  ( 8.596775676211999340, -53.66467110130999885, 9.310147894663000301 ) ) ;
#17052 = CARTESIAN_POINT ( 'NONE',  ( 0.5705388283922003811, -18.65989902471944006, 10.98520465578114269 ) ) ;
#17053 = CARTESIAN_POINT ( 'NONE',  ( 4.741624724934583313, -79.58333333332932114, 8.228481283912117306 ) ) ;
#17054 = DIRECTION ( 'NONE',  ( 1.000000000000000000, 0.000000000000000000, 0.000000000000000000 ) ) ;
#17055 = CARTESIAN_POINT ( 'NONE',  ( -0.8328560967162584872, -77.92807624077448736, -1.259433156755825012 ) ) ;
#17056 = CARTESIAN_POINT ( 'NONE',  ( 8.547140491457867029, -78.81892730245148471, -3.536545408174746274 ) ) ;
#17057 = CARTESIAN_POINT ( 'NONE',  ( 0.000000000000000000, -81.90000000002299885, -10.59999999997999787 ) ) ;
#17058 = CIRCLE ( 'NONE', #47270, 0.6000000000000008660 ) ;
#17059 = CARTESIAN_POINT ( 'NONE',  ( -4.074332639539999690, -81.69600264934798872, -0.9107214065898999733 ) ) ;
#17060 = CARTESIAN_POINT ( 'NONE',  ( 6.954721136732000097, -77.50786001420199511, -7.007357181289999737 ) ) ;
#17061 = CARTESIAN_POINT ( 'NONE',  ( -12.50412785605871946, -24.51985834634420414, 1.235051469882017861 ) ) ;
#17062 = DIRECTION ( 'NONE',  ( 0.7071067811865474617, 0.000000000000000000, -0.7071067811865474617 ) ) ;
#17063 = CARTESIAN_POINT ( 'NONE',  ( -1.984586691443999795, -75.88675793620500087, 11.75553522549000007 ) ) ;
#17064 = CARTESIAN_POINT ( 'NONE',  ( -7.995796640820073797, -60.48684619742725488, -7.555116226631964693 ) ) ;
#17065 = CARTESIAN_POINT ( 'NONE',  ( -0.7820311386674927423, -78.43009031498998240, 12.04485182656622833 ) ) ;
#17066 = CARTESIAN_POINT ( 'NONE',  ( 1.092232985442823212, -78.70833333333331439, -0.6295237254636224522 ) ) ;
#17067 = CARTESIAN_POINT ( 'NONE',  ( 1.459813637468974301, -80.12054394350599296, 0.3988620006733276657 ) ) ;
#17068 = CARTESIAN_POINT ( 'NONE',  ( 1.482146596920999926, -78.12558980333969316, -0.6406678853001999130 ) ) ;
#17069 = CYLINDRICAL_SURFACE ( 'NONE', #9713, 14.00000000000000000 ) ;
#17070 = CARTESIAN_POINT ( 'NONE',  ( -3.530714078838999903, -1.879486066823000234, 0.1002381994080999983 ) ) ;
#17071 = EDGE_CURVE ( 'NONE', #4408, #37493, #57361, .T. ) ;
#17072 = CARTESIAN_POINT ( 'NONE',  ( 3.030935459916999974, -78.72825989114500089, 11.73679554811000081 ) ) ;
#17073 = CARTESIAN_POINT ( 'NONE',  ( 10.42531124908000173, -60.06485148440999922, 7.624341765471999821 ) ) ;
#17075 = CARTESIAN_POINT ( 'NONE',  ( -1.313442439244999926, -79.24940294806400232, -0.1235842678404999867 ) ) ;
#17074 = CARTESIAN_POINT ( 'NONE',  ( -11.47922858557694781, -76.18255052542706096, 2.508348395795582331 ) ) ;
#17076 = CARTESIAN_POINT ( 'NONE',  ( -1.400413196275999805, -83.11904964980398347, 0.4410028580390000230 ) ) ;
#17077 = CARTESIAN_POINT ( 'NONE',  ( -6.271985153401672619, -79.52459541282148336, 8.730686292822458228 ) ) ;
#17078 = ORIENTED_EDGE ( 'NONE', *, *, #38805, .T. ) ;
#17079 = EDGE_CURVE ( 'NONE', #10368, #21583, #34749, .T. ) ;
#17080 = DIRECTION ( 'NONE',  ( 0.000000000000000000, 1.000000000000000000, 0.000000000000000000 ) ) ;
#17081 = CARTESIAN_POINT ( 'NONE',  ( -6.597056085936999992, -79.17951179515100080, 10.21048365676999836 ) ) ;
#17082 = CARTESIAN_POINT ( 'NONE',  ( -9.271561418023951617, -79.22981385905036689, 2.410639693388377580 ) ) ;
#17083 = CARTESIAN_POINT ( 'NONE',  ( 9.396085398178630754, -76.99791666666666856, -7.220923959705230821 ) ) ;
#17084 = CARTESIAN_POINT ( 'NONE',  ( -12.80090744918999945, -56.03767312542999690, -1.980532734072999901 ) ) ;
#17085 = LINE ( 'NONE', #25937, #1577 ) ;
#17086 = CARTESIAN_POINT ( 'NONE',  ( 5.707072418784999712, -79.53235851257699096, 7.943069029044000473 ) ) ;
#17087 = CARTESIAN_POINT ( 'NONE',  ( 12.43569926716000040, -24.88202093001000037, -0.4277578398254000547 ) ) ;
#17088 = DIRECTION ( 'NONE',  ( 0.7071067811865475727, 0.000000000000000000, -0.7071067811865475727 ) ) ;
#17089 = VERTEX_POINT ( 'NONE', #44082 ) ;
#17090 = DIRECTION ( 'NONE',  ( 0.000000000000000000, 1.000000000000000000, 0.000000000000000000 ) ) ;
#17091 = CARTESIAN_POINT ( 'NONE',  ( -9.233730314758000546, -79.77988667140100176, -2.745678512080999667 ) ) ;
#17092 = CARTESIAN_POINT ( 'NONE',  ( -1.500000000000000000, -79.39999999999999147, 0.000000000000000000 ) ) ;
#17093 = CARTESIAN_POINT ( 'NONE',  ( 0.3926218265389221362, -78.54583333333334849, -1.460959015002473160 ) ) ;
#17094 = CARTESIAN_POINT ( 'NONE',  ( -3.302441756588000210, -84.59192953870899601, 1.295542768871000172 ) ) ;
#17095 = ORIENTED_EDGE ( 'NONE', *, *, #52260, .T. ) ;
#17096 = DIRECTION ( 'NONE',  ( 1.000000000000000000, 0.000000000000000000, 0.000000000000000000 ) ) ;
#17097 = VECTOR ( 'NONE', #51999, 1000.000000000000114 ) ;
#17098 = CARTESIAN_POINT ( 'NONE',  ( -9.500000000000000000, -78.39999999999999147, 0.000000000000000000 ) ) ;
#17099 = CARTESIAN_POINT ( 'NONE',  ( 3.250000000000000444, -1.239583333333333481, -0.4254240051736113415 ) ) ;
#17100 = ORIENTED_EDGE ( 'NONE', *, *, #17294, .F. ) ;
#17101 = AXIS2_PLACEMENT_3D ( 'NONE', #43475, #15732, #11892 ) ;
#17102 = CARTESIAN_POINT ( 'NONE',  ( -7.646788101807000082, -55.42771363232999704, -10.00831428589000005 ) ) ;
#17103 = CARTESIAN_POINT ( 'NONE',  ( 1.841371367509999857, -79.90994107844498728, -9.592189096167999196 ) ) ;
#17104 = ORIENTED_EDGE ( 'NONE', *, *, #35004, .F. ) ;
#17105 = ORIENTED_EDGE ( 'NONE', *, *, #14435, .F. ) ;
#17107 = ADVANCED_FACE ( 'NONE', ( #8938 ), #7425, .F. ) ;
#17106 = CARTESIAN_POINT ( 'NONE',  ( 6.764901149608999908, -77.36370303413399085, -9.901050649137001614 ) ) ;
#17108 = CARTESIAN_POINT ( 'NONE',  ( 0.000000000000000000, -75.15999999999999659, 0.000000000000000000 ) ) ;
#17109 = CARTESIAN_POINT ( 'NONE',  ( -1.215029926349999956, -77.61107607421000409, 0.5215463190299000074 ) ) ;
#17110 = EDGE_CURVE ( 'NONE', #5115, #50169, #31181, .T. ) ;
#17111 = ORIENTED_EDGE ( 'NONE', *, *, #23707, .F. ) ;
#17112 = CARTESIAN_POINT ( 'NONE',  ( 4.897371265365999982, -77.02075584965399457, 7.847181321287999722 ) ) ;
#17113 = CYLINDRICAL_SURFACE ( 'NONE', #49903, 1.500000000000000000 ) ;
#17114 = CARTESIAN_POINT ( 'NONE',  ( -1.980611416588874629, -55.27402268162218490, 12.74335092660349567 ) ) ;
#17115 = CARTESIAN_POINT ( 'NONE',  ( -12.75337166745000061, -77.17524667502999591, -1.077318095482000082 ) ) ;
#17116 = CARTESIAN_POINT ( 'NONE',  ( 1.633411169670999863, -77.88662988452688296, -11.09730050697999992 ) ) ;
#17117 = CARTESIAN_POINT ( 'NONE',  ( -12.10214643675714008, -78.46315847178392744, -1.986460023565977062 ) ) ;
#17118 = CARTESIAN_POINT ( 'NONE',  ( 1.504274447196719100, -86.39318692756698681, 3.466210801031044397 ) ) ;
#17119 = CARTESIAN_POINT ( 'NONE',  ( -5.268979267983999293, -78.81559565747798501, 9.902321347348999936 ) ) ;
#17120 = CARTESIAN_POINT ( 'NONE',  ( 0.7916942038310399443, -79.96867701788805505, 9.217398666066213053 ) ) ;
#17121 = LINE ( 'NONE', #54023, #51097 ) ;
#17122 = STYLED_ITEM ( 'NONE', ( #22705 ), #463 ) ;
#17123 = ORIENTED_EDGE ( 'NONE', *, *, #14195, .F. ) ;
#17124 = CARTESIAN_POINT ( 'NONE',  ( 7.410162453131999172, -79.43869284577598933, 8.486367113423000319 ) ) ;
#17125 = CARTESIAN_POINT ( 'NONE',  ( 4.220602197252363297, -77.26272508603567246, -8.230959913729840594 ) ) ;
#17126 = CARTESIAN_POINT ( 'NONE',  ( 1.309314855877999895, -79.98214323184599550, -0.1620500492231000123 ) ) ;
#17127 = CARTESIAN_POINT ( 'NONE',  ( -1.249999999999999778, -83.01041666666662877, -0.1636246173744686228 ) ) ;
#17128 = CARTESIAN_POINT ( 'NONE',  ( 11.08610830971117522, -77.08773842544198374, -1.708745595551396157 ) ) ;
#17129 = CARTESIAN_POINT ( 'NONE',  ( 1.211010829604999950, -77.87558980333969316, -0.5234676170970000708 ) ) ;
#17130 = CARTESIAN_POINT ( 'NONE',  ( 2.798597658857805648, -3.047393581727702916, -2.136609592447876071 ) ) ;
#17131 = EDGE_CURVE ( 'NONE', #1567, #38582, #4216, .T. ) ;
#17132 = CARTESIAN_POINT ( 'NONE',  ( 12.75761570867000039, -22.77819125662999866, 1.931043762602999925 ) ) ;
#17133 = CARTESIAN_POINT ( 'NONE',  ( 2.425729133266999670E-14, -6.000000000000000000, 0.000000000000000000 ) ) ;
#17134 = DIRECTION ( 'NONE',  ( -0.7071067811814920612, -1.249159897326986052E-07, 0.7071067811915919821 ) ) ;
#17135 = DIRECTION ( 'NONE',  ( 0.000000000000000000, 1.000000000000000000, 0.000000000000000000 ) ) ;
#17136 = CARTESIAN_POINT ( 'NONE',  ( 4.711402524194999941, -78.89724708133699949, 10.11406376844000121 ) ) ;
#17137 = CARTESIAN_POINT ( 'NONE',  ( 10.18491080493000212, -18.69283319134000010, -7.640030264154999529 ) ) ;
#17138 = CARTESIAN_POINT ( 'NONE',  ( -7.858171174022000827, -79.08164813617541711, 9.108036400545000077 ) ) ;
#17139 = CARTESIAN_POINT ( 'NONE',  ( 4.160603301095000539, -79.44891918789778629, 0.3097350621069000498 ) ) ;
#17140 = VERTEX_POINT ( 'NONE', #17799 ) ;
#17141 = CARTESIAN_POINT ( 'NONE',  ( -9.096312194199068557, -77.19999999999997442, 6.047136293109013572 ) ) ;
#17142 = CARTESIAN_POINT ( 'NONE',  ( -0.4406873220133000202, -81.61548177752000299, -1.134095991600000186 ) ) ;
#17143 = CARTESIAN_POINT ( 'NONE',  ( 9.250000000000000000, -79.24999999999998579, 0.000000000000000000 ) ) ;
#17144 = CARTESIAN_POINT ( 'NONE',  ( 10.69384760718000038, -78.21110719282100376, -5.399785902169999652 ) ) ;
#17145 = DIRECTION ( 'NONE',  ( 0.000000000000000000, 0.7071067811866525998, -0.7071067811864425456 ) ) ;
#17146 = CARTESIAN_POINT ( 'NONE',  ( -1.588687380433000174, -83.18688350838499446, 0.5002921117598999601 ) ) ;
#17147 = CARTESIAN_POINT ( 'NONE',  ( -11.79984144923200340, -76.38290029571203377, 2.513141340760493669 ) ) ;
#17148 = CARTESIAN_POINT ( 'NONE',  ( 8.384816012895999648, -78.83780194988500511, -4.923277454554000343 ) ) ;
#17149 = CARTESIAN_POINT ( 'NONE',  ( -7.148970245326999873, -78.76537169604299038, -6.453327391511999522 ) ) ;
#17150 = CARTESIAN_POINT ( 'NONE',  ( -1.632307027713000069, -55.13072810409999391, -12.46200249210000166 ) ) ;
#17151 = CARTESIAN_POINT ( 'NONE',  ( 0.000000000000000000, -87.20000000000000284, 0.000000000000000000 ) ) ;
#17152 = CARTESIAN_POINT ( 'NONE',  ( 4.571463104798920263, -85.94828561723799965, 0.5247301960423848000 ) ) ;
#17153 = ORIENTED_EDGE ( 'NONE', *, *, #29293, .T. ) ;
#17154 = EDGE_CURVE ( 'NONE', #22005, #8827, #42524, .T. ) ;
#17155 = CARTESIAN_POINT ( 'NONE',  ( 0.8513654298648299923, -2.247209519113824161, -3.168457469390551395 ) ) ;
#17156 = CARTESIAN_POINT ( 'NONE',  ( 11.89728672164147660, -78.94942626805544705, 0.01537117205770647047 ) ) ;
#17157 = CARTESIAN_POINT ( 'NONE',  ( -3.999289396771888327, -78.67389998729011324, 0.07539443523754257859 ) ) ;
#17158 = B_SPLINE_CURVE_WITH_KNOTS ( 'NONE', 3,
 ( #34264, #38123, #12134, #7702, #33399, #43731, #29546, #25127, #51727, #3283, #21276, #47015, #6833, #24844, #2133, #20136, #38415, #56146, #11279, #15695, #29257, #42859, #56434, #20705, #32375, #44012, #17138, #8566, #30981, #49020, #57574, #22140 ),
 .UNSPECIFIED., .F., .F.,
 ( 4, 1, 1, 1, 1, 1, 1, 1, 1, 1, 1, 1, 1, 1, 1, 1, 1, 1, 1, 1, 1, 1, 1, 1, 1, 1, 1, 1, 1, 4 ),
 ( 0.000000000000000000, 0.001396860765158759038, 0.03786267284115284182, 0.07432848491735072338, 0.1107942969933448096, 0.1472601090695426773, 0.1837259211455369856, 0.2201917332217348533, 0.2566575452977291616, 0.2931233573739268072, 0.3295891694499208935, 0.3660549815259152018, 0.4025207936021130695, 0.4389866056781073778, 0.4754524177543050234, 0.5119182298302993317, 0.5483840419064972549, 0.5848498539824913411, 0.6213156660586891533, 0.6577814781346832396, 0.6942472902108811628, 0.7307131022868754711, 0.7671789143630732832, 0.8036447264390675915, 0.8401105385152655147, 0.8765763505912593789, 0.9130421626674571911, 0.9495079747434516104, 0.9859737868196494226, 1.000000000000000000 ),
 .UNSPECIFIED. ) ;
#17159 = CARTESIAN_POINT ( 'NONE',  ( -0.6514878906251000412, -79.80987778408999134, 10.95625855609000077 ) ) ;
#17160 = CARTESIAN_POINT ( 'NONE',  ( 10.90625000000000000, -80.29374999999798490, -5.301077343649000152E-10 ) ) ;
#17161 = CARTESIAN_POINT ( 'NONE',  ( -1.051549137210000096, -76.55937287232799804, -12.34225577480999902 ) ) ;
#17162 = FACE_OUTER_BOUND ( 'NONE', #26529, .T. ) ;
#17163 = DIRECTION ( 'NONE',  ( -1.000000000000000000, 0.000000000000000000, 0.000000000000000000 ) ) ;
#17164 = ORIENTED_EDGE ( 'NONE', *, *, #16117, .F. ) ;
#17165 = CARTESIAN_POINT ( 'NONE',  ( -8.926133614190998600, -79.65775739383899179, 6.676731181684000482 ) ) ;
#17166 = CARTESIAN_POINT ( 'NONE',  ( -0.007339070148793539611, -79.97594915642548585, 1.249695971876270129 ) ) ;
#17167 = FACE_OUTER_BOUND ( 'NONE', #14693, .T. ) ;
#17168 = B_SPLINE_CURVE_WITH_KNOTS ( 'NONE', 3,
 ( #58317, #17879, #13430, #54188, #13726, #31723, #30562, #14887, #5744, #19045, #37036, #23460, #55050, #23752, #41473, #32592, #45631, #37618 ),
 .UNSPECIFIED., .F., .F.,
 ( 4, 2, 2, 2, 2, 2, 2, 2, 4 ),
 ( 0.000000000000000000, 0.1249999999999999722, 0.2499999999999999445, 0.3749999999999998890, 0.4999999999999998890, 0.6249999999999998890, 0.7499999999999997780, 0.8749999999999998890, 1.000000000000000000 ),
 .UNSPECIFIED. ) ;
#17169 = CARTESIAN_POINT ( 'NONE',  ( 7.439427647571000612, -79.42614197053399039, -8.315438409070999626 ) ) ;
#17170 = CARTESIAN_POINT ( 'NONE',  ( 1.125737367536490563, -76.36666666666664582, 10.74999999999998757 ) ) ;
#17171 = LINE ( 'NONE', #3596, #22797 ) ;
#17172 = CARTESIAN_POINT ( 'NONE',  ( -0.5209265914808703934, -81.44646803115288947, -1.419575930094677751 ) ) ;
#17173 = CARTESIAN_POINT ( 'NONE',  ( 2.284509925729999669, -78.18669951884498914, 12.06552085823000020 ) ) ;
#17174 = VERTEX_POINT ( 'NONE', #23963 ) ;
#17175 = CARTESIAN_POINT ( 'NONE',  ( 9.621742412375313691, -17.37938300089657417, -8.060146969350251211 ) ) ;
#17176 = CARTESIAN_POINT ( 'NONE',  ( 0.000000000000000000, -82.00000000000000000, 0.000000000000000000 ) ) ;
#17177 = PLANE ( 'NONE',  #57261 ) ;
#17178 = VERTEX_POINT ( 'NONE', #36959 ) ;
#17179 = ORIENTED_EDGE ( 'NONE', *, *, #51244, .T. ) ;
#17180 = CARTESIAN_POINT ( 'NONE',  ( 10.74994633437535541, -78.84663129478072108, -0.4671562791492399058 ) ) ;
#17181 = ORIENTED_EDGE ( 'NONE', *, *, #405, .T. ) ;
#17182 = CARTESIAN_POINT ( 'NONE',  ( 0.000000000000000000, -77.49999999999998579, 0.000000000000000000 ) ) ;
#17183 = ORIENTED_EDGE ( 'NONE', *, *, #15692, .T. ) ;
#17184 = CARTESIAN_POINT ( 'NONE',  ( -3.427405331535606781, -81.00000000000000000, -10.36637788387490922 ) ) ;
#17185 = CARTESIAN_POINT ( 'NONE',  ( -9.889498855898999352, -78.10460208417299555, 4.888716273084000363 ) ) ;
#17186 = CARTESIAN_POINT ( 'NONE',  ( 6.559997675027998909, -78.44513998579799363, 7.127949055663999722 ) ) ;
#17187 = CARTESIAN_POINT ( 'NONE',  ( -6.486048890515720089, -78.16333030288288342, -6.594899609276845709 ) ) ;
#17188 = AXIS2_PLACEMENT_3D ( 'NONE', #6130, #55736, #10573 ) ;
#17189 = CARTESIAN_POINT ( 'NONE',  ( -10.39759693597000023, -79.79670861399999637, -4.208097972746998927 ) ) ;
#17190 = VERTEX_POINT ( 'NONE', #41981 ) ;
#17191 = ORIENTED_EDGE ( 'NONE', *, *, #51109, .T. ) ;
#17192 = CARTESIAN_POINT ( 'NONE',  ( -5.470294744961789135, -77.52538948961748133, 7.459090554855953847 ) ) ;
#17193 = DIRECTION ( 'NONE',  ( -1.000000000000000000, 0.000000000000000000, 0.000000000000000000 ) ) ;
#17194 = DIRECTION ( 'NONE',  ( 0.7071067811865475727, 0.000000000000000000, 0.7071067811865475727 ) ) ;
#17195 = CARTESIAN_POINT ( 'NONE',  ( -9.685922776715001348, -77.26497176072199125, 0.5943755449006998814 ) ) ;
#17196 = CARTESIAN_POINT ( 'NONE',  ( 7.655555357453000198, -19.22204592323999961, 10.38646360831000059 ) ) ;
#17197 = EDGE_CURVE ( 'NONE', #47139, #54085, #29085, .T. ) ;
#17198 = CARTESIAN_POINT ( 'NONE',  ( -8.465317046980235460, -79.43746713076286881, -4.311381249254191417 ) ) ;
#17199 = LINE ( 'NONE', #21631, #8197 ) ;
#17200 = CARTESIAN_POINT ( 'NONE',  ( -8.744140569415000286, -80.37595639081598620, 7.086030162020000134 ) ) ;
#17201 = VECTOR ( 'NONE', #34648, 1000.000000000000000 ) ;
#17202 = CARTESIAN_POINT ( 'NONE',  ( 12.65987793663000005, -17.06302453494999583, -0.9847129294438998759 ) ) ;
#17203 = CARTESIAN_POINT ( 'NONE',  ( -10.47513974133999959, -23.80361494181999760, -7.624776006159999397 ) ) ;
#17204 = CARTESIAN_POINT ( 'NONE',  ( -11.44035017613066074, -76.68158408336353205, 2.681016756718579419 ) ) ;
#17205 = ORIENTED_EDGE ( 'NONE', *, *, #5130, .F. ) ;
#17206 = CARTESIAN_POINT ( 'NONE',  ( 11.20573829663000076, -79.79121893549199740, 4.825001155745000325 ) ) ;
#17207 = FACE_OUTER_BOUND ( 'NONE', #23429, .T. ) ;
#17208 = CARTESIAN_POINT ( 'NONE',  ( -1.360213228908000005, -77.81762791332599249, -11.90234785270000017 ) ) ;
#17209 = CARTESIAN_POINT ( 'NONE',  ( -8.485548443539000729, -17.11931586736000455, -9.101490738460999097 ) ) ;
#17211 = CARTESIAN_POINT ( 'NONE',  ( 0.000000000000000000, -7.000000000000000000, 0.000000000000000000 ) ) ;
#17210 = CARTESIAN_POINT ( 'NONE',  ( 7.653559626076999578, -55.50151115525000023, 10.01235002620999914 ) ) ;
#17212 = CARTESIAN_POINT ( 'NONE',  ( 3.647699722741000183, -86.17851881763699851, -1.624060551956000076 ) ) ;
#17213 = CARTESIAN_POINT ( 'NONE',  ( 10.59551070214999946, -57.04351820043999766, -7.678690995233999672 ) ) ;
#17214 = LINE ( 'NONE', #30498, #26698 ) ;
#17215 = CARTESIAN_POINT ( 'NONE',  ( -9.398554024959999253, -78.43631111317900206, -5.993477931829000127 ) ) ;
#17216 = DIRECTION ( 'NONE',  ( 0.000000000000000000, 0.000000000000000000, -1.000000000000000000 ) ) ;
#17217 = CARTESIAN_POINT ( 'NONE',  ( -1.439896632895359962, -80.08541666668128300, 10.99999999999999645 ) ) ;
#17218 = ORIENTED_EDGE ( 'NONE', *, *, #30468, .T. ) ;
#17219 = CARTESIAN_POINT ( 'NONE',  ( 3.113304451009999863, -78.39783470746900207, -10.55022916317000181 ) ) ;
#17220 = ADVANCED_FACE ( 'NONE', ( #36671 ), #22439, .F. ) ;
#17221 = CARTESIAN_POINT ( 'NONE',  ( -1.669849926076999891, -55.42771399551000400, 12.48404299551000030 ) ) ;
#17222 = CARTESIAN_POINT ( 'NONE',  ( -12.58335110166999904, -20.25111654322000021, 1.667961430005999945 ) ) ;
#17223 = CARTESIAN_POINT ( 'NONE',  ( 2.997795270929999756, -2.833281426754000076, -2.074863749804000346 ) ) ;
#17224 = CARTESIAN_POINT ( 'NONE',  ( -6.884807209879999057, -78.27072815847299125, -8.855368954042999619 ) ) ;
#17225 = CARTESIAN_POINT ( 'NONE',  ( -4.784380313523538319, -77.38333333333332575, -8.300970689365453126 ) ) ;
#17226 = FACE_OUTER_BOUND ( 'NONE', #5934, .T. ) ;
#17227 = CARTESIAN_POINT ( 'NONE',  ( 0.5045596072229000528, -61.93528913004999481, 12.66210649714999903 ) ) ;
#17228 = CARTESIAN_POINT ( 'NONE',  ( -0.4254240051736147277, -3.114583333333332593, -3.250000000000000888 ) ) ;
#17229 = CARTESIAN_POINT ( 'NONE',  ( -2.684675547274000262, -83.46474735065199013, -3.197204561977000203 ) ) ;
#17230 = CARTESIAN_POINT ( 'NONE',  ( 2.854661674668000058E-14, -82.00000000000000000, 0.000000000000000000 ) ) ;
#17231 = EDGE_CURVE ( 'NONE', #33530, #40010, #21385, .T. ) ;
#17232 = CARTESIAN_POINT ( 'NONE',  ( -3.838255874262739731, -77.05221981673027187, -11.44667041316091272 ) ) ;
#17233 = EDGE_CURVE ( 'NONE', #49594, #37512, #56726, .T. ) ;
#17234 = B_SPLINE_SURFACE_WITH_KNOTS ( 'NONE', 3, 3, ( 
 ( #50996, #9664, #10544, #14954, #28231, #5234, #50707, #51289, #14658, #46283, #55114, #23525, #55408, #24112, #33247, #55706, #5807, #4943, #9960, #23814, #23239, #45400, #41833, #1695, #37389, #27653, #28528, #46577, #40958, #10844, #45989, #19107, #54827, #549, #18526 ),
 ( #36518, #14368, #50410, #27941, #1119, #37098, #2846, #15548, #52154, #43579, #11140, #2278, #3142, #15841, #33829, #56865, #16424, #51867, #11421, #35566, #21994, #58315, #13426, #21424, #57720, #39714, #31428, #4592, #7847, #25847, #51144, #52582, #57003, #21274, #39282 ),
 ( #57292, #15985, #33975, #49018, #54036, #26854, #49312, #22435, #39852, #8862, #36307, #44885, #31566, #13575, #36011, #31866, #4734, #53742, #49908, #9743, #40743, #17725, #18610, #54332, #40450, #8564, #45184, #35713, #27441, #4435, #13872, #53439, #26554, #49615, #42 ),
 ( #13278, #32156, #9455, #627, #18018, #40147, #45477, #5020, #31270, #9162, #35408, #21845, #12981, #57868, #18316, #22732, #30979, #23024, #41036, #58159, #36598, #27143, #54622, #336, #17421, #14158, #27731, #50195, #45775, #44583, #4140, #22138, #55488, #23891, #32735 ) ),
 .UNSPECIFIED., .F., .F., .F.,
 ( 4, 4 ),
 ( 4, 1, 1, 1, 1, 1, 1, 1, 1, 1, 1, 1, 1, 1, 1, 1, 1, 1, 1, 1, 1, 1, 1, 1, 1, 1, 1, 1, 1, 1, 1, 1, 4 ),
 ( -0.1377334280162000046, 1.137733428016000081 ),
 ( -0.01298507462686999958, 0.008115671641791000201, 0.02921641791044999811, 0.05031716417909999628, 0.07141791044776001074, 0.09251865671641999744, 0.1136194029850999959, 0.1347201492536999889, 0.1558208955223999992, 0.1769216417910000061, 0.1980223880596999886, 0.2191231343283999988, 0.2402238805970000057, 0.2613246268657000160, 0.2824253731342999951, 0.3035261194030000054, 0.3246268656715999845, 0.3457276119402999948, 0.3668283582090000050, 0.3879291044776000397, 0.4090298507462999944, 0.4301305970149000291, 0.4512313432835999838, 0.4723320895522000185, 0.4934328358209000287, 0.5145335820895999834, 0.5356343283582000181, 0.5567350746268999728, 0.5778358208955000075, 0.5989365671641999622, 0.6200373134327999969, 0.6411380597014999516, 0.6622388059702000174 ),
 .UNSPECIFIED. ) ;
#17235 = CARTESIAN_POINT ( 'NONE',  ( -11.18527010467000160, -78.26729255600099577, 1.312896411821999898 ) ) ;
#17236 = CARTESIAN_POINT ( 'NONE',  ( -1.500000000000000000, -81.40000000000000568, 0.000000000000000000 ) ) ;
#17237 = CARTESIAN_POINT ( 'NONE',  ( 0.3690512077139999625, -78.03748392311000259, -1.504494153444999816 ) ) ;
#17238 = CARTESIAN_POINT ( 'NONE',  ( 2.632967082928999947, -77.12290855547149704, 9.306700570505000769 ) ) ;
#17239 = CARTESIAN_POINT ( 'NONE',  ( 0.9042486337774866545, -82.92610658917844546, -1.210803591118944089 ) ) ;
#17240 = CARTESIAN_POINT ( 'NONE',  ( -12.79895559718999998, -60.60469146232000526, 2.015913954445999856 ) ) ;
#17241 = CARTESIAN_POINT ( 'NONE',  ( 3.041187196987005681, -80.24796802560094022, -10.31335799952287502 ) ) ;
#17242 = CARTESIAN_POINT ( 'NONE',  ( -12.50000000000000000, -24.68359816828999698, -1.003641515615000035 ) ) ;
#17243 = CARTESIAN_POINT ( 'NONE',  ( -7.764220096252848258, -17.74399029336390754, -10.21028322255594389 ) ) ;
#17244 = AXIS2_PLACEMENT_3D ( 'NONE', #57026, #12155, #39302 ) ;
#17245 = B_SPLINE_CURVE_WITH_KNOTS ( 'NONE', 3,
 ( #30812, #27554, #18432, #13985, #44705, #36134, #26385, #13394, #5141, #22849 ),
 .UNSPECIFIED., .F., .F.,
 ( 4, 2, 2, 2, 4 ),
 ( 0.000000000000000000, 0.2500000000000000555, 0.5000000000000001110, 0.7500000000000002220, 1.000000000000000000 ),
 .UNSPECIFIED. ) ;
#17246 = CIRCLE ( 'NONE', #55915, 10.50000000000000000 ) ;
#17247 = CARTESIAN_POINT ( 'NONE',  ( -3.970056213021999625, -78.90008180218299572, 11.35542513096999961 ) ) ;
#17248 = CARTESIAN_POINT ( 'NONE',  ( 5.645478026989999343, -79.99019400902760424, -9.744872608167998607 ) ) ;
#17249 = CARTESIAN_POINT ( 'NONE',  ( -9.392738704232332481, -77.55834533578540402, 5.413616812572119130 ) ) ;
#17250 = VERTEX_POINT ( 'NONE', #15696 ) ;
#17251 = CARTESIAN_POINT ( 'NONE',  ( -1.782734487917835953, -24.12245368560020253, 12.71547286926173825 ) ) ;
#17252 = VERTEX_POINT ( 'NONE', #25420 ) ;
#17253 = CARTESIAN_POINT ( 'NONE',  ( 0.000000000000000000, -2.660000000000000142, 0.000000000000000000 ) ) ;
#17254 = ORIENTED_EDGE ( 'NONE', *, *, #17538, .F. ) ;
#17255 = DIRECTION ( 'NONE',  ( -1.000000000000000000, 0.000000000000000000, 0.000000000000000000 ) ) ;
#17256 = CARTESIAN_POINT ( 'NONE',  ( 0.1493788696755103118, -79.08541666236438061, -3.407719317120471825 ) ) ;
#17257 = CARTESIAN_POINT ( 'NONE',  ( 3.413317904202999742, -78.92310371897299603, 10.36940822202999790 ) ) ;
#17258 = CARTESIAN_POINT ( 'NONE',  ( -6.043427764450786555, -76.38333333329933339, -10.48543666025110177 ) ) ;
#17259 = CARTESIAN_POINT ( 'NONE',  ( -3.037813758603999936, -79.17120297221410397, -2.545166726939000146 ) ) ;
#17260 = CARTESIAN_POINT ( 'NONE',  ( -4.205654323444776743, -79.31107025363671426, 8.523780649771993012 ) ) ;
#17261 = ORIENTED_EDGE ( 'NONE', *, *, #46258, .T. ) ;
#17262 = LINE ( 'NONE', #12829, #21234 ) ;
#17263 = CARTESIAN_POINT ( 'NONE',  ( 3.109857617603999813, -79.15086356186999694, -11.96079293226000040 ) ) ;
#17264 = VERTEX_POINT ( 'NONE', #24555 ) ;
#17265 = ORIENTED_EDGE ( 'NONE', *, *, #7349, .F. ) ;
#17266 = CARTESIAN_POINT ( 'NONE',  ( 0.000000000000000000, -75.10000000032299283, 0.000000000000000000 ) ) ;
#17267 = CARTESIAN_POINT ( 'NONE',  ( -1.500000000000000000, -83.24999999999998579, 0.000000000000000000 ) ) ;
#17268 = PRODUCT_DEFINITION_SHAPE ( 'NONE', 'NONE',  #10957 ) ;
#17269 = CARTESIAN_POINT ( 'NONE',  ( -0.9565643533716999825, -80.20431228332999751, 0.9292797142584000580 ) ) ;
#17270 = DIRECTION ( 'NONE',  ( -0.7071067811865475727, 0.000000000000000000, 0.7071067811865475727 ) ) ;
#17271 = CARTESIAN_POINT ( 'NONE',  ( -1.658366784370784108, -86.17851881763698429, -3.632231483840216768 ) ) ;
#17272 = CARTESIAN_POINT ( 'NONE',  ( 3.401880147206532978, -85.81571308423876587, 1.208734972710103328 ) ) ;
#17273 = CARTESIAN_POINT ( 'NONE',  ( -10.72428337452000058, -76.95682288379001079, 7.546888592172999566 ) ) ;
#17274 = CARTESIAN_POINT ( 'NONE',  ( 11.48986902082000050, -77.02860818038000446, 5.271442771914999881 ) ) ;
#17275 = VECTOR ( 'NONE', #15475, 1000.000000000000114 ) ;
#17276 = CARTESIAN_POINT ( 'NONE',  ( 7.936766385091000409, -76.33656526534099385, 7.448366782227999749 ) ) ;
#17277 = DIRECTION ( 'NONE',  ( 0.000000000000000000, -1.000000000000000000, 0.000000000000000000 ) ) ;
#17278 = CARTESIAN_POINT ( 'NONE',  ( 4.118797911448999649, -79.65606415136248586, 0.3066228704314999942 ) ) ;
#17279 = DIRECTION ( 'NONE',  ( -0.7071067811865475727, 0.000000000000000000, 0.7071067811865475727 ) ) ;
#17280 = CARTESIAN_POINT ( 'NONE',  ( -0.007828081787127551261, -2.975669492385137449, 3.249705167704726172 ) ) ;
#17281 = CARTESIAN_POINT ( 'NONE',  ( 3.423421051771000201, -82.28567549782599144, 0.3453239421332999770 ) ) ;
#17282 = VECTOR ( 'NONE', #56600, 1000.000000000000000 ) ;
#17283 = DIRECTION ( 'NONE',  ( 0.000000000000000000, -1.000000000000000000, 0.000000000000000000 ) ) ;
#17284 = CARTESIAN_POINT ( 'NONE',  ( -0.8698067890798458768, -80.98156680119757311, 10.71467698395598767 ) ) ;
#17285 = CARTESIAN_POINT ( 'NONE',  ( 1.618170588614999961, -80.47036452348720559, -11.14857479085000058 ) ) ;
#17286 = CARTESIAN_POINT ( 'NONE',  ( 3.594201416108000036, -3.059342895222999736, 1.252117639952999850 ) ) ;
#17287 = CARTESIAN_POINT ( 'NONE',  ( -0.8489568036168347875, -79.81738908755133366, -0.9503365090294664252 ) ) ;
#17288 = TOROIDAL_SURFACE ( 'NONE', #3968, 13.50000000000000000, 0.5000000000000000000 ) ;
#17289 = ORIENTED_EDGE ( 'NONE', *, *, #43887, .F. ) ;
#17290 = DIRECTION ( 'NONE',  ( 0.000000000000000000, 0.000000000000000000, 1.000000000000000000 ) ) ;
#17291 = EDGE_CURVE ( 'NONE', #29449, #185, #2719, .T. ) ;
#17292 = DIRECTION ( 'NONE',  ( 1.000000000000000000, 6.386283326366000088E-09, -1.411431172417000032E-10 ) ) ;
#17293 = CARTESIAN_POINT ( 'NONE',  ( -0.1187445621502999926, -81.33979215996299672, -1.328335755224000048 ) ) ;
#17294 = EDGE_CURVE ( 'NONE', #51311, #22854, #48172, .T. ) ;
#17295 = CARTESIAN_POINT ( 'NONE',  ( -12.59651451717999926, -18.60944962361000066, -1.801708894189000043 ) ) ;
#17296 = CARTESIAN_POINT ( 'NONE',  ( -9.287618194362000423, -77.61375265978000471, -9.114789584104999065 ) ) ;
#17297 = BREP_WITH_VOIDS ( 'NONE', #3218, ( #32916 ) );
#17298 = DIRECTION ( 'NONE',  ( -0.9999548435846228323, 0.000000000000000000, -0.009503199022040118363 ) ) ;
#17299 = CARTESIAN_POINT ( 'NONE',  ( 10.11462645681450034, -18.61287635839325461, 7.639895286233333138 ) ) ;
#17300 = ORIENTED_EDGE ( 'NONE', *, *, #29220, .F. ) ;
#17301 = CARTESIAN_POINT ( 'NONE',  ( -4.454457568640999732, -80.65734865577489643, 10.34731867136000005 ) ) ;
#17302 = CARTESIAN_POINT ( 'NONE',  ( -9.469606800734000629, -79.65752053325199711, 5.597012331546999953 ) ) ;
#17303 = ADVANCED_FACE ( 'NONE', ( #25705 ), #1759, .F. ) ;
#17304 = CARTESIAN_POINT ( 'NONE',  ( -1.107301413750000130, -80.78176359222798908, -0.6019302607798000526 ) ) ;
#17305 = CARTESIAN_POINT ( 'NONE',  ( 7.627487525417000036, -18.70221245812999911, -10.35845608625999859 ) ) ;
#17306 = CARTESIAN_POINT ( 'NONE',  ( 9.511010664898998712, -78.15562873964798030, 1.514558053418999961 ) ) ;
#17307 = CARTESIAN_POINT ( 'NONE',  ( -3.902769136194000232, -86.15275002252400327, 1.102018856806000091 ) ) ;
#17308 = CARTESIAN_POINT ( 'NONE',  ( 1.773208520488963824, -79.96215963365355606, 10.60254057701149577 ) ) ;
#17309 = CARTESIAN_POINT ( 'NONE',  ( 1.493900225960000050, -80.28364115338500540, -0.2592381030950999810 ) ) ;
#17310 = VERTEX_POINT ( 'NONE', #43433 ) ;
#17311 = CARTESIAN_POINT ( 'NONE',  ( -4.643650396336004960, -77.18947228263908755, -9.695312717224595644 ) ) ;
#17312 = CARTESIAN_POINT ( 'NONE',  ( -6.760013919724074505, -78.77291666666668846, -8.796335266379974982 ) ) ;
#17313 = CARTESIAN_POINT ( 'NONE',  ( -3.621447497675031268, -78.99318692614360771, 7.242894995350018128 ) ) ;
#17314 = ORIENTED_EDGE ( 'NONE', *, *, #48689, .F. ) ;
#17315 = ORIENTED_EDGE ( 'NONE', *, *, #29008, .F. ) ;
#17316 = CARTESIAN_POINT ( 'NONE',  ( 9.295311691678000088, -79.60238712864799027, 5.972861453165999812 ) ) ;
#17317 = VECTOR ( 'NONE', #18567, 1000.000000000000227 ) ;
#17318 = LINE ( 'NONE', #56907, #37822 ) ;
#17319 = CARTESIAN_POINT ( 'NONE',  ( 7.094168877687000219, -80.19133504314000049, 8.690698855587999816 ) ) ;
#17320 = ORIENTED_EDGE ( 'NONE', *, *, #31993, .F. ) ;
#17321 = CARTESIAN_POINT ( 'NONE',  ( -7.278283919121999901, -77.68490340765200131, 9.747261860606000639 ) ) ;
#17322 = ORIENTED_EDGE ( 'NONE', *, *, #56415, .F. ) ;
#17323 = ORIENTED_EDGE ( 'NONE', *, *, #36384, .T. ) ;
#17324 = CIRCLE ( 'NONE', #10743, 1.000000000000000000 ) ;
#17325 = CARTESIAN_POINT ( 'NONE',  ( 3.077458782618233357, -78.05205802293652084, 11.44329248034590485 ) ) ;
#17326 = CARTESIAN_POINT ( 'NONE',  ( -7.479908383216000267, -79.80559761149552855, -6.281056869080000382 ) ) ;
#17327 = VERTEX_POINT ( 'NONE', #56147 ) ;
#17328 = CARTESIAN_POINT ( 'NONE',  ( 1.151164884410004641, -82.06119791428943699, -0.8836085541159298673 ) ) ;
#17329 = ORIENTED_EDGE ( 'NONE', *, *, #39977, .T. ) ;
#17330 = CARTESIAN_POINT ( 'NONE',  ( 0.2301609875668271243, -80.28964598758351201, -1.253928556708755915 ) ) ;
#17331 = CARTESIAN_POINT ( 'NONE',  ( -2.042798770927879648, -78.77851879815550262, -3.387993206663126866 ) ) ;
#17332 = EDGE_CURVE ( 'NONE', #48463, #37820, #54549, .T. ) ;
#17333 = CARTESIAN_POINT ( 'NONE',  ( 9.422860735104000796, -53.54048607621999878, 8.643926020445999114 ) ) ;
#17334 = CARTESIAN_POINT ( 'NONE',  ( -7.678690995240000206, -20.24351820077000141, -10.59551070215999857 ) ) ;
#17335 = CARTESIAN_POINT ( 'NONE',  ( 7.545211988112344947, -79.56380208332930692, 5.799587082756866963 ) ) ;
#17336 = CARTESIAN_POINT ( 'NONE',  ( -1.814796094202807186, -80.23779093740807866, 11.06304992301285672 ) ) ;
#17337 = AXIS2_PLACEMENT_3D ( 'NONE', #33383, #51710, #20969 ) ;
#17338 = CARTESIAN_POINT ( 'NONE',  ( -1.360213228908000227, -77.76594546010713316, -11.90234785270000195 ) ) ;
#17339 = CARTESIAN_POINT ( 'NONE',  ( -10.14948852604999985, -19.24899164588000389, -7.674614791898999755 ) ) ;
#17340 = DIRECTION ( 'NONE',  ( -1.000000000000000000, 0.000000000000000000, 0.000000000000000000 ) ) ;
#17341 = CARTESIAN_POINT ( 'NONE',  ( -0.7554284705563483193, -79.98333333333333428, -1.310679582531387721 ) ) ;
#17342 = VECTOR ( 'NONE', #38793, 1000.000000000000000 ) ;
#17343 = CARTESIAN_POINT ( 'NONE',  ( -3.973290944682999370, -78.47775883115959061, 0.5746058003935000658 ) ) ;
#17344 = CARTESIAN_POINT ( 'NONE',  ( 5.915537232129000067, -77.08008667140099135, 7.766375951189000482 ) ) ;
#17345 = CARTESIAN_POINT ( 'NONE',  ( -4.099999999699000419, -75.20000000030088927, 8.298667500436000154E-10 ) ) ;
#17346 = B_SPLINE_CURVE_WITH_KNOTS ( 'NONE', 3,
 ( #9933, #4630, #27912, #58353, #45962, #17915, #31760, #31166, #35604, #22032 ),
 .UNSPECIFIED., .F., .F.,
 ( 4, 2, 2, 2, 4 ),
 ( 0.5000000051225159670, 0.6250000038418869197, 0.7500000025612578725, 0.8750000012806289362, 1.000000000000000000 ),
 .UNSPECIFIED. ) ;
#17347 = DIRECTION ( 'NONE',  ( -1.000000000000000000, 0.000000000000000000, 0.000000000000000000 ) ) ;
#17348 = CARTESIAN_POINT ( 'NONE',  ( -2.019183793707000074, -23.78720277242999970, 12.79944116704999857 ) ) ;
#17349 = DIRECTION ( 'NONE',  ( 0.000000000000000000, -1.000000000000000000, 1.543800620547000024E-14 ) ) ;
#17350 = EDGE_CURVE ( 'NONE', #22602, #20949, #35432, .T. ) ;
#17351 = CARTESIAN_POINT ( 'NONE',  ( 8.857115352654000517, -79.36940095943376150, -3.584237475251999872 ) ) ;
#17352 = CIRCLE ( 'NONE', #30541, 1.000000000000000000 ) ;
#17354 = ADVANCED_FACE ( 'NONE', ( #47016 ), #20992, .F. ) ;
#17353 = CARTESIAN_POINT ( 'NONE',  ( -1.217210213920586703, -80.89993084598471285, -0.8960687109477767365 ) ) ;
#17355 = CARTESIAN_POINT ( 'NONE',  ( 12.46083365857999858, -60.48341615446999953, -1.628972628240000109 ) ) ;
#17356 = CARTESIAN_POINT ( 'NONE',  ( -1.140592747978000032, -79.46513063462899140, -0.9947442812858000583 ) ) ;
#17357 = B_SPLINE_CURVE_WITH_KNOTS ( 'NONE', 3,
 ( #52536, #39237, #44541, #57249, #52822, #12377, #30655, #48408, #3521, #57534, #17093, #44252, #55154, #18575, #46034, #14701, #41289, #1161 ),
 .UNSPECIFIED., .F., .F.,
 ( 4, 2, 2, 2, 2, 2, 2, 2, 4 ),
 ( 0.000000000000000000, 0.1250000000000000000, 0.2500000000000000000, 0.3750000000000000000, 0.5000000000000000000, 0.6250000000000000000, 0.7500000000000000000, 0.8750000000000000000, 1.000000000000000000 ),
 .UNSPECIFIED. ) ;
#17358 = CARTESIAN_POINT ( 'NONE',  ( 0.000000000000000000, -77.04999999999999716, 0.000000000000000000 ) ) ;
#17359 = VECTOR ( 'NONE', #55216, 1000.000000000000000 ) ;
#17360 = CARTESIAN_POINT ( 'NONE',  ( -10.87089293717000160, -77.01929369090099442, 0.9996073426339999735 ) ) ;
#17361 = CARTESIAN_POINT ( 'NONE',  ( 6.544501642745999881, -77.61134018205299867, -10.25436633016999899 ) ) ;
#17362 = DIRECTION ( 'NONE',  ( 0.07798810297687770732, 0.04890180918248850789, 0.9957542211071702676 ) ) ;
#17364 = CARTESIAN_POINT ( 'NONE',  ( 1.211010829604999950, -77.95947474015589762, -0.5234676170970000708 ) ) ;
#17363 = DIRECTION ( 'NONE',  ( -1.000000000000000000, 0.000000000000000000, 0.000000000000000000 ) ) ;
#17365 = CARTESIAN_POINT ( 'NONE',  ( 0.6237791458550000501, -82.80325357425300581, -1.329415719495999904 ) ) ;
#17366 = CARTESIAN_POINT ( 'NONE',  ( -3.728013830608571055, -79.50331027668923412, 10.08280175580265059 ) ) ;
#17367 = ORIENTED_EDGE ( 'NONE', *, *, #25909, .F. ) ;
#17368 = CARTESIAN_POINT ( 'NONE',  ( -10.59548767699999949, -20.24263462181000151, -7.678667886068000215 ) ) ;
#17369 = CARTESIAN_POINT ( 'NONE',  ( -11.50904265702000018, -79.23277905684599887, 3.913699539746000156 ) ) ;
#17370 = CARTESIAN_POINT ( 'NONE',  ( -7.325508896758000432, -80.57304051666800149, 8.435678689013998977 ) ) ;
#17371 = EDGE_CURVE ( 'NONE', #35060, #56888, #36191, .T. ) ;
#17372 = CARTESIAN_POINT ( 'NONE',  ( 0.9463392500275673580, -79.76874999999999716, 11.99969609698326778 ) ) ;
#17373 = CARTESIAN_POINT ( 'NONE',  ( -10.00844230538000090, -60.16891112520000462, 7.647097279411999793 ) ) ;
#17374 = CARTESIAN_POINT ( 'NONE',  ( -3.536550279337999925, -1.729884069545000180, -0.5317485034389000109 ) ) ;
#17375 = CARTESIAN_POINT ( 'NONE',  ( 3.221881332551000288, -80.05522572818799176, 9.234895928605999060 ) ) ;
#17376 = CARTESIAN_POINT ( 'NONE',  ( 12.72554383680000001, -23.20159311629000243, -1.930239506950999884 ) ) ;
#17377 = CARTESIAN_POINT ( 'NONE',  ( -1.667936697358999965, -56.03537109808000594, 12.53241208775000004 ) ) ;
#17378 = VERTEX_POINT ( 'NONE', #33976 ) ;
#17379 = CARTESIAN_POINT ( 'NONE',  ( -12.71536175399154800, -54.67444297150642285, 1.781227265964418827 ) ) ;
#17380 = CARTESIAN_POINT ( 'NONE',  ( 9.546819346421999697, -24.68527546640000025, -8.130850183241999929 ) ) ;
#17381 = CARTESIAN_POINT ( 'NONE',  ( 0.000000000000000000, -77.50000000000000000, 0.000000000000000000 ) ) ;
#17382 = CARTESIAN_POINT ( 'NONE',  ( -10.04116292117000064, -59.56462890159999546, -7.682344222584999827 ) ) ;
#17383 = CARTESIAN_POINT ( 'NONE',  ( 3.547276804185000021, -85.43367953870898646, 0.03714848770851999354 ) ) ;
#17384 = AXIS2_PLACEMENT_3D ( 'NONE', #31872, #54338, #13877 ) ;
#17385 = ORIENTED_EDGE ( 'NONE', *, *, #2465, .T. ) ;
#17386 = CARTESIAN_POINT ( 'NONE',  ( 7.601397897754999633, -18.75000000000000000, -9.369164850722000892 ) ) ;
#17387 = CARTESIAN_POINT ( 'NONE',  ( -10.26031322985315697, -77.74064956233091550, -5.914412738676674053 ) ) ;
#17388 = CARTESIAN_POINT ( 'NONE',  ( 0.000000000000000000, -83.49999999999998579, 0.000000000000000000 ) ) ;
#17389 = EDGE_LOOP ( 'NONE', ( #1392, #20108, #4861, #47425, #35985 ) ) ;
#17390 = CARTESIAN_POINT ( 'NONE',  ( -12.75763395697999947, -59.57795407677000554, 1.931043742978000077 ) ) ;
#17391 = CARTESIAN_POINT ( 'NONE',  ( -9.317995624384998621, -53.66762134137999851, -8.588852713974999276 ) ) ;
#17392 = APPLICATION_PROTOCOL_DEFINITION ( 'draft international standard', 'automotive_design', 1998, #29998 ) ;
#17393 = CARTESIAN_POINT ( 'NONE',  ( -5.726462542197000793, -79.90529868759999488, -7.912542777261000637 ) ) ;
#17394 = ORIENTED_EDGE ( 'NONE', *, *, #30558, .F. ) ;
#17395 = ORIENTED_EDGE ( 'NONE', *, *, #54871, .T. ) ;
#17396 = CARTESIAN_POINT ( 'NONE',  ( 9.461695017160998589, -76.88557108724299383, -7.941295693778001485 ) ) ;
#17397 = CARTESIAN_POINT ( 'NONE',  ( 0.000000000000000000, -74.64999999999999147, 0.000000000000000000 ) ) ;
#17398 = EDGE_LOOP ( 'NONE', ( #11173, #43551, #35968, #6676, #24777 ) ) ;
#17399 = CARTESIAN_POINT ( 'NONE',  ( 12.54238271617994371, -18.47146427654176293, 1.749799002660173519 ) ) ;
#17400 = ADVANCED_FACE ( 'NONE', ( #51728 ), #34265, .T. ) ;
#17401 = CARTESIAN_POINT ( 'NONE',  ( 9.051220798599112882, -77.62926713907424414, 3.499889976320043061 ) ) ;
#17402 = CARTESIAN_POINT ( 'NONE',  ( 0.8868875279287172786, -80.28835734964251003, -0.8803813265097053531 ) ) ;
#17403 = CARTESIAN_POINT ( 'NONE',  ( 11.83733200052000178, -78.36477256742000463, 5.266624269285999915 ) ) ;
#17404 = PRODUCT_DEFINITION_CONTEXT ( 'detailed design', #33019, 'design' ) ;
#17405 = EDGE_CURVE ( 'NONE', #900, #13233, #11856, .T. ) ;
#17406 = CARTESIAN_POINT ( 'NONE',  ( -10.96060824219999930, -77.23295765248289513, 2.383941600041999731 ) ) ;
#17407 = CARTESIAN_POINT ( 'NONE',  ( 12.99510751537000353, -26.30294702886003222, 6.911973076623003642 ) ) ;
#17408 = CARTESIAN_POINT ( 'NONE',  ( -2.503178322334999262, -86.39318692614398287, 3.378898422409667202 ) ) ;
#17409 = CARTESIAN_POINT ( 'NONE',  ( -11.04065564778000130, -79.38755886051600896, 1.980412446595999798 ) ) ;
#17410 = CARTESIAN_POINT ( 'NONE',  ( 3.532511455861872651, -79.94390816463113936, 8.548848039690394529 ) ) ;
#17411 = CARTESIAN_POINT ( 'NONE',  ( 10.04568514501610998, -17.44913840260318949, 7.921286339712268365 ) ) ;
#17412 = ORIENTED_EDGE ( 'NONE', *, *, #11201, .T. ) ;
#17413 = CARTESIAN_POINT ( 'NONE',  ( -10.93895610016999953, -79.10158459378298801, 2.695955081989000135 ) ) ;
#17414 = CARTESIAN_POINT ( 'NONE',  ( -11.91862232004000077, -76.03188042556000426, 3.079279237876999531 ) ) ;
#17415 = CYLINDRICAL_SURFACE ( 'NONE', #18334, 1.250000000000000000 ) ;
#17416 = CARTESIAN_POINT ( 'NONE',  ( 0.9591145717409618188, -2.996237724664126301, -3.388105781299149744 ) ) ;
#17417 = CARTESIAN_POINT ( 'NONE',  ( 12.80900240957999969, -20.24634220924000161, 1.930989144707000005 ) ) ;
#17418 = CARTESIAN_POINT ( 'NONE',  ( -12.87024489160000051, -19.21538333566000034, -2.062597265787999845 ) ) ;
#17419 = CARTESIAN_POINT ( 'NONE',  ( 3.000000000000000000, -80.79999999999999716, 0.000000000000000000 ) ) ;
#17420 = CARTESIAN_POINT ( 'NONE',  ( 10.73159385090000129, -78.78487766400598957, -3.053603293876000269 ) ) ;
#17421 = CARTESIAN_POINT ( 'NONE',  ( 6.848349084398000386, -77.06641498579800498, -6.921892615137999805 ) ) ;
#17422 = CARTESIAN_POINT ( 'NONE',  ( 10.53101998747000145, -18.69360374348000065, -7.613962827178999859 ) ) ;
#17423 = CARTESIAN_POINT ( 'NONE',  ( -1.154999620367486157, -83.06888870240290146, 0.4778175114515754163 ) ) ;
#17424 = CARTESIAN_POINT ( 'NONE',  ( -10.71602610194999805, -79.72613058880257597, 3.314346869870000489 ) ) ;
#17425 = AXIS2_PLACEMENT_3D ( 'NONE', #30630, #34189, #43085 ) ;
#17426 = ORIENTED_EDGE ( 'NONE', *, *, #36998, .F. ) ;
#17427 = CARTESIAN_POINT ( 'NONE',  ( 0.000000000000000000, -80.70000000003399521, 0.000000000000000000 ) ) ;
#17429 = EDGE_CURVE ( 'NONE', #47573, #53816, #56590, .T. ) ;
#17428 = CARTESIAN_POINT ( 'NONE',  ( -1.407332420019999919, -81.97970439103998785, -0.4193609517060999936 ) ) ;
#17430 = VECTOR ( 'NONE', #23879, 1000.000000000000000 ) ;
#17431 = CARTESIAN_POINT ( 'NONE',  ( 1.401632346086000069, -80.60461938843998553, -0.7415008327037999614 ) ) ;
#17432 = DIRECTION ( 'NONE',  ( 0.000000000000000000, 1.000000000000000000, 0.000000000000000000 ) ) ;
#17433 = CARTESIAN_POINT ( 'NONE',  ( -1.360213228908000005, -77.61426225349798358, -11.90234785270000017 ) ) ;
#17434 = CARTESIAN_POINT ( 'NONE',  ( 4.837913609831387518, -77.00000000000001421, 7.928126058622019023 ) ) ;
#17435 = CARTESIAN_POINT ( 'NONE',  ( -0.6622445160018815002, -78.83150205867622162, -1.088607957794830217 ) ) ;
#17436 = CARTESIAN_POINT ( 'NONE',  ( 9.113984702984998520, -77.88244088799798703, 7.705244011730999709 ) ) ;
#17437 = CARTESIAN_POINT ( 'NONE',  ( 9.722066209057999231, -78.88135194988498711, 0.1588365413100999990 ) ) ;
#17438 = CARTESIAN_POINT ( 'NONE',  ( -1.466594960164999906, -54.71841800914999965, -12.44238958329999889 ) ) ;
#17439 = DIRECTION ( 'NONE',  ( 1.000000000000000000, 0.000000000000000000, 0.000000000000000000 ) ) ;
#17440 = CARTESIAN_POINT ( 'NONE',  ( -2.705739474708930281, -85.88547955769999476, 3.652324231546577149 ) ) ;
#17441 = ORIENTED_EDGE ( 'NONE', *, *, #44862, .F. ) ;
#17442 = CARTESIAN_POINT ( 'NONE',  ( -2.370458031814262512, -78.19500000000000739, 9.242975026304344865 ) ) ;
#17443 = CARTESIAN_POINT ( 'NONE',  ( 12.50000000000000000, -65.72928575305999743, 0.000000000000000000 ) ) ;
#17444 = CARTESIAN_POINT ( 'NONE',  ( 2.262521961001000115, -79.96634689244729088, -12.06088927786000120 ) ) ;
#17445 = CARTESIAN_POINT ( 'NONE',  ( -3.620804144604786057, -78.40681307385639798, 0.06825924720741134710 ) ) ;
#17446 = EDGE_CURVE ( 'NONE', #29475, #19884, #3624, .T. ) ;
#17447 = CARTESIAN_POINT ( 'NONE',  ( -0.6572886123566999972, -82.73688322013099139, 1.530761476772000140 ) ) ;
#17448 = CARTESIAN_POINT ( 'NONE',  ( 7.218984044805000444, -79.24803069743599337, 8.267423174273998754 ) ) ;
#17449 = EDGE_CURVE ( 'NONE', #33741, #15471, #30983, .T. ) ;
#17450 = CARTESIAN_POINT ( 'NONE',  ( 1.003693376009467508, -17.03776007890333943, 12.70247752664556273 ) ) ;
#17451 = CARTESIAN_POINT ( 'NONE',  ( 9.353092632424999664, -76.74803656385299178, 8.121372504915999713 ) ) ;
#17452 = CARTESIAN_POINT ( 'NONE',  ( -11.00000000000000000, -79.69999999999998863, 0.000000000000000000 ) ) ;
#17453 = DIRECTION ( 'NONE',  ( -1.000000000000000000, 0.000000000000000000, 0.000000000000000000 ) ) ;
#17454 = EDGE_LOOP ( 'NONE', ( #45741, #40268, #22342, #33451, #42630 ) ) ;
#17455 = CARTESIAN_POINT ( 'NONE',  ( 11.14495853502000067, -79.95735716685899774, -0.2109943715695999922 ) ) ;
#17456 = CARTESIAN_POINT ( 'NONE',  ( 0.9801167568178164036, -79.90410533936980642, 0.7793211621830089531 ) ) ;
#17457 = DIRECTION ( 'NONE',  ( 0.000000000000000000, 0.000000000000000000, -1.000000000000000000 ) ) ;
#17458 = CARTESIAN_POINT ( 'NONE',  ( -0.6622892437428999912, -79.62278845086298418, 11.13790800686000004 ) ) ;
#17459 = CARTESIAN_POINT ( 'NONE',  ( -12.50745077485999879, -53.80005551680000053, 2.011910316382000212E-09 ) ) ;
#17460 = CARTESIAN_POINT ( 'NONE',  ( -11.00000000000000000, -23.74999999999999645, 0.1604995627986234297 ) ) ;
#17461 = CARTESIAN_POINT ( 'NONE',  ( -7.806617969149999503, -78.75641514274398958, 9.479055599837000301 ) ) ;
#17462 = ORIENTED_EDGE ( 'NONE', *, *, #13710, .F. ) ;
#17463 = ADVANCED_FACE ( 'NONE', ( #39574 ), #26859, .T. ) ;
#17464 = DIRECTION ( 'NONE',  ( -1.000000000000000000, 0.000000000000000000, 0.000000000000000000 ) ) ;
#17465 = CARTESIAN_POINT ( 'NONE',  ( 0.000000000000000000, -75.15999999999999659, 0.000000000000000000 ) ) ;
#17466 = CARTESIAN_POINT ( 'NONE',  ( -10.47020627418440242, -78.47916666666667140, 2.813789756862221214 ) ) ;
#17467 = CIRCLE ( 'NONE', #2403, 0.8000000000000000444 ) ;
#17468 = FACE_OUTER_BOUND ( 'NONE', #5852, .T. ) ;
#17469 = VERTEX_POINT ( 'NONE', #22143 ) ;
#17470 = ORIENTED_EDGE ( 'NONE', *, *, #19177, .T. ) ;
#17471 = CARTESIAN_POINT ( 'NONE',  ( 8.300970689365454902, -78.60833333333327744, -4.784380313523529438 ) ) ;
#17472 = CARTESIAN_POINT ( 'NONE',  ( 9.652542402417001455, -76.94351332859899628, 0.04854625845423999470 ) ) ;
#17473 = AXIS2_PLACEMENT_3D ( 'NONE', #47671, #38776, #7197 ) ;
#17474 = VERTEX_POINT ( 'NONE', #57576 ) ;
#17475 = CARTESIAN_POINT ( 'NONE',  ( 9.376176103360082337, -79.51460875094232961, 1.742736205308521802 ) ) ;
#17476 = ORIENTED_EDGE ( 'NONE', *, *, #57467, .T. ) ;
#17477 = CARTESIAN_POINT ( 'NONE',  ( 9.830801209626999437, -24.09088558010999748, 7.765011064334000679 ) ) ;
#17478 = EDGE_CURVE ( 'NONE', #44945, #10899, #841, .T. ) ;
#17479 = ADVANCED_FACE ( 'NONE', ( #16859 ), #53746, .F. ) ;
#17480 = CARTESIAN_POINT ( 'NONE',  ( -7.374059913654000376, -79.18548998579800013, -6.282030610069000431 ) ) ;
#17481 = CARTESIAN_POINT ( 'NONE',  ( -3.533434062681735544, -78.19395196561279704, -8.548428288705636646 ) ) ;
#17482 = CARTESIAN_POINT ( 'NONE',  ( -7.408849624938999234, -79.26590222969299759, -8.421820339245000397 ) ) ;
#17483 = CARTESIAN_POINT ( 'NONE',  ( -0.1625384163739970467, -79.48544409746807560, 1.242284532507756278 ) ) ;
#17484 = ORIENTED_EDGE ( 'NONE', *, *, #14549, .F. ) ;
#17485 = EDGE_LOOP ( 'NONE', ( #28298, #6296, #27388 ) ) ;
#17486 = CARTESIAN_POINT ( 'NONE',  ( 2.036425055830775488, -77.45743550615227946, 9.023012778983279247 ) ) ;
#17487 = CARTESIAN_POINT ( 'NONE',  ( -9.050627908549000011, -77.35806749281498185, -6.322205650057999726 ) ) ;
#17488 = CARTESIAN_POINT ( 'NONE',  ( 9.500000000000000000, -77.64999999999999147, 0.000000000000000000 ) ) ;
#17489 = CARTESIAN_POINT ( 'NONE',  ( 9.131029190779001325, -77.55266531942498887, -3.285576857342999979 ) ) ;
#17490 = CARTESIAN_POINT ( 'NONE',  ( -9.990509419794001644, -76.27765497417000518, 8.015179320152999054 ) ) ;
#17491 = CARTESIAN_POINT ( 'NONE',  ( -6.781111407274376113, -79.46151114110770664, -6.653164290666497394 ) ) ;
#17492 = CARTESIAN_POINT ( 'NONE',  ( 10.42531124903999995, -55.53514851492000304, -7.624341765436000173 ) ) ;
#17493 = CARTESIAN_POINT ( 'NONE',  ( -1.635010352784000087, -80.54300105216999839, -10.62493487727000030 ) ) ;
#17494 = CARTESIAN_POINT ( 'NONE',  ( 12.83838672491000032, -18.79401612030999758, -2.062170725306000207 ) ) ;
#17495 = CARTESIAN_POINT ( 'NONE',  ( -9.414507962619001802, -25.26263135926000203, -8.652357372777000677 ) ) ;
#17496 = CARTESIAN_POINT ( 'NONE',  ( -11.67265798347707140, -76.69004288209750086, 1.396753407656934787 ) ) ;
#17497 = ORIENTED_EDGE ( 'NONE', *, *, #50452, .T. ) ;
#17498 = CARTESIAN_POINT ( 'NONE',  ( -10.86381291811999894, -79.48018145514599553, -5.803755483477999633 ) ) ;
#17499 = CARTESIAN_POINT ( 'NONE',  ( -7.633478597807999755, -55.59901960186999759, 10.36292351976000070 ) ) ;
#17500 = CARTESIAN_POINT ( 'NONE',  ( -6.022804356561167971, -78.02249797650281948, 8.904300299157986487 ) ) ;
#17501 = CARTESIAN_POINT ( 'NONE',  ( 5.537129384246000541, -78.97065855411999280, 10.62336504503000079 ) ) ;
#17502 = CARTESIAN_POINT ( 'NONE',  ( -8.878349648294999952, -16.93036913510000119, -8.870329531829000302 ) ) ;
#17504 = CARTESIAN_POINT ( 'NONE',  ( -2.019183793707000074, -18.21279722757000030, -12.79944116704999857 ) ) ;
#17503 = CARTESIAN_POINT ( 'NONE',  ( 7.653559502293999728, -60.09849137195000424, 10.01234990230000044 ) ) ;
#17505 = CARTESIAN_POINT ( 'NONE',  ( -0.3664097463224703644, -53.82809982435230012, 12.50575740040853390 ) ) ;
#17506 = CARTESIAN_POINT ( 'NONE',  ( 10.55911395186000057, -56.01538333533000014, -7.642160924870000649 ) ) ;
#17507 = DIRECTION ( 'NONE',  ( -0.7071067811865974218, 0.7071067811864975017, -8.595326187306963091E-09 ) ) ;
#17508 = CARTESIAN_POINT ( 'NONE',  ( -10.58739904582000158, -77.85109353173099578, -3.839393962977000196 ) ) ;
#17509 = FACE_OUTER_BOUND ( 'NONE', #40411, .T. ) ;
#17510 = CARTESIAN_POINT ( 'NONE',  ( -8.361631869233999481, -80.26504353420789073, 7.535039759702999440 ) ) ;
#17511 = ORIENTED_EDGE ( 'NONE', *, *, #19753, .F. ) ;
#17512 = CARTESIAN_POINT ( 'NONE',  ( 0.8521412958799197135, -1.455789518402647031, 3.164999420474257530 ) ) ;
#17513 = CARTESIAN_POINT ( 'NONE',  ( -1.460729357743000056, -54.70908756765000192, 12.44211643236999976 ) ) ;
#17514 = AXIS2_PLACEMENT_3D ( 'NONE', #55351, #37040, #32304 ) ;
#17515 = CARTESIAN_POINT ( 'NONE',  ( 0.000000000000000000, -82.25000000001401190, -1.249999999985999866 ) ) ;
#17516 = CARTESIAN_POINT ( 'NONE',  ( -3.122751374266999669, -1.580997856415000014, -1.547189057874000184 ) ) ;
#17517 = B_SPLINE_CURVE_WITH_KNOTS ( 'NONE', 3,
 ( #35755, #3885, #17466, #53197, #13913, #54077, #374, #31906, #26897, #13615, #35456, #21887, #49948, #4772, #13025, #4483, #27478, #53484 ),
 .UNSPECIFIED., .F., .F.,
 ( 4, 2, 2, 2, 2, 2, 2, 2, 4 ),
 ( 0.000000000000000000, 0.1250000000000000000, 0.2500000000000000000, 0.3750000000000000000, 0.5000000000000000000, 0.6250000000000000000, 0.7500000000000000000, 0.8750000000000000000, 1.000000000000000000 ),
 .UNSPECIFIED. ) ;
#17518 = CARTESIAN_POINT ( 'NONE',  ( 9.106330615755000579, -79.18979598044998625, -1.992521687893000104 ) ) ;
#17519 = FACE_BOUND ( 'NONE', #10130, .T. ) ;
#17520 = EDGE_CURVE ( 'NONE', #8754, #50383, #51630, .T. ) ;
#17521 = CARTESIAN_POINT ( 'NONE',  ( 0.000000000000000000, -81.99999999999998579, -10.50000000000000000 ) ) ;
#17522 = CARTESIAN_POINT ( 'NONE',  ( 0.9781264271447999148, -61.74031143843999558, 12.65967462882999861 ) ) ;
#17523 = CARTESIAN_POINT ( 'NONE',  ( 12.61271781521000079, -18.80306329050999992, 1.798333084007999849 ) ) ;
#17524 = CIRCLE ( 'NONE', #5270, 9.599999999999999645 ) ;
#17525 = CARTESIAN_POINT ( 'NONE',  ( 1.290108009600000161, -84.30649735065199479, 3.970544182317999660 ) ) ;
#17526 = FACE_OUTER_BOUND ( 'NONE', #528, .T. ) ;
#17527 = VECTOR ( 'NONE', #42041, 1000.000000000000114 ) ;
#17528 = CARTESIAN_POINT ( 'NONE',  ( 9.498848458907630743, -79.06748417780224258, 0.1004247326035953569 ) ) ;
#17529 = CARTESIAN_POINT ( 'NONE',  ( 2.958310398169000432, -77.35523885853200454, -10.74723220921999989 ) ) ;
#17530 = CARTESIAN_POINT ( 'NONE',  ( 1.167992134012648231, -81.87908179006763021, 0.4465703791935540234 ) ) ;
#17531 = CARTESIAN_POINT ( 'NONE',  ( -1.401271510176000046, -78.92838903957999719, -0.6604077434914998879 ) ) ;
#17532 = DIRECTION ( 'NONE',  ( 1.000000000000000000, 0.000000000000000000, 0.000000000000000000 ) ) ;
#17533 = CARTESIAN_POINT ( 'NONE',  ( 1.490703458528794600, -82.98683660370730308, -0.2499861325332328188 ) ) ;
#17534 = CARTESIAN_POINT ( 'NONE',  ( -2.598917237794085455, -2.552083333333333481, -1.997276839918474600 ) ) ;
#17535 = CARTESIAN_POINT ( 'NONE',  ( -4.082680704644886305, -80.19438284699886310, -9.944308183758115760 ) ) ;
#17536 = DIRECTION ( 'NONE',  ( 0.000000000000000000, -1.000000000000000000, 0.000000000000000000 ) ) ;
#17537 = LINE ( 'NONE', #31978, #15318 ) ;
#17538 = EDGE_CURVE ( 'NONE', #35854, #1173, #34711, .T. ) ;
#17539 = ORIENTED_EDGE ( 'NONE', *, *, #14042, .T. ) ;
#17540 = CARTESIAN_POINT ( 'NONE',  ( 1.042299842011717770, -81.80361443818746636, -0.6898479045106226115 ) ) ;
#17541 = EDGE_CURVE ( 'NONE', #44945, #29444, #14670, .T. ) ;
#17542 = CARTESIAN_POINT ( 'NONE',  ( -12.50000000000000000, -55.55000000278000272, 1.750000000000000000 ) ) ;
#17543 = CARTESIAN_POINT ( 'NONE',  ( -9.744524944696001612, -79.43148518439899419, -5.412839751281999234 ) ) ;
#17544 = DIRECTION ( 'NONE',  ( 0.7071067811865969777, -0.7071067811864980568, -1.359271113201994007E-10 ) ) ;
#17545 = ORIENTED_EDGE ( 'NONE', *, *, #13563, .T. ) ;
#17546 = ORIENTED_EDGE ( 'NONE', *, *, #35835, .F. ) ;
#17547 = DIRECTION ( 'NONE',  ( -1.558387406072000046E-11, -1.000000000000000000, -1.336738014604999829E-10 ) ) ;
#17548 = ORIENTED_EDGE ( 'NONE', *, *, #40614, .F. ) ;
#17549 = ORIENTED_EDGE ( 'NONE', *, *, #24648, .F. ) ;
#17550 = CARTESIAN_POINT ( 'NONE',  ( 11.05000000000000071, -82.00000000000000000, 0.000000000000000000 ) ) ;
#17551 = CARTESIAN_POINT ( 'NONE',  ( -1.699346936231083793, -78.95052082955746187, -2.957013875707059647 ) ) ;
#17552 = EDGE_CURVE ( 'NONE', #55944, #21753, #53766, .T. ) ;
#17553 = CARTESIAN_POINT ( 'NONE',  ( -10.22609403765000025, -79.67173935843099741, -4.138687607718999573 ) ) ;
#17554 = CARTESIAN_POINT ( 'NONE',  ( -1.570796326794885012, -76.41458333330569985, -12.00000000000000178 ) ) ;
#17555 = CARTESIAN_POINT ( 'NONE',  ( 2.314800267987999760, -82.53821485768798993, -2.958588558779999822 ) ) ;
#17556 = CARTESIAN_POINT ( 'NONE',  ( -5.569985714943742394, -79.32475174562625853, 7.695716824889310637 ) ) ;
#17557 = ORIENTED_EDGE ( 'NONE', *, *, #19466, .F. ) ;
#17558 = CARTESIAN_POINT ( 'NONE',  ( -7.062685404271999090, -77.78023905895217638, 8.485436034813998774 ) ) ;
#17559 = CARTESIAN_POINT ( 'NONE',  ( -10.70115325243999926, -78.54730848226999740, -6.181997344542000228 ) ) ;
#17560 = B_SPLINE_CURVE_WITH_KNOTS ( 'NONE', 3,
 ( #12451, #44620, #44043, #9190, #27175, #26309, #31306, #30446, #45213, #13016, #21598, #3593, #4761, #26017, #3880, #21879, #39603, #44913 ),
 .UNSPECIFIED., .F., .F.,
 ( 4, 2, 2, 2, 2, 2, 2, 2, 4 ),
 ( 0.000000000000000000, 0.1250000000000000000, 0.2500000000000000000, 0.3750000000000000000, 0.5000000000000000000, 0.6250000000000000000, 0.7500000000000000000, 0.8750000000000000000, 1.000000000000000000 ),
 .UNSPECIFIED. ) ;
#17561 = EDGE_LOOP ( 'NONE', ( #55236, #44144, #41588, #52032 ) ) ;
#17562 = VERTEX_POINT ( 'NONE', #7789 ) ;
#17563 = CARTESIAN_POINT ( 'NONE',  ( 0.000000000000000000, -76.14999999999999147, 0.000000000000000000 ) ) ;
#17564 = DIRECTION ( 'NONE',  ( 0.000000000000000000, 0.000000000000000000, -1.000000000000000000 ) ) ;
#17565 = VECTOR ( 'NONE', #44821, 1000.000000000000000 ) ;
#17566 = CARTESIAN_POINT ( 'NONE',  ( 0.9788970803261000109, -79.91247514884599923, -0.9057243817226000582 ) ) ;
#17567 = CARTESIAN_POINT ( 'NONE',  ( 9.051070938631999852, -77.48890712634099032, 3.499832029064999794 ) ) ;
#17568 = CARTESIAN_POINT ( 'NONE',  ( -3.622867166186050536, -86.12610001270962812, 1.695533395769002638 ) ) ;
#17570 = EDGE_CURVE ( 'NONE', #54661, #25114, #27710, .T. ) ;
#17569 = LINE ( 'NONE', #34975, #15758 ) ;
#17571 = AXIS2_PLACEMENT_3D ( 'NONE', #52448, #2573, #25571 ) ;
#17572 = AXIS2_PLACEMENT_3D ( 'NONE', #9551, #18699, #45282 ) ;
#17573 = CARTESIAN_POINT ( 'NONE',  ( -8.110204649352999340, -78.43694664278000062, 9.400142180594000862 ) ) ;
#17574 = CARTESIAN_POINT ( 'NONE',  ( 5.354686402641000598, -76.58457105268000475, 11.45119097547000031 ) ) ;
#17575 = ADVANCED_FACE ( 'NONE', ( #34921 ), #30870, .F. ) ;
#17576 = CARTESIAN_POINT ( 'NONE',  ( 9.514701387850999836, -76.23623749738399624, -5.285895731461000224 ) ) ;
#17577 = AXIS2_PLACEMENT_3D ( 'NONE', #51009, #1709, #19703 ) ;
#17578 = CARTESIAN_POINT ( 'NONE',  ( -8.674899888355607658, -78.62823151048618797, -3.212842792980429518 ) ) ;
#17579 = CARTESIAN_POINT ( 'NONE',  ( 3.110929027860000140, -81.09520976391398506, -2.455221122833000091 ) ) ;
#17580 = CARTESIAN_POINT ( 'NONE',  ( -10.01332852686999964, -55.51943464808999806, 7.654537165450999936 ) ) ;
#17581 = CARTESIAN_POINT ( 'NONE',  ( -0.1382660771586305126, -2.978707574826329640, 3.247216946312587726 ) ) ;
#17582 = CARTESIAN_POINT ( 'NONE',  ( 3.260489991048999947, -82.29725264934799611, -1.390623913068999906 ) ) ;
#17583 = CARTESIAN_POINT ( 'NONE',  ( -7.648026768019999366, -23.24999998419999869, -10.12290050217000115 ) ) ;
#17584 = CARTESIAN_POINT ( 'NONE',  ( -0.8451721318799240157, -80.98139021206071675, 10.71663691162798315 ) ) ;
#17585 = CARTESIAN_POINT ( 'NONE',  ( -2.612980907336999614, -80.44026683748349171, -10.95817168551000087 ) ) ;
#17586 = CARTESIAN_POINT ( 'NONE',  ( -3.370587613551000228, -1.760959338694000120, 0.9429417476038000068 ) ) ;
#17587 = CARTESIAN_POINT ( 'NONE',  ( -1.018555708747796107, -80.19902807273064127, 0.7675077034654457231 ) ) ;
#17588 = ORIENTED_EDGE ( 'NONE', *, *, #42567, .F. ) ;
#17589 = CARTESIAN_POINT ( 'NONE',  ( 9.250000000000000000, -78.84999999999999432, 1.340711541092999922E-14 ) ) ;
#17590 = CARTESIAN_POINT ( 'NONE',  ( -10.71369944335147117, -79.22083333333333144, -2.879226727952084453 ) ) ;
#17591 = CARTESIAN_POINT ( 'NONE',  ( -1.310615285706999922, -81.73669314701200506, -0.2467057407436999972 ) ) ;
#17592 = DIRECTION ( 'NONE',  ( 0.000000000000000000, 1.000000000000000000, 0.000000000000000000 ) ) ;
#17593 = CARTESIAN_POINT ( 'NONE',  ( -9.692839446179998930, -78.46716024849999371, 7.074522137259999788 ) ) ;
#17594 = CARTESIAN_POINT ( 'NONE',  ( 7.565372432932000457, -79.70598667140099280, -5.616098813059000605 ) ) ;
#17595 = CARTESIAN_POINT ( 'NONE',  ( 12.71798269385000069, -18.70221245812999911, -1.931086388578000079 ) ) ;
#17596 = ORIENTED_EDGE ( 'NONE', *, *, #18189, .T. ) ;
#17597 = CARTESIAN_POINT ( 'NONE',  ( -9.837773999814896086, -54.48535604133265764, 7.850041801394331387 ) ) ;
#17598 = CARTESIAN_POINT ( 'NONE',  ( -5.812473449021000604, -77.09729030948868456, 9.660279995464000180 ) ) ;
#17599 = CARTESIAN_POINT ( 'NONE',  ( -1.241956275658999909, -82.32625246582099976, -0.4726577424567999786 ) ) ;
#17600 = CARTESIAN_POINT ( 'NONE',  ( -12.00000000000000178, -78.91041666666664867, -1.570796326794897668 ) ) ;
#17601 = CARTESIAN_POINT ( 'NONE',  ( -3.833926501619000060, -78.04896150565798507, -8.716156481626001096 ) ) ;
#17603 = CARTESIAN_POINT ( 'NONE',  ( -3.858199361241999803, -0.8397668567873000089, -1.117275487237999965 ) ) ;
#17602 = CARTESIAN_POINT ( 'NONE',  ( -1.813335989237000234, -85.74518770028200265, 3.710867668353999616 ) ) ;
#17604 = DIRECTION ( 'NONE',  ( 0.000000000000000000, -1.000000000000000000, 0.000000000000000000 ) ) ;
#17605 = CARTESIAN_POINT ( 'NONE',  ( -1.379800422845999908, -80.58131689367100137, -0.6283944928419999965 ) ) ;
#17606 = ORIENTED_EDGE ( 'NONE', *, *, #38010, .T. ) ;
#17607 = VECTOR ( 'NONE', #44834, 1000.000000000000000 ) ;
#17608 = CARTESIAN_POINT ( 'NONE',  ( 8.059793245469082379, -77.29260984181965455, -7.115412693491175666 ) ) ;
#17609 = CARTESIAN_POINT ( 'NONE',  ( -2.460449926407452192, -78.99659071566932766, 8.997086085319750737 ) ) ;
#17610 = CARTESIAN_POINT ( 'NONE',  ( -3.399999999999689937, -78.72609999968184979, -1.426627331148062801E-14 ) ) ;
#17611 = ORIENTED_EDGE ( 'NONE', *, *, #41867, .T. ) ;
#17612 = CIRCLE ( 'NONE', #32680, 9.599999999999999645 ) ;
#17613 = ORIENTED_EDGE ( 'NONE', *, *, #18928, .T. ) ;
#17614 = CARTESIAN_POINT ( 'NONE',  ( -6.999846649096999940, -79.30106226310599027, 8.407732347380999727 ) ) ;
#17615 = CYLINDRICAL_SURFACE ( 'NONE', #1996, 11.75000000000000000 ) ;
#17616 = CARTESIAN_POINT ( 'NONE',  ( -3.516941471767000227, -80.40586707127998523, -10.40795029645000014 ) ) ;
#17617 = CIRCLE ( 'NONE', #38345, 1.199999999999999956 ) ;
#17618 = ORIENTED_EDGE ( 'NONE', *, *, #9007, .F. ) ;
#17619 = CARTESIAN_POINT ( 'NONE',  ( 7.966054476048999078, -77.50865908154399619, 9.040893068079999040 ) ) ;
#17620 = AXIS2_PLACEMENT_3D ( 'NONE', #17925, #34742, #8185 ) ;
#17621 = VERTEX_POINT ( 'NONE', #21074 ) ;
#17622 = ORIENTED_EDGE ( 'NONE', *, *, #30060, .F. ) ;
#17623 = CARTESIAN_POINT ( 'NONE',  ( -2.963063481827658219, -2.634561461520561032, -1.334362463457642534 ) ) ;
#17624 = EDGE_CURVE ( 'NONE', #45467, #52988, #33363, .T. ) ;
#17625 = CARTESIAN_POINT ( 'NONE',  ( 10.48428321214112202, -76.60764424186088206, -6.042971066631413812 ) ) ;
#17626 = CARTESIAN_POINT ( 'NONE',  ( -7.919595949288999570, -59.94999999969000015, -8.768124086712999699 ) ) ;
#17627 = ORIENTED_EDGE ( 'NONE', *, *, #9369, .T. ) ;
#17628 = ORIENTED_EDGE ( 'NONE', *, *, #53424, .T. ) ;
#17629 = DIRECTION ( 'NONE',  ( -1.000000000000000000, 0.000000000000000000, 0.000000000000000000 ) ) ;
#17630 = CARTESIAN_POINT ( 'NONE',  ( 2.060606489177889689, -78.96264282632948550, -3.567929020052158950 ) ) ;
#17631 = FACE_BOUND ( 'NONE', #14346, .T. ) ;
#17632 = CARTESIAN_POINT ( 'NONE',  ( -7.653559502275999016, -23.29849137228000444, -10.01234990228999955 ) ) ;
#17633 = CARTESIAN_POINT ( 'NONE',  ( -3.783563790603477806, -77.29730020392733536, -11.14627141929872067 ) ) ;
#17634 = DIRECTION ( 'NONE',  ( 1.000000000000000000, 0.000000000000000000, 0.000000000000000000 ) ) ;
#17635 = EDGE_CURVE ( 'NONE', #11225, #39417, #50595, .T. ) ;
#17636 = CARTESIAN_POINT ( 'NONE',  ( 5.137083998358000336, -77.31100733245999379, -10.56753840748999984 ) ) ;
#17637 = CYLINDRICAL_SURFACE ( 'NONE', #18082, 0.5000000000000006661 ) ;
#17638 = CARTESIAN_POINT ( 'NONE',  ( -1.250000000000000000, -79.50000000000000000, 0.000000000000000000 ) ) ;
#17639 = CIRCLE ( 'NONE', #6318, 13.00000000000000000 ) ;
#17640 = CARTESIAN_POINT ( 'NONE',  ( 1.960173199283000267, -79.72080496681199691, 3.683447210608000066 ) ) ;
#17641 = CARTESIAN_POINT ( 'NONE',  ( 9.334420024193999410, -77.54426001420199555, -3.215556494258000164 ) ) ;
#17642 = CARTESIAN_POINT ( 'NONE',  ( -12.50240681834000078, -24.68234730741999883, 1.005418943852999902 ) ) ;
#17643 = LINE ( 'NONE', #4358, #56589 ) ;
#17644 = CARTESIAN_POINT ( 'NONE',  ( 1.807051837523000026, -24.30078415243000123, 12.77977401834999860 ) ) ;
#17645 = CARTESIAN_POINT ( 'NONE',  ( -5.239266479141337030, -80.01428708882451701, 9.745699944792930225 ) ) ;
#17647 = CARTESIAN_POINT ( 'NONE',  ( -1.490122748909000094, -84.99032934161199648, -3.219331321608999819 ) ) ;
#17646 = CIRCLE ( 'NONE', #45824, 2.799999999999999822 ) ;
#17648 = CARTESIAN_POINT ( 'NONE',  ( 2.939819053343999844, -1.106200577025999943, 2.890138559307000143 ) ) ;
#17649 = LINE ( 'NONE', #26487, #57809 ) ;
#17650 = AXIS2_PLACEMENT_3D ( 'NONE', #20101, #11533, #38091 ) ;
#17651 = CARTESIAN_POINT ( 'NONE',  ( -1.404361994020937088, -80.87968703033534723, -0.5636150327419870987 ) ) ;
#17652 = CARTESIAN_POINT ( 'NONE',  ( -1.250000000000000000, -78.60000000000000853, 0.000000000000000000 ) ) ;
#17653 = CARTESIAN_POINT ( 'NONE',  ( -1.049525737143000015, -77.97675193319649622, -1.227116502697000122 ) ) ;
#17654 = VECTOR ( 'NONE', #57906, 1000.000000000000000 ) ;
#17655 = CARTESIAN_POINT ( 'NONE',  ( 10.90625000000000000, -80.29374999999798490, -5.301077343649000152E-10 ) ) ;
#17656 = EDGE_CURVE ( 'NONE', #27335, #23838, #13907, .T. ) ;
#17657 = CARTESIAN_POINT ( 'NONE',  ( 10.50536548972000084, -77.75467495194999401, -2.968612793496999913 ) ) ;
#17658 = CARTESIAN_POINT ( 'NONE',  ( 11.26957934775000147, -78.65591505001499684, 4.877733875464000057 ) ) ;
#17659 = DIRECTION ( 'NONE',  ( -0.7071067811865474617, 0.000000000000000000, 0.7071067811865474617 ) ) ;
#17660 = CARTESIAN_POINT ( 'NONE',  ( -5.413904038987160661, -79.08333333333332860, -9.393203674808278336 ) ) ;
#17662 = CARTESIAN_POINT ( 'NONE',  ( 1.272474653676000100, -78.51097266169500699, -0.6251940786299999830 ) ) ;
#17661 = DIRECTION ( 'NONE',  ( 1.000000000000000000, 0.000000000000000000, 0.000000000000000000 ) ) ;
#17663 = CARTESIAN_POINT ( 'NONE',  ( 0.7473949548134999343, -82.10881715536000058, 1.530103832088000049 ) ) ;
#17664 = ORIENTED_EDGE ( 'NONE', *, *, #46042, .F. ) ;
#17665 = CARTESIAN_POINT ( 'NONE',  ( -10.18491068059999805, -18.69283065396999888, -7.640030139758000161 ) ) ;
#17666 = CARTESIAN_POINT ( 'NONE',  ( -11.29127801606999881, -79.09732492801998660, 3.839647735398000084 ) ) ;
#17667 = CARTESIAN_POINT ( 'NONE',  ( -5.970469449440000353, -81.06265812071879395, 9.021904006163001810 ) ) ;
#17668 = B_SPLINE_CURVE_WITH_KNOTS ( 'NONE', 3,
 ( #5536, #42734, #24721, #50731, #46014, #41559, #5829, #23836, #41852, #14975, #32973, #51018, #10568, #38866, #2581, #20583, #48045, #12580, #29993, #21440, #3724, #29708, #16442, #17016, #30286, #34998, #34132, #3439, #39451, #39157 ),
 .UNSPECIFIED., .F., .F.,
 ( 4, 2, 2, 2, 2, 2, 2, 2, 2, 2, 2, 2, 2, 2, 4 ),
 ( 0.000000000000000000, 0.1249999999999994171, 0.1874999999999991396, 0.2499999999999988898, 0.3124999999999986677, 0.3749999999999983347, 0.4999999999999971689, 0.5624999999999965583, 0.6249999999999960032, 0.6874999999999954481, 0.7499999999999950040, 0.8124999999999944489, 0.8437499999999948930, 0.8749999999999952260, 1.000000000000000000 ),
 .UNSPECIFIED. ) ;
#17669 = CARTESIAN_POINT ( 'NONE',  ( 0.000000000000000000, -86.09999999999999432, 0.000000000000000000 ) ) ;
#17670 = CARTESIAN_POINT ( 'NONE',  ( 0.000000000000000000, -80.79999999999999716, 0.000000000000000000 ) ) ;
#17671 = CARTESIAN_POINT ( 'NONE',  ( -6.659967121051000305, -76.90830639992499584, -9.025682433062998555 ) ) ;
#17672 = CARTESIAN_POINT ( 'NONE',  ( -10.19022265129000004, -59.99634105610000034, 7.646946115762000673 ) ) ;
#17673 = CARTESIAN_POINT ( 'NONE',  ( 2.268344470944000157, -78.97289170186299145, -9.471763527590001175 ) ) ;
#17674 = CARTESIAN_POINT ( 'NONE',  ( 3.525388664395999960, -0.7875064129436999405, -0.3052335303999000327 ) ) ;
#17675 = CARTESIAN_POINT ( 'NONE',  ( 9.492565570809029296, -76.49917531041499785, -7.041922512536913814 ) ) ;
#17676 = CARTESIAN_POINT ( 'NONE',  ( -1.799501877760999902, -55.51082434643999619, 12.60552522433000000 ) ) ;
#17677 = ORIENTED_EDGE ( 'NONE', *, *, #3204, .T. ) ;
#17678 = DIRECTION ( 'NONE',  ( 0.000000000000000000, 0.000000000000000000, 1.000000000000000000 ) ) ;
#17679 = CARTESIAN_POINT ( 'NONE',  ( -3.992191694170000194, -79.72926001420199782, 8.886347659747999117 ) ) ;
#17680 = DIRECTION ( 'NONE',  ( 1.000000000000000000, 7.077858357939000336E-11, -7.077867239723000107E-11 ) ) ;
#17681 = CARTESIAN_POINT ( 'NONE',  ( -10.38646360829999971, -59.57795407677000554, -7.655555357447999754 ) ) ;
#17682 = CARTESIAN_POINT ( 'NONE',  ( -1.630114970985000022, -79.90535085241999980, -0.3434887894992000312 ) ) ;
#17683 = CARTESIAN_POINT ( 'NONE',  ( 12.00000000000000888, -77.03958333333333997, -1.570796326794872577 ) ) ;
#17684 = ORIENTED_EDGE ( 'NONE', *, *, #43146, .T. ) ;
#17685 = DIRECTION ( 'NONE',  ( 0.000000000000000000, 1.000000000000000000, 0.000000000000000000 ) ) ;
#17686 = CARTESIAN_POINT ( 'NONE',  ( 11.75000000000000000, -77.95000000000000284, 2.316376715183999699E-14 ) ) ;
#17687 = CARTESIAN_POINT ( 'NONE',  ( -1.667916687244999974, -23.29849137228000444, 12.49168433579000137 ) ) ;
#17688 = AXIS2_PLACEMENT_3D ( 'NONE', #22802, #54683, #49977 ) ;
#17689 = ORIENTED_EDGE ( 'NONE', *, *, #6, .F. ) ;
#17690 = CARTESIAN_POINT ( 'NONE',  ( -12.83044039277999993, -60.10639625617000092, 2.062670899148999926 ) ) ;
#17691 = CARTESIAN_POINT ( 'NONE',  ( -8.260145278118999457, -53.85964900942000355, -9.643338478971999805 ) ) ;
#17692 = EDGE_CURVE ( 'NONE', #45372, #31856, #51302, .T. ) ;
#17693 = PRODUCT_CONTEXT ( 'NONE', #29998, 'mechanical' ) ;
#17694 = CARTESIAN_POINT ( 'NONE',  ( -7.545891804452000251, -79.71510512889798861, 6.201630566990999682 ) ) ;
#17695 = ORIENTED_EDGE ( 'NONE', *, *, #46678, .F. ) ;
#17696 = AXIS2_PLACEMENT_3D ( 'NONE', #29589, #25752, #43773 ) ;
#17697 = ORIENTED_EDGE ( 'NONE', *, *, #7679, .F. ) ;
#17698 = CARTESIAN_POINT ( 'NONE',  ( -11.89890540480000070, -77.10472319096498950, 2.846590415137000285 ) ) ;
#17699 = FACE_OUTER_BOUND ( 'NONE', #27112, .T. ) ;
#17700 = EDGE_CURVE ( 'NONE', #47139, #38464, #54469, .T. ) ;
#17701 = CARTESIAN_POINT ( 'NONE',  ( 0.4964284668415000490, -78.41931985888000156, -1.571764949136999823 ) ) ;
#17702 = EDGE_LOOP ( 'NONE', ( #52414, #19242, #5051, #35297 ) ) ;
#17703 = B_SPLINE_CURVE_WITH_KNOTS ( 'NONE', 3,
 ( #12816, #30814, #48846, #37734, #55758, #33297, #51334, #46914, #42470, #2037 ),
 .UNSPECIFIED., .F., .F.,
 ( 4, 2, 2, 2, 4 ),
 ( 0.000000000000000000, 0.2500000000000000000, 0.5000000000000000000, 0.7500000000000000000, 1.000000000000000000 ),
 .UNSPECIFIED. ) ;
#17704 = CARTESIAN_POINT ( 'NONE',  ( 10.36292447790000004, -18.79904187578000219, 7.633480004415999609 ) ) ;
#17705 = DIRECTION ( 'NONE',  ( -0.7071067811865474617, 0.000000000000000000, -0.7071067811865474617 ) ) ;
#17706 = CARTESIAN_POINT ( 'NONE',  ( 7.256259382531156099, -77.65769096820322659, 6.443642414277258368 ) ) ;
#17707 = VECTOR ( 'NONE', #43279, 1000.000000000000000 ) ;
#17708 = PLANE ( 'NONE',  #3460 ) ;
#17709 = CARTESIAN_POINT ( 'NONE',  ( -3.372301964606999825, -76.89007569364000005, 12.67255275672000003 ) ) ;
#17710 = CARTESIAN_POINT ( 'NONE',  ( 10.34070037867000202, -77.96833891353188051, -4.346035695907999319 ) ) ;
#17711 = CARTESIAN_POINT ( 'NONE',  ( 13.63885489310999510, -22.78578169018999944, 7.254376133916000668 ) ) ;
#17712 = CARTESIAN_POINT ( 'NONE',  ( 3.112536659741847345, -86.17851879815597727, -1.385790604991341546 ) ) ;
#17713 = CARTESIAN_POINT ( 'NONE',  ( -6.324515969367999979, -78.97901371548900329, -9.263833350438000380 ) ) ;
#17714 = CARTESIAN_POINT ( 'NONE',  ( 7.021204365543900039, -79.90651252694955531, 6.021971066871157241 ) ) ;
#17715 = EDGE_CURVE ( 'NONE', #36961, #21517, #20006, .T. ) ;
#17716 = CARTESIAN_POINT ( 'NONE',  ( 8.532671861026141613, -16.87201063390074651, 9.433519686760231338 ) ) ;
#17717 = VERTEX_POINT ( 'NONE', #18110 ) ;
#17718 = CARTESIAN_POINT ( 'NONE',  ( -9.512698799462512511, -77.24565731317359507, 0.5183019084032332024 ) ) ;
#17719 = CARTESIAN_POINT ( 'NONE',  ( 12.21199139566000014, -76.31204719422001403, 1.550091862394999964 ) ) ;
#17720 = CARTESIAN_POINT ( 'NONE',  ( -0.6623784515263000383, -79.99942042488599725, -1.472572141918999877 ) ) ;
#17721 = CARTESIAN_POINT ( 'NONE',  ( -3.137247185147045148, -3.311698843223778166, 1.599361815492593264 ) ) ;
#17722 = CARTESIAN_POINT ( 'NONE',  ( 12.60413652831999975, -23.30716934606000024, 1.799502287743000029 ) ) ;
#17723 = CARTESIAN_POINT ( 'NONE',  ( -4.885220488697999741, -76.60923828122899693, 11.26753068192000029 ) ) ;
#17724 = CARTESIAN_POINT ( 'NONE',  ( -1.417334032777999964, -79.02654225787900089, -0.4910847579886000736 ) ) ;
#17725 = CARTESIAN_POINT ( 'NONE',  ( 9.266295309513999712, -77.21501332859899946, 2.616508480087999633 ) ) ;
#17726 = CARTESIAN_POINT ( 'NONE',  ( 7.284200816657673272, -76.87346977519162294, 9.621121000730060047 ) ) ;
#17727 = CARTESIAN_POINT ( 'NONE',  ( -10.47020627418439354, -79.52083333333331439, -2.813789756862263847 ) ) ;
#17728 = CARTESIAN_POINT ( 'NONE',  ( -13.02716421901072685, -75.95264176747838292, -0.01989893052437335594 ) ) ;
#17729 = B_SPLINE_SURFACE_WITH_KNOTS ( 'NONE', 3, 3, ( 
 ( #48839, #40854, #31681, #4846 ),
 ( #31387, #156, #53855, #36127 ),
 ( #3951, #26667, #22842, #50017 ),
 ( #17240, #18132, #17838, #49428 ),
 ( #49727, #9270, #39676, #31090 ),
 ( #12807, #54143, #26964, #446 ),
 ( #30806, #36415, #26379, #54443 ),
 ( #18425, #44699, #13979, #57979 ),
 ( #8678, #44995, #4550, #13684 ),
 ( #31975, #27548, #45591, #5136 ),
 ( #23135, #46469, #10150, #19295 ) ),
 .UNSPECIFIED., .F., .F., .F.,
 ( 4, 1, 1, 1, 1, 1, 1, 1, 4 ),
 ( 4, 4 ),
 ( -0.02001474922158999817, 0.000000000000000000, 0.1666666666667000196, 0.3333333333333000081, 0.5000000000000000000, 0.6666666666667000474, 0.8333333333333000637, 1.000000000000000000, 1.020283381528000133 ),
 ( -0.3582002740342999925, 1.358862457857999972 ),
 .UNSPECIFIED. ) ;
#17730 = CARTESIAN_POINT ( 'NONE',  ( 0.000000000000000000, -77.19999999999998863, 0.000000000000000000 ) ) ;
#17731 = VERTEX_POINT ( 'NONE', #13955 ) ;
#17732 = CARTESIAN_POINT ( 'NONE',  ( -1.285835855790000037, -81.91654517592999696, 0.7092774996876000104 ) ) ;
#17733 = CARTESIAN_POINT ( 'NONE',  ( -0.6515920321739999688, -80.60493433575999234, -1.183807013712999900 ) ) ;
#17734 = CARTESIAN_POINT ( 'NONE',  ( -1.178447680628000205, -80.55308451575899653, -0.9280415206345000723 ) ) ;
#17735 = LINE ( 'NONE', #13583, #13532 ) ;
#17736 = CARTESIAN_POINT ( 'NONE',  ( 6.184758847501745649, -77.00000000000000000, 6.951421119677088534 ) ) ;
#17737 = CARTESIAN_POINT ( 'NONE',  ( -0.5544740949720999845, -82.17239317537999455, 1.570928860995999932 ) ) ;
#17738 = CARTESIAN_POINT ( 'NONE',  ( 10.95272639356999989, -78.85909624325299205, 4.740592608656999829 ) ) ;
#17739 = CARTESIAN_POINT ( 'NONE',  ( 4.495978696100999983, -77.90669805011499705, 8.621246072682998474 ) ) ;
#17740 = CARTESIAN_POINT ( 'NONE',  ( -2.065394024360999836, -55.37838567321000482, -12.82193048525000023 ) ) ;
#17741 = CARTESIAN_POINT ( 'NONE',  ( 9.596002108778172612, -78.49791666666668277, -7.374560639698962028 ) ) ;
#17742 = CARTESIAN_POINT ( 'NONE',  ( -0.2676215762113999808, -79.33579419080099626, 11.02860431212999970 ) ) ;
#17743 = CARTESIAN_POINT ( 'NONE',  ( 3.723051508230033502, -85.94828561723799965, 2.704164226566601492 ) ) ;
#17744 = ORIENTED_EDGE ( 'NONE', *, *, #1954, .T. ) ;
#17745 = CARTESIAN_POINT ( 'NONE',  ( -1.250000000000000000, -79.50000000000000000, 0.000000000000000000 ) ) ;
#17746 = CARTESIAN_POINT ( 'NONE',  ( 0.9218200799623692543, -79.22291666666664867, 1.199500263597272687 ) ) ;
#17747 = CARTESIAN_POINT ( 'NONE',  ( -3.436577009133267691, -78.54828564506388489, 0.06478620501008579280 ) ) ;
#17748 = CARTESIAN_POINT ( 'NONE',  ( 9.028681611143001717, -78.19400356791099682, -5.970393136294000591 ) ) ;
#17749 = CARTESIAN_POINT ( 'NONE',  ( -0.2494208068357447461, -17.00711039237069144, -12.50614183112945277 ) ) ;
#17750 = CARTESIAN_POINT ( 'NONE',  ( -11.35613837876999987, -76.40844191910899497, 4.947237039123000280 ) ) ;
#17751 = CARTESIAN_POINT ( 'NONE',  ( 0.5204347304194590906, -78.56791883825732725, 11.73731741140708529 ) ) ;
#17752 = CARTESIAN_POINT ( 'NONE',  ( -5.052420809101000088E-14, -80.84999999994218456, 0.000000000000000000 ) ) ;
#17753 = ORIENTED_EDGE ( 'NONE', *, *, #49358, .F. ) ;
#17754 = ADVANCED_FACE ( 'NONE', ( #53829 ), #15679, .F. ) ;
#17755 = CARTESIAN_POINT ( 'NONE',  ( 8.858182419534999852, -80.07955691727549663, 6.954620140474000678 ) ) ;
#17756 = CARTESIAN_POINT ( 'NONE',  ( 0.06191098829455312508, -79.97165892281826416, 1.249638892610136720 ) ) ;
#17757 = PRESENTATION_LAYER_ASSIGNMENT (  '', '', ( #41308 ) ) ;
#17758 = LINE ( 'NONE', #9773, #53734 ) ;
#17759 = LINE ( 'NONE', #2805, #9945 ) ;
#17760 = CARTESIAN_POINT ( 'NONE',  ( -0.5280093414736000135, -78.86429488387997822, -11.14507989169999824 ) ) ;
#17761 = CARTESIAN_POINT ( 'NONE',  ( -12.50483450104916194, -53.93545458963708938, 0.6958188033158416719 ) ) ;
#17762 = CARTESIAN_POINT ( 'NONE',  ( -9.723199427802001082, -54.32306055813000256, 7.958735710007999842 ) ) ;
#17763 = PRODUCT_DEFINITION_SHAPE ( 'NONE', 'NONE',  #45957 ) ;
#17764 = CARTESIAN_POINT ( 'NONE',  ( -11.14010510836999934, -77.86114773376000642, -5.166607915801000317 ) ) ;
#17765 = CARTESIAN_POINT ( 'NONE',  ( -1.199500263597270022, -81.05208333333335702, -0.9218200799623730290 ) ) ;
#17766 = DIRECTION ( 'NONE',  ( 0.7071067811865475727, 0.000000000000000000, 0.7071067811865475727 ) ) ;
#17767 = CARTESIAN_POINT ( 'NONE',  ( -8.084233020759592492, -79.64022715548099995, 7.554717540679545706 ) ) ;
#17768 = CARTESIAN_POINT ( 'NONE',  ( -12.00000000000000000, -55.54999999966999980, 1.250000000000000000 ) ) ;
#17769 = ORIENTED_EDGE ( 'NONE', *, *, #49858, .T. ) ;
#17770 = EDGE_LOOP ( 'NONE', ( #668, #37997, #41293, #26928 ) ) ;
#17771 = CARTESIAN_POINT ( 'NONE',  ( 10.54627086670829428, -78.83456760177642764, -2.082643228401557245 ) ) ;
#17772 = ADVANCED_FACE ( 'NONE', ( #48816 ), #9248, .F. ) ;
#17773 = ORIENTED_EDGE ( 'NONE', *, *, #47567, .T. ) ;
#17774 = CARTESIAN_POINT ( 'NONE',  ( -8.619769076539709474, -79.78588492011769517, -4.179965034922113354 ) ) ;
#17775 = ORIENTED_EDGE ( 'NONE', *, *, #31865, .T. ) ;
#17776 = CARTESIAN_POINT ( 'NONE',  ( 3.123036614452256110, -82.55416668342336095, 1.451080448598909944 ) ) ;
#17777 = CARTESIAN_POINT ( 'NONE',  ( 11.01479880718999915, -77.88671134015899611, -0.6131407820820000687 ) ) ;
#17778 = AXIS2_PLACEMENT_3D ( 'NONE', #53151, #7984, #2988 ) ;
#17779 = CARTESIAN_POINT ( 'NONE',  ( 7.356278612544847384, -55.49583131490126675, -8.178338515874344239 ) ) ;
#17780 = CARTESIAN_POINT ( 'NONE',  ( -5.644471715163000169, -78.11696332859899883, 8.009852484315999277 ) ) ;
#17781 = CARTESIAN_POINT ( 'NONE',  ( 14.00000000000000000, -91.29999999999999716, 0.000000000000000000 ) ) ;
#17782 = CARTESIAN_POINT ( 'NONE',  ( -8.286771986066998608, -78.63946634065099772, 7.559597915363999832 ) ) ;
#17783 = CARTESIAN_POINT ( 'NONE',  ( 0.8704580601414534380, -79.41396526092823649, 0.8969229247981558295 ) ) ;
#17784 = EDGE_CURVE ( 'NONE', #21964, #2879, #21334, .T. ) ;
#17785 = VERTEX_POINT ( 'NONE', #9542 ) ;
#17786 = ORIENTED_EDGE ( 'NONE', *, *, #55271, .F. ) ;
#17787 = CARTESIAN_POINT ( 'NONE',  ( 2.599724825704791797, -77.45250025653473358, 8.877253526477543843 ) ) ;
#17788 = CARTESIAN_POINT ( 'NONE',  ( -3.203604947276999848, -77.76827721380398373, 10.56508708803000118 ) ) ;
#17789 = ADVANCED_FACE ( 'NONE', ( #17509 ), #48804, .T. ) ;
#17790 = CARTESIAN_POINT ( 'NONE',  ( 0.000000000000000000, -87.64999999984398471, 0.000000000000000000 ) ) ;
#17791 = CARTESIAN_POINT ( 'NONE',  ( -9.685922776715001348, -77.32527468639298718, 0.5943755449006998814 ) ) ;
#17792 = CARTESIAN_POINT ( 'NONE',  ( -12.65069897394999998, -75.74449986905000287, -0.01932388167793000142 ) ) ;
#17793 = AXIS2_PLACEMENT_3D ( 'NONE', #32795, #46132, #27502 ) ;
#17794 = CARTESIAN_POINT ( 'NONE',  ( -8.817229174565222038, -79.43036102351236138, -3.552007249728367455 ) ) ;
#17795 = CARTESIAN_POINT ( 'NONE',  ( 7.921329716846313040, -54.24906234234291702, -10.04564005580055053 ) ) ;
#17796 = DIRECTION ( 'NONE',  ( -0.4045626182446106500, -0.8201574091832195545, -0.4045626182446106500 ) ) ;
#17797 = CARTESIAN_POINT ( 'NONE',  ( 12.44209697062000153, -17.91557297456000342, -1.464771213333999844 ) ) ;
#17798 = CARTESIAN_POINT ( 'NONE',  ( -10.36289662401999934, -23.20106470441999846, -7.633500902327000404 ) ) ;
#17799 = CARTESIAN_POINT ( 'NONE',  ( 10.07627163191000008, -23.24999999688999708, -7.601397897754999633 ) ) ;
#17800 = VERTEX_POINT ( 'NONE', #35204 ) ;
#17801 = CARTESIAN_POINT ( 'NONE',  ( 9.131668046799001459, -79.13259514667099381, -8.265509513333999081 ) ) ;
#17802 = CARTESIAN_POINT ( 'NONE',  ( 10.84835523999000095, -76.43206733076499404, -3.797607751403000442 ) ) ;
#17803 = CARTESIAN_POINT ( 'NONE',  ( -3.181107275394350786, -77.99900448743609616, 10.27437500099360079 ) ) ;
#17804 = CARTESIAN_POINT ( 'NONE',  ( 11.53501176087999980, -78.86214129242399906, -3.234124663588000104 ) ) ;
#17805 = CARTESIAN_POINT ( 'NONE',  ( 1.997276839918466829, -3.322916666666666075, 2.598917237794090784 ) ) ;
#17807 = CARTESIAN_POINT ( 'NONE',  ( -1.761265949708000100, -18.29141781213999707, -12.57448205042999945 ) ) ;
#17806 = CARTESIAN_POINT ( 'NONE',  ( -0.5999999999999999778, -5.200000000000000178, -0.5999999999999999778 ) ) ;
#17808 = EDGE_CURVE ( 'NONE', #51923, #4102, #53236, .T. ) ;
#17809 = CARTESIAN_POINT ( 'NONE',  ( 9.723174507645000020, -61.27697503925999456, 7.958760295356000825 ) ) ;
#17810 = CARTESIAN_POINT ( 'NONE',  ( 10.24998526317999925, -57.04916621739000249, -7.705142895613999343 ) ) ;
#17811 = CARTESIAN_POINT ( 'NONE',  ( -9.499999999999998224, -78.31041666666665435, -1.243547092045960367 ) ) ;
#17812 = CARTESIAN_POINT ( 'NONE',  ( 9.608679508909999001, -77.18343933509500232, 5.650475968096999146 ) ) ;
#17813 = DIRECTION ( 'NONE',  ( 0.000000000000000000, 1.000000000000000000, 0.000000000000000000 ) ) ;
#17814 = CARTESIAN_POINT ( 'NONE',  ( -3.497194500561336294, -0.7605524168492561188, -0.4641820427686449424 ) ) ;
#17815 = ORIENTED_EDGE ( 'NONE', *, *, #30139, .F. ) ;
#17816 = CARTESIAN_POINT ( 'NONE',  ( -5.148784662568076406E-06, -79.56241750339395935, -9.437165819784945953 ) ) ;
#17817 = CARTESIAN_POINT ( 'NONE',  ( 0.4450739772405999939, -53.92186785164999918, 12.43586747591000119 ) ) ;
#17818 = DIRECTION ( 'NONE',  ( -0.7071067811865474617, 0.000000000000000000, 0.7071067811865474617 ) ) ;
#17819 = CARTESIAN_POINT ( 'NONE',  ( -3.702886505537000161, -1.801356099613000250, 0.2188527041987999855 ) ) ;
#17820 = AXIS2_PLACEMENT_3D ( 'NONE', #6018, #24028, #32574 ) ;
#17821 = CARTESIAN_POINT ( 'NONE',  ( 2.974672214138999848, -79.30668661348099135, 9.057689976529999853 ) ) ;
#17822 = DIRECTION ( 'NONE',  ( 0.000000000000000000, 0.000000000000000000, -1.000000000000000000 ) ) ;
#17823 = CARTESIAN_POINT ( 'NONE',  ( 3.630949683904999947, -79.79999999999999716, -11.17491406647000041 ) ) ;
#17824 = CARTESIAN_POINT ( 'NONE',  ( -0.8537148449456000154, -61.50498145875999256, 12.43377424877000159 ) ) ;
#17825 = CARTESIAN_POINT ( 'NONE',  ( 12.46083735080000032, -18.31664398787999559, 1.628985986889000204 ) ) ;
#17826 = EDGE_CURVE ( 'NONE', #1911, #15146, #31067, .T. ) ;
#17827 = CARTESIAN_POINT ( 'NONE',  ( 0.3144812618505000157, -82.86349735065198274, 4.163017894414998921 ) ) ;
#17828 = TOROIDAL_SURFACE ( 'NONE', #22543, 9.000000000000000000, 0.5000000000000000000 ) ;
#17829 = DIRECTION ( 'NONE',  ( -0.7071067811865475727, 0.000000000000000000, 0.7071067811865475727 ) ) ;
#17830 = EDGE_CURVE ( 'NONE', #13664, #51037, #55858, .T. ) ;
#17831 = CARTESIAN_POINT ( 'NONE',  ( 0.1323022290353233765, -77.07890511624708552, -12.02134639614113709 ) ) ;
#17832 = CARTESIAN_POINT ( 'NONE',  ( 4.579136177892999982, -78.91051207264999334, -11.61209283926000069 ) ) ;
#17833 = CARTESIAN_POINT ( 'NONE',  ( 6.393694643109999909, -77.38247520153299774, -9.131005934809000024 ) ) ;
#17834 = CARTESIAN_POINT ( 'NONE',  ( 0.2617232932829000047, -79.34874659015000020, -1.644907507304999905 ) ) ;
#17835 = CARTESIAN_POINT ( 'NONE',  ( -1.288905872365999850, -79.49283985636999716, -0.6300432575161000193 ) ) ;
#17836 = CARTESIAN_POINT ( 'NONE',  ( -3.591972190522999764, -77.29573314074899315, 8.980252640667000463 ) ) ;
#17837 = CARTESIAN_POINT ( 'NONE',  ( -1.007661242079784136, -82.68318653106200600, 1.124876851017058588 ) ) ;
#17838 = CARTESIAN_POINT ( 'NONE',  ( -12.57354097144999905, -60.52384125708999818, 1.757953070309000054 ) ) ;
#17839 = CARTESIAN_POINT ( 'NONE',  ( -1.491254300649823561, -80.21401151211460956, -10.64863931018329879 ) ) ;
#17840 = CARTESIAN_POINT ( 'NONE',  ( 12.50000000000000000, -24.68359816828999698, 1.003641515614000168 ) ) ;
#17841 = CARTESIAN_POINT ( 'NONE',  ( -11.20005099196198195, -78.84553010071444135, 0.6168198611958737310 ) ) ;
#17842 = AXIS2_PLACEMENT_3D ( 'NONE', #8408, #26406, #49156 ) ;
#17843 = CARTESIAN_POINT ( 'NONE',  ( 12.54435570279975387, -55.27582218184407026, -1.733918077762380827 ) ) ;
#17844 = CARTESIAN_POINT ( 'NONE',  ( -0.9820397338569999413, -80.80308451575899653, -0.7733679338621000099 ) ) ;
#17845 = CARTESIAN_POINT ( 'NONE',  ( 6.760013919724070064, -79.42291666666666572, 8.796335266379976758 ) ) ;
#17846 = CARTESIAN_POINT ( 'NONE',  ( -10.33279081301000168, -79.92173935843149479, -4.181869747484999955 ) ) ;
#17847 = CARTESIAN_POINT ( 'NONE',  ( -0.7681833999686432657, -80.07291666666668561, -0.9995835529977258327 ) ) ;
#17848 = ORIENTED_EDGE ( 'NONE', *, *, #887, .F. ) ;
#17849 = ORIENTED_EDGE ( 'NONE', *, *, #1288, .T. ) ;
#17850 = CARTESIAN_POINT ( 'NONE',  ( 1.445601399883000182, -81.70519910015499931, -0.7193403082786999914 ) ) ;
#17851 = ORIENTED_EDGE ( 'NONE', *, *, #1000, .F. ) ;
#17852 = DIRECTION ( 'NONE',  ( -1.000000000000000000, 0.000000000000000000, 0.000000000000000000 ) ) ;
#17853 = ORIENTED_EDGE ( 'NONE', *, *, #2244, .F. ) ;
#17854 = DIRECTION ( 'NONE',  ( 0.000000000000000000, -1.000000000000000000, 0.000000000000000000 ) ) ;
#17855 = CARTESIAN_POINT ( 'NONE',  ( 11.10498291493000167, -80.08699962660007543, -1.830582403018000015 ) ) ;
#17856 = CARTESIAN_POINT ( 'NONE',  ( 2.853743189566999534E-14, -82.05000000008600125, 0.000000000000000000 ) ) ;
#17857 = CARTESIAN_POINT ( 'NONE',  ( 3.315825420378000210, -79.29043055640599391, -10.52174111842000137 ) ) ;
#17858 = CARTESIAN_POINT ( 'NONE',  ( 2.817594599424999569, -80.97881882065600223, -2.223714431971000050 ) ) ;
#17859 = CARTESIAN_POINT ( 'NONE',  ( -1.760571071064350956, -79.28971201036856087, 9.336322274714841996 ) ) ;
#17860 = ORIENTED_EDGE ( 'NONE', *, *, #7817, .F. ) ;
#17861 = CARTESIAN_POINT ( 'NONE',  ( 8.680753609988000719, -77.65300022429065052, 6.821192461343000168 ) ) ;
#17862 = CARTESIAN_POINT ( 'NONE',  ( -12.35615978905999945, -79.00715997148999747, -0.2389464526812000167 ) ) ;
#17863 = VERTEX_POINT ( 'NONE', #2992 ) ;
#17864 = ORIENTED_EDGE ( 'NONE', *, *, #43250, .T. ) ;
#17865 = CARTESIAN_POINT ( 'NONE',  ( 1.250000000000000000, -60.24678171298000251, -12.50000000000000000 ) ) ;
#17866 = DIRECTION ( 'NONE',  ( -0.7071067811865474617, -0.7071067811865474617, -3.010159793144197746E-10 ) ) ;
#17867 = EDGE_CURVE ( 'NONE', #43853, #40579, #56240, .T. ) ;
#17868 = CARTESIAN_POINT ( 'NONE',  ( -1.327128730425999992, -79.75779867290000880, 0.1315503032697999675 ) ) ;
#17869 = CARTESIAN_POINT ( 'NONE',  ( 4.746041175454999816, -77.37521180982498947, -8.464384343845999581 ) ) ;
#17870 = CONICAL_SURFACE ( 'NONE', #47096, 4.199999999676998996, 0.7853981633972997312 ) ;
#17871 = CARTESIAN_POINT ( 'NONE',  ( -4.580541315389114132, -86.25171438276197478, -0.4384716419589351766 ) ) ;
#17872 = FACE_BOUND ( 'NONE', #38187, .T. ) ;
#17873 = CARTESIAN_POINT ( 'NONE',  ( -1.169957374810000061, -76.94917510722000031, -12.74520906849999946 ) ) ;
#17874 = CARTESIAN_POINT ( 'NONE',  ( 1.258195058187999926, -80.85973563566999189, 0.4928692076250000276 ) ) ;
#17875 = CARTESIAN_POINT ( 'NONE',  ( 4.834410198815040971, -77.71759693750338727, -8.116238590442467427 ) ) ;
#17876 = DIRECTION ( 'NONE',  ( 0.000000000000000000, 1.000000000000000000, -6.735242868878000753E-11 ) ) ;
#17877 = CARTESIAN_POINT ( 'NONE',  ( 0.8807763160617000375, -81.57621146183899441, 3.863964706566999752 ) ) ;
#17878 = CIRCLE ( 'NONE', #4646, 13.86363636363999952 ) ;
#17879 = CARTESIAN_POINT ( 'NONE',  ( 11.99999999999999822, -76.56041666666666856, 1.570796326794923203 ) ) ;
#17880 = CARTESIAN_POINT ( 'NONE',  ( -5.489853033850980779, -76.78607156998435812, -10.46842530689402828 ) ) ;
#17881 = CARTESIAN_POINT ( 'NONE',  ( -1.280698150711000238, -78.93025264934789220, -3.305257395273999865 ) ) ;
#17882 = AXIS2_PLACEMENT_3D ( 'NONE', #44217, #21766, #17340 ) ;
#17883 = ADVANCED_FACE ( 'NONE', ( #57004 ), #23227, .F. ) ;
#17884 = CARTESIAN_POINT ( 'NONE',  ( 5.246383657897999875, -77.46100733245999947, -10.79237965019999912 ) ) ;
#17885 = CARTESIAN_POINT ( 'NONE',  ( -9.578166812159000898, -80.28977840746540551, 5.930253639820000089 ) ) ;
#17886 = CARTESIAN_POINT ( 'NONE',  ( 1.432628882339999965, -2.438376846448000013, -3.526139092948999743 ) ) ;
#17887 = CARTESIAN_POINT ( 'NONE',  ( 0.3449928021110761911, -80.10361832643582147, 1.227624333057440120 ) ) ;
#17888 = EDGE_LOOP ( 'NONE', ( #55558, #16121, #24816, #51390 ) ) ;
#17889 = DIRECTION ( 'NONE',  ( -1.000000000000000000, 0.000000000000000000, 0.000000000000000000 ) ) ;
#17890 = EDGE_CURVE ( 'NONE', #17264, #57279, #56357, .T. ) ;
#17891 = CARTESIAN_POINT ( 'NONE',  ( 10.75000000000000000, -79.25000000000000000, 0.000000000000000000 ) ) ;
#17892 = CARTESIAN_POINT ( 'NONE',  ( -0.1187445621502999926, -81.29601814238500879, -1.328335755224000048 ) ) ;
#17893 = CARTESIAN_POINT ( 'NONE',  ( -12.46083735080000032, -18.31664398787999559, -1.628985986889000204 ) ) ;
#17894 = CARTESIAN_POINT ( 'NONE',  ( -1.338697082642999803, -78.13413240273000326, -12.94399764267999942 ) ) ;
#17895 = MANIFOLD_SOLID_BREP ( 'Stock-MAS-694-1', #16414 ) ;
#17896 = CARTESIAN_POINT ( 'NONE',  ( 6.529408856002000050, -79.19118667140099888, -7.077026392590000548 ) ) ;
#17897 = CARTESIAN_POINT ( 'NONE',  ( -12.03549681466000010, -76.47233804731999385, 3.421427826494999991 ) ) ;
#17898 = VERTEX_POINT ( 'NONE', #7127 ) ;
#17899 = EDGE_CURVE ( 'NONE', #34384, #38110, #6545, .T. ) ;
#17900 = CARTESIAN_POINT ( 'NONE',  ( 7.919595949288999570, -59.94999999040999938, -9.050966798898000931 ) ) ;
#17901 = CARTESIAN_POINT ( 'NONE',  ( 0.07256738472693000097, -81.61253423276301078, 1.308646213179999851 ) ) ;
#17902 = CARTESIAN_POINT ( 'NONE',  ( -1.930989179114000143, -20.24546192895000019, -12.80896991329000123 ) ) ;
#17903 = CARTESIAN_POINT ( 'NONE',  ( 9.521438313890000060, -77.70787555610998254, 0.1121992162086000028 ) ) ;
#17905 = CARTESIAN_POINT ( 'NONE',  ( -0.7824435345810000220, -1.742598507946000019, 3.939770163431000061 ) ) ;
#17904 = CARTESIAN_POINT ( 'NONE',  ( 3.766997394601000249, -82.17775871403298993, -1.388144962921000092 ) ) ;
#17906 = CARTESIAN_POINT ( 'NONE',  ( -0.6295237254636286695, -82.41666666666667140, 1.092232985442819881 ) ) ;
#17907 = CARTESIAN_POINT ( 'NONE',  ( 1.243995776054000135, -79.89249923068300063, 0.6800984409344000836 ) ) ;
#17908 = ORIENTED_EDGE ( 'NONE', *, *, #41685, .T. ) ;
#17909 = CARTESIAN_POINT ( 'NONE',  ( -3.586356261501751685, -77.19801135428419059, -10.13419940784981499 ) ) ;
#17910 = DIRECTION ( 'NONE',  ( 0.000000000000000000, 0.000000000000000000, 1.000000000000000000 ) ) ;
#17911 = EDGE_LOOP ( 'NONE', ( #40050, #32934, #9003, #56193 ) ) ;
#17912 = ORIENTED_EDGE ( 'NONE', *, *, #19838, .F. ) ;
#17913 = PLANE ( 'NONE',  #962 ) ;
#17914 = EDGE_CURVE ( 'NONE', #31619, #34639, #46006, .T. ) ;
#17915 = CARTESIAN_POINT ( 'NONE',  ( -9.422718869893611071, -76.08255208300656136, -7.240326068120862324 ) ) ;
#17916 = DIRECTION ( 'NONE',  ( 0.4045626180513098857, -0.8201574093739200100, 0.4045626180513098857 ) ) ;
#17917 = ORIENTED_EDGE ( 'NONE', *, *, #683, .T. ) ;
#17918 = CARTESIAN_POINT ( 'NONE',  ( 1.628430890020000188, -78.98730299628599028, 11.59185972383999896 ) ) ;
#17919 = EDGE_LOOP ( 'NONE', ( #2320, #16905, #39657, #41606 ) ) ;
#17920 = B_SPLINE_SURFACE_WITH_KNOTS ( 'NONE', 3, 3, ( 
 ( #41629, #37480, #1209, #19201, #29202, #42224, #55206, #10639, #51090, #28621, #46666, #6193, #46959, #6779, #20079, #24206, #1789, #19785, #37779, #55800, #15351, #10934, #11223, #47247, #24787, #53375, #57232, #56947, #43369, #21504, #16797, #34781, #11792, #16220, #39511 ),
 ( #52805, #34489, #17076, #20646, #52236, #53093, #57805, #17365, #44234, #26218, #30347, #12645, #38930, #29767, #25354, #25071, #21788, #56664, #43665, #8216, #12076, #3787, #47824, #39792, #7354, #12358, #34198, #43094, #35351, #2928, #12924, #3502, #7640, #35058, #30638 ),
 ( #20929, #16507, #47545, #48108, #52519, #25640, #7069, #2652, #48672, #30057, #57516, #3224, #21211, #39219, #48389, #7927, #25927, #43951, #41272, #9101, #36546, #22679, #32104, #50145, #18552, #14107, #40390, #22972, #35650, #53678, #36254, #9688, #31212, #54568, #27675 ),
 ( #13809, #45721, #5256, #31811, #40982, #49251, #856, #18840, #573, #23263, #48960, #4377, #36833, #13218, #45423, #54846, #8503, #26794, #26498, #44522, #17663, #4073, #22075, #40084, #27091, #8802, #35952, #44823, #58399, #17961, #53978, #49853, #13517, #27387, #31511 ) ),
 .UNSPECIFIED., .F., .F., .F.,
 ( 4, 4 ),
 ( 4, 1, 1, 1, 1, 1, 1, 1, 1, 1, 1, 1, 1, 1, 1, 1, 1, 1, 1, 1, 1, 1, 1, 1, 1, 1, 1, 1, 1, 1, 1, 1, 4 ),
 ( -0.1331668876848000060, 1.133166887685000068 ),
 ( -0.02000000000000000042, 0.01250000000000000069, 0.04499999999999999833, 0.07749999999999999944, 0.1100000000000000006, 0.1424999999999999878, 0.1749999999999999889, 0.2074999999999999900, 0.2399999999999999911, 0.2725000000000000200, 0.3049999999999999933, 0.3375000000000000222, 0.3699999999999999956, 0.4025000000000000244, 0.4349999999999999978, 0.4675000000000000266, 0.5000000000000000000, 0.5324999999999999734, 0.5649999999999999467, 0.5975000000000000311, 0.6300000000000000044, 0.6624999999999999778, 0.6949999999999999512, 0.7275000000000000355, 0.7600000000000000089, 0.7924999999999999822, 0.8249999999999999556, 0.8575000000000000400, 0.8900000000000000133, 0.9224999999999999867, 0.9549999999999999600, 0.9875000000000000444, 1.020000000000000018 ),
 .UNSPECIFIED. ) ;
#17921 = ORIENTED_EDGE ( 'NONE', *, *, #32409, .F. ) ;
#17922 = VECTOR ( 'NONE', #49131, 1000.000000000000000 ) ;
#17923 = CARTESIAN_POINT ( 'NONE',  ( -3.250000000000000000, -2.600000000000000089, 0.000000000000000000 ) ) ;
#17924 = CARTESIAN_POINT ( 'NONE',  ( -2.899999999999999911, -80.69999999999998863, 0.000000000000000000 ) ) ;
#17925 = CARTESIAN_POINT ( 'NONE',  ( 12.50000000000000000, -23.44678171330999916, 1.250000000000000000 ) ) ;
#17926 = ORIENTED_EDGE ( 'NONE', *, *, #49819, .T. ) ;
#17927 = CARTESIAN_POINT ( 'NONE',  ( -0.7555692214694499365, -81.81679953337950906, 1.310938934338384154 ) ) ;
#17928 = ORIENTED_EDGE ( 'NONE', *, *, #9736, .T. ) ;
#17929 = CARTESIAN_POINT ( 'NONE',  ( 0.09625703868715393408, -79.78079856828991012, -1.271375911578840778 ) ) ;
#17930 = CARTESIAN_POINT ( 'NONE',  ( -11.96333271148828281, -79.79999999999996874, -0.9383198194705477668 ) ) ;
#17931 = CARTESIAN_POINT ( 'NONE',  ( -7.601397897754999633, -55.55000000278000272, 10.07627163191000008 ) ) ;
#17932 = CARTESIAN_POINT ( 'NONE',  ( -7.668949790020999302, -19.22870851082999977, -10.21381326473999884 ) ) ;
#17933 = CARTESIAN_POINT ( 'NONE',  ( -5.915616301254464915, -77.28183550628908449, -10.26021406754873233 ) ) ;
#17934 = CARTESIAN_POINT ( 'NONE',  ( 12.70556836352000118, -62.02772277195000328, 2.424222323408999617E-09 ) ) ;
#17935 = CARTESIAN_POINT ( 'NONE',  ( 7.642160924878999673, -59.58461666436000570, -10.55911395187000146 ) ) ;
#17936 = CARTESIAN_POINT ( 'NONE',  ( 6.559075508479975447, -78.78789540257247381, -6.522196071853445076 ) ) ;
#17937 = CIRCLE ( 'NONE', #25475, 12.50000000000000000 ) ;
#17938 = LINE ( 'NONE', #17057, #35768 ) ;
#17939 = DIRECTION ( 'NONE',  ( 0.7071067811865475727, 0.000000000000000000, 0.7071067811865475727 ) ) ;
#17940 = CARTESIAN_POINT ( 'NONE',  ( -3.811312777322000134, -78.56950264934789629, 1.220744239273999998 ) ) ;
#17941 = CARTESIAN_POINT ( 'NONE',  ( -1.311199674450999941, -77.43506001420199425, -9.785292850414998966 ) ) ;
#17942 = CARTESIAN_POINT ( 'NONE',  ( -12.77657003524999979, -16.68789974453000369, 0.1588669551757000142 ) ) ;
#17943 = EDGE_CURVE ( 'NONE', #23718, #6742, #17158, .T. ) ;
#17944 = CARTESIAN_POINT ( 'NONE',  ( 8.800000000000000711, 0.000000000000000000, 0.000000000000000000 ) ) ;
#17945 = CYLINDRICAL_SURFACE ( 'NONE', #16323, 1.250000000000000000 ) ;
#17946 = CARTESIAN_POINT ( 'NONE',  ( 3.500000000000000000, -3.500000000000000000, 1.049058100190999900E-13 ) ) ;
#17947 = LINE ( 'NONE', #36238, #58061 ) ;
#17948 = CARTESIAN_POINT ( 'NONE',  ( -1.342840445321999976, -1.150401880087000173, -3.364826939129000216 ) ) ;
#17949 = CARTESIAN_POINT ( 'NONE',  ( 7.651160336697000020, -56.03767313780999615, 10.45205658995000064 ) ) ;
#17950 = CARTESIAN_POINT ( 'NONE',  ( -0.06678984038673288492, -80.97078420075510508, -1.509580312845645533 ) ) ;
#17951 = CARTESIAN_POINT ( 'NONE',  ( 12.66235429711000116, -61.93741783389999966, -0.4955846680318000130 ) ) ;
#17952 = CARTESIAN_POINT ( 'NONE',  ( -1.265160441076000009, -79.39322140577399978, -0.7115061034973000353 ) ) ;
#17953 = CARTESIAN_POINT ( 'NONE',  ( -13.63885489310999510, -22.78578169018999944, -7.254376133916000668 ) ) ;
#17954 = CARTESIAN_POINT ( 'NONE',  ( 10.78933672403999999, -77.26442077791699603, -1.663003020634000073 ) ) ;
#17955 = VECTOR ( 'NONE', #22181, 1000.000000000000000 ) ;
#17956 = CARTESIAN_POINT ( 'NONE',  ( 0.3923696854197999961, -77.06875387357798957, -11.92498586577000097 ) ) ;
#17957 = CARTESIAN_POINT ( 'NONE',  ( 0.000000000000000000, -77.49999999999998579, 0.000000000000000000 ) ) ;
#17958 = CARTESIAN_POINT ( 'NONE',  ( -10.47020627418439354, -79.02083333333332860, -2.813789756862263847 ) ) ;
#17960 = CARTESIAN_POINT ( 'NONE',  ( 1.326698500471999997, -79.06247058323299370, -0.7340390780227000755 ) ) ;
#17959 = DIRECTION ( 'NONE',  ( 0.000000000000000000, -1.000000000000000000, -2.922721309575999778E-13 ) ) ;
#17961 = CARTESIAN_POINT ( 'NONE',  ( 1.647188161489999914, -81.54038421936999725, 0.4319573417677999849 ) ) ;
#17962 = ORIENTED_EDGE ( 'NONE', *, *, #46535, .F. ) ;
#17963 = EDGE_CURVE ( 'NONE', #31041, #8076, #49314, .T. ) ;
#17964 = CARTESIAN_POINT ( 'NONE',  ( -1.490776890111999986, -83.11557450217399889, 3.265167628442000147 ) ) ;
#17965 = CARTESIAN_POINT ( 'NONE',  ( 0.000000000000000000, -77.59999999938000315, 0.000000000000000000 ) ) ;
#17966 = CARTESIAN_POINT ( 'NONE',  ( -6.925639247002999710, -80.71293126068253798, -8.766942257001000272 ) ) ;
#17967 = FACE_OUTER_BOUND ( 'NONE', #9638, .T. ) ;
#17968 = DIRECTION ( 'NONE',  ( 0.000000000000000000, 0.000000000000000000, 1.000000000000000000 ) ) ;
#17969 = CARTESIAN_POINT ( 'NONE',  ( -3.513443458492000016, -78.50133016130298813, -10.65240647004999985 ) ) ;
#17970 = CARTESIAN_POINT ( 'NONE',  ( -10.47840054248000108, -60.58693148419000352, 7.622763498592000531 ) ) ;
#17971 = CARTESIAN_POINT ( 'NONE',  ( 9.697485508432000856, -79.08658701837899230, 0.9045115177663000106 ) ) ;
#17972 = CARTESIAN_POINT ( 'NONE',  ( 5.354686402641000598, -77.09581360186999177, 11.45119097547000031 ) ) ;
#17973 = LINE ( 'NONE', #31224, #37799 ) ;
#17974 = CARTESIAN_POINT ( 'NONE',  ( 12.55458806505999902, -24.16283916848999880, -1.575041344316999936 ) ) ;
#17975 = CARTESIAN_POINT ( 'NONE',  ( -7.850068286643266724, -54.48530314308822398, -9.837745659579251623 ) ) ;
#17976 = EDGE_LOOP ( 'NONE', ( #19377, #12165, #57819 ) ) ;
#17977 = CARTESIAN_POINT ( 'NONE',  ( -1.689459950992686865, -54.50811746068543329, -12.71013585606787366 ) ) ;
#17978 = CYLINDRICAL_SURFACE ( 'NONE', #25058, 9.549999999999998934 ) ;
#17979 = DIRECTION ( 'NONE',  ( 0.000000000000000000, 1.000000000000000000, 0.000000000000000000 ) ) ;
#17980 = EDGE_CURVE ( 'NONE', #23438, #55197, #3056, .T. ) ;
#17981 = CARTESIAN_POINT ( 'NONE',  ( -0.3926218265389189721, -81.50416666666666288, -1.460959015002473604 ) ) ;
#17982 = CARTESIAN_POINT ( 'NONE',  ( 0.2617232932829000047, -79.52639556175999758, -1.644907507304999905 ) ) ;
#17983 = ADVANCED_FACE ( 'NONE', ( #13280 ), #53744, .F. ) ;
#17984 = ORIENTED_EDGE ( 'NONE', *, *, #21885, .F. ) ;
#17985 = AXIS2_PLACEMENT_3D ( 'NONE', #6132, #24139, #42158 ) ;
#17986 = CARTESIAN_POINT ( 'NONE',  ( -10.82992633042000108, -77.44682768747698276, -2.440973915835000341 ) ) ;
#17987 = CARTESIAN_POINT ( 'NONE',  ( 11.15483436911470072, -77.92097904722264445, -3.785860825438485566 ) ) ;
#17988 = CARTESIAN_POINT ( 'NONE',  ( -1.667917367010000040, -23.28056692670000061, 12.49306752634999995 ) ) ;
#17989 = ORIENTED_EDGE ( 'NONE', *, *, #29098, .T. ) ;
#17990 = EDGE_LOOP ( 'NONE', ( #16688, #56840, #34160, #38664 ) ) ;
#17991 = CARTESIAN_POINT ( 'NONE',  ( -10.30768118222999874, -55.05239703883000146, -7.634415485482000108 ) ) ;
#17992 = CARTESIAN_POINT ( 'NONE',  ( 3.269429986698999979, -79.67799007979499493, 9.203886808668999109 ) ) ;
#17993 = EDGE_LOOP ( 'NONE', ( #33738, #52204, #18261, #13473 ) ) ;
#17994 = CARTESIAN_POINT ( 'NONE',  ( -7.694727692044000200, -76.76262287232799508, -9.663281825523000634 ) ) ;
#17995 = CARTESIAN_POINT ( 'NONE',  ( -9.337414570838035388, -78.64153581994834497, -5.340065548460428246 ) ) ;
#17996 = CIRCLE ( 'NONE', #51934, 0.5000000000000004441 ) ;
#17997 = CARTESIAN_POINT ( 'NONE',  ( 1.543541483667999925, -79.04849869623998870, 0.5782440448787000697 ) ) ;
#17998 = ORIENTED_EDGE ( 'NONE', *, *, #27017, .T. ) ;
#17999 = CARTESIAN_POINT ( 'NONE',  ( -7.264520526674999701, -77.62562305011499575, -6.114261184555999762 ) ) ;
#18000 = CARTESIAN_POINT ( 'NONE',  ( 8.485281374238999419, -55.54999999966999980, -8.485281374238999419 ) ) ;
#18001 = CARTESIAN_POINT ( 'NONE',  ( 0.03063463627522158145, -80.22746756300657012, -1.249376046788328809 ) ) ;
#18002 = CARTESIAN_POINT ( 'NONE',  ( -10.63665183518000035, -77.94466387191998535, 7.669898027128999374 ) ) ;
#18003 = CARTESIAN_POINT ( 'NONE',  ( -2.185791986076000004, -77.85939354152488079, -11.00183730042999564 ) ) ;
#18004 = CARTESIAN_POINT ( 'NONE',  ( -2.409209601448000893, -86.31452042059399332, 3.252055376540964104 ) ) ;
#18005 = CARTESIAN_POINT ( 'NONE',  ( 3.113304451009999863, -78.49783470746899638, -10.55022916317000181 ) ) ;
#18006 = CARTESIAN_POINT ( 'NONE',  ( 7.032896718443679696, -79.90636255966268209, 6.008298471892056902 ) ) ;
#18007 = CARTESIAN_POINT ( 'NONE',  ( -0.2823905925365536862, -80.07332856916835340, -11.10458707158487890 ) ) ;
#18008 = ORIENTED_EDGE ( 'NONE', *, *, #15950, .T. ) ;
#18009 = CARTESIAN_POINT ( 'NONE',  ( -12.00000000000000000, -60.04999999966999980, 1.250000000000000000 ) ) ;
#18010 = CARTESIAN_POINT ( 'NONE',  ( -0.4674429229059374746, -77.22105961193567225, -9.250557976676333283 ) ) ;
#18011 = CARTESIAN_POINT ( 'NONE',  ( -0.7332490996008999007, -80.49554665869699477, -1.438596428395999993 ) ) ;
#18012 = CARTESIAN_POINT ( 'NONE',  ( 0.9728932632037999850, -78.96706751772300947, 0.8910916192982000217 ) ) ;
#18013 = CARTESIAN_POINT ( 'NONE',  ( -0.4732678188519857110, -3.234965057628082619, 3.486999387683345386 ) ) ;
#18014 = CARTESIAN_POINT ( 'NONE',  ( -10.21026245503029450, -17.74392421793578833, 7.764236519581510620 ) ) ;
#18015 = CARTESIAN_POINT ( 'NONE',  ( -10.85634995915000012, -76.24039363648499545, -5.741293403527000017 ) ) ;
#18016 = CARTESIAN_POINT ( 'NONE',  ( -9.502896619458471861, -61.54094210167068013, -8.179425867623026036 ) ) ;
#18017 = CARTESIAN_POINT ( 'NONE',  ( -4.472180980751999435, -79.96475654597900018, 10.22208999787000039 ) ) ;
#18018 = CARTESIAN_POINT ( 'NONE',  ( 9.732069852918000308, -77.63191498579799088, 0.3150258461668000165 ) ) ;
#18019 = CARTESIAN_POINT ( 'NONE',  ( 6.375617654102788912, -77.38048332243674565, 10.18566900156049115 ) ) ;
#18020 = CARTESIAN_POINT ( 'NONE',  ( -13.02337492114030937, -76.45447530479343357, -0.3199942328547237813 ) ) ;
#18021 = CARTESIAN_POINT ( 'NONE',  ( -9.393203674808288994, -77.95833333333331439, 5.413904038987134015 ) ) ;
#18022 = AXIS2_PLACEMENT_3D ( 'NONE', #14924, #10516, #28499 ) ;
#18023 = VERTEX_POINT ( 'NONE', #44293 ) ;
#18024 = CARTESIAN_POINT ( 'NONE',  ( 0.4779442704572000045, -82.04270613248999666, -1.511941137165000004 ) ) ;
#18025 = CARTESIAN_POINT ( 'NONE',  ( -0.4634070002434999558, -79.61543996570000559, -1.170148800580000037 ) ) ;
#18026 = CARTESIAN_POINT ( 'NONE',  ( -10.75000000000000000, -79.10000000000000853, 0.000000000000000000 ) ) ;
#18027 = CARTESIAN_POINT ( 'NONE',  ( -1.250000000000000000, -60.04999999966999980, 12.00000000000000000 ) ) ;
#18028 = CARTESIAN_POINT ( 'NONE',  ( 5.100000000000000533, -76.79999999999999716, 0.000000000000000000 ) ) ;
#18029 = CARTESIAN_POINT ( 'NONE',  ( 0.7311670807272000472, -82.10923396026998944, 1.496881327486000002 ) ) ;
#18030 = CARTESIAN_POINT ( 'NONE',  ( 11.93224739473999918, -77.82818225714999016, 0.2386934378577999782 ) ) ;
#18031 = CARTESIAN_POINT ( 'NONE',  ( -9.631455446501000495, -78.02079415034600629, -1.333735528292999906 ) ) ;
#18032 = CARTESIAN_POINT ( 'NONE',  ( 0.9113424693958999123, -53.97464206407000376, -12.54674099554000044 ) ) ;
#18033 = CARTESIAN_POINT ( 'NONE',  ( 4.498561486224415873, -76.04320336603228725, 10.85439371926396390 ) ) ;
#18034 = CARTESIAN_POINT ( 'NONE',  ( 6.766101950298000212, -79.28132150479699192, 8.713300108436000002 ) ) ;
#18035 = CARTESIAN_POINT ( 'NONE',  ( -0.5677917205626995534, -85.94828561723799965, 4.566314625519897419 ) ) ;
#18036 = ORIENTED_EDGE ( 'NONE', *, *, #57484, .F. ) ;
#18037 = CARTESIAN_POINT ( 'NONE',  ( 7.396918292183153554, -78.80208333333332860, 5.684557159767984480 ) ) ;
#18038 = EDGE_CURVE ( 'NONE', #12786, #5620, #19260, .T. ) ;
#18039 = FACE_OUTER_BOUND ( 'NONE', #40590, .T. ) ;
#18040 = CARTESIAN_POINT ( 'NONE',  ( 3.407095545933004122, -78.62148120184446043, -2.010777145231036567 ) ) ;
#18041 = ADVANCED_FACE ( 'NONE', ( #8143 ), #21322, .T. ) ;
#18042 = CARTESIAN_POINT ( 'NONE',  ( -10.75000000000000000, -77.50000000000000000, 0.000000000000000000 ) ) ;
#18043 = VECTOR ( 'NONE', #37721, 1000.000000000000000 ) ;
#18044 = CARTESIAN_POINT ( 'NONE',  ( 8.318585563179999198, -78.29700886712998908, 7.159970128962999780 ) ) ;
#18045 = DIRECTION ( 'NONE',  ( 0.000000000000000000, 0.000000000000000000, -1.000000000000000000 ) ) ;
#18046 = CARTESIAN_POINT ( 'NONE',  ( 10.48543666025108045, -77.69166666666664867, 6.043427764450817641 ) ) ;
#18047 = CARTESIAN_POINT ( 'NONE',  ( 0.000000000000000000, 4.040000000000000036, 0.000000000000000000 ) ) ;
#18048 = DIRECTION ( 'NONE',  ( -0.7071067811865475727, 0.000000000000000000, -0.7071067811865475727 ) ) ;
#18049 = ORIENTED_EDGE ( 'NONE', *, *, #27832, .T. ) ;
#18050 = VECTOR ( 'NONE', #1162, 1000.000000000000000 ) ;
#18051 = CARTESIAN_POINT ( 'NONE',  ( 2.417503760557000447, -80.13402960327920255, 10.77648496335999972 ) ) ;
#18052 = CARTESIAN_POINT ( 'NONE',  ( 8.267707368506879817, -77.21246842999600801, -4.210867517961808026 ) ) ;
#18053 = CARTESIAN_POINT ( 'NONE',  ( 11.86920293296211959, -75.80000000000001137, -1.874119536907680406 ) ) ;
#18054 = CARTESIAN_POINT ( 'NONE',  ( 3.914500761937000028, -78.48547955770030171, 2.310234098304058126 ) ) ;
#18055 = CARTESIAN_POINT ( 'NONE',  ( -0.5000217545454540558, -81.50798104061337312, 1.145512068557146046 ) ) ;
#18056 = EDGE_CURVE ( 'NONE', #1253, #51275, #6608, .T. ) ;
#18057 = CARTESIAN_POINT ( 'NONE',  ( -8.689005542484000699, -78.25395412067899770, 6.824886543446999632 ) ) ;
#18058 = DIRECTION ( 'NONE',  ( 0.7071067811865475727, 0.000000000000000000, 0.7071067811865475727 ) ) ;
#18059 = CARTESIAN_POINT ( 'NONE',  ( -0.8598574106787247873, -81.42622421550363754, -1.245561739481349850 ) ) ;
#18060 = CARTESIAN_POINT ( 'NONE',  ( 9.722718241315000398, -23.25000000000000000, -7.954951288349001004 ) ) ;
#18061 =( BOUNDED_SURFACE ( )  B_SPLINE_SURFACE ( 3, 3, ( 
 ( #38841, #16994, #51861, #2839, #15834, #47730, #42704 ),
 ( #16128, #16418, #16707, #2271, #34400, #48300, #12271 ),
 ( #52431, #11414, #20268, #25841, #34105, #34689, #56568 ),
 ( #12555, #30260, #11991, #57142, #3417, #52719, #7265 ),
 ( #43868, #29395, #21416, #30553, #48585, #20556, #53004 ),
 ( #34974, #47445, #8130, #33821, #25552, #2555, #29969 ),
 ( #48020, #7554, #21125, #20835, #6973, #24975, #42998 ),
 ( #52147, #29680, #25266, #53889, #44432, #26132, #26995 ),
 ( #45031, #48872, #9300, #191, #44152, #9011, #26702 ),
 ( #3985, #18166, #36159, #3699, #58009, #35560, #21702 ),
 ( #49159, #54179, #21987, #39707, #22874, #14009, #39996 ),
 ( #475, #4582, #35261, #27290, #44733, #17871, #26411 ),
 ( #4284, #22281, #13716, #17271, #13125, #53291, #12837 ),
 ( #45327, #40299, #31711, #36444, #58309, #35861, #17568 ),
 ( #54474, #57714, #30838, #13420, #22583, #31421, #31120 ) ),
 .UNSPECIFIED., .F., .F., .F. ) 
 B_SPLINE_SURFACE_WITH_KNOTS ( ( 4, 1, 1, 1, 1, 1, 1, 1, 1, 1, 1, 1, 4 ),
 ( 4, 3, 4 ),
 ( 0.009836358961777999163, 0.09153385889397000486, 0.1732268882812000033, 0.2549245844128000260, 0.3366128623372000028, 0.4183102317861999708, 0.5000049915032999115, 0.5816997502458999270, 0.6633970872647999562, 0.7450853589770999319, 0.8267830756728000718, 0.9084760833474000430, 0.9901736252444659492 ),
 ( 0.000000000000000000, 0.5000000000000000000, 1.000000000000000000 ),
 .UNSPECIFIED. ) 
 GEOMETRIC_REPRESENTATION_ITEM ( )  RATIONAL_B_SPLINE_SURFACE ( (
 ( 1.000000000000000000, 0.8025111795252390934, 0.8025111795252390934, 1.000000000000000000, 0.8025111795252390934, 0.8025111795252390934, 1.000000000000000000),
 ( 1.000000000000000000, 0.8025111795252390934, 0.8025111795252390934, 1.000000000000000000, 0.8025111795252390934, 0.8025111795252390934, 1.000000000000000000),
 ( 1.000000000000000000, 0.8025111795252390934, 0.8025111795252390934, 1.000000000000000000, 0.8025111795252390934, 0.8025111795252390934, 1.000000000000000000),
 ( 1.000000000000000000, 0.8025111795252390934, 0.8025111795252390934, 1.000000000000000000, 0.8025111795252390934, 0.8025111795252390934, 1.000000000000000000),
 ( 1.000000000000000000, 0.8025111795252390934, 0.8025111795252390934, 1.000000000000000000, 0.8025111795252390934, 0.8025111795252390934, 1.000000000000000000),
 ( 1.000000000000000000, 0.8025111795252390934, 0.8025111795252390934, 1.000000000000000000, 0.8025111795252390934, 0.8025111795252390934, 1.000000000000000000),
 ( 1.000000000000000000, 0.8025111795252390934, 0.8025111795252390934, 1.000000000000000000, 0.8025111795252390934, 0.8025111795252390934, 1.000000000000000000),
 ( 1.000000000000000000, 0.8025111795252390934, 0.8025111795252390934, 1.000000000000000000, 0.8025111795252390934, 0.8025111795252390934, 1.000000000000000000),
 ( 1.000000000000000000, 0.8025111795252390934, 0.8025111795252390934, 1.000000000000000000, 0.8025111795252390934, 0.8025111795252390934, 1.000000000000000000),
 ( 1.000000000000000000, 0.8025111795252390934, 0.8025111795252390934, 1.000000000000000000, 0.8025111795252390934, 0.8025111795252390934, 1.000000000000000000),
 ( 1.000000000000000000, 0.8025111795252390934, 0.8025111795252390934, 1.000000000000000000, 0.8025111795252390934, 0.8025111795252390934, 1.000000000000000000),
 ( 1.000000000000000000, 0.8025111795252390934, 0.8025111795252390934, 1.000000000000000000, 0.8025111795252390934, 0.8025111795252390934, 1.000000000000000000),
 ( 1.000000000000000000, 0.8025111795252390934, 0.8025111795252390934, 1.000000000000000000, 0.8025111795252390934, 0.8025111795252390934, 1.000000000000000000),
 ( 1.000000000000000000, 0.8025111795252390934, 0.8025111795252390934, 1.000000000000000000, 0.8025111795252390934, 0.8025111795252390934, 1.000000000000000000),
 ( 1.000000000000000000, 0.8025111795252390934, 0.8025111795252390934, 1.000000000000000000, 0.8025111795252390934, 0.8025111795252390934, 1.000000000000000000) ) ) 
 REPRESENTATION_ITEM ( '' )  SURFACE ( )  );
#18062 = CARTESIAN_POINT ( 'NONE',  ( -12.54238271613678890, -55.27146427614203361, -1.749799002657778102 ) ) ;
#18063 = DIRECTION ( 'NONE',  ( 0.000000000000000000, 1.000000000000000000, 0.000000000000000000 ) ) ;
#18064 = CARTESIAN_POINT ( 'NONE',  ( 11.68767212001977995, -77.07083333333332575, 3.140974612311385972 ) ) ;
#18065 = VERTEX_POINT ( 'NONE', #12848 ) ;
#18066 = EDGE_LOOP ( 'NONE', ( #13472, #56367, #49136 ) ) ;
#18067 = PRESENTATION_LAYER_ASSIGNMENT (  '', '', ( #22777 ) ) ;
#18068 = DIRECTION ( 'NONE',  ( -0.7071067811814920612, -1.249159359038985910E-07, 0.7071067811915919821 ) ) ;
#18069 = VERTEX_POINT ( 'NONE', #47743 ) ;
#18070 = CARTESIAN_POINT ( 'NONE',  ( -3.363908607861598288, -79.65371335578565493, 8.914120539577261582 ) ) ;
#18071 = ORIENTED_EDGE ( 'NONE', *, *, #7408, .T. ) ;
#18072 = CARTESIAN_POINT ( 'NONE',  ( 7.981656248348999227, -24.71865039503999739, 10.08154475890999890 ) ) ;
#18073 = CARTESIAN_POINT ( 'NONE',  ( -2.149738495732000043, -77.75052962514999422, -10.82036777477999934 ) ) ;
#18074 = CARTESIAN_POINT ( 'NONE',  ( 9.250000000000001776, -79.73958333333332860, -1.210822168571047186 ) ) ;
#18075 = CARTESIAN_POINT ( 'NONE',  ( 6.458817137649000450, -79.31613998579798874, -6.573457973844999636 ) ) ;
#18076 = CYLINDRICAL_SURFACE ( 'NONE', #18137, 5.100000000000000533 ) ;
#18077 = CARTESIAN_POINT ( 'NONE',  ( 8.822637088635000069, -80.06907204401800016, 6.926713255916000733 ) ) ;
#18078 = CARTESIAN_POINT ( 'NONE',  ( 11.00000000000000000, -81.00000000000000000, -2.369510767747999942E-13 ) ) ;
#18079 = VERTEX_POINT ( 'NONE', #39143 ) ;
#18080 = VERTEX_POINT ( 'NONE', #34700 ) ;
#18081 = CARTESIAN_POINT ( 'NONE',  ( -1.703864646944121430, -77.48977711739701135, 9.091877587378041525 ) ) ;
#18082 = AXIS2_PLACEMENT_3D ( 'NONE', #35625, #4050, #58077 ) ;
#18083 = CARTESIAN_POINT ( 'NONE',  ( 10.07768261906999996, -78.14667722612898615, -4.508174471003999706 ) ) ;
#18084 = CARTESIAN_POINT ( 'NONE',  ( 8.300970689365454902, -77.60833333333330586, -4.784380313523529438 ) ) ;
#18085 = EDGE_CURVE ( 'NONE', #25178, #51185, #39438, .T. ) ;
#18086 = CIRCLE ( 'NONE', #41644, 0.5000000000000000000 ) ;
#18087 = CARTESIAN_POINT ( 'NONE',  ( -8.073459667400001649, -78.43725928983597839, -5.384232384047000330 ) ) ;
#18088 = CARTESIAN_POINT ( 'NONE',  ( -2.230724462936999775, -75.89422385439000607, 12.93113956155000110 ) ) ;
#18089 = CARTESIAN_POINT ( 'NONE',  ( -4.966864318370061149, -79.48090711910747075, -8.097943653986082069 ) ) ;
#18090 = CARTESIAN_POINT ( 'NONE',  ( -0.7004323366084000968, -78.35998666379998667, -1.469032877812000093 ) ) ;
#18091 = CARTESIAN_POINT ( 'NONE',  ( 7.710118476707999768, -21.74977139563000250, -10.18499221085999906 ) ) ;
#18092 = CARTESIAN_POINT ( 'NONE',  ( -10.93134324956000114, -78.43238734777798982, -0.4399444258272000030 ) ) ;
#18093 = CARTESIAN_POINT ( 'NONE',  ( 0.1636246173744697330, -78.13541666666664298, -1.249999999999999778 ) ) ;
#18094 = CARTESIAN_POINT ( 'NONE',  ( 1.210822168571075386, -78.63541666666665719, -9.249999999999996447 ) ) ;
#18095 = CARTESIAN_POINT ( 'NONE',  ( 3.161638919850000118, -85.14393562394799631, -1.699348249670000088 ) ) ;
#18096 = ORIENTED_EDGE ( 'NONE', *, *, #28451, .F. ) ;
#18097 = CARTESIAN_POINT ( 'NONE',  ( -0.5618369672511999147, -78.81976746904300057, 12.30411280745000013 ) ) ;
#18098 = CARTESIAN_POINT ( 'NONE',  ( 11.12058147857000101, -76.40800415033000093, 2.393126261371000041 ) ) ;
#18099 = CARTESIAN_POINT ( 'NONE',  ( -5.096119853128885602, -78.01436659480762614, 9.465255242693306315 ) ) ;
#18100 = CARTESIAN_POINT ( 'NONE',  ( -7.615853692923001184, -78.56371882276300767, 9.247423260715999405 ) ) ;
#18101 = CARTESIAN_POINT ( 'NONE',  ( -10.53494359615000064, -18.77285042833999995, 7.618393753193999807 ) ) ;
#18103 = CARTESIAN_POINT ( 'NONE',  ( -10.75000000000000000, -79.10000000000000853, 0.000000000000000000 ) ) ;
#18102 = CARTESIAN_POINT ( 'NONE',  ( 0.000000000000000000, 4.040000000000000036, 0.000000000000000000 ) ) ;
#18104 = DIRECTION ( 'NONE',  ( 0.000000000000000000, 1.000000000000000000, 0.000000000000000000 ) ) ;
#18105 = CARTESIAN_POINT ( 'NONE',  ( 4.505820952106676991, -80.94097166855550540, 9.769115195850069711 ) ) ;
#18106 = CARTESIAN_POINT ( 'NONE',  ( 9.194664024258999646, -80.35622046769498183, 6.554488853579999663 ) ) ;
#18107 = B_SPLINE_CURVE_WITH_KNOTS ( 'NONE', 3,
 ( #43328, #16174, #34732, #35016, #57186, #53333, #12600, #3743, #25597, #8456, #21170, #39173, #44196, #29726, #52760, #12881, #12315, #48916 ),
 .UNSPECIFIED., .F., .F.,
 ( 4, 2, 2, 2, 2, 2, 2, 2, 4 ),
 ( 0.000000000000000000, 0.06250000000000124900, 0.1250000000000024980, 0.2500000000000053846, 0.5000000000000034417, 0.7500000000000014433, 0.8125000000000008882, 0.8750000000000003331, 1.000000000000000000 ),
 .UNSPECIFIED. ) ;
#18108 = CARTESIAN_POINT ( 'NONE',  ( 9.500000000000005329, -78.53958333333333997, -1.243547092045939939 ) ) ;
#18109 = CARTESIAN_POINT ( 'NONE',  ( -8.595972950985999006, -77.94605693914598987, -7.096749227412000316 ) ) ;
#18110 = CARTESIAN_POINT ( 'NONE',  ( -11.00000000000000000, -77.59999999999999432, 0.000000000000000000 ) ) ;
#18111 = CARTESIAN_POINT ( 'NONE',  ( 0.6391562500349999842, -80.52070440064619561, -11.12244055969000023 ) ) ;
#18112 = ORIENTED_EDGE ( 'NONE', *, *, #15370, .T. ) ;
#18113 = CARTESIAN_POINT ( 'NONE',  ( 1.200170490674999924, -54.36594297968999712, 12.43444080546999864 ) ) ;
#18114 = CARTESIAN_POINT ( 'NONE',  ( -2.065550207748000133, -60.22565079297999802, -12.82162303857000119 ) ) ;
#18115 = CARTESIAN_POINT ( 'NONE',  ( -9.998727717461511233, -23.92738947620295065, 7.709134076961340121 ) ) ;
#18116 = EDGE_CURVE ( 'NONE', #23662, #18069, #18646, .T. ) ;
#18117 = CARTESIAN_POINT ( 'NONE',  ( 10.34070037867000202, -77.91665569944899516, -4.346035695907999319 ) ) ;
#18118 = CARTESIAN_POINT ( 'NONE',  ( 0.000000000000000000, -80.70000000000000284, 0.000000000000000000 ) ) ;
#18119 = CARTESIAN_POINT ( 'NONE',  ( -3.250000000000000000, -1.500000000000000000, 0.000000000000000000 ) ) ;
#18120 = CARTESIAN_POINT ( 'NONE',  ( 10.75000000000000000, -77.20000000000000284, 1.135012739489781763 ) ) ;
#18121 = CARTESIAN_POINT ( 'NONE',  ( -0.5506765233274999449, -62.05954292211000478, 12.77514798316000011 ) ) ;
#18122 = CARTESIAN_POINT ( 'NONE',  ( 12.59651451717999926, -18.60944962361000066, 1.801708894189000043 ) ) ;
#18123 = CARTESIAN_POINT ( 'NONE',  ( 4.002578937700000949, -84.19782450217398662, 1.018756769644999949 ) ) ;
#18124 = DIRECTION ( 'NONE',  ( 1.000000000000000000, 0.000000000000000000, 0.000000000000000000 ) ) ;
#18125 = CARTESIAN_POINT ( 'NONE',  ( 0.000000000000000000, -46.09579702914000165, 0.000000000000000000 ) ) ;
#18126 = ADVANCED_FACE ( 'NONE', ( #34986 ), #48597, .T. ) ;
#18127 = CARTESIAN_POINT ( 'NONE',  ( 6.226899213932999722, -78.44886817601300777, -9.208165984944999494 ) ) ;
#18128 = CARTESIAN_POINT ( 'NONE',  ( -0.5713041596650000331, -79.30664044673999058, -1.442599867604999808 ) ) ;
#18129 = CARTESIAN_POINT ( 'NONE',  ( -1.386642946985999769, -78.93602415856999244, 0.3678330367775999865 ) ) ;
#18130 = CARTESIAN_POINT ( 'NONE',  ( -2.880544446985999762, -76.93082093378328068, -9.112186890989001142 ) ) ;
#18131 = CARTESIAN_POINT ( 'NONE',  ( -0.7940119350559891043, -83.16902664729457229, 1.287159878948278546 ) ) ;
#18132 = CARTESIAN_POINT ( 'NONE',  ( -12.68624828431999951, -60.56426635971000394, 1.886933512377000133 ) ) ;
#18133 = CARTESIAN_POINT ( 'NONE',  ( 10.62542268813949242, -78.08596328497016259, -1.896582608316532692 ) ) ;
#18134 = CYLINDRICAL_SURFACE ( 'NONE', #24954, 0.5000000000000004441 ) ;
#18135 = CARTESIAN_POINT ( 'NONE',  ( 4.039050189702500404, -78.50472688885261618, -10.27665506351381453 ) ) ;
#18136 = CARTESIAN_POINT ( 'NONE',  ( 1.234706307098893063, -81.83799849444270080, -0.1953252668292917160 ) ) ;
#18137 = AXIS2_PLACEMENT_3D ( 'NONE', #35771, #26910, #45828 ) ;
#18138 = CARTESIAN_POINT ( 'NONE',  ( -6.760013919724082498, -79.52708333333333712, 8.796335266379969653 ) ) ;
#18139 = CARTESIAN_POINT ( 'NONE',  ( -7.362671760698999535, -79.45872152740099637, -8.369328833011000057 ) ) ;
#18140 = CARTESIAN_POINT ( 'NONE',  ( 0.000000000000000000, -5.899999999999999467, 0.000000000000000000 ) ) ;
#18141 = ORIENTED_EDGE ( 'NONE', *, *, #42688, .F. ) ;
#18142 = ORIENTED_EDGE ( 'NONE', *, *, #49214, .F. ) ;
#18143 = CARTESIAN_POINT ( 'NONE',  ( 0.1828674678246000052, -81.35791073648699978, 1.604298418379999980 ) ) ;
#18144 = VERTEX_POINT ( 'NONE', #12282 ) ;
#18145 = DIRECTION ( 'NONE',  ( 0.000000000000000000, 1.000000000000000000, 0.000000000000000000 ) ) ;
#18146 = ORIENTED_EDGE ( 'NONE', *, *, #47949, .T. ) ;
#18147 = CARTESIAN_POINT ( 'NONE',  ( 1.153231315078470320, -80.38161910157300838, 0.4820617830468132414 ) ) ;
#18148 = VECTOR ( 'NONE', #35081, 1000.000000000000114 ) ;
#18149 = FACE_OUTER_BOUND ( 'NONE', #52853, .T. ) ;
#18150 = PRODUCT_RELATED_PRODUCT_CATEGORY ( 'part', '', ( #56856 ) ) ;
#18151 = DIRECTION ( 'NONE',  ( 0.000000000000000000, 0.000000000000000000, 1.000000000000000000 ) ) ;
#18152 = CARTESIAN_POINT ( 'NONE',  ( 0.7554284705563453217, -78.33333333333334281, 1.310679582531389276 ) ) ;
#18153 = CIRCLE ( 'NONE', #10663, 13.86363636363999952 ) ;
#18154 = CARTESIAN_POINT ( 'NONE',  ( -11.68767212001979061, -76.32083333328657204, -3.140974612311365988 ) ) ;
#18155 = CARTESIAN_POINT ( 'NONE',  ( -0.3927644566776000157, -80.85470891495099011, -3.735921117030000183 ) ) ;
#18156 = CARTESIAN_POINT ( 'NONE',  ( -9.470942015330143349, -79.39363629237638520, 0.7411628763851737522 ) ) ;
#18157 = DIRECTION ( 'NONE',  ( -0.6562721000481037681, -0.7545243075597046767, -7.882643894065047749E-10 ) ) ;
#18158 = CARTESIAN_POINT ( 'NONE',  ( -11.67960876285000005, -78.22858449693998750, 2.349052183356000079 ) ) ;
#18159 = VERTEX_POINT ( 'NONE', #52731 ) ;
#18160 = ORIENTED_EDGE ( 'NONE', *, *, #48091, .T. ) ;
#18161 = DIRECTION ( 'NONE',  ( 0.000000000000000000, 0.000000000000000000, -1.000000000000000000 ) ) ;
#18162 = CARTESIAN_POINT ( 'NONE',  ( -1.250000000000000000, -81.99999999999998579, 0.000000000000000000 ) ) ;
#18163 = ADVANCED_FACE ( 'NONE', ( #26143 ), #35459, .T. ) ;
#18164 = CARTESIAN_POINT ( 'NONE',  ( 0.2020314717676000016, -80.40276277685400430, -1.318241039644999946 ) ) ;
#18165 = CARTESIAN_POINT ( 'NONE',  ( -6.766389538252999714, -77.77314541763098532, -6.956053621355001049 ) ) ;
#18166 = CARTESIAN_POINT ( 'NONE',  ( 2.594087562880047493, -86.36264283715696877, -3.643225128093495968 ) ) ;
#18167 = CARTESIAN_POINT ( 'NONE',  ( 10.97835188747000146, -76.13641167266798959, -2.133021021907000048 ) ) ;
#18168 = CARTESIAN_POINT ( 'NONE',  ( 11.83733200052000178, -78.20185341714999083, 5.266624269285999915 ) ) ;
#18169 = EDGE_CURVE ( 'NONE', #47434, #58355, #20849, .T. ) ;
#18170 = CARTESIAN_POINT ( 'NONE',  ( -1.172849536488999922, -80.03866583923000633, 0.6711148834816000885 ) ) ;
#18171 = CARTESIAN_POINT ( 'NONE',  ( 10.72509179124999967, -76.76295827915599546, -1.855488532230999965 ) ) ;
#18172 = CARTESIAN_POINT ( 'NONE',  ( -0.9367133515736633109, -79.15782022828253162, -0.8274681181213610071 ) ) ;
#18173 = DIRECTION ( 'NONE',  ( 1.776356839400000238E-14, 1.000000000000000000, -2.368475785867000094E-14 ) ) ;
#18174 = CARTESIAN_POINT ( 'NONE',  ( -3.523754135837000145, -80.25731627376899269, 2.154453638336999877 ) ) ;
#18175 = CARTESIAN_POINT ( 'NONE',  ( -5.059370734576000395, -80.92182981354159210, -10.06538451635999998 ) ) ;
#18176 = CARTESIAN_POINT ( 'NONE',  ( -10.21380041493999968, -59.57152778012000027, 7.668936932637000048 ) ) ;
#18177 = DIRECTION ( 'NONE',  ( 0.07798810159654839813, 0.04890177473143900166, -0.9957542229071799644 ) ) ;
#18178 = CARTESIAN_POINT ( 'NONE',  ( 0.4740844096781999806, -79.12582046129089974, -3.515651949852999891 ) ) ;
#18179 = CARTESIAN_POINT ( 'NONE',  ( 0.8912423865758999364, -78.08241854487779676, 0.9921004264782997684 ) ) ;
#18180 = LINE ( 'NONE', #50062, #34533 ) ;
#18181 = CARTESIAN_POINT ( 'NONE',  ( 8.828526701892000617, -80.53055989549440596, -6.997593314318000246 ) ) ;
#18182 = CARTESIAN_POINT ( 'NONE',  ( -1.568660613942000071, -1.908528923320000237, -3.467930652269000102 ) ) ;
#18183 = CARTESIAN_POINT ( 'NONE',  ( 0.4457333967380877615, -80.59656868229342308, 1.193944125407572443 ) ) ;
#18184 = VERTEX_POINT ( 'NONE', #16141 ) ;
#18185 = DIRECTION ( 'NONE',  ( 1.000000000000000000, 0.000000000000000000, 0.000000000000000000 ) ) ;
#18186 = AXIS2_PLACEMENT_3D ( 'NONE', #30982, #41038, #13874 ) ;
#18187 = CARTESIAN_POINT ( 'NONE',  ( 8.796335266379992746, -79.39791666666667425, -6.760013919724047859 ) ) ;
#18188 = CARTESIAN_POINT ( 'NONE',  ( -0.4870599102559999838, -82.35928110403600044, -1.180149847382000017 ) ) ;
#18189 = EDGE_CURVE ( 'NONE', #7374, #44340, #6535, .T. ) ;
#18190 = CARTESIAN_POINT ( 'NONE',  ( -9.709808591512000930, -79.82183361358998752, 0.8997258012745000810 ) ) ;
#18191 = CARTESIAN_POINT ( 'NONE',  ( -1.264141272797000060, -77.63459063407999849, -12.95149364859999963 ) ) ;
#18192 = VECTOR ( 'NONE', #29634, 1000.000000000000000 ) ;
#18193 = CARTESIAN_POINT ( 'NONE',  ( 4.052275399702000236, -79.23156001420198891, -8.386988472880998913 ) ) ;
#18194 = CARTESIAN_POINT ( 'NONE',  ( 12.71658889741999943, -23.31584477285000290, -1.931087888049999979 ) ) ;
#18195 = EDGE_LOOP ( 'NONE', ( #26326, #53347, #39479, #38009 ) ) ;
#18196 = CIRCLE ( 'NONE', #43601, 3.799999999999999822 ) ;
#18197 = CARTESIAN_POINT ( 'NONE',  ( -8.385799987675619960, -24.88809827228847738, -9.298537617332518934 ) ) ;
#18198 = CYLINDRICAL_SURFACE ( 'NONE', #55953, 1.750000000000001332 ) ;
#18199 = ADVANCED_FACE ( 'NONE', ( #57445 ), #30848, .F. ) ;
#18200 = CARTESIAN_POINT ( 'NONE',  ( 0.6819515120865000668, -80.96253462192299821, -1.232362876918000172 ) ) ;
#18201 = CARTESIAN_POINT ( 'NONE',  ( 0.000000000000000000, -55.54999999966999980, -12.00000000000000000 ) ) ;
#18202 = CARTESIAN_POINT ( 'NONE',  ( 6.123453098898000491, -78.27635213868897779, 7.292029784470999587 ) ) ;
#18203 = EDGE_CURVE ( 'NONE', #54024, #43980, #7565, .T. ) ;
#18205 = CARTESIAN_POINT ( 'NONE',  ( -0.7824435345810000220, -1.638598507945999927, 3.939770163431000061 ) ) ;
#18204 = CARTESIAN_POINT ( 'NONE',  ( -3.415814973257000453, -85.99726526706999152, 2.400282231302999669 ) ) ;
#18206 = CARTESIAN_POINT ( 'NONE',  ( 0.000000000000000000, -78.79999999980499581, 0.000000000000000000 ) ) ;
#18207 = DIRECTION ( 'NONE',  ( 1.000000000000000000, 0.000000000000000000, 0.000000000000000000 ) ) ;
#18208 = EDGE_LOOP ( 'NONE', ( #42309, #45306, #36782, #11619 ) ) ;
#18209 = CARTESIAN_POINT ( 'NONE',  ( -2.392725975098465074, -77.20730248118280770, -10.48021964594175692 ) ) ;
#18210 = CARTESIAN_POINT ( 'NONE',  ( 3.600000000000000089, -0.6500000000000000222, 0.000000000000000000 ) ) ;
#18211 = DIRECTION ( 'NONE',  ( -1.000000000000000000, 0.000000000000000000, 0.000000000000000000 ) ) ;
#18212 = VERTEX_POINT ( 'NONE', #21713 ) ;
#18213 = ORIENTED_EDGE ( 'NONE', *, *, #39432, .F. ) ;
#18214 = CARTESIAN_POINT ( 'NONE',  ( -0.4635254915624000271, -77.75000000000000000, 1.426584774443000025 ) ) ;
#18215 = CARTESIAN_POINT ( 'NONE',  ( 0.000000000000000000, -91.29999999999999716, 0.000000000000000000 ) ) ;
#18216 = DIRECTION ( 'NONE',  ( 0.000000000000000000, 1.000000000000000000, 0.000000000000000000 ) ) ;
#18217 = VERTEX_POINT ( 'NONE', #39719 ) ;
#18218 = CARTESIAN_POINT ( 'NONE',  ( 9.201871282504999527, -77.99698675917198898, 7.779546039068999441 ) ) ;
#18219 = AXIS2_PLACEMENT_3D ( 'NONE', #18323, #36315, #12428 ) ;
#18220 = ORIENTED_EDGE ( 'NONE', *, *, #11136, .T. ) ;
#18221 = VERTEX_POINT ( 'NONE', #26422 ) ;
#18222 = CARTESIAN_POINT ( 'NONE',  ( -2.277289417900965951, -2.664078063540779251, -2.318001052940313222 ) ) ;
#18223 = EDGE_CURVE ( 'NONE', #1524, #21041, #54335, .T. ) ;
#18224 = AXIS2_PLACEMENT_3D ( 'NONE', #41169, #37025, #23450 ) ;
#18225 = CARTESIAN_POINT ( 'NONE',  ( -1.500000000000000000, -83.31666666666666288, 0.000000000000000000 ) ) ;
#18226 = CARTESIAN_POINT ( 'NONE',  ( -10.42531125070999920, -60.06485145371000556, 7.624341767111000756 ) ) ;
#18227 = B_SPLINE_SURFACE_WITH_KNOTS ( 'NONE', 3, 3, ( 
 ( #42745, #28562, #33857, #2307, #1441, #20304, #28849, #56322, #46609, #7010, #37425, #1730, #19723, #37720, #55741, #15286, #46901, #44186, #12023, #11739, #12868, #2875, #30871, #26442, #39740, #3169, #48906, #52183, #35293, #43319, #25301, #30295, #16453, #17307, #12588 ),
 ( #21159, #20873, #53323, #30587, #8447, #29716, #7299, #7873, #16165, #39459, #39165, #12305, #38876, #44464, #52464, #57175, #57750, #53041, #56896, #4015, #8165, #3732, #3446, #25875, #57463, #48334, #48618, #43902, #34435, #16741, #21733, #22021, #40029, #34143, #47764 ),
 ( #34721, #30003, #35008, #17024, #48057, #7588, #25587, #43609, #52751, #21452, #26167, #54213, #9921, #45362, #8744, #45067, #26735, #27617, #53619, #40630, #32327, #18778, #36480, #53925, #13748, #45657, #9044, #45949, #225, #35893, #44766, #5200, #18204, #13457, #27903 ),
 ( #4619, #17904, #23201, #41206, #27030, #40332, #5480, #36195, #796, #31748, #36770, #54788, #14330, #50374, #54509, #31453, #9629, #22618, #23486, #49793, #35591, #22315, #58341, #13157, #58042, #9339, #49495, #27328, #40923, #4911, #22910, #17602, #31154, #14046, #32040 ),
 ( #511, #49192, #50085, #18487, #4315, #41792, #37059, #51541, #10210, #11098, #6650, #37936, #32909, #29078, #1084, #15510, #50668, #14624, #24071, #5770, #55959, #28783, #47123, #19071, #32616, #1657, #41499, #46829, #28488, #19647, #28189, #24663, #37353, #6061, #42671 ),
 ( #33203, #51251, #1364, #23777, #55663, #46539, #42088, #37649, #46242, #15212, #1955, #10802, #6355, #19360, #24372, #55077, #42384, #55369, #19948, #50953, #2239, #14914, #10505, #33505, #50559, #117, #18387, #49391, #46142, #31938, #5666, #23096, #44958, #22806, #4513 ),
 ( #32515, #50270, #54404, #22514, #698, #31644, #41401, #45257, #40817, #28093, #14229, #5098, #36378, #13942, #408, #49981, #41107, #23676, #23389, #40524, #984, #5382, #18680, #41690, #9525, #10112, #18095, #36090, #53815, #18968, #54108, #14522, #1268, #35785, #36672 ),
 ( #36960, #27511, #13351, #13649, #49687, #8939, #31350, #45552, #9233, #54688, #32228, #9818, #27802, #54973, #26927, #45848, #27218, #4805, #33691, #1552, #32807, #43154, #28975, #7128, #20138, #29548, #24556, #28679, #51147, #10399, #38124, #5961, #37541, #47017, #51440 ),
 ( #33402, #19543, #19258, #10992, #10702, #19842, #2136, #6547, #37837, #24847, #15990, #56148, #15697, #33977, #51730, #55557, #50855, #37251, #42571, #25129, #11280, #47604, #29259, #46731, #6250, #28384, #47306, #23964, #15106, #6835, #42862, #2420, #33103, #20423, #55856 ),
 ( #52014, #14811, #46432, #38417, #55263, #56436, #24265, #15409, #41983, #11569, #42281, #1849, #27074, #40377, #11857, #4666, #53966, #49542, #49238, #53664, #44810, #58087, #58384, #17647, #7417, #48173, #9088, #13794, #31794, #266, #34266, #44509, #25421, #27373, #43434 ) ),
 .UNSPECIFIED., .F., .F., .F.,
 ( 4, 1, 1, 1, 1, 1, 1, 4 ),
 ( 4, 1, 1, 1, 1, 1, 1, 1, 1, 1, 1, 1, 1, 1, 1, 1, 1, 1, 1, 1, 1, 1, 1, 1, 1, 1, 1, 1, 1, 1, 1, 1, 4 ),
 ( 0.4899999999999999911, 0.5000000000000000000, 0.5999999999999999778, 0.6999999999999999556, 0.8000000000000000444, 0.9000000000000000222, 1.000000000000000000, 1.010000000000000009 ),
 ( -0.02000006906724000055, 0.01250004316702999982, 0.04500015540130000019, 0.07750026763557001097, 0.1100003798698000052, 0.1425004921040999850, 0.1750006043384000065, 0.2075007165727000003, 0.2400008288068999907, 0.2725009410411999844, 0.3050010532755000336, 0.3375011655096999963, 0.3700012777439999900, 0.4025013899782999838, 0.4350015022125000019, 0.4675016144467999957, 0.5000017266810999894, 0.5325018389153999276, 0.5650019511495999458, 0.5975020633838999951, 0.6300021756182000443, 0.6625022878524000625, 0.6950024000867000007, 0.7275025123210000499, 0.7600026245552999882, 0.7925027367895000063, 0.8250028490237999446, 0.8575029612580999938, 0.8900030734923000120, 0.9225031857265999502, 0.9550032979608999995, 0.9875034101951999377, 1.020003522429000054 ),
 .UNSPECIFIED. ) ;
#18228 = ORIENTED_EDGE ( 'NONE', *, *, #11013, .F. ) ;
#18229 = ORIENTED_EDGE ( 'NONE', *, *, #53703, .T. ) ;
#18230 = CARTESIAN_POINT ( 'NONE',  ( 6.112347209136727244, -79.28239249943922573, -6.968733846918607533 ) ) ;
#18231 = CARTESIAN_POINT ( 'NONE',  ( -3.999289396772098382, -78.72610001270986402, 0.07539443523754654763 ) ) ;
#18232 = CARTESIAN_POINT ( 'NONE',  ( -0.9465222407332000154, -81.55663953507000485, -0.8164530897714000757 ) ) ;
#18233 = CARTESIAN_POINT ( 'NONE',  ( -7.654537165467999671, -18.71943464842000182, -10.01332852689000141 ) ) ;
#18234 = CARTESIAN_POINT ( 'NONE',  ( 11.44417895085270054, -77.07083333333331154, 3.075537641221564922 ) ) ;
#18235 = EDGE_CURVE ( 'NONE', #33163, #46715, #41187, .T. ) ;
#18236 = AXIS2_PLACEMENT_3D ( 'NONE', #24503, #52244, #38077 ) ;
#18237 = CARTESIAN_POINT ( 'NONE',  ( 7.220923959705223716, -78.62291666666662593, 9.396085398178630754 ) ) ;
#18238 = CARTESIAN_POINT ( 'NONE',  ( 6.444980599755001371, -77.82020409095497371, -10.09843005143000028 ) ) ;
#18239 = CARTESIAN_POINT ( 'NONE',  ( 7.359266617186424497, -78.79822258401679846, -5.604483073908840929 ) ) ;
#18240 = CARTESIAN_POINT ( 'NONE',  ( -12.00000000000000000, -77.79999999999999716, 0.000000000000000000 ) ) ;
#18241 = CARTESIAN_POINT ( 'NONE',  ( -2.879226727952121756, -78.49583333333333712, 10.71369944335146407 ) ) ;
#18242 = DIRECTION ( 'NONE',  ( 0.000000000000000000, 1.000000000000000000, 0.000000000000000000 ) ) ;
#18243 = CARTESIAN_POINT ( 'NONE',  ( -2.796443448903999762, -81.20728455456799111, 2.808181755991999928 ) ) ;
#18244 = CARTESIAN_POINT ( 'NONE',  ( 1.898691536689999904, -77.18026001420200544, 9.688454896930000615 ) ) ;
#18245 = CARTESIAN_POINT ( 'NONE',  ( -0.001628325640062127776, -76.28437499999964189, 12.02130491422682113 ) ) ;
#18246 = CARTESIAN_POINT ( 'NONE',  ( -0.9887300587124998597, -24.93410057768999977, 12.65963207090000076 ) ) ;
#18247 = CARTESIAN_POINT ( 'NONE',  ( -12.56594317991999965, -60.04999999381999487, -1.750000000001000089 ) ) ;
#18248 = CARTESIAN_POINT ( 'NONE',  ( -3.800400640911000050, -0.9038930985898999682, -1.100537862409999956 ) ) ;
#18249 = DIRECTION ( 'NONE',  ( 0.000000000000000000, -1.000000000000000000, 0.000000000000000000 ) ) ;
#18250 = CARTESIAN_POINT ( 'NONE',  ( 1.704789468941017461, -55.09653838334687492, -12.53199752951670121 ) ) ;
#18251 = CARTESIAN_POINT ( 'NONE',  ( 10.18589226629999978, -55.51082276539999327, 7.641012305205999056 ) ) ;
#18252 = CARTESIAN_POINT ( 'NONE',  ( 1.546185472753518253, -80.59627361124843503, -0.05127335055895310828 ) ) ;
#18253 = CARTESIAN_POINT ( 'NONE',  ( 12.77306367233000017, -61.85881314422999822, -1.040970605966999862 ) ) ;
#18254 = CARTESIAN_POINT ( 'NONE',  ( -7.714303428875997959, -15.69705297113999443, -12.53545825868000385 ) ) ;
#18255 = CARTESIAN_POINT ( 'NONE',  ( -6.700596268546000545, -78.59900158500599332, -8.618433365121999756 ) ) ;
#18256 = LINE ( 'NONE', #40978, #25163 ) ;
#18257 = CARTESIAN_POINT ( 'NONE',  ( 3.250000000000000000, -2.250000000000000000, 0.000000000000000000 ) ) ;
#18259 = CARTESIAN_POINT ( 'NONE',  ( -0.6983046762106999150, -78.21329692140810153, 1.233867887851000100 ) ) ;
#18258 = DIRECTION ( 'NONE',  ( 0.000000000000000000, 0.000000000000000000, -1.000000000000000000 ) ) ;
#18260 = DIRECTION ( 'NONE',  ( 0.000000000000000000, -1.000000000000000000, 0.000000000000000000 ) ) ;
#18261 = ORIENTED_EDGE ( 'NONE', *, *, #30633, .T. ) ;
#18262 = CARTESIAN_POINT ( 'NONE',  ( -1.556119267444000087, -85.98999735065198990, 3.184903978129999924 ) ) ;
#18263 = AXIS2_PLACEMENT_3D ( 'NONE', #53468, #18048, #36040 ) ;
#18264 = CARTESIAN_POINT ( 'NONE',  ( -3.040271599595000040, -80.53806783066440289, 10.75083736931999923 ) ) ;
#18265 = B_SPLINE_CURVE_WITH_KNOTS ( 'NONE', 3,
 ( #3048, #52920, #30174, #24896, #34891, #42914, #34027, #30467, #47938, #2756, #17184, #57344, #44063, #11903, #25179, #48498, #8040, #16337, #25467, #20475, #2472, #38470, #21328, #48224, #56486, #26038, #39338, #43202, #16908, #34316, #21615, #43487, #16043, #57629, #53204, #35171, #21043 ),
 .UNSPECIFIED., .F., .F.,
 ( 4, 2, 1, 2, 2, 1, 2, 2, 2, 2, 2, 1, 1, 1, 2, 2, 1, 1, 1, 1, 2, 2, 4 ),
 ( 0.000000000000000000, 0.1250000000000002498, 0.1875000000000003886, 0.2187500000000004441, 0.2500000000000004996, 0.3125000000000004996, 0.3437500000000005551, 0.3750000000000006106, 0.5000000000000008882, 0.5625000000000008882, 0.6250000000000009992, 0.6875000000000011102, 0.7187500000000013323, 0.7343750000000013323, 0.7421875000000013323, 0.7500000000000013323, 0.8125000000000003331, 0.8437499999999997780, 0.8593749999999994449, 0.8671874999999994449, 0.8710937499999994449, 0.8749999999999994449, 1.000000000000000000 ),
 .UNSPECIFIED. ) ;
#18266 = CARTESIAN_POINT ( 'NONE',  ( -1.980464439859999981, -58.55472017426999543, -12.85144117154000121 ) ) ;
#18267 = CARTESIAN_POINT ( 'NONE',  ( -3.201827619569314720, -84.78958334313092848, -1.266442718568655534 ) ) ;
#18268 = CARTESIAN_POINT ( 'NONE',  ( 0.2654799511899000319, -78.52856650430499030, -11.21373274707999990 ) ) ;
#18269 = PLANE ( 'NONE',  #32320 ) ;
#18270 = CARTESIAN_POINT ( 'NONE',  ( -2.581517684854000017, -78.43283894841299286, -9.391243908516001326 ) ) ;
#18271 = CARTESIAN_POINT ( 'NONE',  ( 7.199854605362999926, -77.42884144764001064, -10.39073109867000078 ) ) ;
#18272 = CARTESIAN_POINT ( 'NONE',  ( 10.23553682900219997, -79.80000000000001137, -5.902732043069990553 ) ) ;
#18273 = CARTESIAN_POINT ( 'NONE',  ( 12.44180635029999848, -24.09260544925000147, -1.459447571597000115 ) ) ;
#18274 = CARTESIAN_POINT ( 'NONE',  ( -7.764005369683503410, -54.67720632257901769, -9.931049914567516623 ) ) ;
#18275 = ORIENTED_EDGE ( 'NONE', *, *, #36617, .T. ) ;
#18276 = AXIS2_PLACEMENT_3D ( 'NONE', #39390, #26373, #18925 ) ;
#18277 = CARTESIAN_POINT ( 'NONE',  ( -1.501534314747794197, -54.24847048308625830, -12.70455943736288162 ) ) ;
#18278 = FACE_OUTER_BOUND ( 'NONE', #56693, .T. ) ;
#18279 = DIRECTION ( 'NONE',  ( 0.000000000000000000, 0.000000000000000000, 1.000000000000000000 ) ) ;
#18280 = DIRECTION ( 'NONE',  ( 1.000000000000000000, 0.000000000000000000, 0.000000000000000000 ) ) ;
#18281 = CARTESIAN_POINT ( 'NONE',  ( -12.87024489158000051, -56.01538333533000014, -2.062597265787999845 ) ) ;
#18282 = DIRECTION ( 'NONE',  ( 0.7592504785508672471, -0.04890181650111791178, -0.6489586451871721673 ) ) ;
#18283 = ORIENTED_EDGE ( 'NONE', *, *, #54132, .T. ) ;
#18284 = CARTESIAN_POINT ( 'NONE',  ( -10.89239325544999915, -77.47401871959498010, 2.657546225328000222 ) ) ;
#18285 = CARTESIAN_POINT ( 'NONE',  ( 10.27340958486082911, -60.86161210392387488, -7.712164009451872637 ) ) ;
#18286 = ORIENTED_EDGE ( 'NONE', *, *, #55680, .F. ) ;
#18287 = ORIENTED_EDGE ( 'NONE', *, *, #15507, .T. ) ;
#18288 = EDGE_CURVE ( 'NONE', #49604, #35471, #49772, .T. ) ;
#18289 = CARTESIAN_POINT ( 'NONE',  ( -7.618394506877000261, -55.57286435768999411, -10.53494428257999971 ) ) ;
#18290 = CARTESIAN_POINT ( 'NONE',  ( -9.699833017908000343, -79.32079083895699512, 1.146274062705999963 ) ) ;
#18291 = ORIENTED_EDGE ( 'NONE', *, *, #7675, .T. ) ;
#18292 = CARTESIAN_POINT ( 'NONE',  ( -11.45618833121000080, -76.72164013402299076, -4.619913290770000458 ) ) ;
#18293 = DIRECTION ( 'NONE',  ( 0.000000000000000000, -1.000000000000000000, 0.000000000000000000 ) ) ;
#18294 = CARTESIAN_POINT ( 'NONE',  ( 0.0005663502821746999169, -77.83168747231999873, -1.534844259237000186 ) ) ;
#18295 = CARTESIAN_POINT ( 'NONE',  ( 8.503129636637000388, -77.84335194988499040, -4.225430575863000193 ) ) ;
#18296 = CARTESIAN_POINT ( 'NONE',  ( 8.485281374238999419, 0.000000000000000000, -8.485281374238999419 ) ) ;
#18297 = CARTESIAN_POINT ( 'NONE',  ( 0.7037555052193149585, -77.85416666683801168, -1.219334037115995306 ) ) ;
#18298 = CARTESIAN_POINT ( 'NONE',  ( 1.570796326794909881, -78.93541666666665435, -11.99999999999999822 ) ) ;
#18299 = EDGE_CURVE ( 'NONE', #47367, #27909, #57266, .T. ) ;
#18300 = CIRCLE ( 'NONE', #13608, 9.700000000000001066 ) ;
#18301 = CARTESIAN_POINT ( 'NONE',  ( -2.183112477083999803, -77.64305730667976491, 9.455407409464999802 ) ) ;
#18302 = CARTESIAN_POINT ( 'NONE',  ( 8.240049981720177996, -79.88800312984227503, 4.202220852354948910 ) ) ;
#18303 = CARTESIAN_POINT ( 'NONE',  ( 4.035839202124311242, -79.47083332087994734, 0.3584785459293593490 ) ) ;
#18304 = ORIENTED_EDGE ( 'NONE', *, *, #31348, .T. ) ;
#18305 = CARTESIAN_POINT ( 'NONE',  ( 9.670530767802999250, -76.99862249932546376, -0.1674091926992999912 ) ) ;
#18306 = CARTESIAN_POINT ( 'NONE',  ( -1.829463144348593806, -77.20923816470673273, -9.073295249180375777 ) ) ;
#18307 = CARTESIAN_POINT ( 'NONE',  ( 1.512024872110000029, -79.59676037349100852, -0.1127957995495999927 ) ) ;
#18308 = VECTOR ( 'NONE', #7827, 1000.000000000000114 ) ;
#18309 = CARTESIAN_POINT ( 'NONE',  ( 1.232226824161556822, -61.32290911199036998, -12.50408896753027399 ) ) ;
#18310 = CARTESIAN_POINT ( 'NONE',  ( -2.469193059067599449, -3.286120914691780470, 2.507410431938543294 ) ) ;
#18311 = CARTESIAN_POINT ( 'NONE',  ( 7.633089125635001082, -60.19007426270999872, -10.18115018433999985 ) ) ;
#18313 = EDGE_CURVE ( 'NONE', #3531, #9865, #31803, .T. ) ;
#18312 = CARTESIAN_POINT ( 'NONE',  ( -1.307210027570999911, -79.13383490254000208, -12.19386267984000050 ) ) ;
#18314 = CARTESIAN_POINT ( 'NONE',  ( 8.174587033571999228, -77.38791030902299894, -8.440297792765999674 ) ) ;
#18315 = CARTESIAN_POINT ( 'NONE',  ( -10.75000000005474732, -80.44999999999997442, -1.125737367057300542 ) ) ;
#18316 = CARTESIAN_POINT ( 'NONE',  ( -9.045487252274998724, -77.34916498579799793, 3.604392171359999786 ) ) ;
#18317 = CARTESIAN_POINT ( 'NONE',  ( 11.85843863511279750, -77.28708609005155949, -1.943283807933854135 ) ) ;
#18318 = CARTESIAN_POINT ( 'NONE',  ( -10.39759693597000023, -79.78060327480652347, -4.208097972746998927 ) ) ;
#18319 = ADVANCED_FACE ( 'NONE', ( #22887, #4890 ), #54766, .T. ) ;
#18320 = ORIENTED_EDGE ( 'NONE', *, *, #497, .F. ) ;
#18321 = CARTESIAN_POINT ( 'NONE',  ( -1.477496145247999992, -82.86377592892299049, 0.5756751103899000466 ) ) ;
#18322 = FACE_OUTER_BOUND ( 'NONE', #22702, .T. ) ;
#18323 = CARTESIAN_POINT ( 'NONE',  ( 7.000000000000000000, -81.99999999999998579, 0.000000000000000000 ) ) ;
#18324 = CARTESIAN_POINT ( 'NONE',  ( -5.687706977064000746, -77.91268472315900340, 10.54353137130999940 ) ) ;
#18325 = CARTESIAN_POINT ( 'NONE',  ( 9.290488860786039638, -77.00000000000002842, -1.721794440864784059 ) ) ;
#18326 = CARTESIAN_POINT ( 'NONE',  ( -0.7898276719169999849, -78.69632035071100518, -11.90847071177000061 ) ) ;
#18327 = CARTESIAN_POINT ( 'NONE',  ( 9.722066209057999231, -78.76114415034598437, 0.1588365413100999990 ) ) ;
#18328 = CARTESIAN_POINT ( 'NONE',  ( 9.189097042878000110, -78.48113340475299538, 2.883349701574000168 ) ) ;
#18329 = CARTESIAN_POINT ( 'NONE',  ( 4.536962941760771528, -76.04292347826114451, 10.83842670349287829 ) ) ;
#18330 = CARTESIAN_POINT ( 'NONE',  ( 2.277702604431000033, -78.60041292975199667, -10.79414087890000040 ) ) ;
#18331 = CARTESIAN_POINT ( 'NONE',  ( 3.229228496052769071, -85.94828564506400426, 2.345485728341623943 ) ) ;
#18332 = ORIENTED_EDGE ( 'NONE', *, *, #3399, .T. ) ;
#18333 = CARTESIAN_POINT ( 'NONE',  ( -3.151328970204000157, -76.15439989502468165, -11.89977497055999578 ) ) ;
#18334 = AXIS2_PLACEMENT_3D ( 'NONE', #46582, #555, #9965 ) ;
#18335 = CARTESIAN_POINT ( 'NONE',  ( 3.778552491321001128, -78.40681307243319509, -1.395910297075086959E-15 ) ) ;
#18336 = CARTESIAN_POINT ( 'NONE',  ( -8.631379868284000167, -78.37716771312298647, 6.779623747090999686 ) ) ;
#18337 = FACE_OUTER_BOUND ( 'NONE', #955, .T. ) ;
#18338 = EDGE_CURVE ( 'NONE', #9760, #45320, #7217, .T. ) ;
#18339 = CARTESIAN_POINT ( 'NONE',  ( -10.74112163982999846, -76.41618033130500010, -6.401740506992999791 ) ) ;
#18340 = DIRECTION ( 'NONE',  ( 0.000000000000000000, 0.000000000000000000, 1.000000000000000000 ) ) ;
#18341 = CARTESIAN_POINT ( 'NONE',  ( 6.475177433059985610, -76.82391735373433050, 8.671361647340340539 ) ) ;
#18342 = ORIENTED_EDGE ( 'NONE', *, *, #21861, .F. ) ;
#18343 = AXIS2_PLACEMENT_3D ( 'NONE', #1496, #24786, #42801 ) ;
#18344 = CARTESIAN_POINT ( 'NONE',  ( -10.99597256337999873, -79.22197590580999815, -1.828438666275999935 ) ) ;
#18345 = CARTESIAN_POINT ( 'NONE',  ( 12.70722357730233476, -54.38971352745510046, 1.610228312158712649 ) ) ;
#18346 = CARTESIAN_POINT ( 'NONE',  ( 5.412990059381605157, -75.80000000000001137, -10.58789199075580356 ) ) ;
#18347 = CARTESIAN_POINT ( 'NONE',  ( -0.03413092954076433344, -78.40681307385639798, 3.621286657814484666 ) ) ;
#18349 = CARTESIAN_POINT ( 'NONE',  ( -0.4892219813473719370, -81.50720965163131382, 1.150157418190592695 ) ) ;
#18348 = AXIS2_PLACEMENT_3D ( 'NONE', #44930, #22485, #13325 ) ;
#18350 = CARTESIAN_POINT ( 'NONE',  ( -7.035077178968999867, -79.31377255320299469, -8.660212973301998574 ) ) ;
#18351 = CARTESIAN_POINT ( 'NONE',  ( 0.000000000000000000, -76.75499999999999545, 0.000000000000000000 ) ) ;
#18352 = CARTESIAN_POINT ( 'NONE',  ( -0.6593618895071804431, -81.76024717370675887, 1.360737063013982118 ) ) ;
#18353 = CARTESIAN_POINT ( 'NONE',  ( 1.500000000000000000, -81.25000000000000000, 0.000000000000000000 ) ) ;
#18354 = CARTESIAN_POINT ( 'NONE',  ( 0.5999999999999999778, -5.200000000000000178, 4.000000000000000000 ) ) ;
#18355 = CARTESIAN_POINT ( 'NONE',  ( 1.748323643227930546, -79.56240695551150566, 10.92574688943146022 ) ) ;
#18356 = CARTESIAN_POINT ( 'NONE',  ( 0.000000000000000000, -73.00000000000001421, 0.000000000000000000 ) ) ;
#18357 = ORIENTED_EDGE ( 'NONE', *, *, #10448, .T. ) ;
#18358 = EDGE_LOOP ( 'NONE', ( #14977, #36106, #56684, #31556, #19094 ) ) ;
#18359 = DIRECTION ( 'NONE',  ( 1.000000000000000000, 0.000000000000000000, 0.000000000000000000 ) ) ;
#18360 = CARTESIAN_POINT ( 'NONE',  ( 6.043427764450761686, -79.63333333333329733, 10.48543666025110888 ) ) ;
#18361 = ORIENTED_EDGE ( 'NONE', *, *, #35746, .F. ) ;
#18362 = CARTESIAN_POINT ( 'NONE',  ( 10.02574878253000001, -76.53653125905668730, 4.955627619753999902 ) ) ;
#18363 = CARTESIAN_POINT ( 'NONE',  ( 10.13402523425000012, -23.72303809441999789, 7.647751776486000352 ) ) ;
#18364 = CARTESIAN_POINT ( 'NONE',  ( -0.5999999999999999778, -5.000000000000000000, 0.5999999999999999778 ) ) ;
#18366 = EDGE_CURVE ( 'NONE', #33741, #47577, #18180, .T. ) ;
#18365 = CARTESIAN_POINT ( 'NONE',  ( -0.5292728922702000238, -78.74998998579799547, -9.672698560386999489 ) ) ;
#18367 = CARTESIAN_POINT ( 'NONE',  ( -5.253916984369498167, -78.17694262828045737, -7.614320282445113719 ) ) ;
#18368 = CARTESIAN_POINT ( 'NONE',  ( 5.745747329289000227, -78.59830952192000098, 9.633509135241000720 ) ) ;
#18369 = CARTESIAN_POINT ( 'NONE',  ( 2.058965375186439850, -80.99999999999998579, 10.62807325966601724 ) ) ;
#18370 = ORIENTED_EDGE ( 'NONE', *, *, #57812, .T. ) ;
#18371 = DIRECTION ( 'NONE',  ( 0.000000000000000000, -1.000000000000000000, 1.147693051705999857E-13 ) ) ;
#18372 = ORIENTED_EDGE ( 'NONE', *, *, #20574, .T. ) ;
#18373 = CARTESIAN_POINT ( 'NONE',  ( -0.1831506106021379421, -77.47674350841900548, 9.248349794432215276 ) ) ;
#18374 = CARTESIAN_POINT ( 'NONE',  ( 10.07768261906999996, -78.08637430045799022, -4.508174471003999706 ) ) ;
#18375 = AXIS2_PLACEMENT_3D ( 'NONE', #51709, #51994, #48149 ) ;
#18376 = DIRECTION ( 'NONE',  ( 0.7071067811865474617, 0.000000000000000000, 0.7071067811865474617 ) ) ;
#18377 = CARTESIAN_POINT ( 'NONE',  ( -2.572125540837000290, -78.49410694809398592, -9.357076443458000270 ) ) ;
#18378 = CARTESIAN_POINT ( 'NONE',  ( -2.140299208497000283, -75.94309928261999687, -12.62824205103000175 ) ) ;
#18379 = CARTESIAN_POINT ( 'NONE',  ( -3.140773129254233798, -2.022905696757374194, -0.9277136712588065492 ) ) ;
#18380 = CARTESIAN_POINT ( 'NONE',  ( 1.328072050606999843, -78.47134980335999899, -0.9406846882429998891 ) ) ;
#18381 = CARTESIAN_POINT ( 'NONE',  ( 7.674614791514000167, -19.24899163938999891, -10.14948852566999804 ) ) ;
#18382 = CARTESIAN_POINT ( 'NONE',  ( -4.263934386054000214, -79.02232678876399063, -10.07505235160000012 ) ) ;
#18383 = AXIS2_PLACEMENT_3D ( 'NONE', #57981, #17536, #4256 ) ;
#18384 = CARTESIAN_POINT ( 'NONE',  ( -10.31444895689000063, -24.30075145017000082, -7.758883253342000685 ) ) ;
#18385 = ADVANCED_FACE ( 'NONE', ( #488, #27594 ), #31727, .T. ) ;
#18386 = CARTESIAN_POINT ( 'NONE',  ( -8.190859204290999784, -59.94999999967000548, 7.342331066867000544 ) ) ;
#18387 = CARTESIAN_POINT ( 'NONE',  ( 3.308840272069000221, -85.02754468068998506, -1.778467455431999911 ) ) ;
#18388 = ORIENTED_EDGE ( 'NONE', *, *, #46008, .F. ) ;
#18389 = CARTESIAN_POINT ( 'NONE',  ( 8.267499179258999575, -79.69052343751299361, 9.286453045038999932 ) ) ;
#18390 = CARTESIAN_POINT ( 'NONE',  ( 7.275132094855999654, -76.38840344678598626, -8.898375939052000305 ) ) ;
#18391 = CARTESIAN_POINT ( 'NONE',  ( -5.979430363902880075, -78.02211092265793013, 8.933456918256680979 ) ) ;
#18392 = CARTESIAN_POINT ( 'NONE',  ( -11.48784787867999846, -78.15677909140700308, -3.397854551190000016 ) ) ;
#18393 = CYLINDRICAL_SURFACE ( 'NONE', #25899, 1.000000000000000000 ) ;
#18395 = DIRECTION ( 'NONE',  ( 0.000000000000000000, 1.000000000000000000, 0.000000000000000000 ) ) ;
#18394 = CARTESIAN_POINT ( 'NONE',  ( 7.220923959705269013, -78.47708333333336839, -9.396085398178609438 ) ) ;
#18396 = FACE_OUTER_BOUND ( 'NONE', #23027, .T. ) ;
#18397 = CARTESIAN_POINT ( 'NONE',  ( 6.314250260588329056, -80.92529071434553600, 8.699957920916412846 ) ) ;
#18398 = CARTESIAN_POINT ( 'NONE',  ( 4.580390730373999908, -80.21517580634099431, -10.32100728648999954 ) ) ;
#18399 = CARTESIAN_POINT ( 'NONE',  ( 10.75000000000000000, -77.25000000000000000, 0.000000000000000000 ) ) ;
#18400 = CARTESIAN_POINT ( 'NONE',  ( 7.154950478465999630, -77.21067567809700449, 8.547589380727000474 ) ) ;
#18401 = CARTESIAN_POINT ( 'NONE',  ( -6.043427764450832740, -78.21666666666668277, 10.48543666025107512 ) ) ;
#18402 = CARTESIAN_POINT ( 'NONE',  ( -10.17218724451999989, -80.42734534903739529, 4.253677135873000559 ) ) ;
#18403 = VERTEX_POINT ( 'NONE', #4295 ) ;
#18404 = CARTESIAN_POINT ( 'NONE',  ( 2.460597059312418899, -77.04635416667788661, 9.159220230504379501 ) ) ;
#18405 = CARTESIAN_POINT ( 'NONE',  ( 5.896171905175000560, -77.96999999999999886, 7.127247495676000355 ) ) ;
#18406 = CARTESIAN_POINT ( 'NONE',  ( -12.50000000000000000, -92.79999999999999716, 0.000000000000000000 ) ) ;
#18407 = CARTESIAN_POINT ( 'NONE',  ( -8.729704736441000534, -77.64429226943099138, 7.043462628994999974 ) ) ;
#18408 = CARTESIAN_POINT ( 'NONE',  ( -9.611650271896834852, -79.74166666666666003, -5.539808784079895965 ) ) ;
#18409 = CARTESIAN_POINT ( 'NONE',  ( -9.252740428348994683, -77.32083333333332575, -2.486604901413163926 ) ) ;
#18410 = CARTESIAN_POINT ( 'NONE',  ( 2.678834687796258773, -82.65052081583097277, 2.987155636024215521 ) ) ;
#18411 = ADVANCED_FACE ( 'NONE', ( #3996 ), #9025, .F. ) ;
#18412 = CARTESIAN_POINT ( 'NONE',  ( -10.20000000000000107, -0.5000000000000000000, 0.000000000000000000 ) ) ;
#18413 = CARTESIAN_POINT ( 'NONE',  ( 12.44180763926000033, -17.90743932638000047, 1.459474665415000150 ) ) ;
#18414 = CARTESIAN_POINT ( 'NONE',  ( 3.632657541006000024, -85.55392953870899930, 2.051911650686999877 ) ) ;
#18415 = CARTESIAN_POINT ( 'NONE',  ( 12.50000000000000000, -39.30476017083000073, 0.000000000000000000 ) ) ;
#18416 = CARTESIAN_POINT ( 'NONE',  ( 10.07615509324000058, -54.07367739666999285, -7.986954869161998261 ) ) ;
#18417 = AXIS2_PLACEMENT_3D ( 'NONE', #47404, #58195, #13312 ) ;
#18418 = B_SPLINE_CURVE_WITH_KNOTS ( 'NONE', 3,
 ( #22945, #48935, #45099, #13192, #22349, #8477 ),
 .UNSPECIFIED., .F., .F.,
 ( 4, 2, 4 ),
 ( 0.000000000000000000, 0.5000000000000000000, 1.000000000000000000 ),
 .UNSPECIFIED. ) ;
#18419 = CARTESIAN_POINT ( 'NONE',  ( -9.244881144060999034, -76.75603931249200684, -6.227904302768000555 ) ) ;
#18420 = CARTESIAN_POINT ( 'NONE',  ( -1.542698325316999908, -81.18036382834999642, 0.6290719308543000210 ) ) ;
#18421 = CARTESIAN_POINT ( 'NONE',  ( -1.502804487684999968, -79.37384159782000381, 0.3758151099642999537 ) ) ;
#18422 = CIRCLE ( 'NONE', #5096, 0.5000000000000004441 ) ;
#18423 = CARTESIAN_POINT ( 'NONE',  ( 5.491552160713999875, -77.15710211417409425, 7.961786551375001686 ) ) ;
#18424 = CARTESIAN_POINT ( 'NONE',  ( 0.04925444800588205801, -82.62245651653309153, 1.509272080436812935 ) ) ;
#18425 = CARTESIAN_POINT ( 'NONE',  ( -12.77568181207000109, -62.06511628600999586, 0.5294980821349999367 ) ) ;
#18426 = CARTESIAN_POINT ( 'NONE',  ( 10.28103400416999946, -78.12846167599104774, 3.842432268884000024 ) ) ;
#18427 = ADVANCED_FACE ( 'NONE', ( #18468 ), #45636, .F. ) ;
#18428 = CARTESIAN_POINT ( 'NONE',  ( 10.75000000000000000, -79.84999999999999432, -2.184490103126999767E-14 ) ) ;
#18429 = CARTESIAN_POINT ( 'NONE',  ( 0.8342270367883455329, -77.96802963705810896, 0.9637654413407948928 ) ) ;
#18430 = AXIS2_PLACEMENT_3D ( 'NONE', #25920, #39209, #58390 ) ;
#18431 = CARTESIAN_POINT ( 'NONE',  ( 0.7194808217321505550, -81.77430475710248459, -1.022317606335187756 ) ) ;
#18432 = CARTESIAN_POINT ( 'NONE',  ( 0.9356112540328053173, -61.54107830070423546, 12.50329130249443743 ) ) ;
#18433 = CARTESIAN_POINT ( 'NONE',  ( -3.994755123096000560, -79.29530346938999230, 10.40656197200999955 ) ) ;
#18434 = CARTESIAN_POINT ( 'NONE',  ( 7.452378523309701741, -55.25278097498932794, 8.090910852015767318 ) ) ;
#18435 = VERTEX_POINT ( 'NONE', #4600 ) ;
#18436 = ORIENTED_EDGE ( 'NONE', *, *, #3355, .F. ) ;
#18437 = CARTESIAN_POINT ( 'NONE',  ( -3.500000000146000101, -0.7499999998540000101, 2.054632350152999929E-08 ) ) ;
#18438 = VERTEX_POINT ( 'NONE', #18756 ) ;
#18439 = DIRECTION ( 'NONE',  ( -0.7592504788686247341, -0.04890177850579158214, -0.6489586476785208502 ) ) ;
#18440 = VERTEX_POINT ( 'NONE', #17583 ) ;
#18441 = CARTESIAN_POINT ( 'NONE',  ( -1.798944584243999945, -18.78466771720000139, 12.61116915999999932 ) ) ;
#18442 = FACE_OUTER_BOUND ( 'NONE', #20470, .T. ) ;
#18443 = CARTESIAN_POINT ( 'NONE',  ( -3.407263062984217772, -80.16458332482034166, 0.5042877003416306181 ) ) ;
#18444 = ADVANCED_FACE ( 'NONE', ( #35570 ), #206, .F. ) ;
#18445 = CARTESIAN_POINT ( 'NONE',  ( 3.603299446323999788, -79.65220467013898542, -1.649916185975000227 ) ) ;
#18446 = CARTESIAN_POINT ( 'NONE',  ( 14.00000000000000000, -9.295797029142999435, -3.100994084333000442E-11 ) ) ;
#18447 = CARTESIAN_POINT ( 'NONE',  ( -11.22421241263000091, -78.71717670423001323, 3.993551959072000557 ) ) ;
#18448 = ORIENTED_EDGE ( 'NONE', *, *, #9620, .F. ) ;
#18450 = ORIENTED_EDGE ( 'NONE', *, *, #7112, .T. ) ;
#18449 = EDGE_CURVE ( 'NONE', #54390, #28730, #54505, .T. ) ;
#18451 = CARTESIAN_POINT ( 'NONE',  ( 2.899999999413999774, -80.69999999940999658, 1.301622050773000211E-09 ) ) ;
#18452 = CARTESIAN_POINT ( 'NONE',  ( -1.261445002938999860, -79.27820998021699950, -0.1968185027220000216 ) ) ;
#18453 = CARTESIAN_POINT ( 'NONE',  ( 2.867548251969000095, -77.85841690501798951, -9.270807752789000489 ) ) ;
#18454 = DIRECTION ( 'NONE',  ( 1.000000000000000000, 0.000000000000000000, 0.000000000000000000 ) ) ;
#18455 = CARTESIAN_POINT ( 'NONE',  ( 3.542904717112961954, -85.81974682883925709, 1.393669458272039696 ) ) ;
#18456 = CARTESIAN_POINT ( 'NONE',  ( 12.51393054458000087, -76.64772347022000076, -3.351762257813000190 ) ) ;
#18457 = CARTESIAN_POINT ( 'NONE',  ( -0.4789091134304000463, -81.23884839998999041, -1.232458658897999992 ) ) ;
#18458 = CONICAL_SURFACE ( 'NONE', #42014, 9.400000000000000355, 0.7853981633972997312 ) ;
#18459 = DIRECTION ( 'NONE',  ( 0.7026410690473250398, 0.1122098755728047209, -0.7026410690473250398 ) ) ;
#18460 = EDGE_CURVE ( 'NONE', #38307, #40915, #26077, .T. ) ;
#18461 = CYLINDRICAL_SURFACE ( 'NONE', #46380, 0.5999999999999999778 ) ;
#18462 = CARTESIAN_POINT ( 'NONE',  ( -4.170640425553999719, -80.24573954672798948, 0.1880654775389999922 ) ) ;
#18463 = CARTESIAN_POINT ( 'NONE',  ( 1.328862289696999932, -80.06390824290198793, 11.18676134159000135 ) ) ;
#18464 = FACE_OUTER_BOUND ( 'NONE', #31113, .T. ) ;
#18465 = CARTESIAN_POINT ( 'NONE',  ( 6.732436628721946370, -76.87268005267617355, -9.713303325498781504 ) ) ;
#18466 = CARTESIAN_POINT ( 'NONE',  ( -2.027639380875000175, -80.44857046129098421, -2.910881509572999626 ) ) ;
#18467 = DIRECTION ( 'NONE',  ( 0.000000000000000000, -1.000000000000000000, 0.000000000000000000 ) ) ;
#18468 = FACE_OUTER_BOUND ( 'NONE', #24397, .T. ) ;
#18469 = CARTESIAN_POINT ( 'NONE',  ( -2.612980907336999614, -80.50805539075979311, -10.95817168551000087 ) ) ;
#18470 = CARTESIAN_POINT ( 'NONE',  ( -0.6934022908089999548, -3.206912479849000075, 3.742362521638999961 ) ) ;
#18471 = CARTESIAN_POINT ( 'NONE',  ( 8.819914771577233026, -77.20000000000000284, -6.294782460796893631 ) ) ;
#18472 = VERTEX_POINT ( 'NONE', #46809 ) ;
#18473 = CARTESIAN_POINT ( 'NONE',  ( 0.5999999999999999778, -23.15000000000000213, 10.98362417419999915 ) ) ;
#18474 = CARTESIAN_POINT ( 'NONE',  ( 7.059844924164999647, -78.29877966580299642, -8.992308036032000018 ) ) ;
#18475 = DIRECTION ( 'NONE',  ( 1.000000000000000000, 0.000000000000000000, 0.000000000000000000 ) ) ;
#18476 = FACE_OUTER_BOUND ( 'NONE', #53125, .T. ) ;
#18477 = CARTESIAN_POINT ( 'NONE',  ( 6.466048582241999299, -79.64649766404198772, 7.299322155150999691 ) ) ;
#18478 = CARTESIAN_POINT ( 'NONE',  ( 5.512103878356000131, -76.82285899393998818, 11.78783395355999986 ) ) ;
#18479 = CARTESIAN_POINT ( 'NONE',  ( -7.704382235714319904, -79.53873634255802472, 7.497057296163620599 ) ) ;
#18480 = CARTESIAN_POINT ( 'NONE',  ( -7.624341766656999475, -60.06485146221000093, -10.42531125026000005 ) ) ;
#18481 = CARTESIAN_POINT ( 'NONE',  ( 12.92177931909999877, -20.24263462181000151, -2.062503053667999797 ) ) ;
#18482 = ORIENTED_EDGE ( 'NONE', *, *, #13845, .T. ) ;
#18483 = CARTESIAN_POINT ( 'NONE',  ( -9.833765687860001492, -77.70380051491399342, 5.287935106362000148 ) ) ;
#18484 = CARTESIAN_POINT ( 'NONE',  ( -1.268151001693999858, -80.82146036220999008, -0.3970563801964000494 ) ) ;
#18485 = CARTESIAN_POINT ( 'NONE',  ( 7.705142895586000407, -21.75083378359999742, -10.24998526315000014 ) ) ;
#18486 = CARTESIAN_POINT ( 'NONE',  ( 7.429344776774999382, -78.82343297466498200, 5.780660057059999524 ) ) ;
#18488 = CARTESIAN_POINT ( 'NONE',  ( -0.1204595238885999980, -0.6257393593719999814, 3.497926457646999943 ) ) ;
#18487 = CARTESIAN_POINT ( 'NONE',  ( 3.500498580606000054, -82.26178512955299027, 1.858143047098000045 ) ) ;
#18489 = CARTESIAN_POINT ( 'NONE',  ( 4.000000000000000000, -78.69999999999998863, 0.000000000000000000 ) ) ;
#18490 = CARTESIAN_POINT ( 'NONE',  ( 0.000000000000000000, -63.73717104351998586, 0.000000000000000000 ) ) ;
#18491 = ORIENTED_EDGE ( 'NONE', *, *, #1200, .T. ) ;
#18492 = EDGE_CURVE ( 'NONE', #9748, #16988, #14327, .T. ) ;
#18493 = CARTESIAN_POINT ( 'NONE',  ( -3.536653132374341979, -77.19840948458308105, -10.15163854538700505 ) ) ;
#18494 = CARTESIAN_POINT ( 'NONE',  ( 12.00000000000000000, -79.04999999999999716, 0.000000000000000000 ) ) ;
#18495 = CARTESIAN_POINT ( 'NONE',  ( -3.914500761937032447, -78.91452044229970397, 7.829001523874018709 ) ) ;
#18496 = ORIENTED_EDGE ( 'NONE', *, *, #16512, .F. ) ;
#18497 = ORIENTED_EDGE ( 'NONE', *, *, #17826, .F. ) ;
#18498 = DIRECTION ( 'NONE',  ( 1.000000000000000000, 0.000000000000000000, 0.000000000000000000 ) ) ;
#18499 = DIRECTION ( 'NONE',  ( -1.000000000000000000, 0.000000000000000000, 0.000000000000000000 ) ) ;
#18500 = CYLINDRICAL_SURFACE ( 'NONE', #40716, 12.00000000000000000 ) ;
#18501 = ORIENTED_EDGE ( 'NONE', *, *, #27537, .F. ) ;
#18502 = CARTESIAN_POINT ( 'NONE',  ( -1.845833107322000011, -78.07837470544299663, 11.90750485256000069 ) ) ;
#18503 = ORIENTED_EDGE ( 'NONE', *, *, #10519, .T. ) ;
#18504 = AXIS2_PLACEMENT_3D ( 'NONE', #55133, #51821, #14678 ) ;
#18505 = ORIENTED_EDGE ( 'NONE', *, *, #28091, .F. ) ;
#18506 = CARTESIAN_POINT ( 'NONE',  ( -0.2041385330985947544, -2.721221240235607741, -3.249266545227842418 ) ) ;
#18507 = AXIS2_PLACEMENT_3D ( 'NONE', #13612, #53780, #22176 ) ;
#18508 = TOROIDAL_SURFACE ( 'NONE', #32636, 17.50000000000000000, 5.000000000000000000 ) ;
#18509 = CARTESIAN_POINT ( 'NONE',  ( 11.68767212001977995, -78.57083333333332575, 3.140974612311385972 ) ) ;
#18510 = DIRECTION ( 'NONE',  ( -0.7071067811865969777, 0.7071067811864980568, 2.974164013349989944E-09 ) ) ;
#18511 = EDGE_LOOP ( 'NONE', ( #28132, #34672, #53868 ) ) ;
#18512 = CARTESIAN_POINT ( 'NONE',  ( 1.244892399546890349, -82.84341106141995681, -0.1110735506749953583 ) ) ;
#18513 = VECTOR ( 'NONE', #36459, 1000.000000000000000 ) ;
#18515 = ADVANCED_FACE ( 'NONE', ( #55940 ), #38207, .T. ) ;
#18514 = ORIENTED_EDGE ( 'NONE', *, *, #16242, .T. ) ;
#18516 = CARTESIAN_POINT ( 'NONE',  ( 0.08737939559041406345, -80.01932079608359061, 1.271311736501290035 ) ) ;
#18517 = CARTESIAN_POINT ( 'NONE',  ( 17.50000000000000000, -51.86282895648000135, 3.979093998740999976E-10 ) ) ;
#18518 = FACE_OUTER_BOUND ( 'NONE', #24251, .T. ) ;
#18519 = CARTESIAN_POINT ( 'NONE',  ( 2.076475668830000121, -76.05845572278499844, 10.98918251355999942 ) ) ;
#18520 = FACE_OUTER_BOUND ( 'NONE', #33088, .T. ) ;
#18521 = DIRECTION ( 'NONE',  ( 0.000000000000000000, -1.000000000000000000, 1.221245327088000045E-14 ) ) ;
#18522 = CARTESIAN_POINT ( 'NONE',  ( 7.612971414697999428, -55.47547470607999998, -10.53003223722000037 ) ) ;
#18523 = EDGE_CURVE ( 'NONE', #57578, #46084, #13817, .T. ) ;
#18524 = CARTESIAN_POINT ( 'NONE',  ( 0.8942477714561651858, -78.73292111987908015, -9.209421948466326668 ) ) ;
#18525 = CARTESIAN_POINT ( 'NONE',  ( 10.76566337430111275, -77.11291972185833288, -5.417667412981277408 ) ) ;
#18526 = CARTESIAN_POINT ( 'NONE',  ( -6.103045505686000460, -77.00326001420198452, 6.905034692672999519 ) ) ;
#18527 = CARTESIAN_POINT ( 'NONE',  ( -13.89248035986000041, -9.608407476587998985, -2.632528379381999666E-05 ) ) ;
#18528 = CARTESIAN_POINT ( 'NONE',  ( 0.5765222740522000233, -79.97376498383199817, 1.202579817323000233 ) ) ;
#18529 = EDGE_CURVE ( 'NONE', #12549, #54597, #55350, .T. ) ;
#18530 = CARTESIAN_POINT ( 'NONE',  ( 0.000000000000000000, -80.79999999999999716, -3.000000000000982325 ) ) ;
#18531 = CARTESIAN_POINT ( 'NONE',  ( 4.520621932142114829, -78.29753379422295723, 11.20346742569165777 ) ) ;
#18532 = CARTESIAN_POINT ( 'NONE',  ( -2.046340481354000040, -79.76042549782599167, 3.587616777720000094 ) ) ;
#18533 = CARTESIAN_POINT ( 'NONE',  ( -0.1212951196120999886, -77.81711332859900665, -9.651867515931000341 ) ) ;
#18534 = CARTESIAN_POINT ( 'NONE',  ( 0.000000000000000000, -9.638971321655001034, 0.000000000000000000 ) ) ;
#18535 = CARTESIAN_POINT ( 'NONE',  ( 1.750000000000000000, -23.24999999758999536, 12.50000000000000000 ) ) ;
#18536 = CARTESIAN_POINT ( 'NONE',  ( -0.4802748259353999960, -25.00526907281999911, 12.54896097834000024 ) ) ;
#18537 = CARTESIAN_POINT ( 'NONE',  ( 12.00000000000000000, -79.25000000000000000, 1.072514965728000067E-08 ) ) ;
#18538 = CARTESIAN_POINT ( 'NONE',  ( -1.250013176831791695, -78.10006463709670754, 4.053087819277079897E-06 ) ) ;
#18539 = CARTESIAN_POINT ( 'NONE',  ( -0.1186549498682999831, -0.7591989345079001028, 3.445524895640000196 ) ) ;
#18540 = CARTESIAN_POINT ( 'NONE',  ( 7.624341764906000130, -55.53514850498000044, 10.42531124851000079 ) ) ;
#18541 = CARTESIAN_POINT ( 'NONE',  ( 10.59548767699999949, -57.04263462147999775, 7.678667886061999681 ) ) ;
#18542 = CARTESIAN_POINT ( 'NONE',  ( -1.801750019963999971, -23.39007426722000105, -12.59656967653999970 ) ) ;
#18543 = CARTESIAN_POINT ( 'NONE',  ( -0.03896466140217625523, -78.47771600701551620, 1.249276069285430335 ) ) ;
#18544 = CARTESIAN_POINT ( 'NONE',  ( 0.000000000000000000, 0.000000000000000000, 0.000000000000000000 ) ) ;
#18545 = CARTESIAN_POINT ( 'NONE',  ( 12.99510751537000353, -26.30294702886003222, -6.911973076623003642 ) ) ;
#18546 = VECTOR ( 'NONE', #15901, 1000.000000000000000 ) ;
#18547 = CARTESIAN_POINT ( 'NONE',  ( -1.017498374054518706, -77.33295997921678122, 10.79023145527350991 ) ) ;
#18548 = DIRECTION ( 'NONE',  ( 0.000000000000000000, -1.000000000000000000, 0.000000000000000000 ) ) ;
#18549 = EDGE_CURVE ( 'NONE', #43269, #8841, #15192, .T. ) ;
#18551 = CARTESIAN_POINT ( 'NONE',  ( -1.223493401540999947, -79.25516201241099168, 0.7163828769940999708 ) ) ;
#18550 = CARTESIAN_POINT ( 'NONE',  ( 8.000000000000000000, -81.99999999999998579, 0.000000000000000000 ) ) ;
#18552 = CARTESIAN_POINT ( 'NONE',  ( -0.7427769915940999335, -81.79286360614999296, -1.400956470667000131 ) ) ;
#18553 = ORIENTED_EDGE ( 'NONE', *, *, #56709, .T. ) ;
#18554 = AXIS2_PLACEMENT_3D ( 'NONE', #35494, #53231, #57083 ) ;
#18555 = CARTESIAN_POINT ( 'NONE',  ( 0.2516332205413999712, -85.28007450217398855, -3.580561164506000260 ) ) ;
#18556 = CARTESIAN_POINT ( 'NONE',  ( -7.213067475145999552, -79.55009665242799599, 9.497763435974000856 ) ) ;
#18557 = CARTESIAN_POINT ( 'NONE',  ( 11.01264074648000069, -80.33045002223688869, 0.9768939932525001479 ) ) ;
#18558 = VECTOR ( 'NONE', #1933, 1000.000000000000000 ) ;
#18559 = CARTESIAN_POINT ( 'NONE',  ( -1.980464483675000054, -57.04439829357999514, -12.85140862645999782 ) ) ;
#18560 = CARTESIAN_POINT ( 'NONE',  ( -2.882630883240388631, -86.06145833917183552, 1.884276930884437595 ) ) ;
#18561 = CARTESIAN_POINT ( 'NONE',  ( 0.1392748842281999744, -77.20790617294500180, 11.21600254538999941 ) ) ;
#18562 = CARTESIAN_POINT ( 'NONE',  ( 12.54980553584999825, -53.75222688831999562, 0.05649961219499999993 ) ) ;
#18563 = CARTESIAN_POINT ( 'NONE',  ( -3.206516299415000049, -2.013032031398999777, -0.5298615117031000299 ) ) ;
#18564 = VECTOR ( 'NONE', #50690, 1000.000000000000000 ) ;
#18565 = CARTESIAN_POINT ( 'NONE',  ( 2.459153317701999963, -0.9829018800870999995, -3.188313159924000217 ) ) ;
#18566 = CARTESIAN_POINT ( 'NONE',  ( -9.801770080294998522, -79.26010532903798378, 1.326986863057000088 ) ) ;
#18567 = DIRECTION ( 'NONE',  ( 0.9957542217955427377, -0.04890179608120209104, 0.07798810240277338768 ) ) ;
#18568 = CARTESIAN_POINT ( 'NONE',  ( -7.954951288349001004, -18.75000000000000000, 9.722718241315000398 ) ) ;
#18569 = EDGE_LOOP ( 'NONE', ( #54518, #10570, #42613, #11749, #31922, #3162, #17618, #9205 ) ) ;
#18570 = EDGE_CURVE ( 'NONE', #25098, #21810, #28467, .T. ) ;
#18571 = CARTESIAN_POINT ( 'NONE',  ( 0.9935076048416776606, -53.83183812219430564, -12.70250268212331157 ) ) ;
#18572 = CARTESIAN_POINT ( 'NONE',  ( -1.983076742770497836, -76.97083333328025390, -9.322644974446816946 ) ) ;
#18573 = DIRECTION ( 'NONE',  ( -1.000000000000000000, 0.000000000000000000, 0.000000000000000000 ) ) ;
#18574 = EDGE_CURVE ( 'NONE', #21690, #19884, #6336, .T. ) ;
#18575 = CARTESIAN_POINT ( 'NONE',  ( 1.199500263597271577, -78.59791666666667709, -0.9218200799623702535 ) ) ;
#18576 = CARTESIAN_POINT ( 'NONE',  ( -12.58335110162999904, -58.54888345776999614, -1.667961430005999945 ) ) ;
#18577 = CARTESIAN_POINT ( 'NONE',  ( 1.250000000000000000, -80.84999999999999432, 0.000000000000000000 ) ) ;
#18578 = EDGE_LOOP ( 'NONE', ( #19904, #16181, #35095 ) ) ;
#18579 = CARTESIAN_POINT ( 'NONE',  ( 0.3796936798447000383, -77.62075755425598800, -11.20547256801999936 ) ) ;
#18580 = CARTESIAN_POINT ( 'NONE',  ( 7.610436523699107170, -60.32540704676000587, -10.41144397134746136 ) ) ;
#18581 = ORIENTED_EDGE ( 'NONE', *, *, #55117, .F. ) ;
#18582 = CARTESIAN_POINT ( 'NONE',  ( -10.19022281664999952, -55.60366258855000154, -7.646946378492000207 ) ) ;
#18583 = CARTESIAN_POINT ( 'NONE',  ( -2.217000330786000450, -79.22337286418299129, 9.512392227823999846 ) ) ;
#18584 = EDGE_LOOP ( 'NONE', ( #2329, #21109, #49585, #5494 ) ) ;
#18585 = CARTESIAN_POINT ( 'NONE',  ( -7.644092900757152087, -55.27619833568792274, 10.09634159697596800 ) ) ;
#18586 = CARTESIAN_POINT ( 'NONE',  ( -12.50000000000000000, -60.04999999657000131, -1.750000000000000000 ) ) ;
#18587 = CARTESIAN_POINT ( 'NONE',  ( -0.6427777546026000044, -79.36308811491998938, -1.517687492048999998 ) ) ;
#18588 = ORIENTED_EDGE ( 'NONE', *, *, #22033, .T. ) ;
#18589 = CARTESIAN_POINT ( 'NONE',  ( -5.597970637881999778, -77.05522694988499666, 7.669424558767000022 ) ) ;
#18590 = CIRCLE ( 'NONE', #16689, 11.65000000000000036 ) ;
#18591 = CARTESIAN_POINT ( 'NONE',  ( -8.414570695956999913, -55.64999999967000122, 8.414570695956999913 ) ) ;
#18592 = CARTESIAN_POINT ( 'NONE',  ( 0.6680158199250733064, -80.27032678700797419, -1.057154657451736091 ) ) ;
#18593 = CARTESIAN_POINT ( 'NONE',  ( -9.299140214180997788, -78.14275400357000478, -9.021566674317000434 ) ) ;
#18594 = CARTESIAN_POINT ( 'NONE',  ( -3.699999999670000150, -78.39678895077818765, 3.845529056692000202E-10 ) ) ;
#18595 = B_SPLINE_CURVE_WITH_KNOTS ( 'NONE', 3,
 ( #42492, #51938, #11205, #34761, #29183, #47231, #46940, #43647, #6759, #2912 ),
 .UNSPECIFIED., .F., .F.,
 ( 4, 2, 2, 2, 4 ),
 ( 0.000000000000000000, 0.1875000001591858589, 0.3750000003183717179, 0.5625000004775576601, 0.7500000006367434358 ),
 .UNSPECIFIED. ) ;
#18596 = CARTESIAN_POINT ( 'NONE',  ( 8.993737204470543034, -79.86887876594592228, 2.161928414312813906 ) ) ;
#18597 = AXIS2_PLACEMENT_3D ( 'NONE', #44956, #4803, #44080 ) ;
#18598 = CARTESIAN_POINT ( 'NONE',  ( -3.999588488232725059, -78.71927081250180436, -0.3228834954761045095 ) ) ;
#18599 = ORIENTED_EDGE ( 'NONE', *, *, #57675, .T. ) ;
#18600 = CARTESIAN_POINT ( 'NONE',  ( 8.211976133158094271, -76.95750447567392882, -4.859042301739362024 ) ) ;
#18601 = CARTESIAN_POINT ( 'NONE',  ( 3.007117222848000093, -75.90736186172000544, 11.93703523519999976 ) ) ;
#18602 = CARTESIAN_POINT ( 'NONE',  ( -1.419358333703000019, -79.34869725658599293, 0.07120080608633000407 ) ) ;
#18603 = CIRCLE ( 'NONE', #51613, 1.199999999999999956 ) ;
#18604 = CARTESIAN_POINT ( 'NONE',  ( 2.752649745648064084, -2.544360987267859642, -2.286872036682715770 ) ) ;
#18605 = CARTESIAN_POINT ( 'NONE',  ( 6.233047529871999615, -78.98050366622999263, 9.960502923565000444 ) ) ;
#18606 = CARTESIAN_POINT ( 'NONE',  ( -10.39285214024000048, -78.47279838679000363, 6.510605926401999533 ) ) ;
#18607 = CARTESIAN_POINT ( 'NONE',  ( -3.164411967817999827, -77.30594483241300452, -11.86639179494000018 ) ) ;
#18608 = B_SPLINE_CURVE_WITH_KNOTS ( 'NONE', 3,
 ( #41894, #50770, #5871, #1182 ),
 .UNSPECIFIED., .F., .F.,
 ( 4, 4 ),
 ( 0.000000000000000000, 1.000000000000000000 ),
 .UNSPECIFIED. ) ;
#18609 = CARTESIAN_POINT ( 'NONE',  ( -3.451879464910993622, -85.80681307243298761, 1.536875756006014671 ) ) ;
#18610 = CARTESIAN_POINT ( 'NONE',  ( 9.597740827301000976, -77.18673832859900585, -0.7705299494857000830 ) ) ;
#18611 = CARTESIAN_POINT ( 'NONE',  ( -1.336107520624923994, -77.43385316951449227, 11.99618174931092796 ) ) ;
#18612 = CARTESIAN_POINT ( 'NONE',  ( -2.511165522482547097, -76.34295674094352080, 12.78297198345306818 ) ) ;
#18613 = ORIENTED_EDGE ( 'NONE', *, *, #20105, .T. ) ;
#18614 = CARTESIAN_POINT ( 'NONE',  ( 1.308628125960000110, -82.16918203637000317, -0.6662886516973000051 ) ) ;
#18615 = CARTESIAN_POINT ( 'NONE',  ( -0.5717664302369001028, -81.11020805664000477, -1.224358761826999986 ) ) ;
#18616 = CARTESIAN_POINT ( 'NONE',  ( 0.1636246173744642929, -79.36458333333331439, 1.250000000000000888 ) ) ;
#18617 = CARTESIAN_POINT ( 'NONE',  ( 11.36821324764999908, -77.72277951519299677, -3.778861202892000115 ) ) ;
#18618 = CARTESIAN_POINT ( 'NONE',  ( 7.665367164120238996, -77.00000000000001421, 5.330550266068665444 ) ) ;
#18619 = CARTESIAN_POINT ( 'NONE',  ( 6.071186539538999227, -77.84184313900898644, 10.40848046910999791 ) ) ;
#18620 = CARTESIAN_POINT ( 'NONE',  ( 9.617254819657999221, -78.45270957562398451, -0.5114877307952000463 ) ) ;
#18621 = EDGE_CURVE ( 'NONE', #39575, #3891, #6284, .T. ) ;
#18622 = CARTESIAN_POINT ( 'NONE',  ( 0.0001230185931830488706, -76.07467095836980775, 11.74978004242729668 ) ) ;
#18623 = CARTESIAN_POINT ( 'NONE',  ( 9.849799932654001111, -79.81206640024099386, 4.707101791649999534 ) ) ;
#18624 = CARTESIAN_POINT ( 'NONE',  ( -0.5413909687624368638, -85.80681307243297340, 4.353993567106648754 ) ) ;
#18625 = EDGE_LOOP ( 'NONE', ( #26533, #39685, #14568, #49753, #14708 ) ) ;
#18626 = CARTESIAN_POINT ( 'NONE',  ( 7.678655902612541162, -18.20623020282301852, -10.03844298039529370 ) ) ;
#18627 = EDGE_CURVE ( 'NONE', #30461, #19, #47779, .T. ) ;
#18628 = CARTESIAN_POINT ( 'NONE',  ( -3.850965819624345254, -78.43735716284258785, 0.07259824540930022441 ) ) ;
#18629 = CARTESIAN_POINT ( 'NONE',  ( -5.496747179549230644, -76.28607285822243966, -10.38820195124879397 ) ) ;
#18630 = CARTESIAN_POINT ( 'NONE',  ( 9.981840466370998755, -78.77457889078598896, 4.563647388395000171 ) ) ;
#18631 = CARTESIAN_POINT ( 'NONE',  ( 0.000000000000000000, -6.049999999381999949, 0.000000000000000000 ) ) ;
#18632 = CARTESIAN_POINT ( 'NONE',  ( 12.50728313516224688, -17.00024825485536084, -0.1773837593737443152 ) ) ;
#18633 = CARTESIAN_POINT ( 'NONE',  ( -8.485281374238999419, -18.75000000000000000, 8.485281374238999419 ) ) ;
#18634 = CARTESIAN_POINT ( 'NONE',  ( 7.658894278891000162, -18.79060682915999791, -10.01676917982000070 ) ) ;
#18635 = CARTESIAN_POINT ( 'NONE',  ( 8.441163348740026606, -17.08348045813557192, 9.243160721208877106 ) ) ;
#18636 = VERTEX_POINT ( 'NONE', #42364 ) ;
#18637 = CARTESIAN_POINT ( 'NONE',  ( 8.591781367357000931, -78.51383098776300073, 7.101823234627000048 ) ) ;
#18638 = CARTESIAN_POINT ( 'NONE',  ( 0.000000000000000000, -32.70420297070000260, 0.000000000000000000 ) ) ;
#18639 = CARTESIAN_POINT ( 'NONE',  ( -7.919595949288999570, -55.64999999964999233, 9.050966799188000067 ) ) ;
#18640 = CARTESIAN_POINT ( 'NONE',  ( 3.699999999670001039, -78.39678895079168797, 2.183641461020670693 ) ) ;
#18641 = ADVANCED_FACE ( 'NONE', ( #11077 ), #50646, .T. ) ;
#18642 = CARTESIAN_POINT ( 'NONE',  ( 12.50409240828692958, -61.32129362315870225, 1.233800930082795677 ) ) ;
#18643 = VECTOR ( 'NONE', #306, 1000.000000000000000 ) ;
#18644 = CARTESIAN_POINT ( 'NONE',  ( 0.2631036358232000105, -79.43383300265197988, -11.04575348828999992 ) ) ;
#18645 = DIRECTION ( 'NONE',  ( 1.000000000000000000, 0.000000000000000000, 0.000000000000000000 ) ) ;
#18646 = CIRCLE ( 'NONE', #39363, 9.700000000000001066 ) ;
#18647 = CARTESIAN_POINT ( 'NONE',  ( -9.431004454606608078, -17.19940410572420930, -8.251853356785748161 ) ) ;
#18648 = CIRCLE ( 'NONE', #56361, 0.5000000000000004441 ) ;
#18649 = CARTESIAN_POINT ( 'NONE',  ( 0.000000000000000000, -33.10361340872000113, 0.000000000000000000 ) ) ;
#18650 = DIRECTION ( 'NONE',  ( -1.000000000000000000, 0.000000000000000000, -2.716802477432001181E-13 ) ) ;
#18651 = CARTESIAN_POINT ( 'NONE',  ( -5.755267649934913798, -78.36902568785910717, 9.345839351064629597 ) ) ;
#18652 = EDGE_CURVE ( 'NONE', #21753, #27560, #3664, .T. ) ;
#18653 = CARTESIAN_POINT ( 'NONE',  ( 0.000000000000000000, -78.59999999921299718, -2.699999999213000379 ) ) ;
#18654 = ORIENTED_EDGE ( 'NONE', *, *, #54821, .T. ) ;
#18655 = ORIENTED_EDGE ( 'NONE', *, *, #46553, .F. ) ;
#18656 = CARTESIAN_POINT ( 'NONE',  ( 7.602019699312583256, -78.78750673935347493, -7.600759696224709927 ) ) ;
#18657 = LINE ( 'NONE', #23067, #34203 ) ;
#18658 = ORIENTED_EDGE ( 'NONE', *, *, #17700, .F. ) ;
#18659 = DIRECTION ( 'NONE',  ( -1.000000000000000000, 0.000000000000000000, 0.000000000000000000 ) ) ;
#18660 = CARTESIAN_POINT ( 'NONE',  ( 7.756281347471999155, -24.22006031113999569, 10.15825374573999973 ) ) ;
#18661 = CARTESIAN_POINT ( 'NONE',  ( 9.929702205026998740, -61.43097880247000120, 7.973987073312001073 ) ) ;
#18662 = CARTESIAN_POINT ( 'NONE',  ( 9.271914673454089595, -76.74308161707607212, -7.928664495432715675 ) ) ;
#18663 = CARTESIAN_POINT ( 'NONE',  ( 10.69399390970047747, -78.26269357169036311, -5.399859776636326103 ) ) ;
#18664 = CARTESIAN_POINT ( 'NONE',  ( -5.268979267983999293, -78.68001855092498431, 9.902321347348999936 ) ) ;
#18665 = CARTESIAN_POINT ( 'NONE',  ( 10.98952246480719808, -80.99999999999997158, 0.8689862965050588750 ) ) ;
#18666 = ORIENTED_EDGE ( 'NONE', *, *, #5903, .T. ) ;
#18667 = LINE ( 'NONE', #50255, #46340 ) ;
#18668 = ORIENTED_EDGE ( 'NONE', *, *, #27751, .F. ) ;
#18669 = CARTESIAN_POINT ( 'NONE',  ( -0.5489994406321448972, -77.47989606497139903, 9.234366156267499903 ) ) ;
#18670 = CARTESIAN_POINT ( 'NONE',  ( 9.507661145905998978, -77.63772188748299641, -5.611464101879999333 ) ) ;
#18671 = CARTESIAN_POINT ( 'NONE',  ( 11.00000000000000000, -18.25000000000000000, 1.016729233725000008E-14 ) ) ;
#18672 = CARTESIAN_POINT ( 'NONE',  ( 4.746041175454999816, -77.55612058683698251, -8.464384343845999581 ) ) ;
#18673 = CARTESIAN_POINT ( 'NONE',  ( -9.502921960388910350, -17.25907999995016695, 8.179400289350656550 ) ) ;
#18674 = CARTESIAN_POINT ( 'NONE',  ( 1.500000000000000000, -78.25000000000000000, 0.000000000000000000 ) ) ;
#18675 = CARTESIAN_POINT ( 'NONE',  ( 1.169626569868999821, -78.02236249102999466, 1.131652196797999999 ) ) ;
#18676 = LINE ( 'NONE', #18962, #7323 ) ;
#18677 = CARTESIAN_POINT ( 'NONE',  ( 1.678937288468000055, -78.29192557611499126, 10.81059606312000021 ) ) ;
#18678 = CARTESIAN_POINT ( 'NONE',  ( -7.660411271047999904, -23.19173735492000077, -10.01752031414999955 ) ) ;
#18679 = CARTESIAN_POINT ( 'NONE',  ( -7.892048199460299784, -60.54946977258664731, 7.664266801481004698 ) ) ;
#18680 = CARTESIAN_POINT ( 'NONE',  ( -2.892718313690000098, -84.66293396287998974, -2.125070773710000527 ) ) ;
#18681 = ORIENTED_EDGE ( 'NONE', *, *, #3683, .T. ) ;
#18682 = CARTESIAN_POINT ( 'NONE',  ( -8.405409561606999702, -79.37590556260300900, 9.003060531051000126 ) ) ;
#18683 = CARTESIAN_POINT ( 'NONE',  ( -10.05101082620999797, -76.10235696248199133, 5.326514725976999820 ) ) ;
#18684 = CARTESIAN_POINT ( 'NONE',  ( 4.695313984048824274, -77.93919653761264499, 9.670285837986678956 ) ) ;
#18685 = CARTESIAN_POINT ( 'NONE',  ( -3.165411199172029288, -3.479166666666666963, 0.8506806241676482250 ) ) ;
#18687 = CARTESIAN_POINT ( 'NONE',  ( 10.42531124903999995, -55.53514851492000304, -7.624341765436000173 ) ) ;
#18686 = CARTESIAN_POINT ( 'NONE',  ( -10.26699006316252749, -78.34166666666666856, -5.917523019358070790 ) ) ;
#18688 = CARTESIAN_POINT ( 'NONE',  ( 0.8293971963509981782, -2.893870552623438730, -3.421159378200740342 ) ) ;
#18689 = CARTESIAN_POINT ( 'NONE',  ( 3.654181830570425671, -86.09999999999999432, -1.626946572303649807 ) ) ;
#18690 = CARTESIAN_POINT ( 'NONE',  ( 11.12972475151000040, -78.13671134015899611, -0.6195381557079999713 ) ) ;
#18691 = DIRECTION ( 'NONE',  ( 0.000000000000000000, 0.000000000000000000, -1.000000000000000000 ) ) ;
#18692 = CARTESIAN_POINT ( 'NONE',  ( -6.449172644969999979, -80.46700902863899785, -9.084347907802998279 ) ) ;
#18693 = EDGE_LOOP ( 'NONE', ( #11250, #46700, #36058, #15452 ) ) ;
#18694 = CARTESIAN_POINT ( 'NONE',  ( -9.204193785523999694, -77.16974903538300623, -2.332437886131999871 ) ) ;
#18695 = CARTESIAN_POINT ( 'NONE',  ( -3.461985009909999800, -2.184444768727999975, 1.581285081509000046 ) ) ;
#18696 = CARTESIAN_POINT ( 'NONE',  ( 9.869466656387999137, -76.90891100838200600, -5.330266269891000164 ) ) ;
#18697 = CARTESIAN_POINT ( 'NONE',  ( 6.612939829087000732, -79.63308722408299900, 8.759739992124000452 ) ) ;
#18698 = CARTESIAN_POINT ( 'NONE',  ( 7.646966600018000548, -23.19642081717000082, -10.19019745247000053 ) ) ;
#18699 = DIRECTION ( 'NONE',  ( 0.000000000000000000, 1.000000000000000000, 0.000000000000000000 ) ) ;
#18700 = CARTESIAN_POINT ( 'NONE',  ( -9.984017254981614187, -78.53079889738936004, -4.071156503779041813 ) ) ;
#18701 = CARTESIAN_POINT ( 'NONE',  ( 12.54705919859000041, -17.46307476627999833, 1.287183453418999868 ) ) ;
#18702 = CARTESIAN_POINT ( 'NONE',  ( 3.029351209061000194, -83.75017953870899134, -2.868723822119999767 ) ) ;
#18703 = DIRECTION ( 'NONE',  ( 0.000000000000000000, -1.000000000000000000, 0.000000000000000000 ) ) ;
#18704 = EDGE_CURVE ( 'NONE', #23873, #9942, #52661, .T. ) ;
#18705 = DIRECTION ( 'NONE',  ( 0.000000000000000000, 1.000000000000000000, 0.000000000000000000 ) ) ;
#18706 = B_SPLINE_SURFACE_WITH_KNOTS ( 'NONE', 3, 3, ( 
 ( #25790, #39375, #30783, #53237, #12785, #21358, #44377, #57661, #35205, #53530, #12219, #26071, #3363, #57381, #48817, #40239, #34922, #8956, #26358, #52953, #3929, #12502, #44973, #26940, #39940, #57956, #30501, #48530, #17510, #44097, #35500, #13070, #39081, #31068, #44677 ),
 ( #21075, #57088, #4230, #22228, #58254, #49997, #27816, #36105, #5396, #32824, #4822, #50574, #27526, #40539, #23405, #41415, #37265, #32531, #19274, #27234, #45568, #18111, #14825, #18692, #50869, #50284, #13663, #9543, #31658, #10129, #134, #5113, #55279, #23692, #998 ),
 ( #28107, #13956, #23112, #10415, #18984, #32241, #41120, #36685, #54701, #14245, #9835, #28401, #46157, #9249, #5682, #41705, #45863, #4529, #36976, #22529, #45273, #49702, #54122, #1281, #22821, #40831, #424, #18402, #54989, #54420, #14537, #31952, #6265, #20152, #43169 ),
 ( #46447, #6851, #56162, #20436, #23979, #38139, #47032, #52030, #2726, #24861, #42877, #20722, #2435, #28694, #1566, #11870, #15711, #34279, #47322, #56742, #51744, #55873, #19858, #37556, #38432, #33120, #24280, #33705, #11294, #29274, #46745, #56449, #24570, #42587, #16004 ) ),
 .UNSPECIFIED., .F., .F., .F.,
 ( 4, 4 ),
 ( 4, 1, 1, 1, 1, 1, 1, 1, 1, 1, 1, 1, 1, 1, 1, 1, 1, 1, 1, 1, 1, 1, 1, 1, 1, 1, 1, 1, 1, 1, 1, 1, 4 ),
 ( -0.1772706441294000235, 1.177270644128999955 ),
 ( 0.4972775948320999895, 0.5132957106829999505, 0.5293138265339000226, 0.5453319423849000147, 0.5613500582358000868, 0.5773681740867999679, 0.5933862899377000399, 0.6094044057886000010, 0.6254225216395999931, 0.6414406374904999542, 0.6574587533414000262, 0.6734768691924000183, 0.6894949850432999794, 0.7055131008942999715, 0.7215312167452000436, 0.7375493325960998936, 0.7535674484470999968, 0.7695855642979999578, 0.7856036801490000610, 0.8016217959999000220, 0.8176399118507999830, 0.8336580277017999752, 0.8496761435527000472, 0.8656942594036999283, 0.8817123752546000004, 0.8977304911055000725, 0.9137486069564999536, 0.9297667228074000256, 0.9457848386584000178, 0.9618029545093000898, 0.9778210703601999398, 0.9938391862111999320, 1.009857302061999862 ),
 .UNSPECIFIED. ) ;
#18707 = B_SPLINE_CURVE_WITH_KNOTS ( 'NONE', 3,
 ( #50552, #9810, #37531, #23382, #33393, #28967, #46134, #10986, #27795, #5658, #41392, #14804, #10693, #45839, #23667, #10104, #46422, #36953 ),
 .UNSPECIFIED., .F., .F.,
 ( 4, 2, 2, 2, 2, 2, 2, 2, 4 ),
 ( 0.000000000000000000, 0.1250000000000000000, 0.2500000000000000000, 0.3750000000000000000, 0.5000000000000000000, 0.6250000000000000000, 0.7500000000000000000, 0.8750000000000000000, 1.000000000000000000 ),
 .UNSPECIFIED. ) ;
#18708 = CARTESIAN_POINT ( 'NONE',  ( -8.272053489104999713, -78.23857205644399926, -7.648664291178000063 ) ) ;
#18709 = CARTESIAN_POINT ( 'NONE',  ( 1.587978134902999994, -80.54482878599999651, 0.5035716945827000135 ) ) ;
#18710 = CARTESIAN_POINT ( 'NONE',  ( 1.088015599395999899, -79.22206712645999005, -0.7475960909009999877 ) ) ;
#18711 = CARTESIAN_POINT ( 'NONE',  ( 5.212684961665999595, -77.00044591236508040, -8.147089634514999901 ) ) ;
#18712 = CARTESIAN_POINT ( 'NONE',  ( -1.226932303529735480, -82.19734641482862969, 0.9440816031200599534 ) ) ;
#18713 = DIRECTION ( 'NONE',  ( 0.000000000000000000, -1.000000000000000000, 0.000000000000000000 ) ) ;
#18714 = CARTESIAN_POINT ( 'NONE',  ( 2.550499813263000348, -78.49366228231559717, -10.67515654612000020 ) ) ;
#18715 = CARTESIAN_POINT ( 'NONE',  ( 1.244083471246176797, -79.84158205231473460, -0.1422760444506795119 ) ) ;
#18716 = VECTOR ( 'NONE', #28772, 1000.000000000000000 ) ;
#18717 = ORIENTED_EDGE ( 'NONE', *, *, #6908, .T. ) ;
#18718 = CARTESIAN_POINT ( 'NONE',  ( 0.5884030026776352340, -81.76430342800995277, -1.102917213597483848 ) ) ;
#18719 = DIRECTION ( 'NONE',  ( 1.000000000000000000, 0.000000000000000000, 0.000000000000000000 ) ) ;
#18720 = EDGE_CURVE ( 'NONE', #13326, #49672, #57084, .T. ) ;
#18721 = CARTESIAN_POINT ( 'NONE',  ( 8.680500415593000341, -78.62837685893698847, 7.175156920760000112 ) ) ;
#18722 = LINE ( 'NONE', #54153, #14869 ) ;
#18723 = ORIENTED_EDGE ( 'NONE', *, *, #756, .F. ) ;
#18724 = EDGE_LOOP ( 'NONE', ( #37437, #3726, #41416, #3978 ) ) ;
#18725 = CARTESIAN_POINT ( 'NONE',  ( 1.357451270064000015, -81.76057078788299748, -0.6754762517246000186 ) ) ;
#18726 = VERTEX_POINT ( 'NONE', #3358 ) ;
#18727 = ORIENTED_EDGE ( 'NONE', *, *, #6168, .T. ) ;
#18728 = CARTESIAN_POINT ( 'NONE',  ( -1.933650113856000052, -18.59213746974000259, 12.70909635754000000 ) ) ;
#18729 = PLANE ( 'NONE',  #5601 ) ;
#18730 = VECTOR ( 'NONE', #12986, 1000.000000000000000 ) ;
#18731 = CARTESIAN_POINT ( 'NONE',  ( -1.553970433762575931, -81.43645831985729444, 3.072459199874610025 ) ) ;
#18732 = CARTESIAN_POINT ( 'NONE',  ( 2.860217300723919998, -78.25014487812663333, -8.801743088242798052 ) ) ;
#18733 = CARTESIAN_POINT ( 'NONE',  ( -5.413904038987160661, -78.08333333333332860, -9.393203674808278336 ) ) ;
#18734 = CARTESIAN_POINT ( 'NONE',  ( -1.748404684387999897, -78.71803539972999886, 11.93442954260999933 ) ) ;
#18735 = EDGE_LOOP ( 'NONE', ( #20040, #56608, #51639 ) ) ;
#18736 = ORIENTED_EDGE ( 'NONE', *, *, #57995, .F. ) ;
#18737 = DIRECTION ( 'NONE',  ( 0.000000000000000000, -1.000000000000000000, 2.322499949178999976E-14 ) ) ;
#18738 = CARTESIAN_POINT ( 'NONE',  ( -4.000000000000000000, -75.00000000000001421, 0.5999999999999999778 ) ) ;
#18739 = EDGE_CURVE ( 'NONE', #8049, #8827, #20613, .T. ) ;
#18740 = CARTESIAN_POINT ( 'NONE',  ( 4.299999999593000055, -81.99999999959300112, 2.324861064693000045E-09 ) ) ;
#18741 = CARTESIAN_POINT ( 'NONE',  ( -9.702231720816998362, -78.71113177888697976, -0.1934140619087000024 ) ) ;
#18742 = DIRECTION ( 'NONE',  ( 0.000000000000000000, -1.000000000000000000, 0.000000000000000000 ) ) ;
#18743 = CARTESIAN_POINT ( 'NONE',  ( 2.664092970791406056, -85.87263560081200353, 2.844305389928088790 ) ) ;
#18744 = CARTESIAN_POINT ( 'NONE',  ( -9.247037010692000791, -77.48029308464001019, -9.074963555248000802 ) ) ;
#18745 = CARTESIAN_POINT ( 'NONE',  ( -1.384313526018999818, -80.67041546398999685, -0.4900246725272000003 ) ) ;
#18746 = CARTESIAN_POINT ( 'NONE',  ( -12.71798269385000069, -23.29778754190000001, -1.931086388578000079 ) ) ;
#18747 = PLANE ( 'NONE',  #56730 ) ;
#18748 = CARTESIAN_POINT ( 'NONE',  ( 0.9273277571154000531, -81.25894104959499487, 4.068185826040000563 ) ) ;
#18749 = CARTESIAN_POINT ( 'NONE',  ( 7.551392188974999975, -80.01374543289598762, 8.117862728809001283 ) ) ;
#18750 = CARTESIAN_POINT ( 'NONE',  ( 8.353603324983998490, -78.77841001420199518, -4.904950430745999235 ) ) ;
#18751 = PLANE ( 'NONE',  #37139 ) ;
#18752 = CARTESIAN_POINT ( 'NONE',  ( 7.288337508342944027, -76.16067708288093741, -9.485192864111416711 ) ) ;
#18754 = CARTESIAN_POINT ( 'NONE',  ( -1.327706488546999797, -79.22934748844500064, -0.1249263990498000187 ) ) ;
#18753 = CARTESIAN_POINT ( 'NONE',  ( 11.00000000000000000, -4.000000000000000000, 0.000000000000000000 ) ) ;
#18755 = AXIS2_PLACEMENT_3D ( 'NONE', #25914, #30625, #48658 ) ;
#18756 = CARTESIAN_POINT ( 'NONE',  ( 9.505949683908001546, -79.00000000000000000, -6.906476714433999575 ) ) ;
#18757 = CARTESIAN_POINT ( 'NONE',  ( 3.887965725239291181, -79.99999999999998579, -8.725614487856105939 ) ) ;
#18758 = CARTESIAN_POINT ( 'NONE',  ( 1.068619641472000170, -1.964980382298999961, -3.652926003266999899 ) ) ;
#18759 = DIRECTION ( 'NONE',  ( 1.186310310053999794E-10, -0.9999999999999998890, -1.114594443524999723E-08 ) ) ;
#18760 = ORIENTED_EDGE ( 'NONE', *, *, #20710, .T. ) ;
#18761 = CARTESIAN_POINT ( 'NONE',  ( 9.723174507645000020, -61.27697503925999456, 7.958760295356000825 ) ) ;
#18762 = CARTESIAN_POINT ( 'NONE',  ( 7.892048199460342417, -60.54946977258678942, -7.664266801480966507 ) ) ;
#18763 = CARTESIAN_POINT ( 'NONE',  ( -11.28030014521100810, -77.67311482005982270, 3.843155223038057677 ) ) ;
#18764 = CARTESIAN_POINT ( 'NONE',  ( -4.854815601933999858, -79.41271639797899695, -8.456988451204999535 ) ) ;
#18765 = CARTESIAN_POINT ( 'NONE',  ( 11.82764905900999963, -77.26689612163998788, 5.426413045081000419 ) ) ;
#18766 = CARTESIAN_POINT ( 'NONE',  ( -7.882289591833920639, -79.54063170175217579, 7.310012099975937261 ) ) ;
#18767 = AXIS2_PLACEMENT_3D ( 'NONE', #56785, #21626, #39348 ) ;
#18768 = CARTESIAN_POINT ( 'NONE',  ( 9.832881223348001853, -79.13383998579799083, 0.5566273142183999489 ) ) ;
#18769 = DIRECTION ( 'NONE',  ( 0.000000000000000000, 0.000000000000000000, 1.000000000000000000 ) ) ;
#18770 = EDGE_LOOP ( 'NONE', ( #6528, #40152, #48121, #1035, #14896 ) ) ;
#18771 = EDGE_CURVE ( 'NONE', #14108, #393, #34917, .T. ) ;
#18772 = DIRECTION ( 'NONE',  ( 0.9999999999995751176, 0.000000000000000000, 9.217549102787771002E-07 ) ) ;
#18773 = CARTESIAN_POINT ( 'NONE',  ( -3.967749344305000037, -77.58280535679998025, 10.55286236287999913 ) ) ;
#18774 = EDGE_CURVE ( 'NONE', #8187, #26186, #22289, .T. ) ;
#18775 = CARTESIAN_POINT ( 'NONE',  ( 1.551259236285000176, -81.63757503623300238, -0.4083371041875000218 ) ) ;
#18776 = CARTESIAN_POINT ( 'NONE',  ( 7.613962827179999948, -23.30639625649999758, -10.53101998747000145 ) ) ;
#18777 = CARTESIAN_POINT ( 'NONE',  ( 4.657000555087000393, -77.62260406872297835, -8.305583776142999142 ) ) ;
#18779 = CARTESIAN_POINT ( 'NONE',  ( -3.587712099295000012, -1.780278923320000040, 1.801380527025000067 ) ) ;
#18778 = CARTESIAN_POINT ( 'NONE',  ( -4.139711922552000267, -84.67451069913499850, -0.5407357538481999404 ) ) ;
#18780 = CARTESIAN_POINT ( 'NONE',  ( 11.75000000000000000, -77.95000000000000284, 2.316376715183999699E-14 ) ) ;
#18781 = CARTESIAN_POINT ( 'NONE',  ( -0.9218200799623775810, -81.42708333333332860, 1.199500263597266247 ) ) ;
#18782 = ORIENTED_EDGE ( 'NONE', *, *, #43267, .F. ) ;
#18783 = B_SPLINE_CURVE_WITH_KNOTS ( 'NONE', 3,
 ( #51236, #27602, #24056, #45936, #14610, #33189, #28474, #6343, #32311, #24358, #42371, #55357, #14899, #50942, #46232, #55947, #783, #23764, #18763, #55063, #50069 ),
 .UNSPECIFIED., .F., .F.,
 ( 4, 2, 2, 2, 2, 2, 2, 2, 2, 1, 4 ),
 ( 0.000000000000000000, 0.1250000000000000833, 0.2500000000000001665, 0.3750000000000001665, 0.5000000000000002220, 0.5625000000000002220, 0.6250000000000003331, 0.7500000000000002220, 0.8125000000000002220, 0.8750000000000001110, 1.000000000000000000 ),
 .UNSPECIFIED. ) ;
#18784 = CARTESIAN_POINT ( 'NONE',  ( -7.474107310857593944, -77.16382243072474978, -7.726686437686844044 ) ) ;
#18785 = CARTESIAN_POINT ( 'NONE',  ( 7.223234266884172250, -79.12379502737748282, 9.635782272402776627 ) ) ;
#18786 = VERTEX_POINT ( 'NONE', #38498 ) ;
#18787 = VERTEX_POINT ( 'NONE', #47963 ) ;
#18788 = CARTESIAN_POINT ( 'NONE',  ( 0.000000000000000000, -3.500000000000000000, 0.000000000000000000 ) ) ;
#18789 = CARTESIAN_POINT ( 'NONE',  ( 0.000000000000000000, 4.040000000000000036, 0.000000000000000000 ) ) ;
#18790 = EDGE_CURVE ( 'NONE', #27707, #38980, #19892, .T. ) ;
#18791 = DIRECTION ( 'NONE',  ( 0.000000000000000000, -1.000000000000000000, -9.323016642051001034E-14 ) ) ;
#18792 = ORIENTED_EDGE ( 'NONE', *, *, #40129, .F. ) ;
#18793 = CARTESIAN_POINT ( 'NONE',  ( -1.931043762602999925, -59.57819125629999490, 12.75761570869000039 ) ) ;
#18794 = CARTESIAN_POINT ( 'NONE',  ( 4.928445265185000146, -78.34966785968099146, -10.99573548889999941 ) ) ;
#18795 = ORIENTED_EDGE ( 'NONE', *, *, #9869, .F. ) ;
#18796 = ORIENTED_EDGE ( 'NONE', *, *, #7728, .T. ) ;
#18797 = CARTESIAN_POINT ( 'NONE',  ( 7.342356150419315775, -59.98964892062895871, 8.190836719257342580 ) ) ;
#18798 = VECTOR ( 'NONE', #38680, 1000.000000000000000 ) ;
#18799 = VERTEX_POINT ( 'NONE', #56516 ) ;
#18800 = CARTESIAN_POINT ( 'NONE',  ( -6.043427764450832740, -78.71666666666668277, 10.48543666025107512 ) ) ;
#18801 = CARTESIAN_POINT ( 'NONE',  ( 9.064091738852273039, -79.17377439753506962, 2.844017911560304146 ) ) ;
#18802 = ORIENTED_EDGE ( 'NONE', *, *, #15765, .T. ) ;
#18803 = CARTESIAN_POINT ( 'NONE',  ( -8.583665413900087415, -53.82814424962094080, -9.102144265374381149 ) ) ;
#18804 = ORIENTED_EDGE ( 'NONE', *, *, #23189, .T. ) ;
#18805 = LINE ( 'NONE', #36797, #2634 ) ;
#18806 = DIRECTION ( 'NONE',  ( -1.000000000000000000, 0.000000000000000000, 0.000000000000000000 ) ) ;
#18807 = CONICAL_SURFACE ( 'NONE', #33871, 12.94999999994000106, 0.7853981633972997312 ) ;
#18808 = FACE_OUTER_BOUND ( 'NONE', #31011, .T. ) ;
#18809 = CARTESIAN_POINT ( 'NONE',  ( -12.24999999909999993, -80.79999999910000952, -7.143942175050000083E-09 ) ) ;
#18810 = CARTESIAN_POINT ( 'NONE',  ( -7.860507001410999450, -76.63534038853499908, 7.955276143908999842 ) ) ;
#18811 = LINE ( 'NONE', #22650, #32550 ) ;
#18812 = DIRECTION ( 'NONE',  ( 0.000000000000000000, -1.000000000000000000, 0.000000000000000000 ) ) ;
#18813 = CARTESIAN_POINT ( 'NONE',  ( -7.678667886039000301, -58.55736537918999574, -10.59548767697000038 ) ) ;
#18814 = CARTESIAN_POINT ( 'NONE',  ( -1.765078173649822668, -78.70978827431009961, -9.079997777801024128 ) ) ;
#18815 = CARTESIAN_POINT ( 'NONE',  ( 7.309900215520421796, -76.52113362030404176, 9.201699366411881797 ) ) ;
#18816 = CARTESIAN_POINT ( 'NONE',  ( -0.5999999999999999778, -23.15000000000000213, -10.98362417419999915 ) ) ;
#18817 = CARTESIAN_POINT ( 'NONE',  ( 1.170174673132000187, -79.92415236045100357, 0.6397400908730001001 ) ) ;
#18818 = CARTESIAN_POINT ( 'NONE',  ( -9.174184873855057987, -80.14666432379901551, -6.068958411681329324 ) ) ;
#18819 = CARTESIAN_POINT ( 'NONE',  ( -1.770955775045925495, -78.06626119840052525, -11.95106029758639110 ) ) ;
#18820 = CARTESIAN_POINT ( 'NONE',  ( -3.381245366627000148, -79.76428455456799327, 2.067162445164999696 ) ) ;
#18821 = EDGE_CURVE ( 'NONE', #19308, #25466, #2784, .T. ) ;
#18822 = CARTESIAN_POINT ( 'NONE',  ( -6.374294731314999574, -77.12551332859899844, 7.248560140069000290 ) ) ;
#18823 = CARTESIAN_POINT ( 'NONE',  ( -1.750000000000000000, -57.05022860762000647, 12.65375411742999923 ) ) ;
#18824 = CARTESIAN_POINT ( 'NONE',  ( -0.9577002445776288120, -83.04511862308959280, 0.8030944468889523735 ) ) ;
#18825 = CARTESIAN_POINT ( 'NONE',  ( 13.63885489310999510, -56.01421830980998351, 7.254376133916000668 ) ) ;
#18826 = CARTESIAN_POINT ( 'NONE',  ( 1.069786343357907787, -81.94992733943924179, -0.7820817253628982169 ) ) ;
#18827 = CARTESIAN_POINT ( 'NONE',  ( 6.528141900500715522, -79.99999999999998579, 6.772142874866426077 ) ) ;
#18828 = CARTESIAN_POINT ( 'NONE',  ( -1.211761727240999953, -0.6962337787935000133, 3.553101914771000125 ) ) ;
#18829 = DIRECTION ( 'NONE',  ( 0.000000000000000000, -1.000000000000000000, 0.000000000000000000 ) ) ;
#18830 = CARTESIAN_POINT ( 'NONE',  ( 6.969247251738771354, -79.79316764611728274, -6.112684341057344817 ) ) ;
#18831 = CARTESIAN_POINT ( 'NONE',  ( 1.569236785184999737E-14, 0.000000000000000000, 0.000000000000000000 ) ) ;
#18832 = CARTESIAN_POINT ( 'NONE',  ( -2.065550207748000133, -23.42565079331000177, -12.82162303854000029 ) ) ;
#18833 = CARTESIAN_POINT ( 'NONE',  ( 13.89248034750000116, -69.19159251015000223, 2.632538495191000193E-05 ) ) ;
#18834 = CARTESIAN_POINT ( 'NONE',  ( -2.978010235239999748, -2.500894741108000030, 1.811261547873000088 ) ) ;
#18835 = CARTESIAN_POINT ( 'NONE',  ( -0.3271848554490991434, -80.60416666666665719, -1.217465845835395299 ) ) ;
#18836 = CARTESIAN_POINT ( 'NONE',  ( -11.14010510836999934, -77.40796654052100223, -5.166607915801000317 ) ) ;
#18837 = CARTESIAN_POINT ( 'NONE',  ( -11.00000000000000000, -78.10953167777607575, -1.317564550621140196 ) ) ;
#18839 = CARTESIAN_POINT ( 'NONE',  ( 1.407891339063999991, -79.05671151888600434, 0.1670362498605000023 ) ) ;
#18838 = CARTESIAN_POINT ( 'NONE',  ( 11.19999999999999929, -74.80000000000001137, 0.000000000000000000 ) ) ;
#18840 = CARTESIAN_POINT ( 'NONE',  ( 0.7233469165846999616, -82.92988695178998171, -1.541617362406000113 ) ) ;
#18841 = EDGE_LOOP ( 'NONE', ( #27690, #45896, #19373, #41519 ) ) ;
#18842 = CARTESIAN_POINT ( 'NONE',  ( 3.473803517655999595, -84.07757450217398798, -0.9035632974999000533 ) ) ;
#18843 = CARTESIAN_POINT ( 'NONE',  ( 1.303850919141000153, -79.25712671310500923, -11.85478070107000015 ) ) ;
#18844 = CARTESIAN_POINT ( 'NONE',  ( -4.745830983694999894, -81.18645468754350247, 10.10305395880000034 ) ) ;
#18845 = EDGE_CURVE ( 'NONE', #23097, #12605, #31653, .T. ) ;
#18846 = CARTESIAN_POINT ( 'NONE',  ( -8.597176310153894718, -79.99999999999998579, -3.571827255421711200 ) ) ;
#18847 = CARTESIAN_POINT ( 'NONE',  ( 1.522508719054618709, -85.71458334025085435, 3.052348956963513160 ) ) ;
#18848 = CARTESIAN_POINT ( 'NONE',  ( 12.54987159811999931, -53.74886760158999977, -0.1385534523824999975 ) ) ;
#18849 = PLANE ( 'NONE',  #25517 ) ;
#18850 = CARTESIAN_POINT ( 'NONE',  ( -3.336429633373000136, -0.6982797842361000429, 0.8683076097535999960 ) ) ;
#18851 = CARTESIAN_POINT ( 'NONE',  ( 10.13881649148000008, -76.50783510652000530, -5.938594122520999719 ) ) ;
#18852 = CARTESIAN_POINT ( 'NONE',  ( -6.187990949381768857, -77.00000000000000000, 6.880426350252046852 ) ) ;
#18853 = ORIENTED_EDGE ( 'NONE', *, *, #4889, .F. ) ;
#18854 = CARTESIAN_POINT ( 'NONE',  ( 1.575772165460815666, -54.33845457181070060, -12.70597445614748366 ) ) ;
#18855 = VECTOR ( 'NONE', #10453, 1000.000000000000000 ) ;
#18856 = CARTESIAN_POINT ( 'NONE',  ( 9.342273945276998504, -79.45871332859898928, 1.855243057797000050 ) ) ;
#18857 = CARTESIAN_POINT ( 'NONE',  ( 11.63975115694809226, -75.93720323772257075, -1.845775132419555487 ) ) ;
#18858 = CARTESIAN_POINT ( 'NONE',  ( 7.601397897754999633, -60.04999999966999980, 9.369164850722000892 ) ) ;
#18859 = DIRECTION ( 'NONE',  ( -1.000000000000000000, 0.000000000000000000, 0.000000000000000000 ) ) ;
#18860 = ADVANCED_FACE ( 'NONE', ( #27520 ), #128, .F. ) ;
#18861 = CARTESIAN_POINT ( 'NONE',  ( 10.98464796637060026, -23.30469563149855361, 0.5810037832618359932 ) ) ;
#18862 = ORIENTED_EDGE ( 'NONE', *, *, #54504, .T. ) ;
#18863 = CARTESIAN_POINT ( 'NONE',  ( 10.43567240482000003, -78.62076856562599403, 6.472443173969999464 ) ) ;
#18864 = CARTESIAN_POINT ( 'NONE',  ( 10.82024634786000128, -78.24439760156698753, 0.1816028081696000052 ) ) ;
#18865 = CARTESIAN_POINT ( 'NONE',  ( -1.667916687331000070, -18.70151115557999688, 12.49168451098999988 ) ) ;
#18866 = EDGE_LOOP ( 'NONE', ( #5213, #31276, #32408, #14583, #18920, #5285, #44617, #16615, #47391 ) ) ;
#18867 = DIRECTION ( 'NONE',  ( 0.000000000000000000, 0.000000000000000000, -1.000000000000000000 ) ) ;
#18868 = CARTESIAN_POINT ( 'NONE',  ( 9.523132023602000729, -80.14961334339898258, 1.108936319727999997 ) ) ;
#18869 = ORIENTED_EDGE ( 'NONE', *, *, #3610, .F. ) ;
#18870 = CARTESIAN_POINT ( 'NONE',  ( -12.22965310686000073, -76.12113747164599431, 0.3492514087541000456 ) ) ;
#18871 = CARTESIAN_POINT ( 'NONE',  ( 10.41172477448170497, -23.52013115057688353, -7.610718073406644635 ) ) ;
#18872 = PRESENTATION_LAYER_ASSIGNMENT (  '', '', ( #36766 ) ) ;
#18873 = CARTESIAN_POINT ( 'NONE',  ( 0.7435525986707999246, -78.04141375144000392, 1.342724626677000099 ) ) ;
#18874 = EDGE_LOOP ( 'NONE', ( #13991, #44678, #6148, #14026 ) ) ;
#18875 = CARTESIAN_POINT ( 'NONE',  ( -2.205007487985999770, -76.96359805011501010, 9.235565851336001941 ) ) ;
#18876 = CARTESIAN_POINT ( 'NONE',  ( -0.4665716294809927334, -80.19474127330990143, -1.159543645027278247 ) ) ;
#18877 = CARTESIAN_POINT ( 'NONE',  ( 1.101185748242720974, -77.87369791681820175, -0.8451993228706300432 ) ) ;
#18878 = CARTESIAN_POINT ( 'NONE',  ( 7.032399328097561408, -79.90636888539235372, 6.008881161021868422 ) ) ;
#18879 = CARTESIAN_POINT ( 'NONE',  ( 1.101723890961501473, -79.15951310949000685, 1.033017321146173506 ) ) ;
#18880 = CARTESIAN_POINT ( 'NONE',  ( -2.835184365519229477, -80.01041666022817367, 2.893239195999958824 ) ) ;
#18881 = EDGE_LOOP ( 'NONE', ( #2959, #37735, #7071, #39221 ) ) ;
#18882 = CARTESIAN_POINT ( 'NONE',  ( -9.252740428349008894, -77.77916666666668277, 2.486604901413127955 ) ) ;
#18883 = CARTESIAN_POINT ( 'NONE',  ( 9.569482281372000188, -76.67852883436000866, -7.743360016082000641 ) ) ;
#18884 = CARTESIAN_POINT ( 'NONE',  ( 1.237149555198000073, -79.60251943783799788, -1.037631781681999987 ) ) ;
#18885 = B_SPLINE_SURFACE_WITH_KNOTS ( 'NONE', 3, 3, ( 
 ( #12779, #52946, #7495, #17503 ),
 ( #34341, #3639, #31061, #3074 ),
 ( #25784, #38783, #21642, #39649 ),
 ( #21068, #35198, #43810, #57654 ),
 ( #43513, #39933, #39074, #12496 ),
 ( #56801, #49099, #57082, #57949 ),
 ( #21352, #48809, #30775, #3922 ),
 ( #12212, #7784, #13063, #17210 ) ),
 .UNSPECIFIED., .F., .F., .F.,
 ( 4, 1, 1, 1, 1, 4 ),
 ( 4, 4 ),
 ( -0.01200407347463999970, 0.000000000000000000, 0.3333333333333000081, 0.6666666666667000474, 1.000000000000000000, 1.011997855551999947 ),
 ( -0.3559705542741999906, 1.355970554273999928 ),
 .UNSPECIFIED. ) ;
#18886 = EDGE_CURVE ( 'NONE', #46616, #51746, #45562, .T. ) ;
#18887 = AXIS2_PLACEMENT_3D ( 'NONE', #15073, #51406, #46697 ) ;
#18888 = CARTESIAN_POINT ( 'NONE',  ( -1.161914544699476082, -1.947542654857316924, -3.323423654541866945 ) ) ;
#18889 = CARTESIAN_POINT ( 'NONE',  ( 12.69619287815999975, -20.24916621771999914, 1.799475295154000065 ) ) ;
#18890 = CARTESIAN_POINT ( 'NONE',  ( 9.000511195990998914, -79.32543968971000936, 8.067084866081000172 ) ) ;
#18891 = CARTESIAN_POINT ( 'NONE',  ( 8.135116633385999663, -77.01906566427899747, 9.200136113044999675 ) ) ;
#18892 = CARTESIAN_POINT ( 'NONE',  ( -3.654181830570668144, -86.07389998728979208, 1.626946572303400451 ) ) ;
#18893 = EDGE_CURVE ( 'NONE', #41874, #20606, #29816, .T. ) ;
#18894 = CARTESIAN_POINT ( 'NONE',  ( -7.730500772889000061, -79.99284890031098882, 8.045567737375000306 ) ) ;
#18895 = CARTESIAN_POINT ( 'NONE',  ( 3.088929962604149093, -2.826175003995697654, -1.008836435391547770 ) ) ;
#18896 = CARTESIAN_POINT ( 'NONE',  ( -1.872499823463115165, -77.16255644686364690, -11.87122717985699794 ) ) ;
#18897 = CARTESIAN_POINT ( 'NONE',  ( -10.06692933833248027, -18.29657287077820627, 7.655995045172840463 ) ) ;
#18898 = ORIENTED_EDGE ( 'NONE', *, *, #31409, .T. ) ;
#18899 = CARTESIAN_POINT ( 'NONE',  ( -1.211920851286000023, -81.49548374185999933, -0.6339750518301998650 ) ) ;
#18900 = CARTESIAN_POINT ( 'NONE',  ( -1.250231197918746817, -78.61063498648076120, -0.1636698104632014206 ) ) ;
#18901 = CARTESIAN_POINT ( 'NONE',  ( 8.114920487384752690, -24.82884529334158685, 9.847900218102966008 ) ) ;
#18902 = CARTESIAN_POINT ( 'NONE',  ( 0.1636246173744642929, -82.86458333333334281, 1.250000000000000888 ) ) ;
#18903 = CARTESIAN_POINT ( 'NONE',  ( 7.836764916234119305, -24.30511429678713853, 9.850487231000405686 ) ) ;
#18904 = CARTESIAN_POINT ( 'NONE',  ( 10.24006772854000147, -78.30304150121298790, 6.351124671173999481 ) ) ;
#18905 = CARTESIAN_POINT ( 'NONE',  ( 7.201320854070999644, -77.51472321436799007, 6.394856364399000626 ) ) ;
#18906 = CARTESIAN_POINT ( 'NONE',  ( -0.06404916490611077540, -76.07508406693142433, 11.74976712695074177 ) ) ;
#18907 = CARTESIAN_POINT ( 'NONE',  ( 9.298000630789001519, -79.25408516179498974, 5.937079976835999418 ) ) ;
#18908 = CARTESIAN_POINT ( 'NONE',  ( -2.350111744379241863, -86.10000000000017906, 3.172282531658992877 ) ) ;
#18909 = ORIENTED_EDGE ( 'NONE', *, *, #53369, .T. ) ;
#18910 = CARTESIAN_POINT ( 'NONE',  ( 7.970415440365194115, -17.47707676838366808, -9.713035532436524733 ) ) ;
#18911 = CARTESIAN_POINT ( 'NONE',  ( 1.210731304718440926, -77.96474580276972688, 9.250079891894303685 ) ) ;
#18912 = CONICAL_SURFACE ( 'NONE', #51922, 11.54999999996000071, 0.7853981633972997312 ) ;
#18913 = CARTESIAN_POINT ( 'NONE',  ( -6.532344017558930460, -76.27800419209582117, -9.766768203399665893 ) ) ;
#18914 = CARTESIAN_POINT ( 'NONE',  ( -10.87500000000999911, -76.17499999999400018, 1.221063213659000093E-09 ) ) ;
#18915 = CARTESIAN_POINT ( 'NONE',  ( -2.879226727952096443, -79.20416666666665151, -10.71369944335146940 ) ) ;
#18916 = CARTESIAN_POINT ( 'NONE',  ( -7.918603267607000618, -76.30298211639099293, 9.677277400644999972 ) ) ;
#18917 = DIRECTION ( 'NONE',  ( -0.7071067811865475727, 0.000000000000000000, 0.7071067811865475727 ) ) ;
#18918 = CARTESIAN_POINT ( 'NONE',  ( 9.770419344679000417, -16.94469452567000189, -8.292776877939001423 ) ) ;
#18919 = CARTESIAN_POINT ( 'NONE',  ( 8.872949060679459876, -16.98989818440303523, 8.813905828569408740 ) ) ;
#18920 = ORIENTED_EDGE ( 'NONE', *, *, #29687, .F. ) ;
#18921 = CARTESIAN_POINT ( 'NONE',  ( 7.759949366729999909, -78.89513978978800424, -8.002361301306001096 ) ) ;
#18922 = CARTESIAN_POINT ( 'NONE',  ( 12.70395600756419263, -54.19327811274377638, 1.447166682392545312 ) ) ;
#18923 = CARTESIAN_POINT ( 'NONE',  ( -1.628633640557669793, -79.43583583485381894, 11.72084692437723596 ) ) ;
#18924 = CARTESIAN_POINT ( 'NONE',  ( -0.03344200926162519544, -78.43735717367049176, 3.548192316444005456 ) ) ;
#18925 = DIRECTION ( 'NONE',  ( -0.7071067811865474617, 0.000000000000000000, 0.7071067811865474617 ) ) ;
#18927 = CARTESIAN_POINT ( 'NONE',  ( -0.9038625163532321150, -81.53983264272325471, 0.8630782802490172267 ) ) ;
#18926 = CARTESIAN_POINT ( 'NONE',  ( -1.283123261360999967, -81.17673743600398950, -0.3068555137751999840 ) ) ;
#18928 = EDGE_CURVE ( 'NONE', #38464, #47139, #33620, .T. ) ;
#18929 = AXIS2_PLACEMENT_3D ( 'NONE', #12815, #39111, #8107 ) ;
#18930 = CARTESIAN_POINT ( 'NONE',  ( -9.329078564973897869, -76.99999999999998579, -0.4380577504101695885 ) ) ;
#18931 = CARTESIAN_POINT ( 'NONE',  ( 10.98364304930883151, -23.23021036681280549, -0.5996544714383750252 ) ) ;
#18932 = EDGE_CURVE ( 'NONE', #14174, #245, #55296, .T. ) ;
#18933 = AXIS2_PLACEMENT_3D ( 'NONE', #25147, #7721, #38435 ) ;
#18934 = CARTESIAN_POINT ( 'NONE',  ( -0.06733317885808998149, -78.76457060935999266, -1.419816196976000144 ) ) ;
#18935 = CARTESIAN_POINT ( 'NONE',  ( 9.009247259181915268, -79.77083333333335702, 2.421167930323361972 ) ) ;
#18936 = CARTESIAN_POINT ( 'NONE',  ( -6.920450493081392374, -79.52081221549906331, -8.519106985839389523 ) ) ;
#18937 = CARTESIAN_POINT ( 'NONE',  ( -8.084188863228343180, -79.71354166666438346, -4.672135182878759174 ) ) ;
#18938 = VERTEX_POINT ( 'NONE', #17809 ) ;
#18939 = ORIENTED_EDGE ( 'NONE', *, *, #47656, .F. ) ;
#18940 = CARTESIAN_POINT ( 'NONE',  ( -9.500000000000007105, -77.89249999999998408, 0.8953539062730669906 ) ) ;
#18941 = CARTESIAN_POINT ( 'NONE',  ( 6.844432534029042614, -78.78001192501054106, -8.289462398550917044 ) ) ;
#18942 = VERTEX_POINT ( 'NONE', #23106 ) ;
#18943 = CARTESIAN_POINT ( 'NONE',  ( -10.15953550767560287, -76.71853632512886634, 4.239958222269431865 ) ) ;
#18944 = CARTESIAN_POINT ( 'NONE',  ( -1.594109084609295790, -82.93958334889045148, 3.052517646826329312 ) ) ;
#18945 = EDGE_CURVE ( 'NONE', #13072, #34714, #49657, .T. ) ;
#18946 = CARTESIAN_POINT ( 'NONE',  ( 7.943805570375999991, -61.23402324491999593, 9.641149735098998974 ) ) ;
#18947 = LINE ( 'NONE', #54669, #27749 ) ;
#18948 = CARTESIAN_POINT ( 'NONE',  ( -11.48800504392370136, -78.07278836372438491, -3.397901037234756672 ) ) ;
#18949 = CARTESIAN_POINT ( 'NONE',  ( -1.780884232981000181, -79.94620619628149427, -11.07459082487999957 ) ) ;
#18950 = CARTESIAN_POINT ( 'NONE',  ( 3.249249792562667771, -1.841632792895788073, -0.4039650473228960648 ) ) ;
#18951 = ORIENTED_EDGE ( 'NONE', *, *, #45353, .F. ) ;
#18952 = CARTESIAN_POINT ( 'NONE',  ( -8.803747447820532201, -25.21568152340251601, 9.164340453613974091 ) ) ;
#18953 = ORIENTED_EDGE ( 'NONE', *, *, #57145, .F. ) ;
#18954 = CARTESIAN_POINT ( 'NONE',  ( 9.147648472655747653, -77.36201978443682492, 1.373573847259280889 ) ) ;
#18955 = CARTESIAN_POINT ( 'NONE',  ( -8.283402485401001769, -77.98762868280198290, -7.298588567667000149 ) ) ;
#18956 = B_SPLINE_CURVE_WITH_KNOTS ( 'NONE', 3,
 ( #2525, #44121, #11389, #11960, #3670, #21670, #47414, #47703, #7526, #43540, #3104, #57112, #16678, #17534, #8381, #27256, #22251, #35525 ),
 .UNSPECIFIED., .F., .F.,
 ( 4, 2, 2, 2, 2, 2, 2, 2, 4 ),
 ( 0.000000000000000000, 0.1250000000000000000, 0.2500000000000000000, 0.3750000000000000000, 0.5000000000000000000, 0.6250000000000000000, 0.7500000000000000000, 0.8750000000000000000, 1.000000000000000000 ),
 .UNSPECIFIED. ) ;
#18957 = CARTESIAN_POINT ( 'NONE',  ( 8.899186938125001944, -76.04999999999999716, 6.465637775217000005 ) ) ;
#18958 = CARTESIAN_POINT ( 'NONE',  ( -1.428376501803000131, -77.53332085210548996, 0.2580938706625000023 ) ) ;
#18959 = CARTESIAN_POINT ( 'NONE',  ( -9.466955267137999286, -76.30209268829000280, -8.391502601560000940 ) ) ;
#18960 = CARTESIAN_POINT ( 'NONE',  ( -9.596002108778160178, -78.45208333333329165, -7.374560639698984232 ) ) ;
#18961 = CARTESIAN_POINT ( 'NONE',  ( 1.623578234368999951, -78.02589724511999236, 0.1125035222880000074 ) ) ;
#18962 = CARTESIAN_POINT ( 'NONE',  ( 12.00000000000000000, -79.65000000000000568, 0.000000000000000000 ) ) ;
#18963 = EDGE_CURVE ( 'NONE', #18159, #14764, #54116, .T. ) ;
#18964 = B_SPLINE_CURVE_WITH_KNOTS ( 'NONE', 3,
 ( #19046, #37037, #14018, #55052, #27303, #31129, #35870, #17880, #8720, #44742, #31432, #4293, #22293, #53899, #18465, #9022, #13727, #4596 ),
 .UNSPECIFIED., .F., .F.,
 ( 4, 2, 2, 2, 2, 2, 2, 2, 4 ),
 ( 0.000000000000000000, 0.1250000000000000000, 0.2500000000000000000, 0.3750000000000000000, 0.5000000000000000000, 0.6250000000000000000, 0.7500000000000000000, 0.8750000000000000000, 1.000000000000000000 ),
 .UNSPECIFIED. ) ;
#18965 = CARTESIAN_POINT ( 'NONE',  ( 10.68099162494999987, -79.69654329274898430, 2.367326398803000220 ) ) ;
#18966 = CARTESIAN_POINT ( 'NONE',  ( -8.950141054446001831, -25.20112627276999717, -8.958565985356999661 ) ) ;
#18967 = CARTESIAN_POINT ( 'NONE',  ( -7.353725627630922190, -60.10655143787149512, 8.180687091746444040 ) ) ;
#18968 = CARTESIAN_POINT ( 'NONE',  ( 1.884913056600999948, -85.50468686974798516, 3.054645663329999650 ) ) ;
#18969 = ORIENTED_EDGE ( 'NONE', *, *, #39304, .F. ) ;
#18970 = CARTESIAN_POINT ( 'NONE',  ( 11.88227737747000035, -79.09962671310499616, -3.660809691553999823 ) ) ;
#18971 = AXIS2_PLACEMENT_3D ( 'NONE', #1539, #19531, #28666 ) ;
#18972 = CARTESIAN_POINT ( 'NONE',  ( 10.62431421503999829, -76.29661320193899599, -3.719179278686000067 ) ) ;
#18973 = CARTESIAN_POINT ( 'NONE',  ( 6.557452544417663454, -77.92303101572309743, 8.547671910063542100 ) ) ;
#18974 = CARTESIAN_POINT ( 'NONE',  ( 11.88382656225999945, -78.30602506152000331, -1.513515996960000054 ) ) ;
#18975 = DIRECTION ( 'NONE',  ( 0.000000000000000000, -1.000000000000000000, 0.000000000000000000 ) ) ;
#18976 = AXIS2_PLACEMENT_3D ( 'NONE', #25740, #16026, #3032 ) ;
#18977 = DIRECTION ( 'NONE',  ( 0.000000000000000000, -1.000000000000000000, 0.000000000000000000 ) ) ;
#18978 = CARTESIAN_POINT ( 'NONE',  ( 2.633249659506597951, -2.559142350340922967, 2.439935635806470327 ) ) ;
#18979 = CARTESIAN_POINT ( 'NONE',  ( 3.801865584756635386, -80.94637847883083737, 10.05558785843397196 ) ) ;
#18980 = CARTESIAN_POINT ( 'NONE',  ( 8.297164401012999235, -78.86501084750798896, 4.009864491784999707 ) ) ;
#18981 = CARTESIAN_POINT ( 'NONE',  ( 3.140027144888978938, -85.94828564506399005, -1.398030157552047070 ) ) ;
#18982 = CARTESIAN_POINT ( 'NONE',  ( 1.499018853861999956, -77.75540253813299785, 11.04570246958999924 ) ) ;
#18983 = CARTESIAN_POINT ( 'NONE',  ( -1.359416874709192810E-05, -0.8285695117701413759, -3.421591653122290300 ) ) ;
#18984 = CARTESIAN_POINT ( 'NONE',  ( -5.192477750132000303, -81.04484212712090141, -9.726524605103000098 ) ) ;
#18985 = ORIENTED_EDGE ( 'NONE', *, *, #54547, .T. ) ;
#18986 = DIRECTION ( 'NONE',  ( 0.000000000000000000, -1.000000000000000000, 0.000000000000000000 ) ) ;
#18987 = CARTESIAN_POINT ( 'NONE',  ( -1.753528938721999886, -2.394178536415000114, -3.557562347021000271 ) ) ;
#18988 = CARTESIAN_POINT ( 'NONE',  ( -3.633103876188000125, -77.09956540939499803, 10.61219425078000000 ) ) ;
#18989 = CARTESIAN_POINT ( 'NONE',  ( 10.74341457190999982, -79.04314778309698397, -2.245675826504000216 ) ) ;
#18990 = CARTESIAN_POINT ( 'NONE',  ( 7.758897894424999997, -24.30081253449000300, -10.31443085083000000 ) ) ;
#18991 = CARTESIAN_POINT ( 'NONE',  ( 3.123304715064033843, -82.61197914874944104, 2.518555082941037249 ) ) ;
#18992 = CARTESIAN_POINT ( 'NONE',  ( 7.483407197968000801, -79.75000000000000000, -5.437013583705000208 ) ) ;
#18993 = CARTESIAN_POINT ( 'NONE',  ( -8.121706841713852043, -53.96372996666369204, -9.841114038372756667 ) ) ;
#18994 = CARTESIAN_POINT ( 'NONE',  ( -2.666133258262000094, -84.47167953870898316, 3.209093106279000018 ) ) ;
#18995 = CARTESIAN_POINT ( 'NONE',  ( -1.460959015002473382, -79.52083333333332860, -0.3926218265389205819 ) ) ;
#18996 = CARTESIAN_POINT ( 'NONE',  ( 10.19019671030999952, -55.60356357307000508, -7.646965722228999951 ) ) ;
#18997 = CONICAL_SURFACE ( 'NONE', #21794, 9.099999999966000175, 0.7853981633972997312 ) ;
#18998 = CARTESIAN_POINT ( 'NONE',  ( 6.245083526999000156, -78.35094147377398599, -9.376985981987999708 ) ) ;
#18999 = LINE ( 'NONE', #27543, #49370 ) ;
#19000 = CARTESIAN_POINT ( 'NONE',  ( 0.1159286286506000102, -78.88797770777999574, 1.315005111595999976 ) ) ;
#19001 = CARTESIAN_POINT ( 'NONE',  ( -3.140974612311351777, -79.40416666666665435, -11.68767212001978884 ) ) ;
#19002 = CARTESIAN_POINT ( 'NONE',  ( -0.2221408358902347280, -81.86333133491983460, -1.493708899689074387 ) ) ;
#19003 = DIRECTION ( 'NONE',  ( 0.000000000000000000, 0.000000000000000000, -1.000000000000000000 ) ) ;
#19004 = CARTESIAN_POINT ( 'NONE',  ( 14.00000000000000000, -46.09579702914000165, 0.000000000000000000 ) ) ;
#19005 = CARTESIAN_POINT ( 'NONE',  ( 5.838193839761705917, -77.97708333333333997, -7.596835002782701629 ) ) ;
#19006 = CARTESIAN_POINT ( 'NONE',  ( 12.52133763467702110, -54.87246868424995938, -1.618901766958426469 ) ) ;
#19007 = ORIENTED_EDGE ( 'NONE', *, *, #26588, .T. ) ;
#19008 = CARTESIAN_POINT ( 'NONE',  ( -0.2175832845984233821, -81.71159084714736309, -1.231031275339559583 ) ) ;
#19009 = SHAPE_REPRESENTATION_RELATIONSHIP ( 'NONE' , 'NONE' ,  #33899, #34903 ) ;
#19010 = CARTESIAN_POINT ( 'NONE',  ( 8.677112325477001065, -80.26182985286258997, 6.812460760216000111 ) ) ;
#19011 = LINE ( 'NONE', #37004, #8246 ) ;
#19012 = ORIENTED_EDGE ( 'NONE', *, *, #37486, .T. ) ;
#19013 = ORIENTED_EDGE ( 'NONE', *, *, #10942, .F. ) ;
#19014 = CARTESIAN_POINT ( 'NONE',  ( -1.045973596602999933, -81.61173291773999949, -1.097670891906999957 ) ) ;
#19015 = VECTOR ( 'NONE', #48432, 1000.000000000000000 ) ;
#19016 = ORIENTED_EDGE ( 'NONE', *, *, #55500, .F. ) ;
#19017 = ORIENTED_EDGE ( 'NONE', *, *, #48303, .F. ) ;
#19018 = TOROIDAL_SURFACE ( 'NONE', #11484, 8.500000000000000000, 2.000000000000000000 ) ;
#19019 = CARTESIAN_POINT ( 'NONE',  ( 0.5154756746315999338, -16.86759400236999795, 12.66205448072999928 ) ) ;
#19020 = CARTESIAN_POINT ( 'NONE',  ( -9.850513605849648968, -54.49492088415082236, -7.836738268828330689 ) ) ;
#19021 = SHAPE_DEFINITION_REPRESENTATION ( #57332, #58051 ) ;
#19022 = EDGE_CURVE ( 'NONE', #34390, #9865, #10061, .T. ) ;
#19023 = CARTESIAN_POINT ( 'NONE',  ( -2.805830205465538629, -81.55208331940609412, 1.995571323810327424 ) ) ;
#19024 = CARTESIAN_POINT ( 'NONE',  ( -9.144741847372999999, -78.85421001420199616, -4.101371784086000005 ) ) ;
#19025 = CARTESIAN_POINT ( 'NONE',  ( 3.543073089441956203, -78.25632233163848639, -8.544503082031068786 ) ) ;
#19026 = CARTESIAN_POINT ( 'NONE',  ( 2.813789756862274505, -78.14583333333331439, -10.47020627418438821 ) ) ;
#19027 = ORIENTED_EDGE ( 'NONE', *, *, #51400, .T. ) ;
#19028 = VERTEX_POINT ( 'NONE', #26935 ) ;
#19029 = CARTESIAN_POINT ( 'NONE',  ( -8.797281764083550115, -77.57502926220332995, 2.858311938275306385 ) ) ;
#19030 = DIRECTION ( 'NONE',  ( 0.000000000000000000, -1.000000000000000000, 0.000000000000000000 ) ) ;
#19031 = DIRECTION ( 'NONE',  ( 0.5721800012453843731, -0.8201280669351780350, 0.000000000000000000 ) ) ;
#19032 = CARTESIAN_POINT ( 'NONE',  ( -1.821913034590999348E-14, -80.60000000000000853, -12.05000000000000071 ) ) ;
#19033 = CARTESIAN_POINT ( 'NONE',  ( 9.662203867310999783, -79.02724916671898825, 0.9012207007054000574 ) ) ;
#19034 = CARTESIAN_POINT ( 'NONE',  ( 10.10713367729994872, -61.26653151294045330, 7.860990029212568508 ) ) ;
#19035 = CARTESIAN_POINT ( 'NONE',  ( 1.750000000000000000, -60.04999999657000131, -12.50000000000000000 ) ) ;
#19036 = CARTESIAN_POINT ( 'NONE',  ( -10.50899237707999845, -77.86882557138000038, 7.577845091584000770 ) ) ;
#19037 = EDGE_CURVE ( 'NONE', #18065, #3338, #39265, .T. ) ;
#19038 = CARTESIAN_POINT ( 'NONE',  ( 1.447659443890000119, -80.92320979808999937, -0.6470525719642999940 ) ) ;
#19039 = DIRECTION ( 'NONE',  ( -0.4045602624632933519, 0.8201597332661866302, 0.4045602624632933519 ) ) ;
#19040 = CARTESIAN_POINT ( 'NONE',  ( -8.444233576716495548, -76.63875340865895680, 8.172707986422794946 ) ) ;
#19041 = B_SPLINE_CURVE_WITH_KNOTS ( 'NONE', 3,
 ( #15438, #37572, #6280, #32543, #45876, #55588 ),
 .UNSPECIFIED., .F., .F.,
 ( 4, 1, 1, 4 ),
 ( 0.000000000000000000, 0.3333333333333000081, 0.6666666666667000474, 1.000000000000000000 ),
 .UNSPECIFIED. ) ;
#19042 = COLOUR_RGB ( '', 0.09019608, 0.27058824, 0.51372549) ;
#19043 = CARTESIAN_POINT ( 'NONE',  ( -3.561876371173000155, -80.12548912224700359, 2.177761901471999995 ) ) ;
#19044 = CARTESIAN_POINT ( 'NONE',  ( -10.34138800174999950, -80.73365051625088995, 4.468208825537999473 ) ) ;
#19045 = CARTESIAN_POINT ( 'NONE',  ( -1.570796326794938524, -76.68541666666665435, 11.99999999999999645 ) ) ;
#19046 = CARTESIAN_POINT ( 'NONE',  ( -11.75000000000000000, -76.70000000000000284, 1.487410190129999909E-14 ) ) ;
#19047 = CARTESIAN_POINT ( 'NONE',  ( -3.543875382632000193, -80.20807046129100115, 0.1596868623460999947 ) ) ;
#19048 = CARTESIAN_POINT ( 'NONE',  ( -0.9420598709024999851, -79.23518609424799308, -0.8215979549846998964 ) ) ;
#19049 = CARTESIAN_POINT ( 'NONE',  ( 6.043427764450763462, -78.23333333333330586, 10.48543666025111065 ) ) ;
#19050 = CARTESIAN_POINT ( 'NONE',  ( 11.99999999887680957, -79.24999999999998579, 1.256637070374686971 ) ) ;
#19051 = EDGE_CURVE ( 'NONE', #3192, #24970, #43998, .T. ) ;
#19052 = CARTESIAN_POINT ( 'NONE',  ( -1.209804193477999945, -2.416592054135000112, -3.608664049297999998 ) ) ;
#19053 = DIRECTION ( 'NONE',  ( 0.000000000000000000, 1.000000000000000000, 0.000000000000000000 ) ) ;
#19054 = ORIENTED_EDGE ( 'NONE', *, *, #13316, .T. ) ;
#19055 = CARTESIAN_POINT ( 'NONE',  ( -1.840981145238566263, -3.500000000000000888, -2.837856670349830690 ) ) ;
#19056 = CARTESIAN_POINT ( 'NONE',  ( 7.401770473313899146, -60.25155696365192171, -8.137215171344832854 ) ) ;
#19057 = ADVANCED_FACE ( 'NONE', ( #18396 ), #26353, .F. ) ;
#19058 = FACE_OUTER_BOUND ( 'NONE', #8737, .T. ) ;
#19059 = CARTESIAN_POINT ( 'NONE',  ( -8.906990490675001482, -79.29582576494699708, 3.969308329408999469 ) ) ;
#19060 = CIRCLE ( 'NONE', #41677, 0.8000000000000000444 ) ;
#19061 = CARTESIAN_POINT ( 'NONE',  ( 9.175280770439000477, -76.64017995137999151, -8.221808909867000636 ) ) ;
#19062 = CARTESIAN_POINT ( 'NONE',  ( 7.556724790768792666, -79.41296073501848696, 7.645833190873140950 ) ) ;
#19063 = AXIS2_PLACEMENT_3D ( 'NONE', #43757, #57895, #3588 ) ;
#19064 = CARTESIAN_POINT ( 'NONE',  ( 2.823168074518000115, -79.09231332859899055, -8.995533882827999150 ) ) ;
#19065 = DIRECTION ( 'NONE',  ( 0.000000000000000000, -1.000000000000000000, 0.000000000000000000 ) ) ;
#19066 = FACE_OUTER_BOUND ( 'NONE', #50575, .T. ) ;
#19067 = CARTESIAN_POINT ( 'NONE',  ( 3.020225255027999989, -77.32576797881199582, -10.86205221496000028 ) ) ;
#19068 = CARTESIAN_POINT ( 'NONE',  ( 0.9071727510942999562, -81.67625285498098719, 1.202471848463999793 ) ) ;
#19069 = DIRECTION ( 'NONE',  ( -0.7071067811865473507, 1.433669009702094715E-08, 0.7071067811865473507 ) ) ;
#19070 = CARTESIAN_POINT ( 'NONE',  ( 5.750341064076999409, -78.19810873382799343, -7.452836517345999390 ) ) ;
#19072 = CARTESIAN_POINT ( 'NONE',  ( 7.764005369688973701, -54.67720632256306601, 9.931049914561711489 ) ) ;
#19071 = CARTESIAN_POINT ( 'NONE',  ( -1.664698873050999950, -84.66679343488898724, -3.596493796894000283 ) ) ;
#19073 = FACE_OUTER_BOUND ( 'NONE', #18874, .T. ) ;
#19074 = CARTESIAN_POINT ( 'NONE',  ( -0.7554284705563540925, -80.81666666666667709, 1.310679582531384391 ) ) ;
#19075 = CARTESIAN_POINT ( 'NONE',  ( -0.1963495408493673433, -81.38541666666669983, 1.499999999999999334 ) ) ;
#19076 = EDGE_CURVE ( 'NONE', #31846, #42112, #8572, .T. ) ;
#19077 = CARTESIAN_POINT ( 'NONE',  ( 0.000000000000000000, -77.19999999999998863, -9.250000000000047962 ) ) ;
#19078 = CARTESIAN_POINT ( 'NONE',  ( 3.250000000000000000, -2.750000000000000000, 0.000000000000000000 ) ) ;
#19079 = AXIS2_PLACEMENT_3D ( 'NONE', #24069, #51831, #20803 ) ;
#19080 = ORIENTED_EDGE ( 'NONE', *, *, #40129, .T. ) ;
#19081 = B_SPLINE_CURVE_WITH_KNOTS ( 'NONE', 3,
 ( #14248, #9839, #139, #18115, #4826, #22825, #45572, #54426 ),
 .UNSPECIFIED., .F., .F.,
 ( 4, 2, 2, 4 ),
 ( 0.000000000000000000, 0.5000000000000026645, 0.7500000000000013323, 1.000000000000000000 ),
 .UNSPECIFIED. ) ;
#19082 = CARTESIAN_POINT ( 'NONE',  ( 11.66950233118999947, -79.43216740133399867, -2.920592611544999606 ) ) ;
#19083 = DIRECTION ( 'NONE',  ( 1.224058188705999773E-08, -0.9999999999999998890, -4.602708956829999399E-10 ) ) ;
#19084 = DIRECTION ( 'NONE',  ( 0.000000000000000000, 1.000000000000000000, 0.000000000000000000 ) ) ;
#19085 = ORIENTED_EDGE ( 'NONE', *, *, #38896, .F. ) ;
#19086 = CARTESIAN_POINT ( 'NONE',  ( 8.130811096204000776, -61.48523690322999613, 9.546858433459998849 ) ) ;
#19087 = ORIENTED_EDGE ( 'NONE', *, *, #40886, .T. ) ;
#19088 = ORIENTED_EDGE ( 'NONE', *, *, #33890, .T. ) ;
#19089 = ORIENTED_EDGE ( 'NONE', *, *, #38573, .F. ) ;
#19090 = CARTESIAN_POINT ( 'NONE',  ( -0.05186576338884000409, -79.81593595582098999, 3.546671651303999973 ) ) ;
#19091 = CARTESIAN_POINT ( 'NONE',  ( 4.000000000000000000, -5.200000000000000178, 0.5999999999999999778 ) ) ;
#19092 = VERTEX_POINT ( 'NONE', #32236 ) ;
#19093 = DIRECTION ( 'NONE',  ( -1.000000000000000000, 0.000000000000000000, 0.000000000000000000 ) ) ;
#19094 = ORIENTED_EDGE ( 'NONE', *, *, #11923, .T. ) ;
#19095 = CARTESIAN_POINT ( 'NONE',  ( 6.436424241555000592, -80.32391735373440156, 8.610165096135999008 ) ) ;
#19096 = CARTESIAN_POINT ( 'NONE',  ( -5.681466576401967394, -78.42513435468593741, -7.867322627890024123 ) ) ;
#19097 = CARTESIAN_POINT ( 'NONE',  ( -2.375990957848951091, -78.85171438276198330, -3.940594315429740480 ) ) ;
#19098 = CARTESIAN_POINT ( 'NONE',  ( 10.42531124908000173, -60.06485148440999922, 7.624341765471999821 ) ) ;
#19099 = CARTESIAN_POINT ( 'NONE',  ( -4.800187936532999800, -76.17640816003999760, 10.10109298474000106 ) ) ;
#19100 = DIRECTION ( 'NONE',  ( 0.000000000000000000, 1.000000000000000000, 0.000000000000000000 ) ) ;
#19101 = EDGE_CURVE ( 'NONE', #25114, #23377, #6491, .T. ) ;
#19102 = AXIS2_PLACEMENT_3D ( 'NONE', #35655, #53685, #13523 ) ;
#19103 = CARTESIAN_POINT ( 'NONE',  ( 7.626500902235000545, -60.11584477251999203, -10.35747158364999976 ) ) ;
#19104 = CARTESIAN_POINT ( 'NONE',  ( 6.577769324041149446, -78.78812245580762408, -6.503367146901806173 ) ) ;
#19105 = CARTESIAN_POINT ( 'NONE',  ( 8.326578794153654428, -76.51178312418663552, 8.289917251876268267 ) ) ;
#19106 = EDGE_CURVE ( 'NONE', #2535, #26886, #17617, .T. ) ;
#19107 = CARTESIAN_POINT ( 'NONE',  ( -9.324187677468000146, -77.05981001420200016, 1.279235053889000051 ) ) ;
#19108 = CARTESIAN_POINT ( 'NONE',  ( 8.485281374238999419, -59.94999999967000548, -8.485281374238999419 ) ) ;
#19109 = CARTESIAN_POINT ( 'NONE',  ( -9.956980069057893346, -80.13546169738316394, -4.683283042152130982 ) ) ;
#19110 = CARTESIAN_POINT ( 'NONE',  ( -5.869402599192000025, -78.36567021304000491, 10.46661899222999992 ) ) ;
#19111 = CARTESIAN_POINT ( 'NONE',  ( -3.703301542149999737, -80.12117549782598758, -1.828677444530000251 ) ) ;
#19112 = AXIS2_PLACEMENT_3D ( 'NONE', #56326, #38012, #10582 ) ;
#19113 = CARTESIAN_POINT ( 'NONE',  ( -12.72397198033999999, -18.77854962937000138, 1.930909771329999858 ) ) ;
#19114 = CARTESIAN_POINT ( 'NONE',  ( -0.4786064949803862101, -83.00633325748620450, 1.154698265544586766 ) ) ;
#19115 = DIRECTION ( 'NONE',  ( 0.000000000000000000, 0.000000000000000000, -1.000000000000000000 ) ) ;
#19116 = B_SPLINE_CURVE_WITH_KNOTS ( 'NONE', 3,
 ( #40095, #48397, #13227, #22685, #17084, #35962 ),
 .UNSPECIFIED., .F., .F.,
 ( 4, 1, 1, 4 ),
 ( 0.000000000000000000, 0.3333333333333000081, 0.6666666666667000474, 1.000000000000000000 ),
 .UNSPECIFIED. ) ;
#19117 = CARTESIAN_POINT ( 'NONE',  ( -0.2132868980366808553, -82.13802635239025562, 1.307894579808998703 ) ) ;
#19118 = LINE ( 'NONE', #37108, #12797 ) ;
#19119 = AXIS2_PLACEMENT_3D ( 'NONE', #11512, #11224, #56092 ) ;
#19120 = ADVANCED_FACE ( 'NONE', ( #24855 ), #669, .F. ) ;
#19121 = CARTESIAN_POINT ( 'NONE',  ( -0.5884528863794137310, -79.75615526183086956, 1.392588485531083942 ) ) ;
#19122 = CARTESIAN_POINT ( 'NONE',  ( 9.722718241315000398, -18.55321828668999729, 7.954951288349001004 ) ) ;
#19123 = DIRECTION ( 'NONE',  ( -0.7071067811865474617, 0.000000000000000000, 0.7071067811865474617 ) ) ;
#19124 = CARTESIAN_POINT ( 'NONE',  ( 12.57434559697999887, -23.71110719500000030, 1.760800161976000089 ) ) ;
#19125 = CARTESIAN_POINT ( 'NONE',  ( -9.733207905157767570, -77.41453182438010572, 4.714720079839265665 ) ) ;
#19126 = FACE_OUTER_BOUND ( 'NONE', #42847, .T. ) ;
#19128 = CARTESIAN_POINT ( 'NONE',  ( 10.94409238583000032, -78.60603169964656445, 0.8311789410725000105 ) ) ;
#19127 = CARTESIAN_POINT ( 'NONE',  ( -1.310679582531386611, -80.04166666666668561, -0.7554284705563495406 ) ) ;
#19129 = CARTESIAN_POINT ( 'NONE',  ( -11.60215227398000160, -76.73358059650999508, 3.298237476086999909 ) ) ;
#19130 = ORIENTED_EDGE ( 'NONE', *, *, #50184, .T. ) ;
#19131 = CARTESIAN_POINT ( 'NONE',  ( -0.7993968753929999727, -83.71682450217399207, -4.052094290298000168 ) ) ;
#19132 = CARTESIAN_POINT ( 'NONE',  ( 2.357318282665999742, -80.85060369710272710, -11.04016127279999893 ) ) ;
#19133 = CARTESIAN_POINT ( 'NONE',  ( -7.655983890242670675, -18.29663439995314178, -10.06694524887581288 ) ) ;
#19134 = CARTESIAN_POINT ( 'NONE',  ( -0.1963495408493605987, -81.61458333333334281, -1.500000000000000444 ) ) ;
#19135 = CARTESIAN_POINT ( 'NONE',  ( -11.21668965365999959, -77.90213061526299043, -0.06311738993059998193 ) ) ;
#19136 = CARTESIAN_POINT ( 'NONE',  ( 12.77649734579999929, -53.49171487479999598, 0.06478328530388999251 ) ) ;
#19137 = CARTESIAN_POINT ( 'NONE',  ( 8.488869829350999652, -79.17888658829198789, 4.102512142575000631 ) ) ;
#19138 = AXIS2_PLACEMENT_3D ( 'NONE', #33552, #51591, #57378 ) ;
#19139 = CARTESIAN_POINT ( 'NONE',  ( -3.282842942682000054, -1.838913946619999962, -1.459606374259000194 ) ) ;
#19140 = CARTESIAN_POINT ( 'NONE',  ( 3.851650068366999857, -78.96264283715740362, 0.000000000000000000 ) ) ;
#19141 = CARTESIAN_POINT ( 'NONE',  ( -4.467577721914089750, -76.11770833332741404, 10.04328771562428813 ) ) ;
#19142 = EDGE_CURVE ( 'NONE', #33872, #41200, #28329, .T. ) ;
#19143 = ORIENTED_EDGE ( 'NONE', *, *, #53135, .T. ) ;
#19144 = CARTESIAN_POINT ( 'NONE',  ( 12.00000000000000000, -77.14999999999999147, 0.000000000000000000 ) ) ;
#19145 = CARTESIAN_POINT ( 'NONE',  ( 1.718598680027600523, -54.55037066937039469, -12.71111582765235148 ) ) ;
#19146 = CARTESIAN_POINT ( 'NONE',  ( -7.504986677982999232, -79.68093998579799120, -5.686679248032999290 ) ) ;
#19147 = FACE_OUTER_BOUND ( 'NONE', #42500, .T. ) ;
#19148 = VERTEX_POINT ( 'NONE', #53165 ) ;
#19149 = CARTESIAN_POINT ( 'NONE',  ( 12.50000000000000000, -60.04999999725999515, -1.750000000000000000 ) ) ;
#19150 = ORIENTED_EDGE ( 'NONE', *, *, #46483, .T. ) ;
#19151 = CARTESIAN_POINT ( 'NONE',  ( 6.544501642745999881, -77.92906724646599059, -10.25436633016999899 ) ) ;
#19152 = CARTESIAN_POINT ( 'NONE',  ( -9.580931538672000869, -77.88704419146098701, 5.608155544205999377 ) ) ;
#19153 = CARTESIAN_POINT ( 'NONE',  ( -1.667917367065999912, -18.71943464842000182, 12.49306764015999960 ) ) ;
#19154 = ORIENTED_EDGE ( 'NONE', *, *, #1578, .F. ) ;
#19155 = EDGE_CURVE ( 'NONE', #57897, #22013, #30993, .T. ) ;
#19156 = VERTEX_POINT ( 'NONE', #48744 ) ;
#19157 = AXIS2_PLACEMENT_3D ( 'NONE', #50358, #42074, #28473 ) ;
#19158 = CARTESIAN_POINT ( 'NONE',  ( -1.067955516321597242, -80.55659099282243574, 0.6499150159960976891 ) ) ;
#19159 = AXIS2_PLACEMENT_3D ( 'NONE', #47410, #7229, #46537 ) ;
#19160 = FILL_AREA_STYLE_COLOUR ( '', #56759 ) ;
#19161 = CARTESIAN_POINT ( 'NONE',  ( 8.249323304235000265, -80.21534508975349809, -5.229696851825000437 ) ) ;
#19162 = VERTEX_POINT ( 'NONE', #4743 ) ;
#19163 = CARTESIAN_POINT ( 'NONE',  ( -10.47145679359999981, -76.08015473334098999, 6.327539751872000018 ) ) ;
#19164 = CARTESIAN_POINT ( 'NONE',  ( 10.35105862822000056, -79.84913938103490239, 3.468557695829999954 ) ) ;
#19165 = ORIENTED_EDGE ( 'NONE', *, *, #23876, .F. ) ;
#19166 = CARTESIAN_POINT ( 'NONE',  ( 5.387243066085122933, -80.76671136794503525, -9.328540033652242158 ) ) ;
#19167 = CARTESIAN_POINT ( 'NONE',  ( 6.214091009702999102, -77.81182694988498838, -7.179311535719000048 ) ) ;
#19168 = DIRECTION ( 'NONE',  ( -1.000000000000000000, 0.000000000000000000, 0.000000000000000000 ) ) ;
#19169 = CARTESIAN_POINT ( 'NONE',  ( 3.911991157192746815, -82.46277140582677134, -0.8315225724521397854 ) ) ;
#19170 = CARTESIAN_POINT ( 'NONE',  ( 1.350260416954781384, -77.89973958345846938, -0.1758964602772491170 ) ) ;
#19171 = CARTESIAN_POINT ( 'NONE',  ( -9.302864017704999711, -76.79717616445388728, -6.266965030820998983 ) ) ;
#19172 = EDGE_CURVE ( 'NONE', #13771, #2820, #347, .T. ) ;
#19173 = CARTESIAN_POINT ( 'NONE',  ( -8.995441680298000620, -77.13613897360269789, 3.759289608065000010 ) ) ;
#19174 = CARTESIAN_POINT ( 'NONE',  ( -0.6085898190276557429, -79.25767112076529486, 1.380970375365989433 ) ) ;
#19175 = CARTESIAN_POINT ( 'NONE',  ( -3.271252402253135294, -80.04895832732434258, 2.391540143840818811 ) ) ;
#19176 = ORIENTED_EDGE ( 'NONE', *, *, #9229, .T. ) ;
#19177 = EDGE_CURVE ( 'NONE', #4309, #43096, #53425, .T. ) ;
#19178 = CARTESIAN_POINT ( 'NONE',  ( 7.568503529865000523, -76.30497314281001309, 9.708412483427999007 ) ) ;
#19179 = AXIS2_PLACEMENT_3D ( 'NONE', #13660, #31655, #39937 ) ;
#19180 = CARTESIAN_POINT ( 'NONE',  ( -1.647983664004335713, -2.263003773417186171, 3.111148793556432146 ) ) ;
#19181 = DIRECTION ( 'NONE',  ( -1.000000000000000000, 0.000000000000000000, 0.000000000000000000 ) ) ;
#19182 = CARTESIAN_POINT ( 'NONE',  ( 12.16303714866999997, -79.27753849292000154, 1.568404430622000190 ) ) ;
#19183 = CARTESIAN_POINT ( 'NONE',  ( 12.24159337356999977, -76.30973022145700213, -0.9828625608234000666 ) ) ;
#19184 = CARTESIAN_POINT ( 'NONE',  ( -3.620209227049993039, -85.94828561723799965, 1.611820994701015364 ) ) ;
#19185 = CARTESIAN_POINT ( 'NONE',  ( 2.620693402520182236, -2.799838841147761936, -1.925851656741417228 ) ) ;
#19186 = CARTESIAN_POINT ( 'NONE',  ( -4.143196849663613790, -77.64733255783154675, -11.57321364922782969 ) ) ;
#19187 = CARTESIAN_POINT ( 'NONE',  ( -9.723199429427999974, -17.52306056076000118, 7.958735708429999889 ) ) ;
#19188 = TOROIDAL_SURFACE ( 'NONE', #13520, 26.50000000000000000, 14.00000000000000000 ) ;
#19189 = B_SPLINE_SURFACE_WITH_KNOTS ( 'NONE', 3, 3, ( 
 ( #38749, #11896, #16035, #48214 ),
 ( #38167, #11613, #47643, #33735 ),
 ( #2748, #25749, #34019, #51773 ),
 ( #26028, #52056, #43772, #20750 ),
 ( #30457, #15738, #57336, #6878 ),
 ( #52340, #38461, #39328, #34597 ),
 ( #11322, #29301, #29874, #47350 ),
 ( #25172, #7461, #56478, #24888 ) ),
 .UNSPECIFIED., .F., .F., .F.,
 ( 4, 1, 1, 1, 1, 4 ),
 ( 4, 4 ),
 ( -0.01200407345747999885, 0.000000000000000000, 0.3333333333333000081, 0.6666666666667000474, 1.000000000000000000, 1.011997855551999947 ),
 ( -0.3559705542741000150, 1.355970554273999928 ),
 .UNSPECIFIED. ) ;
#19190 = ADVANCED_FACE ( 'NONE', ( #9172 ), #12985, .F. ) ;
#19191 = ORIENTED_EDGE ( 'NONE', *, *, #42988, .F. ) ;
#19192 = CARTESIAN_POINT ( 'NONE',  ( -1.186490757027999887, -81.53774735892999104, -0.2694786029208000033 ) ) ;
#19193 = CARTESIAN_POINT ( 'NONE',  ( 7.705600964031999567, -77.19390341397898680, 5.723878957493999664 ) ) ;
#19194 = CARTESIAN_POINT ( 'NONE',  ( 8.792818914773597783, -25.22696626442860790, 9.175540344814811178 ) ) ;
#19195 = DIRECTION ( 'NONE',  ( 0.000000000000000000, 0.000000000000000000, -1.000000000000000000 ) ) ;
#19196 = CARTESIAN_POINT ( 'NONE',  ( -2.640046357426999890, -2.819378508794999849, 2.612394753782000034 ) ) ;
#19197 = CIRCLE ( 'NONE', #2231, 14.00000000000000000 ) ;
#19198 = CARTESIAN_POINT ( 'NONE',  ( 12.02223179210000126, -78.76423986341698935, 0.8134715296432000198 ) ) ;
#19199 = CARTESIAN_POINT ( 'NONE',  ( 5.053427186728000287, -78.53798106301098869, 8.198541555267000902 ) ) ;
#19200 = CARTESIAN_POINT ( 'NONE',  ( 0.09944289326072909552, -76.07403084298707086, 11.74944078188181429 ) ) ;
#19201 = CARTESIAN_POINT ( 'NONE',  ( -0.6142531002814000107, -82.99257374592500014, 1.203711489715000305 ) ) ;
#19202 = CARTESIAN_POINT ( 'NONE',  ( 3.106054555984665289, -86.10000000000019327, -1.382904586457952556 ) ) ;
#19203 = ORIENTED_EDGE ( 'NONE', *, *, #17570, .T. ) ;
#19204 = AXIS2_PLACEMENT_3D ( 'NONE', #46096, #41646, #41358 ) ;
#19205 = DIRECTION ( 'NONE',  ( 0.000000000000000000, -1.000000000000000000, 0.000000000000000000 ) ) ;
#19206 = CARTESIAN_POINT ( 'NONE',  ( 10.83169831117340642, -79.04172495591551240, -4.820018971670366525 ) ) ;
#19207 = CARTESIAN_POINT ( 'NONE',  ( -1.276771495430000038E-14, -69.50420297070000686, 0.000000000000000000 ) ) ;
#19208 = CARTESIAN_POINT ( 'NONE',  ( 6.718030245586000149, -79.16787185144298178, -8.679405866825000260 ) ) ;
#19209 = CARTESIAN_POINT ( 'NONE',  ( -6.633107506946999798, -76.45391306960999600, -10.59980473414000102 ) ) ;
#19210 = DIRECTION ( 'NONE',  ( 0.7071067811865474617, 0.000000000000000000, 0.7071067811865474617 ) ) ;
#19211 = CARTESIAN_POINT ( 'NONE',  ( 9.310166272083998606, -16.86468533975999762, -8.596757084891999412 ) ) ;
#19212 = DIRECTION ( 'NONE',  ( 0.000000000000000000, -1.000000000000000000, 0.000000000000000000 ) ) ;
#19213 = ORIENTED_EDGE ( 'NONE', *, *, #34452, .T. ) ;
#19214 = CARTESIAN_POINT ( 'NONE',  ( -10.80063122475000092, -78.79944879618999209, -3.190662894339999944 ) ) ;
#19215 = CARTESIAN_POINT ( 'NONE',  ( 12.70455814335207378, -17.43992875976934798, 1.489882837238664770 ) ) ;
#19216 = CARTESIAN_POINT ( 'NONE',  ( -11.75721612854724363, -79.54603331170258684, 0.5654014867660701604 ) ) ;
#19217 = CARTESIAN_POINT ( 'NONE',  ( -0.03487126055828242838, -78.39678895079168797, 3.699835671046090901 ) ) ;
#19218 = CARTESIAN_POINT ( 'NONE',  ( -2.383965290753023769, -77.84388370242140809, 11.78518095179793512 ) ) ;
#19219 = CARTESIAN_POINT ( 'NONE',  ( -0.8865732340429423042, -81.53829647950151127, 0.8807237917444714626 ) ) ;
#19220 = DIRECTION ( 'NONE',  ( 0.000000000000000000, 0.000000000000000000, -1.000000000000000000 ) ) ;
#19221 = CARTESIAN_POINT ( 'NONE',  ( 3.665025684363000025, -3.476287900391999752, -1.025097465345000236 ) ) ;
#19222 = EDGE_CURVE ( 'NONE', #18472, #15737, #18256, .T. ) ;
#19223 = CARTESIAN_POINT ( 'NONE',  ( 1.249381860769000152, -78.80611706015999118, -0.3870755167071000535 ) ) ;
#19224 = CARTESIAN_POINT ( 'NONE',  ( 11.00000000000000000, -77.94999999999998863, 0.000000000000000000 ) ) ;
#19225 = CARTESIAN_POINT ( 'NONE',  ( 10.87605760524872345, -79.68936634149505949, -1.476207922926128457 ) ) ;
#19226 = AXIS2_PLACEMENT_3D ( 'NONE', #57340, #52916, #26034 ) ;
#19227 = DIRECTION ( 'NONE',  ( 0.000000000000000000, 1.000000000000000000, 0.000000000000000000 ) ) ;
#19228 = ORIENTED_EDGE ( 'NONE', *, *, #20290, .F. ) ;
#19229 = VERTEX_POINT ( 'NONE', #24129 ) ;
#19230 = CARTESIAN_POINT ( 'NONE',  ( -7.541360678298866027, -77.84749999999998238, 5.846326858574209417 ) ) ;
#19231 = CARTESIAN_POINT ( 'NONE',  ( 6.075412649139570576, -78.77296812514245516, -8.868588324655249266 ) ) ;
#19232 = ORIENTED_EDGE ( 'NONE', *, *, #54587, .T. ) ;
#19233 = CARTESIAN_POINT ( 'NONE',  ( 7.995633008690000487, -76.56161320104568802, 7.819446035993999899 ) ) ;
#19234 = CARTESIAN_POINT ( 'NONE',  ( 2.277009439587376338, -82.65052084978994174, 2.539082304559017178 ) ) ;
#19235 = CARTESIAN_POINT ( 'NONE',  ( -0.3926218265389256890, -80.29583333333334849, 1.460959015002472050 ) ) ;
#19236 = CARTESIAN_POINT ( 'NONE',  ( 7.631889049370999878, -60.02121504819000108, 10.36222434951000082 ) ) ;
#19237 = DIRECTION ( 'NONE',  ( 1.000000000000000000, 0.000000000000000000, 0.000000000000000000 ) ) ;
#19238 = CARTESIAN_POINT ( 'NONE',  ( 0.4844351086939314155, -77.42168479355439104, 11.97018437499462351 ) ) ;
#19239 = CARTESIAN_POINT ( 'NONE',  ( 6.879576957522999692, -79.08856369595298474, 8.859431780707000215 ) ) ;
#19240 = ORIENTED_EDGE ( 'NONE', *, *, #30139, .T. ) ;
#19241 = DIRECTION ( 'NONE',  ( 0.9999999930530777403, 0.000000000000000000, 0.0001178721535675973718 ) ) ;
#19242 = ORIENTED_EDGE ( 'NONE', *, *, #55070, .T. ) ;
#19243 = EDGE_CURVE ( 'NONE', #11038, #43183, #7255, .T. ) ;
#19244 = CARTESIAN_POINT ( 'NONE',  ( 8.964791593824459781, -77.37004751899343091, 2.291628598551814999 ) ) ;
#19245 = CARTESIAN_POINT ( 'NONE',  ( 3.792698199283999649, -78.14336073446899888, -10.36819406884000117 ) ) ;
#19246 = DIRECTION ( 'NONE',  ( 0.000000000000000000, 1.000000000000000000, 0.000000000000000000 ) ) ;
#19247 = CARTESIAN_POINT ( 'NONE',  ( 7.256139241522999939, -77.69823973248199422, 6.443535727668999513 ) ) ;
#19248 = CARTESIAN_POINT ( 'NONE',  ( -8.251806177691921818, -17.19944067082638739, 9.431051272834954702 ) ) ;
#19249 = CYLINDRICAL_SURFACE ( 'NONE', #24701, 1.500000000000000000 ) ;
#19250 = CARTESIAN_POINT ( 'NONE',  ( 1.621809933883000099, -78.52703137313999093, 0.1356303529659999840 ) ) ;
#19251 = CARTESIAN_POINT ( 'NONE',  ( 2.484010139066000100, -79.24607046129089838, -3.352049501643000085 ) ) ;
#19252 = CARTESIAN_POINT ( 'NONE',  ( -0.9111626473548137817, -79.16027324500811346, -0.8557194560358774016 ) ) ;
#19253 = CARTESIAN_POINT ( 'NONE',  ( 10.94008345411999983, -78.17955615878399556, 0.05084573220516999670 ) ) ;
#19254 = CARTESIAN_POINT ( 'NONE',  ( -8.188293269161999177, -24.70494400568999893, -9.395718629078000816 ) ) ;
#19255 = CIRCLE ( 'NONE', #52255, 1.750000000000001332 ) ;
#19256 = CARTESIAN_POINT ( 'NONE',  ( 12.92177931909999877, -57.04263462147999775, -2.062503053667999797 ) ) ;
#19257 = EDGE_CURVE ( 'NONE', #55023, #30580, #41737, .T. ) ;
#19258 = CARTESIAN_POINT ( 'NONE',  ( 3.546564817179000073, -82.45880512652999528, -0.05579705918139000326 ) ) ;
#19259 = ORIENTED_EDGE ( 'NONE', *, *, #39730, .T. ) ;
#19260 = B_SPLINE_CURVE_WITH_KNOTS ( 'NONE', 3,
 ( #22437, #12702, #52868, #14375, #45997, #30698, #40452, #39854, #30412, #5523, #53441, #48733, #17423, #8276, #23531, #9967, #44, #18824, #39572, #25986, #34838, #12423, #12983, #48447, #7988, #3563, #3848, #26279, #57870, #11429, #38275, #55715, #15558, #1126, #15263, #23822, #19405, #19114, #15848, #19997, #20281, #24118, #55121, #51874, #37696, #29409, #28826, #50715, #28536, #10256, #11147, #37105, #42136, #33837, #2285, #37983, #37397, #33255, #29122, #51004, #47462, #56007, #10853, #1703, #19697, #46584, #51297, #46875, #6986, #47168, #46289, #6699, #24708, #24419, #6110, #42433, #42720, #56295, #6402, #2002, #33550, #14665, #41544, #51589, #55414, #32662, #10553, #28238, #5816, #41840, #1415, #14962, #32959, #25565, #57153, #56873, #43585, #7852, #16718, #3148, #30565, #17004 ),
 .UNSPECIFIED., .F., .F.,
 ( 4, 2, 2, 2, 1, 1, 1, 2, 2, 2, 2, 2, 1, 1, 1, 2, 2, 2, 2, 2, 1, 1, 1, 2, 2, 2, 2, 2, 2, 2, 2, 1, 2, 2, 2, 2, 1, 1, 2, 2, 2, 2, 2, 2, 2, 2, 2, 1, 2, 2, 2, 2, 1, 1, 1, 2, 2, 2, 4 ),
 ( 0.000000000000000000, 0.06250000000008198997, 0.09375000000012330414, 0.1093750000001438710, 0.1171875000001541683, 0.1210937500001593031, 0.1230468750001619399, 0.1240234375001631334, 0.1250000000001643130, 0.1875000000002498834, 0.2187500000002923772, 0.2343750000003131384, 0.2421875000003240463, 0.2460937500003289036, 0.2480468750003312906, 0.2490234375003324285, 0.2500000000003335665, 0.3125000000004117262, 0.3437500000004511391, 0.3593750000004708456, 0.3671875000004808376, 0.3710937500004856116, 0.3730468750004848344, 0.3740234375004842238, 0.3750000000004836131, 0.4375000000004443668, 0.4687500000004250489, 0.5000000000004057865, 0.5312500000003864686, 0.5468750000003772538, 0.5546875000003725908, 0.5585937500003702594, 0.5605468750003689271, 0.5625000000003675948, 0.5937500000003431699, 0.6093750000003311795, 0.6171875000003249623, 0.6210937500003218537, 0.6230468750003202993, 0.6250000000003187450, 0.6875000000002745582, 0.7187500000002521316, 0.7343750000002409184, 0.7421875000002361444, 0.7500000000002312595, 0.7812500000002134959, 0.7968750000002042810, 0.8046875000001999512, 0.8085937500001977307, 0.8125000000001955103, 0.8437500000001791900, 0.8593750000001713074, 0.8671875000001671996, 0.8710937500001649791, 0.8730468750001639799, 0.8740234375001629807, 0.8750000000001620926, 0.9375000000000810463, 1.000000000000000000 ),
 .UNSPECIFIED. ) ;
#19261 = CARTESIAN_POINT ( 'NONE',  ( -10.48543666025109289, -79.44166666666666288, -6.043427764450796325 ) ) ;
#19262 = CARTESIAN_POINT ( 'NONE',  ( -1.605277969432999940, -80.85709877522999989, -0.5682425234610001263 ) ) ;
#19263 = CARTESIAN_POINT ( 'NONE',  ( 4.370542281221782233, -77.94187509226848931, 9.823968797400164377 ) ) ;
#19264 = EDGE_CURVE ( 'NONE', #44340, #26124, #48719, .T. ) ;
#19265 = CARTESIAN_POINT ( 'NONE',  ( 4.458743082292000004, -77.47854620581199470, 11.11915799896999957 ) ) ;
#19266 = CARTESIAN_POINT ( 'NONE',  ( -9.783235115942000348, -17.46434390394999880, 7.961033122320000821 ) ) ;
#19267 = DIRECTION ( 'NONE',  ( 1.000000000000000000, 0.000000000000000000, 0.000000000000000000 ) ) ;
#19268 = CARTESIAN_POINT ( 'NONE',  ( 1.007525990681730432, -3.101944840528865655, 3.373179531834999079 ) ) ;
#19269 = CARTESIAN_POINT ( 'NONE',  ( 2.210712544800999879, -79.33340584965399955, -9.468498208576999531 ) ) ;
#19270 = CARTESIAN_POINT ( 'NONE',  ( 5.750341064076999409, -77.75648151147798615, -7.452836517345999390 ) ) ;
#19271 = CARTESIAN_POINT ( 'NONE',  ( -3.184161977317994108, -85.88547957940599531, 1.417680250971013356 ) ) ;
#19272 = CARTESIAN_POINT ( 'NONE',  ( -9.889498855898999352, -78.42232914858598747, 4.888716273084000363 ) ) ;
#19273 = CARTESIAN_POINT ( 'NONE',  ( -7.650089724727000551, -76.72148282161819566, -9.607224057717001386 ) ) ;
#19274 = CARTESIAN_POINT ( 'NONE',  ( 9.770225111710999499, -80.60124745865709883, -5.353494744805000316 ) ) ;
#19275 = VERTEX_POINT ( 'NONE', #41460 ) ;
#19276 = AXIS2_PLACEMENT_3D ( 'NONE', #51900, #48622, #16169 ) ;
#19277 = CARTESIAN_POINT ( 'NONE',  ( -4.299999999593000055, -81.99999999959300112, -2.324862195016999523E-09 ) ) ;
#19278 = DIRECTION ( 'NONE',  ( -0.9999999999995751176, 0.000000000000000000, -9.217549100139771309E-07 ) ) ;
#19279 = CARTESIAN_POINT ( 'NONE',  ( -9.302864017704999711, -76.74549295037100194, -6.266965030821000759 ) ) ;
#19280 = CARTESIAN_POINT ( 'NONE',  ( 7.218984044805000444, -79.12742484609498206, 8.267423174273998754 ) ) ;
#19281 = CARTESIAN_POINT ( 'NONE',  ( 9.317978910659999059, -25.13238463018999980, -8.588869595444998950 ) ) ;
#19282 = CARTESIAN_POINT ( 'NONE',  ( -0.9444306527324454192, -82.88177081832023418, 3.899503811090379024 ) ) ;
#19283 = AXIS2_PLACEMENT_3D ( 'NONE', #29600, #20190, #20759 ) ;
#19284 = CARTESIAN_POINT ( 'NONE',  ( -2.717027075192881114, -78.60471625112383265, -10.43420719071179548 ) ) ;
#19285 = CARTESIAN_POINT ( 'NONE',  ( -1.250000000000000000, -81.09999999999999432, 0.000000000000000000 ) ) ;
#19286 = CARTESIAN_POINT ( 'NONE',  ( 3.029657250468000385, -83.75644503318798684, -2.869013636082000218 ) ) ;
#19287 = EDGE_CURVE ( 'NONE', #13102, #15626, #28450, .T. ) ;
#19288 = CARTESIAN_POINT ( 'NONE',  ( 0.7554284705563453217, -80.33333333333332860, 1.310679582531389276 ) ) ;
#19289 = CARTESIAN_POINT ( 'NONE',  ( 10.00831378476999944, -55.42769332259999260, -7.646786280026000249 ) ) ;
#19290 = CARTESIAN_POINT ( 'NONE',  ( 0.000000000000000000, -13.07071424677999971, 0.000000000000000000 ) ) ;
#19291 = CARTESIAN_POINT ( 'NONE',  ( 0.6544915521845998674, -81.17247804586000370, 1.531959166345999934 ) ) ;
#19292 = DIRECTION ( 'NONE',  ( 0.000000000000000000, 1.000000000000000000, 0.000000000000000000 ) ) ;
#19293 = CARTESIAN_POINT ( 'NONE',  ( 3.140974612311327796, -77.65416666666665435, 11.68767212001979594 ) ) ;
#19294 = CARTESIAN_POINT ( 'NONE',  ( -1.501968397107060316, -81.74187130586206251, 0.1553300411971603456 ) ) ;
#19295 = CARTESIAN_POINT ( 'NONE',  ( -12.43640309388999832, -61.71747517570000241, -0.05224034426411999776 ) ) ;
#19296 = CARTESIAN_POINT ( 'NONE',  ( -5.969148455088877370, -80.17823147499480285, -8.940398062078001473 ) ) ;
#19297 = CARTESIAN_POINT ( 'NONE',  ( -2.486604901413152824, -77.90416666666666856, -9.252740428349003565 ) ) ;
#19298 = EDGE_CURVE ( 'NONE', #42334, #49068, #35316, .T. ) ;
#19299 = CARTESIAN_POINT ( 'NONE',  ( -1.500000000000000222, -77.91041666666667709, -0.1963495408493622363 ) ) ;
#19300 = ORIENTED_EDGE ( 'NONE', *, *, #2135, .T. ) ;
#19301 = EDGE_CURVE ( 'NONE', #18636, #425, #8206, .T. ) ;
#19302 = CARTESIAN_POINT ( 'NONE',  ( 13.95956770371999944, -45.71924237694000226, 5.182383547123999630E-05 ) ) ;
#19303 = B_SPLINE_CURVE_WITH_KNOTS ( 'NONE', 3,
 ( #7080, #2375, #56958, #16519 ),
 .UNSPECIFIED., .F., .F.,
 ( 4, 4 ),
 ( 0.000000000000000000, 1.000000000000000000 ),
 .UNSPECIFIED. ) ;
#19304 = CARTESIAN_POINT ( 'NONE',  ( -11.13008859988999966, -78.88675832436199187, 0.6129668257943999832 ) ) ;
#19305 = AXIS2_PLACEMENT_3D ( 'NONE', #29192, #10926, #28906 ) ;
#19306 = CARTESIAN_POINT ( 'NONE',  ( 0.000000000000000000, -80.74999999950000529, -2.949999999500999781 ) ) ;
#19307 = EDGE_LOOP ( 'NONE', ( #35887, #37511, #18501, #49076, #12389, #10979, #24083, #12719, #46790, #44856 ) ) ;
#19308 = VERTEX_POINT ( 'NONE', #2696 ) ;
#19309 = CARTESIAN_POINT ( 'NONE',  ( -1.253545579602000082, -82.06400559251599702, 0.6623148383621999535 ) ) ;
#19310 = ORIENTED_EDGE ( 'NONE', *, *, #32952, .T. ) ;
#19311 = ORIENTED_EDGE ( 'NONE', *, *, #35614, .T. ) ;
#19312 = CARTESIAN_POINT ( 'NONE',  ( -1.310679582531389498, -81.95833333334499571, 0.7554284705563444335 ) ) ;
#19313 = CARTESIAN_POINT ( 'NONE',  ( -1.287598599762399321, -77.77604166675226338, -0.7431007365616121296 ) ) ;
#19314 = CARTESIAN_POINT ( 'NONE',  ( 0.000000000000000000, 0.000000000000000000, 0.000000000000000000 ) ) ;
#19315 = CARTESIAN_POINT ( 'NONE',  ( 1.769645564550136996, -80.70416665604813033, -2.954788210828755091 ) ) ;
#19316 = AXIS2_PLACEMENT_3D ( 'NONE', #31101, #49442, #45604 ) ;
#19317 = CARTESIAN_POINT ( 'NONE',  ( 1.852771442128949175, -78.24118117197441791, -9.062483227336022296 ) ) ;
#19318 = CARTESIAN_POINT ( 'NONE',  ( -9.500000000000000000, -77.89999999999999147, 0.000000000000000000 ) ) ;
#19319 = VERTEX_POINT ( 'NONE', #28742 ) ;
#19320 = ORIENTED_EDGE ( 'NONE', *, *, #42418, .T. ) ;
#19321 = CARTESIAN_POINT ( 'NONE',  ( -7.746552609361182284, -77.55398491059833077, 5.056132427002594909 ) ) ;
#19322 = DIRECTION ( 'NONE',  ( 0.000000000000000000, -1.000000000000000000, 0.000000000000000000 ) ) ;
#19323 = CARTESIAN_POINT ( 'NONE',  ( -1.250000000000001332, -81.48958333333334281, 0.1636246173744632659 ) ) ;
#19324 = DIRECTION ( 'NONE',  ( 0.6489586447325770280, -0.04890182339238829945, 0.7592504784955730335 ) ) ;
#19325 = CARTESIAN_POINT ( 'NONE',  ( -4.814859605045999302, -78.68616321717099993, 8.425427962446999430 ) ) ;
#19327 = CIRCLE ( 'NONE', #54714, 12.05000000000000071 ) ;
#19326 = CARTESIAN_POINT ( 'NONE',  ( -7.601397897754999633, -60.04999999657000131, -10.07627163191000008 ) ) ;
#19328 = CARTESIAN_POINT ( 'NONE',  ( -10.42274798266999980, -20.24634220924000161, 7.691916945430000041 ) ) ;
#19329 = CARTESIAN_POINT ( 'NONE',  ( 12.00000000000000000, -76.64999999999999147, 0.000000000000000000 ) ) ;
#19330 = CARTESIAN_POINT ( 'NONE',  ( 0.2122939316688999822, -79.21759604279999678, -1.334248387208000208 ) ) ;
#19331 = DIRECTION ( 'NONE',  ( 0.7071067811865475727, 0.000000000000000000, 0.7071067811865475727 ) ) ;
#19332 = CARTESIAN_POINT ( 'NONE',  ( -2.386348275546000153, -80.48624039569099864, -3.425631633863999603 ) ) ;
#19333 = CARTESIAN_POINT ( 'NONE',  ( 8.440675369999999234, -80.00371287089478756, 7.053722371789000967 ) ) ;
#19334 = CARTESIAN_POINT ( 'NONE',  ( -3.327183877592000183, -78.47356001420199334, 9.097860994781999722 ) ) ;
#19335 = CARTESIAN_POINT ( 'NONE',  ( 11.68767212001978173, -77.17083333333333428, 3.140974612311388192 ) ) ;
#19336 = CARTESIAN_POINT ( 'NONE',  ( 1.378124299131000097, -80.68907046129099569, -3.268841696656000106 ) ) ;
#19338 = CARTESIAN_POINT ( 'NONE',  ( 1.224162466603000210, -77.93941928053710910, -0.5291525010897000225 ) ) ;
#19337 = FACE_OUTER_BOUND ( 'NONE', #5214, .T. ) ;
#19339 = CARTESIAN_POINT ( 'NONE',  ( 0.6056868765398906174, -79.46999359693003839, 9.249787030607762972 ) ) ;
#19340 = CARTESIAN_POINT ( 'NONE',  ( -1.750000000001000089, -23.25000000990999993, -12.56594317857000043 ) ) ;
#19341 = CARTESIAN_POINT ( 'NONE',  ( 2.234646451474000095, -2.642397890054000165, 3.080979982494000069 ) ) ;
#19342 = LINE ( 'NONE', #41774, #45959 ) ;
#19343 = B_SPLINE_CURVE_WITH_KNOTS ( 'NONE', 3,
 ( #49072, #26329, #13628, #49668, #35467, #48785 ),
 .UNSPECIFIED., .F., .F.,
 ( 4, 1, 1, 4 ),
 ( 0.000000000000000000, 0.3333333333333000081, 0.6666666666667000474, 1.000000000000000000 ),
 .UNSPECIFIED. ) ;
#19344 = ORIENTED_EDGE ( 'NONE', *, *, #55333, .F. ) ;
#19345 = CARTESIAN_POINT ( 'NONE',  ( -2.460865576472458738, -3.500000000000000000, -2.303415178628417603 ) ) ;
#19346 = CARTESIAN_POINT ( 'NONE',  ( 7.353725627631179762, -60.10655143787244015, -8.180687091746213113 ) ) ;
#19347 = CARTESIAN_POINT ( 'NONE',  ( 3.250000000000000000, -2.850000000000000089, 0.000000000000000000 ) ) ;
#19348 = CIRCLE ( 'NONE', #43838, 3.600000000000000089 ) ;
#19349 = CARTESIAN_POINT ( 'NONE',  ( 1.931043742978000077, -59.57795407677000554, 12.75763395697999947 ) ) ;
#19350 = CARTESIAN_POINT ( 'NONE',  ( -12.66315144082999922, -53.62197088156000291, -0.06064144874946000158 ) ) ;
#19351 = CARTESIAN_POINT ( 'NONE',  ( 10.66182291595043452, -79.36152322765421729, 1.544088080186965195 ) ) ;
#19352 = EDGE_CURVE ( 'NONE', #53710, #7256, #23740, .T. ) ;
#19353 = CARTESIAN_POINT ( 'NONE',  ( 5.793497013506000215, -79.61881332859898919, -7.828108358733000038 ) ) ;
#19354 = DIRECTION ( 'NONE',  ( 0.7071067811865474617, 3.445410891336226740E-11, 0.7071067811865474617 ) ) ;
#19355 = EDGE_CURVE ( 'NONE', #32332, #26523, #46674, .T. ) ;
#19356 = CARTESIAN_POINT ( 'NONE',  ( 3.952028055797999873, -77.52568593946898545, 10.55876001981000023 ) ) ;
#19357 = CARTESIAN_POINT ( 'NONE',  ( 0.000000000000000000, -0.2000000000000005107, -13.99999999999696954 ) ) ;
#19358 = CARTESIAN_POINT ( 'NONE',  ( 12.00000000000000000, -18.75000000000000000, 1.750000000000000000 ) ) ;
#19359 = FACE_OUTER_BOUND ( 'NONE', #45155, .T. ) ;
#19361 = CARTESIAN_POINT ( 'NONE',  ( -3.858199361241999803, -0.8744335234539000190, -1.117275487237999965 ) ) ;
#19360 = CARTESIAN_POINT ( 'NONE',  ( 2.727633873738000148, -83.46428928222098875, -2.582902200820999639 ) ) ;
#19362 = CARTESIAN_POINT ( 'NONE',  ( -6.053394164830000257, -79.64034805011499429, -7.392643757108000813 ) ) ;
#19363 = CARTESIAN_POINT ( 'NONE',  ( -1.460959015002474493, -80.87916666666667709, 0.3926218265389144757 ) ) ;
#19364 = CARTESIAN_POINT ( 'NONE',  ( -0.5412065714428999641, -79.74942042488599725, -1.203187872875000064 ) ) ;
#19365 = CARTESIAN_POINT ( 'NONE',  ( -6.990209140086781403, -77.16870983874881063, -8.167017623392847980 ) ) ;
#19366 = DIRECTION ( 'NONE',  ( -0.7071067811864970576, -0.7071067811865969777, -3.680441358138984842E-08 ) ) ;
#19367 = ORIENTED_EDGE ( 'NONE', *, *, #39188, .T. ) ;
#19369 = ADVANCED_FACE ( 'NONE', ( #14006 ), #32003, .T. ) ;
#19368 = VERTEX_POINT ( 'NONE', #45619 ) ;
#19370 = CARTESIAN_POINT ( 'NONE',  ( 3.552363299575000077, -79.78274967992298627, -11.49294985030999960 ) ) ;
#19371 = CARTESIAN_POINT ( 'NONE',  ( -12.50657368826013993, -61.77245458960371138, -0.3553454088953992285 ) ) ;
#19372 = CARTESIAN_POINT ( 'NONE',  ( 9.199999999999999289, -77.00000000000000000, 0.000000000000000000 ) ) ;
#19373 = ORIENTED_EDGE ( 'NONE', *, *, #51295, .T. ) ;
#19374 = CARTESIAN_POINT ( 'NONE',  ( -11.01904509677000021, -78.09203558730200712, 4.584337204197000304 ) ) ;
#19375 = ORIENTED_EDGE ( 'NONE', *, *, #34608, .F. ) ;
#19376 = B_SPLINE_SURFACE_WITH_KNOTS ( 'NONE', 3, 3, ( 
 ( #15993, #1271, #42865, #19546, #47020, #37254, #37544, #24850, #20141, #38420, #19262, #55561, #37841, #33981, #46435, #19847, #15412, #32811, #2423, #1555, #33405, #47310, #2139, #10403, #52018, #15700, #29262, #10995, #51443, #6550, #28978, #56151, #24559, #28388, #42576 ),
 ( #55266, #33694, #11572, #23967, #6839, #51733, #14814, #29552, #47607, #23680, #5964, #41986, #33107, #25709, #57874, #17431, #3288, #35416, #52874, #16572, #39001, #56731, #25992, #52304, #25424, #16862, #39288, #25132, #43736, #48176, #57010, #21281, #39577, #16290, #52589 ),
 ( #53446, #29837, #12139, #57300, #34269, #8282, #43439, #30127, #30702, #44016, #11860, #26284, #57580, #53160, #12427, #34843, #48452, #30420, #3568, #7995, #47889, #7708, #12709, #12990, #30987, #3853, #38710, #21572, #7420, #7131, #2999, #20996, #43157, #39860, #34557 ),
 ( #17142, #2714, #20711, #35128, #48738, #44298, #21851, #36017, #58167, #18615, #44592, #31574, #23326, #9750, #49026, #27446, #44891, #17733, #49, #36892, #49621, #26863, #35720, #36604, #9168, #4442, #917, #41044, #27736, #54044, #8869, #54627, #14164, #18025, #31278 ) ),
 .UNSPECIFIED., .F., .F., .F.,
 ( 4, 4 ),
 ( 4, 1, 1, 1, 1, 1, 1, 1, 1, 1, 1, 1, 1, 1, 1, 1, 1, 1, 1, 1, 1, 1, 1, 1, 1, 1, 1, 1, 1, 1, 1, 1, 4 ),
 ( -0.1331668876848000060, 1.133166887685000068 ),
 ( -0.02000000000000000042, 0.01250000000000000069, 0.04499999999999999833, 0.07749999999999999944, 0.1100000000000000006, 0.1424999999999999878, 0.1749999999999999889, 0.2074999999999999900, 0.2399999999999999911, 0.2725000000000000200, 0.3049999999999999933, 0.3375000000000000222, 0.3699999999999999956, 0.4025000000000000244, 0.4349999999999999978, 0.4675000000000000266, 0.5000000000000000000, 0.5324999999999999734, 0.5649999999999999467, 0.5975000000000000311, 0.6300000000000000044, 0.6624999999999999778, 0.6949999999999999512, 0.7275000000000000355, 0.7600000000000000089, 0.7924999999999999822, 0.8249999999999999556, 0.8575000000000000400, 0.8900000000000000133, 0.9224999999999999867, 0.9549999999999999600, 0.9875000000000000444, 1.020000000000000018 ),
 .UNSPECIFIED. ) ;
#19377 = ORIENTED_EDGE ( 'NONE', *, *, #19287, .F. ) ;
#19378 = EDGE_CURVE ( 'NONE', #34134, #13032, #41167, .T. ) ;
#19379 = ORIENTED_EDGE ( 'NONE', *, *, #56141, .F. ) ;
#19380 = CARTESIAN_POINT ( 'NONE',  ( -2.027483865207000413, -80.41718807822699944, -2.910477459209999562 ) ) ;
#19381 = CARTESIAN_POINT ( 'NONE',  ( -9.312499999988999022, -77.13750000001088836, -2.050180145195999796E-09 ) ) ;
#19382 = ADVANCED_FACE ( 'NONE', ( #54748 ), #45964, .T. ) ;
#19383 = CIRCLE ( 'NONE', #10922, 5.000000000000000888 ) ;
#19384 = ORIENTED_EDGE ( 'NONE', *, *, #48516, .F. ) ;
#19385 = CARTESIAN_POINT ( 'NONE',  ( 1.231359744498104147, -82.83660106426310676, -0.2141053253869658335 ) ) ;
#19386 = CARTESIAN_POINT ( 'NONE',  ( -7.705142895592000052, -58.55083378327000077, 10.24998526315000014 ) ) ;
#19387 = ORIENTED_EDGE ( 'NONE', *, *, #5120, .T. ) ;
#19388 = DIRECTION ( 'NONE',  ( 0.7071067811865470176, -0.7071067811865470176, 3.647649194621239524E-08 ) ) ;
#19389 = CARTESIAN_POINT ( 'NONE',  ( -0.5296483783707884863, -79.34647407982620848, -1.412499042453858600 ) ) ;
#19390 = LINE ( 'NONE', #46275, #11437 ) ;
#19391 = DIRECTION ( 'NONE',  ( -1.000000000000000000, 0.000000000000000000, 0.000000000000000000 ) ) ;
#19392 = CARTESIAN_POINT ( 'NONE',  ( 8.898653440358000211, -78.46734835141977271, -3.871004561473999850 ) ) ;
#19393 = CARTESIAN_POINT ( 'NONE',  ( 5.380788203752000065, -76.03337378079599773, 9.804131929786001010 ) ) ;
#19394 = DIRECTION ( 'NONE',  ( 0.000000000000000000, 0.000000000000000000, -1.000000000000000000 ) ) ;
#19395 = CARTESIAN_POINT ( 'NONE',  ( -7.705142895613999343, -57.04916621739000249, -10.24998526317999925 ) ) ;
#19396 = CARTESIAN_POINT ( 'NONE',  ( -7.227278212944055369, -78.65368819820857027, -5.773064082365189975 ) ) ;
#19397 = CARTESIAN_POINT ( 'NONE',  ( 8.344849100831723376, -76.51161235786649684, 8.271546587476944268 ) ) ;
#19398 = CARTESIAN_POINT ( 'NONE',  ( 0.5812841321855933829, -23.30416868477314551, -10.98463311464191250 ) ) ;
#19399 = DIRECTION ( 'NONE',  ( -1.000000000000000000, 0.000000000000000000, 0.000000000000000000 ) ) ;
#19400 = CARTESIAN_POINT ( 'NONE',  ( -1.178447680628000205, -80.95308451575900222, -0.9280415206345000723 ) ) ;
#19401 = CARTESIAN_POINT ( 'NONE',  ( -8.300970689365472666, -77.25833333333336839, 4.784380313523514339 ) ) ;
#19402 = CARTESIAN_POINT ( 'NONE',  ( -3.553457639398999834, -80.00478455456800475, -1.754685045573999957 ) ) ;
#19403 = CARTESIAN_POINT ( 'NONE',  ( 0.000000000000000000, -75.15999999999999659, 0.000000000000000000 ) ) ;
#19404 = CARTESIAN_POINT ( 'NONE',  ( -10.55336135317719304, -78.08483439053425457, 2.046528030539819021 ) ) ;
#19405 = CARTESIAN_POINT ( 'NONE',  ( -0.4788566569365060865, -83.00635035241097626, 1.154595247919521173 ) ) ;
#19406 = CARTESIAN_POINT ( 'NONE',  ( 9.500000000000000000, -77.14999999999999147, 0.000000000000000000 ) ) ;
#19407 = LINE ( 'NONE', #55416, #21938 ) ;
#19408 = CARTESIAN_POINT ( 'NONE',  ( 1.129337479010032785, -82.04397684591522477, 0.6933189978229028494 ) ) ;
#19409 = LINE ( 'NONE', #19700, #11065 ) ;
#19410 = DIRECTION ( 'NONE',  ( 0.7071067811865475727, 0.000000000000000000, -0.7071067811865475727 ) ) ;
#19411 = CARTESIAN_POINT ( 'NONE',  ( -0.4865042478690436711, -3.500000000000000888, 3.248882910818546410 ) ) ;
#19412 = FACE_OUTER_BOUND ( 'NONE', #57993, .T. ) ;
#19413 = CARTESIAN_POINT ( 'NONE',  ( -1.477284502223000118, -24.72631500296999718, -12.77254812468999923 ) ) ;
#19414 = CARTESIAN_POINT ( 'NONE',  ( 12.51072239526000196, -26.30294702885999669, 0.7871079366006996647 ) ) ;
#19415 = CARTESIAN_POINT ( 'NONE',  ( -5.505695391233000002, -78.58694415034598535, -8.014431902511001127 ) ) ;
#19416 = CARTESIAN_POINT ( 'NONE',  ( -7.610716808838798642, -23.52015489479942190, -10.41172350877303820 ) ) ;
#19417 = CARTESIAN_POINT ( 'NONE',  ( -1.092232985442822102, -80.54166666666664298, -0.6295237254636245616 ) ) ;
#19418 = CARTESIAN_POINT ( 'NONE',  ( 10.02592289919787305, -77.23099517276321535, 4.055125067876876876 ) ) ;
#19419 = CARTESIAN_POINT ( 'NONE',  ( 7.686918321190000292, -21.75560170997999876, 10.48771805380000011 ) ) ;
#19420 = CARTESIAN_POINT ( 'NONE',  ( 5.099999999822000696, -75.20000000017779485, -7.534001399281000208E-10 ) ) ;
#19421 = CARTESIAN_POINT ( 'NONE',  ( -3.997988644197999708, -76.15750634111999773, 11.37999976687000014 ) ) ;
#19422 = ORIENTED_EDGE ( 'NONE', *, *, #21590, .F. ) ;
#19423 = B_SPLINE_SURFACE_WITH_KNOTS ( 'NONE', 3, 3, ( 
 ( #57808, #58103, #17665, #48962 ),
 ( #34784, #34493, #52239, #12079 ),
 ( #29771, #26500, #30061, #21791 ),
 ( #17368, #30924, #47827, #35354 ),
 ( #7930, #16800, #7643, #7358 ),
 ( #43372, #53380, #12361, #12927 ),
 ( #43668, #2931, #3505, #45417 ),
 ( #35345, #58094, #9392, #13801 ) ),
 .UNSPECIFIED., .F., .F., .F.,
 ( 4, 1, 1, 1, 1, 4 ),
 ( 4, 4 ),
 ( -0.01200407345748999953, 0.000000000000000000, 0.3333333333333000081, 0.6666666666667000474, 1.000000000000000000, 1.011997855551999947 ),
 ( -0.3559705542741999906, 1.355970554273999928 ),
 .UNSPECIFIED. ) ;
#19424 = CARTESIAN_POINT ( 'NONE',  ( -1.715387267769999946, -83.11557450217399889, 3.757119535535999866 ) ) ;
#19425 = AXIS2_PLACEMENT_3D ( 'NONE', #55430, #31807, #9394 ) ;
#19426 = CARTESIAN_POINT ( 'NONE',  ( -2.590408569657000282, -80.88335807551204937, -11.10753917875999974 ) ) ;
#19427 = CARTESIAN_POINT ( 'NONE',  ( 9.197769436456411540, -78.34157941349792509, -0.9820442832495991370 ) ) ;
#19428 = CARTESIAN_POINT ( 'NONE',  ( 10.18249594442404415, -54.50907903244432617, 7.792385963361820878 ) ) ;
#19429 = CARTESIAN_POINT ( 'NONE',  ( 9.144378690012999300, -77.60253084224299869, -6.496033325431000094 ) ) ;
#19430 = DIRECTION ( 'NONE',  ( 1.000000000000000000, 0.000000000000000000, 0.000000000000000000 ) ) ;
#19431 = CARTESIAN_POINT ( 'NONE',  ( 9.618404959434000645, -78.09175299886499033, 1.531659799953999812 ) ) ;
#19432 = CARTESIAN_POINT ( 'NONE',  ( 0.3958579896396000608, -81.53291524179999783, -1.618315812554999900 ) ) ;
#19433 = DIRECTION ( 'NONE',  ( 0.000000000000000000, 1.000000000000000000, 0.000000000000000000 ) ) ;
#19434 = CARTESIAN_POINT ( 'NONE',  ( -1.667916687331000070, -55.50151115525000023, 12.49168451095999899 ) ) ;
#19435 = ORIENTED_EDGE ( 'NONE', *, *, #13028, .F. ) ;
#19436 = CIRCLE ( 'NONE', #37368, 10.69999999999999929 ) ;
#19437 = CARTESIAN_POINT ( 'NONE',  ( -0.5999999999999999778, -18.84999999999999787, -10.98362417419999915 ) ) ;
#19438 = CARTESIAN_POINT ( 'NONE',  ( -2.099388381696000023E-14, -0.04999999937965000224, 0.000000000000000000 ) ) ;
#19439 = VECTOR ( 'NONE', #15658, 1000.000000000000000 ) ;
#19440 = ORIENTED_EDGE ( 'NONE', *, *, #23707, .T. ) ;
#19441 = ADVANCED_FACE ( 'NONE', ( #12404 ), #16841, .T. ) ;
#19442 = CARTESIAN_POINT ( 'NONE',  ( 1.315129997485000146, -78.39761010257180374, 0.2213803045116000123 ) ) ;
#19443 = CARTESIAN_POINT ( 'NONE',  ( 9.250000000000000000, -77.74999999999998579, 0.000000000000000000 ) ) ;
#19444 = CARTESIAN_POINT ( 'NONE',  ( 1.838439579890999820, -80.04146898612899008, 11.40569499701999945 ) ) ;
#19445 = ORIENTED_EDGE ( 'NONE', *, *, #3397, .T. ) ;
#19446 = CARTESIAN_POINT ( 'NONE',  ( -9.840265838668001308, -78.30887766239899861, -7.152041583326999685 ) ) ;
#19447 = CARTESIAN_POINT ( 'NONE',  ( 10.20678250203529025, -61.03575784435037122, -7.770339463558867621 ) ) ;
#19448 = VERTEX_POINT ( 'NONE', #21550 ) ;
#19449 = ORIENTED_EDGE ( 'NONE', *, *, #39082, .F. ) ;
#19450 = CARTESIAN_POINT ( 'NONE',  ( -10.01676960210999923, -55.59061945207999855, -7.658895148190000057 ) ) ;
#19451 = CARTESIAN_POINT ( 'NONE',  ( -9.387315177295000979, -79.98803648194748916, 2.697965643110000311 ) ) ;
#19452 = EDGE_CURVE ( 'NONE', #15698, #1523, #8551, .T. ) ;
#19453 = EDGE_LOOP ( 'NONE', ( #50435, #19594, #5354, #55829, #57189, #44334, #53427, #45849, #46058, #17860 ) ) ;
#19454 = CARTESIAN_POINT ( 'NONE',  ( 12.72394144133999916, -55.57839271467000231, 1.930881231431999856 ) ) ;
#19455 = CARTESIAN_POINT ( 'NONE',  ( 10.25201842917796924, -24.12180395215443696, -7.730408553586223697 ) ) ;
#19456 = ORIENTED_EDGE ( 'NONE', *, *, #24089, .F. ) ;
#19457 = CARTESIAN_POINT ( 'NONE',  ( -12.54673765596000123, -24.82199238237999950, -0.9174244429638999110 ) ) ;
#19458 = CARTESIAN_POINT ( 'NONE',  ( -0.3738612770365654647, -80.20118014076501822, -1.192774224883461187 ) ) ;
#19459 = CARTESIAN_POINT ( 'NONE',  ( -0.5222397221475469919, -16.83701780599070474, -12.70447686583903923 ) ) ;
#19460 = CARTESIAN_POINT ( 'NONE',  ( -10.31421052434999908, -76.72175206120299151, 3.823226550887000030 ) ) ;
#19461 = CARTESIAN_POINT ( 'NONE',  ( -12.76303204294000082, -18.73514849292999784, -1.980584515756000030 ) ) ;
#19462 = CARTESIAN_POINT ( 'NONE',  ( 1.459619044399156129, -79.07920200935929245, -0.3821340575799183625 ) ) ;
#19463 = CARTESIAN_POINT ( 'NONE',  ( -0.4747412272618017348, -79.04687498282052616, -4.009948279880011235 ) ) ;
#19464 = ORIENTED_EDGE ( 'NONE', *, *, #35611, .T. ) ;
#19465 = CARTESIAN_POINT ( 'NONE',  ( -3.438348731682000281, -76.61980657813998619, -11.82003900998999946 ) ) ;
#19466 = EDGE_CURVE ( 'NONE', #54466, #55944, #26239, .T. ) ;
#19467 = AXIS2_PLACEMENT_3D ( 'NONE', #11198, #52493, #34462 ) ;
#19468 = CARTESIAN_POINT ( 'NONE',  ( 3.065643863220296694, -2.058380345162022618, -1.728768913878805602 ) ) ;
#19469 = CARTESIAN_POINT ( 'NONE',  ( 7.986976573832000881, -61.52634345601000376, -10.07613380459999952 ) ) ;
#19470 = CARTESIAN_POINT ( 'NONE',  ( 12.21456857099000004, -78.72553890088001083, -1.096995930408000142 ) ) ;
#19471 = CARTESIAN_POINT ( 'NONE',  ( -11.38972971424999869, -76.59660938959198972, -4.593112662244999811 ) ) ;
#19472 = CARTESIAN_POINT ( 'NONE',  ( -3.380118192975993807, -85.79678895079199208, 1.504925579246014111 ) ) ;
#19473 = CONICAL_SURFACE ( 'NONE', #10973, 8.749999999256001360, 0.7853981633972997312 ) ;
#19474 = DIRECTION ( 'NONE',  ( 1.000000000000000000, 0.000000000000000000, 0.000000000000000000 ) ) ;
#19475 = CARTESIAN_POINT ( 'NONE',  ( -7.839627085707410181, -77.98089410207293781, 9.247057760909966007 ) ) ;
#19476 = CARTESIAN_POINT ( 'NONE',  ( -9.066796825632000179, -78.80009492674068383, -6.603885667862000375 ) ) ;
#19477 = EDGE_LOOP ( 'NONE', ( #13104, #20962, #16395 ) ) ;
#19478 = DIRECTION ( 'NONE',  ( 0.000000000000000000, 0.000000000000000000, -1.000000000000000000 ) ) ;
#19479 = CARTESIAN_POINT ( 'NONE',  ( -6.246652488582999929, -77.32445024881999984, 7.288235269262000493 ) ) ;
#19480 = CARTESIAN_POINT ( 'NONE',  ( 12.50000000000000000, -55.54999999966999980, -1.250000000000000000 ) ) ;
#19481 = CARTESIAN_POINT ( 'NONE',  ( -0.1636246173744726473, -78.88541666666664298, 1.249999999999999112 ) ) ;
#19482 = CARTESIAN_POINT ( 'NONE',  ( -2.751186307780999929, -2.732297659067000062, 2.722370634480000273 ) ) ;
#19483 = CARTESIAN_POINT ( 'NONE',  ( -9.747171129529000666, -78.05887766239899861, -7.084379058567000342 ) ) ;
#19484 = CARTESIAN_POINT ( 'NONE',  ( -6.424145201942000227, -78.14004745520499284, 7.175205111309999495 ) ) ;
#19486 = CARTESIAN_POINT ( 'NONE',  ( 10.26300017817221999, -77.91922858884991854, -4.172146172881584292 ) ) ;
#19485 = CARTESIAN_POINT ( 'NONE',  ( -10.64136828584240391, -76.16485984116189911, 4.983422431193929469 ) ) ;
#19487 = CARTESIAN_POINT ( 'NONE',  ( 8.414343270883998471, -78.83155805217599266, 6.955155862361000807 ) ) ;
#19488 = CARTESIAN_POINT ( 'NONE',  ( 3.402340145821319606, -85.80681307385597734, 2.471221923361610173 ) ) ;
#19489 = ORIENTED_EDGE ( 'NONE', *, *, #8311, .F. ) ;
#19490 = CARTESIAN_POINT ( 'NONE',  ( -9.000000000000000000, -0.5000000000000000000, 0.000000000000000000 ) ) ;
#19491 = CARTESIAN_POINT ( 'NONE',  ( 0.000000000000000000, -80.70000000000000284, 0.000000000000000000 ) ) ;
#19492 = DIRECTION ( 'NONE',  ( -1.000000000000000000, 0.000000000000000000, 0.000000000000000000 ) ) ;
#19493 = CARTESIAN_POINT ( 'NONE',  ( -9.813193589766999736, -79.02741007977999743, -4.915816122623000162 ) ) ;
#19494 = CARTESIAN_POINT ( 'NONE',  ( 0.000000000000000000, -75.15999999999999659, 0.000000000000000000 ) ) ;
#19495 = CARTESIAN_POINT ( 'NONE',  ( 4.081138785858000162, -78.91908747365698673, 8.644947643559998340 ) ) ;
#19496 = CARTESIAN_POINT ( 'NONE',  ( 10.01676221091000052, -18.79058563473000021, -7.658899961851000526 ) ) ;
#19497 = CARTESIAN_POINT ( 'NONE',  ( 7.958763980604000032, -17.52301961031999866, 9.723170659100999202 ) ) ;
#19498 = VERTEX_POINT ( 'NONE', #54885 ) ;
#19499 = CARTESIAN_POINT ( 'NONE',  ( -9.103325846391999931, -78.82668513919199427, -6.630491919364000175 ) ) ;
#19500 = CARTESIAN_POINT ( 'NONE',  ( -9.164301350569918014, -77.48739481387521266, 1.453017405635841808 ) ) ;
#19501 = CARTESIAN_POINT ( 'NONE',  ( 11.75055246895291994, -79.79038423862893126, -1.413995404558705760 ) ) ;
#19502 = LINE ( 'NONE', #15065, #53297 ) ;
#19503 = CARTESIAN_POINT ( 'NONE',  ( -9.236974595845435232, -77.51476500836666617, -9.065058572735408049 ) ) ;
#19504 = ADVANCED_FACE ( 'NONE', ( #14434 ), #54425, .F. ) ;
#19505 = CARTESIAN_POINT ( 'NONE',  ( 0.8823246602996009935, -81.41312424128729219, 0.8850044837457081703 ) ) ;
#19506 =( BOUNDED_SURFACE ( )  B_SPLINE_SURFACE ( 3, 3, ( 
 ( #12030, #7595, #8171, #16459 ),
 ( #3452, #12595, #25594, #17610 ),
 ( #39466, #35599, #53329, #43614 ),
 ( #26449, #53626, #21741, #26174 ),
 ( #30593, #12875, #57756, #57182 ),
 ( #44773, #22324, #40340, #34440 ),
 ( #16749, #34728, #17313, #52757 ),
 ( #48341, #25880, #43907, #35300 ),
 ( #45665, #55084, #46250, #50382 ),
 ( #45958, #45370, #36777, #32623 ),
 ( #14631, #14338, #18495, #45075 ),
 ( #54516, #5488, #54797, #58348 ),
 ( #9929, #40931, #519, #22917 ),
 ( #23493, #5778, #41506, #1092 ),
 ( #10218, #31460, #4626, #23785 ) ),
 .UNSPECIFIED., .F., .F., .F. ) 
 B_SPLINE_SURFACE_WITH_KNOTS ( ( 4, 1, 1, 1, 1, 1, 1, 1, 1, 1, 1, 1, 4 ),
 ( 4, 4 ),
 ( 0.009836338020448129327, 0.09153385889397000486, 0.1732268882812000033, 0.2549245844128000260, 0.3366128623372000028, 0.4183102317861999708, 0.5000049915032999115, 0.5816997502458999270, 0.6633970872647999562, 0.7450853589770999319, 0.8267830756728000718, 0.9084760833474000430, 0.9901736249421290159 ),
 ( 0.000000000000000000, 1.000000000000000000 ),
 .UNSPECIFIED. ) 
 GEOMETRIC_REPRESENTATION_ITEM ( )  RATIONAL_B_SPLINE_SURFACE ( (
 ( 1.000000000000000000, 0.3333333333333318715, 0.3333333333333318715, 1.000000000000000000),
 ( 1.000000000000000000, 0.3333333333333318715, 0.3333333333333318715, 1.000000000000000000),
 ( 1.000000000000000000, 0.3333333333333318715, 0.3333333333333318715, 1.000000000000000000),
 ( 1.000000000000000000, 0.3333333333333318715, 0.3333333333333318715, 1.000000000000000000),
 ( 1.000000000000000000, 0.3333333333333318715, 0.3333333333333318715, 1.000000000000000000),
 ( 1.000000000000000000, 0.3333333333333318715, 0.3333333333333318715, 1.000000000000000000),
 ( 1.000000000000000000, 0.3333333333333318715, 0.3333333333333318715, 1.000000000000000000),
 ( 1.000000000000000000, 0.3333333333333318715, 0.3333333333333318715, 1.000000000000000000),
 ( 1.000000000000000000, 0.3333333333333318715, 0.3333333333333318715, 1.000000000000000000),
 ( 1.000000000000000000, 0.3333333333333318715, 0.3333333333333318715, 1.000000000000000000),
 ( 1.000000000000000000, 0.3333333333333318715, 0.3333333333333318715, 1.000000000000000000),
 ( 1.000000000000000000, 0.3333333333333318715, 0.3333333333333318715, 1.000000000000000000),
 ( 1.000000000000000000, 0.3333333333333318715, 0.3333333333333318715, 1.000000000000000000),
 ( 1.000000000000000000, 0.3333333333333318715, 0.3333333333333318715, 1.000000000000000000),
 ( 1.000000000000000000, 0.3333333333333318715, 0.3333333333333318715, 1.000000000000000000) ) ) 
 REPRESENTATION_ITEM ( '' )  SURFACE ( )  );
#19507 = ADVANCED_FACE ( 'NONE', ( #50475 ), #13480, .F. ) ;
#19508 = CARTESIAN_POINT ( 'NONE',  ( -2.848604465265602403, -78.95447547272175370, -10.84928852802099009 ) ) ;
#19509 = CARTESIAN_POINT ( 'NONE',  ( -9.320350064846081750, -77.00000000000000000, 0.5764697903331228446 ) ) ;
#19510 = CARTESIAN_POINT ( 'NONE',  ( 10.98768939184196647, -23.45050660130683795, -0.5207199486368357944 ) ) ;
#19511 = VECTOR ( 'NONE', #1761, 1000.000000000000000 ) ;
#19512 = CARTESIAN_POINT ( 'NONE',  ( 0.000000000000000000, -87.25000000009099210, -9.649999999909001147 ) ) ;
#19513 = CIRCLE ( 'NONE', #52506, 1.000000000000000000 ) ;
#19514 = CARTESIAN_POINT ( 'NONE',  ( -10.13801387673548682, -78.48139510519006024, -4.205769073302976224 ) ) ;
#19515 = CARTESIAN_POINT ( 'NONE',  ( -11.68767212001979594, -77.27916666666666856, 3.140974612311315806 ) ) ;
#19516 = ORIENTED_EDGE ( 'NONE', *, *, #19661, .F. ) ;
#19517 = EDGE_CURVE ( 'NONE', #37628, #42913, #40245, .T. ) ;
#19518 = AXIS2_PLACEMENT_3D ( 'NONE', #17388, #43976, #48983 ) ;
#19519 = EDGE_LOOP ( 'NONE', ( #6575, #41345, #45752, #12104 ) ) ;
#19520 = DIRECTION ( 'NONE',  ( 0.000000000000000000, 1.000000000000000000, 0.000000000000000000 ) ) ;
#19521 = CARTESIAN_POINT ( 'NONE',  ( 8.948459357138670356, -78.80341436924688026, -5.956977988863866535 ) ) ;
#19522 = AXIS2_PLACEMENT_3D ( 'NONE', #36793, #4929, #41521 ) ;
#19523 = VERTEX_POINT ( 'NONE', #38044 ) ;
#19524 = CARTESIAN_POINT ( 'NONE',  ( 7.778176538613999824, -76.43620349110052814, -8.035785801754000701 ) ) ;
#19525 = CARTESIAN_POINT ( 'NONE',  ( -8.914528142879424522, -79.37164879542098106, 3.287790175345898902 ) ) ;
#19526 = CARTESIAN_POINT ( 'NONE',  ( 10.31444895690999886, -61.10075144983999706, 7.758883253367000243 ) ) ;
#19527 = CARTESIAN_POINT ( 'NONE',  ( 0.5999999999999999778, -18.84999999999000053, 11.79999999999999893 ) ) ;
#19528 = CARTESIAN_POINT ( 'NONE',  ( 9.789953784408815807, -78.75102124931834169, -6.904838711737845358 ) ) ;
#19529 = CARTESIAN_POINT ( 'NONE',  ( -0.4146318973827000098, -79.38816346897299070, -11.20920117498000046 ) ) ;
#19530 = ORIENTED_EDGE ( 'NONE', *, *, #43250, .F. ) ;
#19531 = DIRECTION ( 'NONE',  ( 0.000000000000000000, -1.000000000000000000, 0.000000000000000000 ) ) ;
#19532 = VERTEX_POINT ( 'NONE', #33316 ) ;
#19533 = CARTESIAN_POINT ( 'NONE',  ( 8.794698800388047744, -77.37511376347532632, 2.866210580583882450 ) ) ;
#19534 = CARTESIAN_POINT ( 'NONE',  ( -0.9898995639662998558, -79.68446749155899056, 0.8721608040441000131 ) ) ;
#19535 = CARTESIAN_POINT ( 'NONE',  ( 1.500000000000000000, -77.75000000000000000, 0.000000000000000000 ) ) ;
#19536 = CARTESIAN_POINT ( 'NONE',  ( -0.9855275769405000830, -77.61600855774059937, -1.152289182367999931 ) ) ;
#19537 = CARTESIAN_POINT ( 'NONE',  ( -10.12290050256999940, -18.75000002239000096, -7.648026768411000376 ) ) ;
#19538 = CARTESIAN_POINT ( 'NONE',  ( 10.35453599130000057, -76.65783510652001098, -6.064947188958000446 ) ) ;
#19539 = CARTESIAN_POINT ( 'NONE',  ( 1.341343219651000229, -79.09091657910998663, -0.9216622887798999741 ) ) ;
#19540 = CARTESIAN_POINT ( 'NONE',  ( 10.92979202429999930, -79.25475665554398574, 1.617881315982000245 ) ) ;
#19541 = CARTESIAN_POINT ( 'NONE',  ( -8.220407391935999897, -24.81950084232000364, -9.523310056109000499 ) ) ;
#19542 = CARTESIAN_POINT ( 'NONE',  ( 12.87022657272000004, -56.01514526721999943, -2.062597299672999540 ) ) ;
#19543 = CARTESIAN_POINT ( 'NONE',  ( 3.235133020217000333, -82.37863818301799768, -1.192152034091999990 ) ) ;
#19544 = ORIENTED_EDGE ( 'NONE', *, *, #50116, .F. ) ;
#19545 = CARTESIAN_POINT ( 'NONE',  ( -10.96763318152921407, -77.20000000000001705, 0.8289010833759121732 ) ) ;
#19546 = CARTESIAN_POINT ( 'NONE',  ( -1.576937714420000081, -81.29921328099999300, 0.6430338560479000876 ) ) ;
#19547 = CARTESIAN_POINT ( 'NONE',  ( 8.098906566116852446, -77.90749627220959894, 7.103892318221430635 ) ) ;
#19548 = CARTESIAN_POINT ( 'NONE',  ( 0.9627474882855999727, -78.19750779982500433, -11.94107121277999894 ) ) ;
#19549 = CARTESIAN_POINT ( 'NONE',  ( -7.645391692608000334, -18.78469634161999835, 10.18949678827999961 ) ) ;
#19550 = EDGE_CURVE ( 'NONE', #35953, #44782, #33246, .T. ) ;
#19551 = CARTESIAN_POINT ( 'NONE',  ( -1.268945471415019455, -78.24314195652412707, 0.1161799656682465792 ) ) ;
#19552 = CARTESIAN_POINT ( 'NONE',  ( 3.498582912420285407, -3.490953291830131811, -0.3978866406648630116 ) ) ;
#19553 = CARTESIAN_POINT ( 'NONE',  ( 10.43503646057562229, -80.86970219550423167, 2.582246741427850267 ) ) ;
#19554 = LINE ( 'NONE', #23108, #14643 ) ;
#19555 = CARTESIAN_POINT ( 'NONE',  ( -3.654181830570668144, -86.07389998728979208, 1.626946572303400229 ) ) ;
#19556 = CARTESIAN_POINT ( 'NONE',  ( 6.225574660483999878, -78.28614743357699979, 9.107357164861998200 ) ) ;
#19557 = CARTESIAN_POINT ( 'NONE',  ( -11.38972971424999869, -76.68050008331320555, -4.593112662244999811 ) ) ;
#19558 = DIRECTION ( 'NONE',  ( 0.9999548435846228323, 0.000000000000000000, 0.009503199022040218977 ) ) ;
#19559 = ORIENTED_EDGE ( 'NONE', *, *, #34746, .F. ) ;
#19560 = CARTESIAN_POINT ( 'NONE',  ( -1.208084210770999922, -81.73085454120899840, 0.5648970606752000689 ) ) ;
#19561 = CARTESIAN_POINT ( 'NONE',  ( -0.8445585116414000559, -61.51040443210000319, -12.43380736240999873 ) ) ;
#19562 = VECTOR ( 'NONE', #42029, 1000.000000000000114 ) ;
#19563 = CARTESIAN_POINT ( 'NONE',  ( -7.889735440111223852, -55.04957415510977370, 7.666647577131773694 ) ) ;
#19564 = CARTESIAN_POINT ( 'NONE',  ( 0.1392748842281999744, -77.14011761966898462, 11.21600254538999941 ) ) ;
#19565 = CARTESIAN_POINT ( 'NONE',  ( -7.508490145779999736, -78.87459365710098780, -8.005410190140000992 ) ) ;
#19566 = AXIS2_PLACEMENT_3D ( 'NONE', #51184, #19580, #19003 ) ;
#19567 = CARTESIAN_POINT ( 'NONE',  ( 7.948089776770999926, -24.44033979720000360, -9.636757666087000018 ) ) ;
#19568 = CARTESIAN_POINT ( 'NONE',  ( -3.787130605393867810, -83.28645832267650917, -1.440612511541762064 ) ) ;
#19569 = DIRECTION ( 'NONE',  ( 0.000000000000000000, -0.7071067811866525998, -0.7071067811864425456 ) ) ;
#19570 = CARTESIAN_POINT ( 'NONE',  ( -7.624341764906000130, -55.53514850498000044, -10.42531124851000079 ) ) ;
#19571 = CARTESIAN_POINT ( 'NONE',  ( -3.362765314666999572, -84.83869503318800298, -2.470196700500999487 ) ) ;
#19572 = CARTESIAN_POINT ( 'NONE',  ( 1.500000000000000000, -80.26041666666668561, 0.1963495408493652339 ) ) ;
#19573 = CARTESIAN_POINT ( 'NONE',  ( 7.969034948567999876, -54.17623147781999648, -9.934750886883000121 ) ) ;
#19574 = CARTESIAN_POINT ( 'NONE',  ( -10.40633193566000081, -78.21047970211098743, -4.317081191017999586 ) ) ;
#19575 = EDGE_CURVE ( 'NONE', #27322, #13927, #15768, .T. ) ;
#19576 = CARTESIAN_POINT ( 'NONE',  ( -0.5713041596650000331, -79.36585677060999444, -1.442599867604999808 ) ) ;
#19577 = CARTESIAN_POINT ( 'NONE',  ( 0.1536065772846999800, -77.82239276298000163, 1.313283405909000168 ) ) ;
#19578 = CARTESIAN_POINT ( 'NONE',  ( 11.99999999999999822, -77.56041666666668277, 1.570796326794923203 ) ) ;
#19579 = CARTESIAN_POINT ( 'NONE',  ( 1.188464411453045155, -82.05564304759461436, 0.9880997565357596546 ) ) ;
#19580 = DIRECTION ( 'NONE',  ( 0.000000000000000000, -1.000000000000000000, 0.000000000000000000 ) ) ;
#19581 = ORIENTED_EDGE ( 'NONE', *, *, #32809, .F. ) ;
#19582 = CARTESIAN_POINT ( 'NONE',  ( 1.222194407272268135, -79.83372676383018529, -0.2630658939555856612 ) ) ;
#19583 = CARTESIAN_POINT ( 'NONE',  ( -8.792808668394924254, -53.57303577587560994, 9.175550543417134719 ) ) ;
#19584 = ORIENTED_EDGE ( 'NONE', *, *, #49441, .F. ) ;
#19585 = CARTESIAN_POINT ( 'NONE',  ( -0.8804009821880611764, -81.66335410272444051, -0.8868692789278864730 ) ) ;
#19586 = SURFACE_SIDE_STYLE ('',( #46477 ) ) ;
#19587 = CARTESIAN_POINT ( 'NONE',  ( 2.165712778014000417, -78.75057660935300419, 10.93454565734000106 ) ) ;
#19588 = DIRECTION ( 'NONE',  ( 0.000000000000000000, -0.7071067811866525998, -0.7071067811864425456 ) ) ;
#19589 = ORIENTED_EDGE ( 'NONE', *, *, #44608, .T. ) ;
#19590 = EDGE_CURVE ( 'NONE', #8688, #56557, #20494, .T. ) ;
#19591 = ORIENTED_EDGE ( 'NONE', *, *, #37223, .T. ) ;
#19592 = CARTESIAN_POINT ( 'NONE',  ( 0.1717165440430999945, -81.41328242421499795, 1.506471234578999896 ) ) ;
#19593 = ADVANCED_FACE ( 'NONE', ( #34465 ), #7328, .T. ) ;
#19594 = ORIENTED_EDGE ( 'NONE', *, *, #52535, .F. ) ;
#19595 = ORIENTED_EDGE ( 'NONE', *, *, #43314, .T. ) ;
#19596 = CARTESIAN_POINT ( 'NONE',  ( 1.667269374596999976, -18.79060116514999734, 12.49858097730999873 ) ) ;
#19597 = DIRECTION ( 'NONE',  ( 1.000000000000000000, 0.000000000000000000, 0.000000000000000000 ) ) ;
#19598 = APPLICATION_PROTOCOL_DEFINITION ( 'draft international standard', 'automotive_design', 1998, #48140 ) ;
#19599 = CARTESIAN_POINT ( 'NONE',  ( 2.262828338668485983, -82.24583331669903430, -2.595881390529711119 ) ) ;
#19600 = CARTESIAN_POINT ( 'NONE',  ( 7.374560639698993114, -76.47708333331846120, -9.596002108778149520 ) ) ;
#19601 = CARTESIAN_POINT ( 'NONE',  ( 6.545761160578629223, -78.28756486186320274, -6.535701422592273602 ) ) ;
#19602 = CARTESIAN_POINT ( 'NONE',  ( -1.407171709420418138, -78.11458333333331439, -10.75000000000000000 ) ) ;
#19603 = CONICAL_SURFACE ( 'NONE', #55422, 2.149999999947999729, 0.7853981633972997312 ) ;
#19604 = EDGE_LOOP ( 'NONE', ( #11872, #51731, #25383, #24799 ) ) ;
#19605 = EDGE_LOOP ( 'NONE', ( #58132, #19232, #7887, #25382 ) ) ;
#19606 = CARTESIAN_POINT ( 'NONE',  ( 12.00000000000000000, -77.64999999999999147, 0.000000000000000000 ) ) ;
#19607 = CARTESIAN_POINT ( 'NONE',  ( -12.72923908218061406, -23.77554307156079005, 1.930512971251469478 ) ) ;
#19608 = CARTESIAN_POINT ( 'NONE',  ( 1.199500263597268246, -79.30208333333332860, 0.9218200799623752495 ) ) ;
#19609 = DIRECTION ( 'NONE',  ( 0.000000000000000000, 1.000000000000000000, 0.000000000000000000 ) ) ;
#19610 = CARTESIAN_POINT ( 'NONE',  ( 1.260641617779999946, -77.63448153939899044, 9.621927669549000584 ) ) ;
#19611 = EDGE_CURVE ( 'NONE', #18221, #33152, #57930, .T. ) ;
#19612 =( GEOMETRIC_REPRESENTATION_CONTEXT ( 3 ) GLOBAL_UNCERTAINTY_ASSIGNED_CONTEXT ( ( #2411 ) ) GLOBAL_UNIT_ASSIGNED_CONTEXT ( ( #44948, #13341, #31337 ) ) REPRESENTATION_CONTEXT ( 'NONE', 'WORKASPACE' ) );
#19613 = CARTESIAN_POINT ( 'NONE',  ( 0.000000000000000000, 4.040000000000000036, 0.000000000000000000 ) ) ;
#19614 = CARTESIAN_POINT ( 'NONE',  ( 3.615006554704453201, -85.81033527783026216, 1.103425733751174587 ) ) ;
#19615 = CARTESIAN_POINT ( 'NONE',  ( 4.336551063001060413, -77.45429869360749819, -11.23466680206521673 ) ) ;
#19616 = CARTESIAN_POINT ( 'NONE',  ( -0.5581707956298000983, -81.04937075464998486, 1.358247929972999701 ) ) ;
#19617 = CYLINDRICAL_SURFACE ( 'NONE', #35667, 1.000000000000000000 ) ;
#19618 = CARTESIAN_POINT ( 'NONE',  ( 0.9278479323973001236, -81.32799336705899407, 4.070467834415999242 ) ) ;
#19619 = CARTESIAN_POINT ( 'NONE',  ( -10.01749678874999994, -55.60819056964000140, 7.660430392551000445 ) ) ;
#19620 = CARTESIAN_POINT ( 'NONE',  ( -5.580112777935000601, -77.99451001420200669, 7.918523194479999638 ) ) ;
#19621 = CARTESIAN_POINT ( 'NONE',  ( -1.250000000000000000, -55.54999999966999980, 12.00000000000000000 ) ) ;
#19622 = CARTESIAN_POINT ( 'NONE',  ( 1.667936688463999895, -22.76486430425999785, -12.53239398059000109 ) ) ;
#19623 = EDGE_CURVE ( 'NONE', #35254, #43036, #31140, .T. ) ;
#19625 = CARTESIAN_POINT ( 'NONE',  ( 1.194090705999000024, -17.55968341096999552, -12.43436538489999954 ) ) ;
#19624 = DIRECTION ( 'NONE',  ( 0.000000000000000000, -1.000000000000000000, 0.000000000000000000 ) ) ;
#19626 = CARTESIAN_POINT ( 'NONE',  ( 0.000000000000000000, -2.660000000000000142, 0.000000000000000000 ) ) ;
#19627 = CARTESIAN_POINT ( 'NONE',  ( -10.42531124905999995, -18.73514851523999880, 7.624341765453999997 ) ) ;
#19628 = CARTESIAN_POINT ( 'NONE',  ( 2.234646451474000095, -2.677064556719999988, 3.080979982494000069 ) ) ;
#19629 = CARTESIAN_POINT ( 'NONE',  ( 8.600237018945074752, -77.19999999999998863, -6.594552368571869216 ) ) ;
#19630 = EDGE_CURVE ( 'NONE', #33033, #25961, #40661, .T. ) ;
#19631 = ORIENTED_EDGE ( 'NONE', *, *, #9718, .F. ) ;
#19632 = CARTESIAN_POINT ( 'NONE',  ( -2.925837195856660244, -3.499999999999999556, -1.558917296219500592 ) ) ;
#19633 = CARTESIAN_POINT ( 'NONE',  ( 0.3116081092048096912, -18.31315380225280975, -10.99615594221662640 ) ) ;
#19634 = CARTESIAN_POINT ( 'NONE',  ( -2.879226727952091114, -79.09583333333331723, 10.71369944335146940 ) ) ;
#19635 = CARTESIAN_POINT ( 'NONE',  ( 0.7419868901144667239, -78.42466652974195540, 1.005884453515640597 ) ) ;
#19636 = CARTESIAN_POINT ( 'NONE',  ( 6.393851920857000160, -79.71037340482598665, 7.217821578210998901 ) ) ;
#19637 = CARTESIAN_POINT ( 'NONE',  ( 1.750000000001000089, -22.75100836360999779, -12.60354432389999957 ) ) ;
#19638 = CARTESIAN_POINT ( 'NONE',  ( 0.000000000000000000, -0.09999999858569999511, 0.000000000000000000 ) ) ;
#19639 = CARTESIAN_POINT ( 'NONE',  ( 1.750000000000000000, -23.24999999688999708, -12.50000000000000000 ) ) ;
#19640 = CIRCLE ( 'NONE', #1786, 9.599999999999999645 ) ;
#19641 = CARTESIAN_POINT ( 'NONE',  ( 2.791340874175999520, -79.15608667140098476, -8.894122046368000412 ) ) ;
#19642 = CARTESIAN_POINT ( 'NONE',  ( 0.000000000000000000, -75.10000000032299283, 0.000000000000000000 ) ) ;
#19643 = CARTESIAN_POINT ( 'NONE',  ( -4.822148453319999639, -77.33252430226399099, -10.07035697449999923 ) ) ;
#19644 = CARTESIAN_POINT ( 'NONE',  ( 1.593230767012999927, -81.16732750385499173, 0.1864398872768000259 ) ) ;
#19645 = CARTESIAN_POINT ( 'NONE',  ( -0.5982973345652318198, -82.01490259020367546, 1.110242726331215790 ) ) ;
#19646 = CARTESIAN_POINT ( 'NONE',  ( -8.334831687997999339, -78.48234702511798844, 4.375131454052000102 ) ) ;
#19648 = CARTESIAN_POINT ( 'NONE',  ( -0.4617212151683000032, -1.236168933658999824, 3.989551193614000013 ) ) ;
#19647 = CARTESIAN_POINT ( 'NONE',  ( 2.081147779020000144, -85.38829592649000233, 3.372659028315000196 ) ) ;
#19649 = CARTESIAN_POINT ( 'NONE',  ( 8.857115352654000517, -79.40955584965399794, -3.584237475251999872 ) ) ;
#19650 = FACE_OUTER_BOUND ( 'NONE', #51340, .T. ) ;
#19651 = CARTESIAN_POINT ( 'NONE',  ( 7.614522461194726866, -80.28763416514415496, -7.588239908555904023 ) ) ;
#19652 = CARTESIAN_POINT ( 'NONE',  ( -6.215526947630453769, -77.17609984879747742, -8.770830743108882999 ) ) ;
#19653 = FACE_OUTER_BOUND ( 'NONE', #30244, .T. ) ;
#19654 = AXIS2_PLACEMENT_3D ( 'NONE', #38705, #33690, #15988 ) ;
#19655 = ORIENTED_EDGE ( 'NONE', *, *, #43557, .T. ) ;
#19656 = EDGE_LOOP ( 'NONE', ( #7026, #27351, #32308, #46416 ) ) ;
#19657 = CARTESIAN_POINT ( 'NONE',  ( 0.4713521909880000194, -79.07356383116399456, 12.02020425643999957 ) ) ;
#19658 = CARTESIAN_POINT ( 'NONE',  ( 0.6291625305437360538, -78.26672467768266017, -1.091960772762393006 ) ) ;
#19659 = CARTESIAN_POINT ( 'NONE',  ( 7.634645345497309776, -18.52415927528287654, 10.10912681051257778 ) ) ;
#19660 = ORIENTED_EDGE ( 'NONE', *, *, #57590, .T. ) ;
#19661 = EDGE_CURVE ( 'NONE', #2249, #10966, #7846, .T. ) ;
#19662 = CARTESIAN_POINT ( 'NONE',  ( -11.91766194687999914, -78.11916490272500369, 0.6362673702790999641 ) ) ;
#19663 = EDGE_CURVE ( 'NONE', #44855, #32127, #4940, .T. ) ;
#19664 = EDGE_LOOP ( 'NONE', ( #52136, #31171, #10888 ) ) ;
#19665 = ORIENTED_EDGE ( 'NONE', *, *, #55500, .T. ) ;
#19666 = CARTESIAN_POINT ( 'NONE',  ( -10.75000000000000355, -78.98958333333331439, 1.407171709420384609 ) ) ;
#19667 = ORIENTED_EDGE ( 'NONE', *, *, #8464, .F. ) ;
#19668 = CARTESIAN_POINT ( 'NONE',  ( 1.666655288874999918, -79.68942003686028386, 3.131584311337999971 ) ) ;
#19669 = CARTESIAN_POINT ( 'NONE',  ( 6.101084436648303466, -79.21938963383225030, 7.282006857732869598 ) ) ;
#19670 = EDGE_LOOP ( 'NONE', ( #16818, #19445, #19972 ) ) ;
#19671 = CARTESIAN_POINT ( 'NONE',  ( -7.601397897754999633, -55.54999999966999980, 9.369164850722000892 ) ) ;
#19672 = CARTESIAN_POINT ( 'NONE',  ( -7.691916945401000127, -58.55365779174999830, 10.42274798264000069 ) ) ;
#19673 = ORIENTED_EDGE ( 'NONE', *, *, #33087, .T. ) ;
#19674 = CARTESIAN_POINT ( 'NONE',  ( -1.218920058826058916, -79.58278420342887216, 0.2778685722280217485 ) ) ;
#19675 = CARTESIAN_POINT ( 'NONE',  ( 1.378196749914432973, -78.03568483536376732, 0.6686781945394131288 ) ) ;
#19676 = CARTESIAN_POINT ( 'NONE',  ( 1.005394801847710129, -79.80000000000001137, -11.73748890211396301 ) ) ;
#19677 = CARTESIAN_POINT ( 'NONE',  ( -7.919595949288999570, -55.65000000488999632, -8.768124086549999419 ) ) ;
#19678 = CARTESIAN_POINT ( 'NONE',  ( 0.002996482912751207480, -0.9843749999025924735, 3.305856831758737790 ) ) ;
#19680 = EDGE_CURVE ( 'NONE', #1025, #6714, #24057, .T. ) ;
#19679 = AXIS2_PLACEMENT_3D ( 'NONE', #12347, #30334, #47810 ) ;
#19681 = CARTESIAN_POINT ( 'NONE',  ( -5.681372509047000641, -78.32522920577524417, -7.867192369580999767 ) ) ;
#19682 = CARTESIAN_POINT ( 'NONE',  ( 7.778176538613999824, -76.38452096864399721, -8.035785801754000701 ) ) ;
#19683 = CARTESIAN_POINT ( 'NONE',  ( -3.075537641221584018, -77.19583333333332575, 11.44417895085269876 ) ) ;
#19684 = EDGE_CURVE ( 'NONE', #40274, #1677, #4652, .T. ) ;
#19685 = FACE_OUTER_BOUND ( 'NONE', #55317, .T. ) ;
#19686 = CARTESIAN_POINT ( 'NONE',  ( -7.833419388303895836, -78.64479959160827605, -4.919153442762366879 ) ) ;
#19687 = CARTESIAN_POINT ( 'NONE',  ( 3.011810901700481935, -76.55381572931285916, 11.35858098727523569 ) ) ;
#19688 = CARTESIAN_POINT ( 'NONE',  ( -0.3116081092089518778, -23.68684619774715117, -10.99615594221646475 ) ) ;
#19689 = CARTESIAN_POINT ( 'NONE',  ( 0.000000000000000000, -75.15999999999999659, 0.000000000000000000 ) ) ;
#19690 = B_SPLINE_CURVE_WITH_KNOTS ( 'NONE', 3,
 ( #27958, #50140, #45418, #1715, #37117, #50726, #14103, #36539, #41555, #14387, #18835, #28247, #22967, #46301, #19417, #37407, #55428, #40977 ),
 .UNSPECIFIED., .F., .F.,
 ( 4, 2, 2, 2, 2, 2, 2, 2, 4 ),
 ( 0.000000000000000000, 0.1250000000000000833, 0.2500000000000001110, 0.3750000000000000000, 0.4999999999999999445, 0.6249999999999998890, 0.7499999999999997780, 0.8749999999999998890, 1.000000000000000000 ),
 .UNSPECIFIED. ) ;
#19691 = CARTESIAN_POINT ( 'NONE',  ( -5.622587949631386195, -80.18243779068814092, -9.454352941869160531 ) ) ;
#19692 = CARTESIAN_POINT ( 'NONE',  ( -3.007576031741168610, -3.070405536610469888, 1.229591291355605298 ) ) ;
#19693 = CARTESIAN_POINT ( 'NONE',  ( 3.263605101345000037, -79.15917549782629692, -1.494195225221999879 ) ) ;
#19694 = CARTESIAN_POINT ( 'NONE',  ( -10.65825678370000063, -79.61563558397199358, -5.693941594808000772 ) ) ;
#19695 = CARTESIAN_POINT ( 'NONE',  ( -10.58971709958329477, -78.08629155915249953, 1.850469969248101254 ) ) ;
#19696 = VECTOR ( 'NONE', #46205, 1000.000000000000114 ) ;
#19697 = CARTESIAN_POINT ( 'NONE',  ( 0.4701836139821906069, -82.94435837239699083, 1.158166872552657045 ) ) ;
#19698 = DIRECTION ( 'NONE',  ( 0.000000000000000000, 1.000000000000000000, 0.000000000000000000 ) ) ;
#19699 = CARTESIAN_POINT ( 'NONE',  ( -8.315421822073089331, -76.26185017328086246, -8.301069858640518717 ) ) ;
#19700 = CARTESIAN_POINT ( 'NONE',  ( 11.00000000000000000, -78.94999999999998863, -1.064824513673000067E-14 ) ) ;
#19701 = EDGE_CURVE ( 'NONE', #38648, #19229, #831, .T. ) ;
#19702 = CARTESIAN_POINT ( 'NONE',  ( -10.00831380746999955, -60.17230364551999600, -7.646786653150000390 ) ) ;
#19703 = DIRECTION ( 'NONE',  ( -1.000000000000000000, 0.000000000000000000, 0.000000000000000000 ) ) ;
#19704 = CARTESIAN_POINT ( 'NONE',  ( 10.04116292117000064, -59.56462890159999546, 7.682344222584999827 ) ) ;
#19705 = DIRECTION ( 'NONE',  ( 0.000000000000000000, 0.000000000000000000, 1.000000000000000000 ) ) ;
#19706 = CARTESIAN_POINT ( 'NONE',  ( 2.210712544800999879, -79.15309415034599283, -9.468498208576999531 ) ) ;
#19707 = CARTESIAN_POINT ( 'NONE',  ( -9.073558136264555429, -25.22808769493118319, -8.894842552359547128 ) ) ;
#19708 = CARTESIAN_POINT ( 'NONE',  ( 1.750000000000000000, -18.75000000240999753, -12.50000000000000000 ) ) ;
#19709 = CARTESIAN_POINT ( 'NONE',  ( 6.634077760214808883, -78.12828546955671527, -8.488125058123570099 ) ) ;
#19710 = CARTESIAN_POINT ( 'NONE',  ( -0.1577822530794796563, -78.22391181108908143, -11.07750337872512780 ) ) ;
#19711 = CARTESIAN_POINT ( 'NONE',  ( 8.867070753125000593, -78.54984699098105239, -6.468312982590000537 ) ) ;
#19712 = CARTESIAN_POINT ( 'NONE',  ( -9.761040558467000139, -76.80558987842999841, -7.085928052393999366 ) ) ;
#19713 = ORIENTED_EDGE ( 'NONE', *, *, #38085, .T. ) ;
#19714 = CARTESIAN_POINT ( 'NONE',  ( 4.129628149831999551, -82.63457450217399014, -0.06497298467246999387 ) ) ;
#19715 = EDGE_CURVE ( 'NONE', #31102, #15817, #48765, .T. ) ;
#19716 = CARTESIAN_POINT ( 'NONE',  ( 1.860817577827999836, -80.63854927348660340, 11.25277748102000075 ) ) ;
#19717 = AXIS2_PLACEMENT_3D ( 'NONE', #32569, #37598, #2191 ) ;
#19718 = CARTESIAN_POINT ( 'NONE',  ( 9.035162686194604831, -78.33298600581431970, -1.982237826727912156 ) ) ;
#19719 = CARTESIAN_POINT ( 'NONE',  ( 12.66316452100000056, -61.97866137636000161, -0.04044945982128999445 ) ) ;
#19720 = CARTESIAN_POINT ( 'NONE',  ( 1.633411169670999863, -78.03831233027200653, -11.09730050697999992 ) ) ;
#19721 = CARTESIAN_POINT ( 'NONE',  ( 8.485281374238999419, -18.75000000000000000, -8.485281374238999419 ) ) ;
#19722 = CARTESIAN_POINT ( 'NONE',  ( 9.189097042878000110, -78.66725766396999120, 2.883349701574000168 ) ) ;
#19723 = CARTESIAN_POINT ( 'NONE',  ( 1.268533116358999902, -83.66757477367698925, -3.974591678799999972 ) ) ;
#19724 = DIRECTION ( 'NONE',  ( 0.000000000000000000, -1.000000000000000000, 0.000000000000000000 ) ) ;
#19725 = CARTESIAN_POINT ( 'NONE',  ( 10.61868686143207441, -80.99999999999998579, -2.878266372804510809 ) ) ;
#19726 = ORIENTED_EDGE ( 'NONE', *, *, #11880, .T. ) ;
#19727 = CARTESIAN_POINT ( 'NONE',  ( -12.50000000000000000, -55.54999999966999980, -1.250000000000000000 ) ) ;
#19728 = CARTESIAN_POINT ( 'NONE',  ( 3.228614917279000185, -80.84644807899644547, -10.79283437469000084 ) ) ;
#19729 = VECTOR ( 'NONE', #31365, 1000.000000000000000 ) ;
#19730 = CARTESIAN_POINT ( 'NONE',  ( 2.622076063046486993, -78.97800812098877543, -2.767894580093630985 ) ) ;
#19731 = ORIENTED_EDGE ( 'NONE', *, *, #37152, .T. ) ;
#19732 = CARTESIAN_POINT ( 'NONE',  ( -1.182296476285000120, -78.63983461367500638, 0.6170503964917000150 ) ) ;
#19733 = CARTESIAN_POINT ( 'NONE',  ( -2.948156184611000263, -78.70343179000198575, 10.64829886688000116 ) ) ;
#19734 = CARTESIAN_POINT ( 'NONE',  ( 7.421131282012294328, -77.69826720182105362, -5.651170926980095821 ) ) ;
#19735 = CARTESIAN_POINT ( 'NONE',  ( 0.01020306644930230565, -80.72629856499307266, -1.249600794397132564 ) ) ;
#19736 = ORIENTED_EDGE ( 'NONE', *, *, #48653, .F. ) ;
#19737 = CARTESIAN_POINT ( 'NONE',  ( -11.66523904145000046, -78.28174834697500728, -3.450322983582000180 ) ) ;
#19738 = CARTESIAN_POINT ( 'NONE',  ( -4.809507827685000514, -77.21046664206399157, -10.07512781268000168 ) ) ;
#19739 = CARTESIAN_POINT ( 'NONE',  ( -10.98521615365918080, -23.34051012009600612, -0.5703160980903254629 ) ) ;
#19740 = EDGE_LOOP ( 'NONE', ( #14393, #52282, #2260, #49443, #47217, #32045, #13542, #37360, #34909 ) ) ;
#19741 = ORIENTED_EDGE ( 'NONE', *, *, #36346, .T. ) ;
#19742 = VECTOR ( 'NONE', #4578, 1000.000000000000000 ) ;
#19743 = B_SPLINE_CURVE_WITH_KNOTS ( 'NONE', 3,
 ( #28187, #22908, #50372, #22616, #40920, #10208 ),
 .UNSPECIFIED., .F., .F.,
 ( 4, 2, 4 ),
 ( 0.000000000000000000, 0.5000000000000000000, 1.000000000000000000 ),
 .UNSPECIFIED. ) ;
#19744 = CARTESIAN_POINT ( 'NONE',  ( -1.092042939088145648, -80.55956894660957346, 0.6086570842360274902 ) ) ;
#19745 = CARTESIAN_POINT ( 'NONE',  ( 6.606167539452195925, -77.77712013868713825, -8.596032059636364409 ) ) ;
#19746 = CARTESIAN_POINT ( 'NONE',  ( -5.809791519574999619, -79.31614844811198850, 7.851562197947999699 ) ) ;
#19747 = ORIENTED_EDGE ( 'NONE', *, *, #43046, .F. ) ;
#19748 = FACE_OUTER_BOUND ( 'NONE', #14607, .T. ) ;
#19749 = CARTESIAN_POINT ( 'NONE',  ( 3.281228840419999848, -79.22270349199298778, -10.41195962760999905 ) ) ;
#19750 = EDGE_LOOP ( 'NONE', ( #21637, #18491, #46111, #21120 ) ) ;
#19751 = CARTESIAN_POINT ( 'NONE',  ( -12.43646124688000043, -24.91751819622000141, 0.05236837568998999742 ) ) ;
#19752 = CARTESIAN_POINT ( 'NONE',  ( -3.437217408589384515, -78.69999999999998863, -1.942147800595266816 ) ) ;
#19753 = EDGE_CURVE ( 'NONE', #8616, #20811, #28945, .T. ) ;
#19754 = CARTESIAN_POINT ( 'NONE',  ( -0.8249880669573600445, -80.16805825303950428, -0.9389422545057994896 ) ) ;
#19755 = DIRECTION ( 'NONE',  ( -1.308367906941000013E-10, -1.000000000000000000, -3.608117760387000167E-10 ) ) ;
#19756 = CARTESIAN_POINT ( 'NONE',  ( 2.013948389145618467, -78.19072913613844378, -9.514067696212755720 ) ) ;
#19757 = CARTESIAN_POINT ( 'NONE',  ( 2.941330672729000284, -77.07006883366948102, 9.389085009981000596 ) ) ;
#19758 = CARTESIAN_POINT ( 'NONE',  ( -1.275548104907354485, -78.30286137473437691, 0.8563608086819030074 ) ) ;
#19759 = CARTESIAN_POINT ( 'NONE',  ( -0.3693480770463897778, -82.05312501633302702, -4.021025545053856121 ) ) ;
#19760 = CARTESIAN_POINT ( 'NONE',  ( -9.662446363796000526, -76.42949170666001635, 7.627099640079999965 ) ) ;
#19761 = CARTESIAN_POINT ( 'NONE',  ( -9.393203674808267678, -77.54166666666665719, -5.413904038987171319 ) ) ;
#19762 = CARTESIAN_POINT ( 'NONE',  ( -3.272648110252596165, -1.879334845439307067, -1.300867599518198858 ) ) ;
#19763 = CONICAL_SURFACE ( 'NONE', #12214, 0.6999999997695030007, 0.7853981633972997312 ) ;
#19764 = CARTESIAN_POINT ( 'NONE',  ( 10.47840054248000108, -60.58693148419000352, -7.622763498592000531 ) ) ;
#19765 = CARTESIAN_POINT ( 'NONE',  ( -9.356096982537000173, -78.89205726075000769, 7.928589704419000128 ) ) ;
#19766 = CARTESIAN_POINT ( 'NONE',  ( 4.297951556683999641, -76.78734615778300565, -11.50435740523999861 ) ) ;
#19767 = CARTESIAN_POINT ( 'NONE',  ( 12.70249541838869156, -17.03496187198601319, -0.9988462570604047519 ) ) ;
#19768 = EDGE_CURVE ( 'NONE', #31323, #31846, #12915, .T. ) ;
#19769 = CARTESIAN_POINT ( 'NONE',  ( 2.141122524434464047, -2.783241521950269526, -2.454054550522687617 ) ) ;
#19770 = CARTESIAN_POINT ( 'NONE',  ( -2.676544870374850227, -77.44274814402791662, 11.77617227856609716 ) ) ;
#19771 = CARTESIAN_POINT ( 'NONE',  ( 6.766402264611000028, -79.42653081578252738, -8.946167390840999545 ) ) ;
#19772 = ORIENTED_EDGE ( 'NONE', *, *, #22178, .T. ) ;
#19773 = CARTESIAN_POINT ( 'NONE',  ( 0.6721823118158000154, -81.85354343447998815, 1.172239651246999914 ) ) ;
#19774 = CARTESIAN_POINT ( 'NONE',  ( 2.291826089449000126, -77.03724721216990190, -9.321303964228999206 ) ) ;
#19775 = CARTESIAN_POINT ( 'NONE',  ( 9.433548213854539455, -25.12797454612102754, 8.532643227186095913 ) ) ;
#19776 = AXIS2_PLACEMENT_3D ( 'NONE', #10143, #11310, #34298 ) ;
#19777 = CARTESIAN_POINT ( 'NONE',  ( 0.7681833999686413783, -78.82291666666668561, 0.9995835529977274980 ) ) ;
#19778 = CARTESIAN_POINT ( 'NONE',  ( 3.699199734595000066, -3.138587262671999945, 0.3322231105728999934 ) ) ;
#19779 = CIRCLE ( 'NONE', #13178, 0.6000000000000008660 ) ;
#19780 = CARTESIAN_POINT ( 'NONE',  ( 11.05834404496999923, -78.79136917884000013, 4.786306364259000468 ) ) ;
#19781 = CARTESIAN_POINT ( 'NONE',  ( -9.316314781052998484, -77.29436066386098503, -2.840095070410999956 ) ) ;
#19782 = EDGE_CURVE ( 'NONE', #51555, #31846, #18418, .T. ) ;
#19784 = CARTESIAN_POINT ( 'NONE',  ( -9.834111732579202680, -77.73812671110431438, -5.101590220333413583 ) ) ;
#19783 = CARTESIAN_POINT ( 'NONE',  ( -10.04720586219557177, -76.15599413331796086, 6.103539320034618854 ) ) ;
#19785 = CARTESIAN_POINT ( 'NONE',  ( -1.266615395500999997, -82.10834473437999748, -0.4708042714212999913 ) ) ;
#19786 = CARTESIAN_POINT ( 'NONE',  ( -10.54577208822472834, -79.58458823469565857, 2.085048453671053181 ) ) ;
#19787 = EDGE_LOOP ( 'NONE', ( #24734, #55684, #30173, #42602 ) ) ;
#19788 = CARTESIAN_POINT ( 'NONE',  ( 12.76303204522000101, -23.26485147686999966, 1.980584515753000208 ) ) ;
#19789 = EDGE_CURVE ( 'NONE', #8017, #4894, #13491, .T. ) ;
#19790 = CARTESIAN_POINT ( 'NONE',  ( -1.980584515756000030, -60.06485150062000145, -12.76303204342999997 ) ) ;
#19791 = DIRECTION ( 'NONE',  ( -1.000000000000000000, 0.000000000000000000, 0.000000000000000000 ) ) ;
#19792 = CARTESIAN_POINT ( 'NONE',  ( -3.673218652927999539, -79.39261068610500161, 10.34270183798999909 ) ) ;
#19793 = CYLINDRICAL_SURFACE ( 'NONE', #8169, 1.500000000000000000 ) ;
#19794 = CARTESIAN_POINT ( 'NONE',  ( -9.029190506544999550, -79.10582576494698515, -3.140825197024999849 ) ) ;
#19795 = CARTESIAN_POINT ( 'NONE',  ( 7.657744736620999859, -18.33080421803999727, -9.966195456754999071 ) ) ;
#19796 = CARTESIAN_POINT ( 'NONE',  ( 8.179400486892387079, -17.25908162455774075, 9.502921779304051242 ) ) ;
#19797 = VERTEX_POINT ( 'NONE', #31481 ) ;
#19798 = CARTESIAN_POINT ( 'NONE',  ( -7.330610599118999815, -79.20799394121699777, 8.549626471514999437 ) ) ;
#19799 = CARTESIAN_POINT ( 'NONE',  ( 10.97853902630967937, -76.08461633803946711, -2.133057381744011938 ) ) ;
#19800 = CARTESIAN_POINT ( 'NONE',  ( -11.58850405216667667, -79.03337548462275208, 2.406487868672887664 ) ) ;
#19801 = CARTESIAN_POINT ( 'NONE',  ( -2.060840846990595221, -78.54828564506389910, 3.417916694071717387 ) ) ;
#19802 = CARTESIAN_POINT ( 'NONE',  ( -4.144949124996972323, -77.55034540772489038, -11.57804869542019155 ) ) ;
#19803 = CARTESIAN_POINT ( 'NONE',  ( 0.8303084959499684725, -81.41757219168246706, 0.9342352573978692787 ) ) ;
#19804 = AXIS2_PLACEMENT_3D ( 'NONE', #31492, #49539, #44807 ) ;
#19805 = CARTESIAN_POINT ( 'NONE',  ( 0.1730703278797017797, -78.28605927411624066, -1.262361427074957687 ) ) ;
#19806 = CARTESIAN_POINT ( 'NONE',  ( -8.033785430678635819, -76.99999999999998579, -4.895566815014301909 ) ) ;
#19807 = CARTESIAN_POINT ( 'NONE',  ( -11.05000000000000071, -76.00000000000000000, 0.000000000000000000 ) ) ;
#19808 = B_SPLINE_CURVE_WITH_KNOTS ( 'NONE', 3,
 ( #11101, #28491, #46832, #24375, #14333, #46245, #23780, #27906, #28786, #55372, #24666, #10213, #45952, #42674, #1087, #38233, #32330, #23489 ),
 .UNSPECIFIED., .F., .F.,
 ( 4, 2, 2, 2, 2, 2, 2, 2, 4 ),
 ( 0.000000000000000000, 0.1250000000000000833, 0.2500000000000001110, 0.3750000000000000000, 0.4999999999999999445, 0.6249999999999998890, 0.7499999999999997780, 0.8749999999999998890, 1.000000000000000000 ),
 .UNSPECIFIED. ) ;
#19809 = EDGE_CURVE ( 'NONE', #30476, #55619, #13483, .T. ) ;
#19810 = CARTESIAN_POINT ( 'NONE',  ( -0.9836304129562999377, -79.07916002803999334, 1.026102791697000027 ) ) ;
#19811 = CYLINDRICAL_SURFACE ( 'NONE', #6669, 5.000000000000000000 ) ;
#19812 = CARTESIAN_POINT ( 'NONE',  ( 10.28119625626286116, -78.22856391619605176, 3.842492908960651210 ) ) ;
#19813 = CARTESIAN_POINT ( 'NONE',  ( -6.234243430155317789, -79.72916666666543506, -6.929937226105533199 ) ) ;
#19814 = VERTEX_POINT ( 'NONE', #49824 ) ;
#19815 = ORIENTED_EDGE ( 'NONE', *, *, #22742, .F. ) ;
#19816 = CARTESIAN_POINT ( 'NONE',  ( 3.168421713927999761, -77.47183533742300199, -12.18315494261000076 ) ) ;
#19817 = CARTESIAN_POINT ( 'NONE',  ( 8.368138856150174831, -78.79614046870541699, -6.748098975523931564 ) ) ;
#19818 = AXIS2_PLACEMENT_3D ( 'NONE', #48482, #24881, #15731 ) ;
#19819 = ORIENTED_EDGE ( 'NONE', *, *, #16660, .F. ) ;
#19820 = CARTESIAN_POINT ( 'NONE',  ( 10.08162962782999905, -17.28146287379999890, 7.981572332336000386 ) ) ;
#19821 = AXIS2_PLACEMENT_3D ( 'NONE', #45312, #45011, #27853 ) ;
#19822 = CARTESIAN_POINT ( 'NONE',  ( -0.7554284705563540925, -80.31666666666664867, 1.310679582531384391 ) ) ;
#19823 = CARTESIAN_POINT ( 'NONE',  ( 7.880031981693000454, -79.23622702059999767, 8.980504559447000545 ) ) ;
#19824 = CARTESIAN_POINT ( 'NONE',  ( 9.783241737811998462, -61.33564621498000946, 7.961026681588999843 ) ) ;
#19825 = CARTESIAN_POINT ( 'NONE',  ( -7.654125837341301697, -77.12040900012513589, -9.499792065586241563 ) ) ;
#19826 = CARTESIAN_POINT ( 'NONE',  ( -1.835150331438888616, -77.93714178660536618, 11.83859006001563507 ) ) ;
#19827 = CARTESIAN_POINT ( 'NONE',  ( -11.04065564778000130, -79.31977030723999178, 1.980412446595999798 ) ) ;
#19828 = ORIENTED_EDGE ( 'NONE', *, *, #38046, .T. ) ;
#19829 = CARTESIAN_POINT ( 'NONE',  ( 11.09211448529823762, -78.07761170217334268, 4.008287385160122618 ) ) ;
#19830 = EDGE_LOOP ( 'NONE', ( #25642, #25660, #23228 ) ) ;
#19831 = CARTESIAN_POINT ( 'NONE',  ( 8.796562682441143366, -77.37506290377116613, 2.860481962223264230 ) ) ;
#19832 = CARTESIAN_POINT ( 'NONE',  ( -7.803971648336165856, -78.28613751752133965, 8.057272210502093301 ) ) ;
#19833 = CARTESIAN_POINT ( 'NONE',  ( 0.2526653223220000632, -78.35443884410990734, 1.594795962155999947 ) ) ;
#19834 = DIRECTION ( 'NONE',  ( 0.000000000000000000, 1.000000000000000000, 0.000000000000000000 ) ) ;
#19835 = DIRECTION ( 'NONE',  ( 1.000000000000000000, 0.000000000000000000, 0.000000000000000000 ) ) ;
#19836 = CARTESIAN_POINT ( 'NONE',  ( -0.7004323366084000968, -78.47841931153999440, -1.469032877812000093 ) ) ;
#19837 = CARTESIAN_POINT ( 'NONE',  ( 0.1299632413661999941, -79.36712607287400090, 11.04812215732000169 ) ) ;
#19838 = EDGE_CURVE ( 'NONE', #11618, #26528, #27061, .T. ) ;
#19839 = CARTESIAN_POINT ( 'NONE',  ( 0.000000000000000000, -81.00000000000000000, 0.000000000000000000 ) ) ;
#19840 = CARTESIAN_POINT ( 'NONE',  ( -7.657745562908000458, -23.66920625126000033, -9.966193613329998868 ) ) ;
#19841 = CARTESIAN_POINT ( 'NONE',  ( -0.9999999970759999579, -75.20000000292399989, -7.200000017194999380 ) ) ;
#19842 = CARTESIAN_POINT ( 'NONE',  ( 0.2671681181389000126, -82.81955637232998413, 3.536976524314999981 ) ) ;
#19843 = AXIS2_PLACEMENT_3D ( 'NONE', #26777, #53963, #35633 ) ;
#19844 = ORIENTED_EDGE ( 'NONE', *, *, #9778, .F. ) ;
#19845 = ADVANCED_FACE ( 'NONE', ( #6098, #41829 ), #32652, .T. ) ;
#19846 = CARTESIAN_POINT ( 'NONE',  ( -5.768141930173999121, -78.78679903547799768, 11.01445829398999798 ) ) ;
#19847 = CARTESIAN_POINT ( 'NONE',  ( 1.505228744355000092, -80.54130269966999833, -0.7963060858757999849 ) ) ;
#19848 = FACE_BOUND ( 'NONE', #49983, .T. ) ;
#19849 = CARTESIAN_POINT ( 'NONE',  ( 11.95248949435000085, -78.82148205457200163, 0.8087524912306001124 ) ) ;
#19850 = CARTESIAN_POINT ( 'NONE',  ( -7.758650587948999977, -17.84922688128999724, 9.996717134846999642 ) ) ;
#19851 = CARTESIAN_POINT ( 'NONE',  ( -0.5951243518625245477, -78.16363383461164460, 1.127832697537623829 ) ) ;
#19852 = CARTESIAN_POINT ( 'NONE',  ( -3.265816405937842060, -3.219552046736191553, 1.312226571638672512 ) ) ;
#19853 = CARTESIAN_POINT ( 'NONE',  ( -0.8481231068849000021, -79.07210584965399391, 9.686304223355000076 ) ) ;
#19854 = CARTESIAN_POINT ( 'NONE',  ( 0.8359750594766999221, -78.21126277754198952, -9.376158072868999938 ) ) ;
#19855 = FACE_OUTER_BOUND ( 'NONE', #1242, .T. ) ;
#19856 = CARTESIAN_POINT ( 'NONE',  ( 8.921077980507002181, -78.25891109057499762, 6.489691983999000158 ) ) ;
#19857 = CARTESIAN_POINT ( 'NONE',  ( 7.144724566336000393, -76.47558639178819817, 9.988770583665001368 ) ) ;
#19858 = CARTESIAN_POINT ( 'NONE',  ( -3.014980776116999994, -80.62931084346850241, -10.48587037275000000 ) ) ;
#19859 = ORIENTED_EDGE ( 'NONE', *, *, #3816, .T. ) ;
#19860 = CARTESIAN_POINT ( 'NONE',  ( 1.316231252753000014, -81.98475626391700644, 0.2147359707272000207 ) ) ;
#19861 = CARTESIAN_POINT ( 'NONE',  ( 1.798954018877999994, -60.01530973353999343, -12.61117007304000026 ) ) ;
#19862 = EDGE_CURVE ( 'NONE', #26523, #3682, #149, .T. ) ;
#19863 = CARTESIAN_POINT ( 'NONE',  ( 10.75000000000000000, -80.34999999999999432, 0.000000000000000000 ) ) ;
#19864 = CARTESIAN_POINT ( 'NONE',  ( -3.633103876188000125, -77.16735396267098679, 10.61219425078000000 ) ) ;
#19865 = CARTESIAN_POINT ( 'NONE',  ( -7.022507694776999543, -79.23979426342499721, 8.434951230355999030 ) ) ;
#19866 = CARTESIAN_POINT ( 'NONE',  ( 0.000000000000000000, -80.49999999999998579, -5.000000000000000000 ) ) ;
#19867 = CARTESIAN_POINT ( 'NONE',  ( -1.587910676672080967, -83.47916665808423886, -3.726481291835321841 ) ) ;
#19868 = CARTESIAN_POINT ( 'NONE',  ( -7.695965602004000594, -76.50616330962898815, 9.405193249304000247 ) ) ;
#19869 = LINE ( 'NONE', #32250, #21915 ) ;
#19870 = VERTEX_POINT ( 'NONE', #34623 ) ;
#19871 = TOROIDAL_SURFACE ( 'NONE', #3779, 12.50000000000000000, 1.500000000000000000 ) ;
#19872 = CARTESIAN_POINT ( 'NONE',  ( -0.4360978520027915528, -80.00346707738961527, 1.172260374082638945 ) ) ;
#19873 = AXIS2_PLACEMENT_3D ( 'NONE', #35663, #26230, #43965 ) ;
#19874 = CARTESIAN_POINT ( 'NONE',  ( 1.500000000000000888, -79.73958333333334281, -0.1963495408493590444 ) ) ;
#19875 = CARTESIAN_POINT ( 'NONE',  ( 7.634437838894000627, -55.05219468418000162, -10.30764259108000225 ) ) ;
#19876 = CARTESIAN_POINT ( 'NONE',  ( 11.13061814830999907, -77.01442077791699603, -1.715606072514000102 ) ) ;
#19877 = CARTESIAN_POINT ( 'NONE',  ( -0.9131908197385000259, -81.40406183460000022, -1.254418330386999791 ) ) ;
#19878 = CARTESIAN_POINT ( 'NONE',  ( -1.186038146469999832, -79.55615654513999857, -0.5797594326791000174 ) ) ;
#19879 = CARTESIAN_POINT ( 'NONE',  ( 1.570796326794857478, -77.66458333333333997, 12.00000000000000533 ) ) ;
#19880 = CARTESIAN_POINT ( 'NONE',  ( 1.023096227096927491, -81.93418301853687069, -1.110676516153182414 ) ) ;
#19881 = CARTESIAN_POINT ( 'NONE',  ( -1.215509798056741531, -83.29877716300683232, 0.8975879569896133559 ) ) ;
#19882 = CARTESIAN_POINT ( 'NONE',  ( 1.243547092045970581, -77.93541666666665435, -9.500000000000000000 ) ) ;
#19883 = CARTESIAN_POINT ( 'NONE',  ( -0.3277658534251963740, -80.99651576041503631, 1.218475390182661711 ) ) ;
#19884 = VERTEX_POINT ( 'NONE', #52370 ) ;
#19885 = CARTESIAN_POINT ( 'NONE',  ( -0.4528890155571457798, -81.69566638204462095, -1.164992333293775051 ) ) ;
#19886 = CARTESIAN_POINT ( 'NONE',  ( -10.53927088184999938, -79.93499373684079501, 3.259678459687000096 ) ) ;
#19887 = CARTESIAN_POINT ( 'NONE',  ( -0.5999999999999999778, -23.15000000000000213, -10.98362417419999915 ) ) ;
#19888 = EDGE_LOOP ( 'NONE', ( #52818, #31398, #30947, #47282 ) ) ;
#19889 = EDGE_LOOP ( 'NONE', ( #8596, #36656, #16402, #54349 ) ) ;
#19890 = AXIS2_PLACEMENT_3D ( 'NONE', #40017, #45056, #17592 ) ;
#19892 = B_SPLINE_CURVE_WITH_KNOTS ( 'NONE', 3,
 ( #43228, #52379, #30203, #48249, #7786, #52948, #48525, #43813, #33769, #51808, #11365, #16074, #47386, #6918, #24925, #42943 ),
 .UNSPECIFIED., .F., .F.,
 ( 4, 2, 2, 2, 2, 2, 2, 4 ),
 ( 0.000000000000000000, 0.08929374297993872278, 0.1785874859598774456, 0.2678812289398161406, 0.3571749719197548911, 0.4464687148996936417, 0.5357624578796322812, 0.7143499438395097823 ),
 .UNSPECIFIED. ) ;
#19891 = CARTESIAN_POINT ( 'NONE',  ( -1.501972381289000014, -82.05824652816899345, -0.2076389427764999962 ) ) ;
#19893 = ORIENTED_EDGE ( 'NONE', *, *, #54006, .T. ) ;
#19895 = ADVANCED_FACE ( 'NONE', ( #42640, #3350 ), #21346, .T. ) ;
#19894 = VERTEX_POINT ( 'NONE', #25200 ) ;
#19896 = CARTESIAN_POINT ( 'NONE',  ( -0.8445585116437001050, -17.28959556757000016, 12.43380736237000050 ) ) ;
#19897 = CARTESIAN_POINT ( 'NONE',  ( 0.000000000000000000, -74.64999999999999147, 0.000000000000000000 ) ) ;
#19898 = APPLICATION_PROTOCOL_DEFINITION ( 'draft international standard', 'automotive_design', 1998, #14927 ) ;
#19899 = CARTESIAN_POINT ( 'NONE',  ( 0.9218200799623742503, -78.17708333333332860, -1.199500263597268912 ) ) ;
#19900 = CARTESIAN_POINT ( 'NONE',  ( 1.958352037450999727, -78.68001001420199714, 9.829161269560000136 ) ) ;
#19901 = CARTESIAN_POINT ( 'NONE',  ( 7.109588333167061514, -78.29483705384265591, -5.917559077586919791 ) ) ;
#19902 = CARTESIAN_POINT ( 'NONE',  ( 11.21485848424000054, -79.94681080473810653, -0.2123177049684000228 ) ) ;
#19903 = ORIENTED_EDGE ( 'NONE', *, *, #24024, .T. ) ;
#19904 = ORIENTED_EDGE ( 'NONE', *, *, #56554, .F. ) ;
#19905 = CARTESIAN_POINT ( 'NONE',  ( -9.079656017920873623, -77.58448292774525612, 1.803135903180888899 ) ) ;
#19906 = CIRCLE ( 'NONE', #22753, 3.000000000000000000 ) ;
#19907 = CARTESIAN_POINT ( 'NONE',  ( 0.000000000000000000, -75.09999999979599750, 0.000000000000000000 ) ) ;
#19908 = CARTESIAN_POINT ( 'NONE',  ( 10.10565965529137422, -76.05000000000001137, -4.494725398901759483 ) ) ;
#19909 = VECTOR ( 'NONE', #32943, 1000.000000000000000 ) ;
#19910 = CARTESIAN_POINT ( 'NONE',  ( 2.867548251969000095, -77.91871983068898544, -9.270807752789000489 ) ) ;
#19911 = CARTESIAN_POINT ( 'NONE',  ( 9.760776772971999193, -92.33215535459000023, 3.252741292258000451E-10 ) ) ;
#19912 = DIRECTION ( 'NONE',  ( 0.000000000000000000, 1.000000000000000000, 0.000000000000000000 ) ) ;
#19913 = CARTESIAN_POINT ( 'NONE',  ( 7.374560639698954922, -76.72291666666664867, 9.596002108778179718 ) ) ;
#19914 = CARTESIAN_POINT ( 'NONE',  ( -0.5839839591423000575, -79.36543996570000559, -1.474617623361999863 ) ) ;
#19915 = CARTESIAN_POINT ( 'NONE',  ( -8.061017305527000687, -59.94999999967000548, 8.909545442949999838 ) ) ;
#19916 = CARTESIAN_POINT ( 'NONE',  ( -7.593391408704848189, -76.63053360682752668, 8.968398750625850013 ) ) ;
#19917 = ADVANCED_FACE ( 'NONE', ( #34907 ), #2207, .F. ) ;
#19918 = FACE_OUTER_BOUND ( 'NONE', #32713, .T. ) ;
#19919 = CARTESIAN_POINT ( 'NONE',  ( 1.290219381540931742, -79.54546911372847262, 0.8289380708588135471 ) ) ;
#19920 = CARTESIAN_POINT ( 'NONE',  ( 2.253288347564000205, -79.08636332859900619, -9.650850687256999905 ) ) ;
#19921 = CARTESIAN_POINT ( 'NONE',  ( 7.374560639698954922, -77.22291666666666288, 9.596002108778179718 ) ) ;
#19922 = DIRECTION ( 'NONE',  ( 0.7071067811864966135, 0.7071067811865965336, 5.001433494089977624E-08 ) ) ;
#19924 = CARTESIAN_POINT ( 'NONE',  ( 1.758095523367999791, -18.27708336119999899, -12.57362173515999970 ) ) ;
#19923 = CARTESIAN_POINT ( 'NONE',  ( 1.199500263597268246, -78.70208333333333428, 0.9218200799623752495 ) ) ;
#19925 = CARTESIAN_POINT ( 'NONE',  ( -11.68767212001980127, -78.37916666666666288, 3.140974612311317138 ) ) ;
#19926 = DIRECTION ( 'NONE',  ( 0.000000000000000000, -0.7071067811864425456, 0.7071067811866525998 ) ) ;
#19927 = FACE_OUTER_BOUND ( 'NONE', #10600, .T. ) ;
#19928 = CARTESIAN_POINT ( 'NONE',  ( -3.180605150700375638, -1.214306347645720985, 1.530408170426506897 ) ) ;
#19929 = ORIENTED_EDGE ( 'NONE', *, *, #48693, .F. ) ;
#19930 = CARTESIAN_POINT ( 'NONE',  ( -6.760013919724056741, -78.27291666666666003, -8.796335266379987416 ) ) ;
#19931 = DIRECTION ( 'NONE',  ( 0.7071067811865475727, 0.000000000000000000, 0.7071067811865475727 ) ) ;
#19932 = CARTESIAN_POINT ( 'NONE',  ( -6.760013919724083387, -79.12708333333333144, 8.796335266379969653 ) ) ;
#19933 = CARTESIAN_POINT ( 'NONE',  ( 0.7167766847591896529, -78.42666800608485289, 1.023989290741913694 ) ) ;
#19934 = ADVANCED_FACE ( 'NONE', ( #51798 ), #22932, .F. ) ;
#19935 = VECTOR ( 'NONE', #47203, 1000.000000000000114 ) ;
#19936 = CARTESIAN_POINT ( 'NONE',  ( 9.531612390470000307, -79.15514289792399438, 1.458175310291999871 ) ) ;
#19937 = CARTESIAN_POINT ( 'NONE',  ( -1.189541931187000134, -77.06571553208000580, -12.95855809378999979 ) ) ;
#19938 = CARTESIAN_POINT ( 'NONE',  ( -1.489475662155156366, -79.46257339460650826, -9.601386891029047632 ) ) ;
#19939 = CARTESIAN_POINT ( 'NONE',  ( -1.242042303480714205, -79.48436884964252158, 10.67792447292398705 ) ) ;
#19940 = CARTESIAN_POINT ( 'NONE',  ( 8.654165682147999306, -79.16893998579799074, 4.701175118119000018 ) ) ;
#19941 = CARTESIAN_POINT ( 'NONE',  ( -9.500000000000000000, -77.39999999999999147, 0.000000000000000000 ) ) ;
#19942 = CARTESIAN_POINT ( 'NONE',  ( -5.700319242863999492, -77.22504179105499134, 9.473880686520999461 ) ) ;
#19943 = CARTESIAN_POINT ( 'NONE',  ( -0.9157810684381340049, -76.31873599581450662, -11.71594503368780771 ) ) ;
#19944 = CARTESIAN_POINT ( 'NONE',  ( -1.355217461342999918, -80.94787865541199778, -0.7366976956675999055 ) ) ;
#19945 = CARTESIAN_POINT ( 'NONE',  ( 5.100000000000000533, -75.20000000000000284, 0.000000000000000000 ) ) ;
#19946 = VECTOR ( 'NONE', #56132, 1000.000000000000000 ) ;
#19947 = CARTESIAN_POINT ( 'NONE',  ( -9.338489578732000140, -78.51077085424698510, 1.184823571421999899 ) ) ;
#19949 = CARTESIAN_POINT ( 'NONE',  ( 1.636761686205415067, -2.833333333333333481, 2.839805762151342616 ) ) ;
#19948 = CARTESIAN_POINT ( 'NONE',  ( -0.7078687434456000238, -84.06554135855498089, 3.689212947271000242 ) ) ;
#19950 = CARTESIAN_POINT ( 'NONE',  ( -8.630067035710000667, -79.66535194988499313, -4.100810385846999750 ) ) ;
#19951 = CARTESIAN_POINT ( 'NONE',  ( -0.9218200799623778030, -80.82708333333336270, 1.199500263597266914 ) ) ;
#19952 = CARTESIAN_POINT ( 'NONE',  ( 8.165383881631132823, -80.29366675105114837, -6.993337379266368004 ) ) ;
#19953 = CARTESIAN_POINT ( 'NONE',  ( -7.580572135914469101, -77.16272471331792815, -7.622152899789345959 ) ) ;
#19954 = DIRECTION ( 'NONE',  ( -7.037892281487000491E-12, 1.000000000000000000, 4.198156442306999976E-10 ) ) ;
#19955 = VECTOR ( 'NONE', #37089, 1000.000000000000114 ) ;
#19956 = PRODUCT_RELATED_PRODUCT_CATEGORY ( 'part', '', ( #38457 ) ) ;
#19957 = VERTEX_POINT ( 'NONE', #38777 ) ;
#19958 = VERTEX_POINT ( 'NONE', #11353 ) ;
#19959 = CARTESIAN_POINT ( 'NONE',  ( -5.246265831776000255, -79.72298241822798559, -10.82514862071000117 ) ) ;
#19960 = FACE_OUTER_BOUND ( 'NONE', #57007, .T. ) ;
#19961 = DIRECTION ( 'NONE',  ( -1.000000000000000000, 0.000000000000000000, 0.000000000000000000 ) ) ;
#19962 = EDGE_LOOP ( 'NONE', ( #45309, #14644, #16189, #12466 ) ) ;
#19963 = CARTESIAN_POINT ( 'NONE',  ( -5.666254562607999645, -78.03777695645399604, 10.50376416711000083 ) ) ;
#19964 = ORIENTED_EDGE ( 'NONE', *, *, #32479, .T. ) ;
#19966 = ADVANCED_FACE ( 'NONE', ( #16355 ), #25487, .F. ) ;
#19965 = ORIENTED_EDGE ( 'NONE', *, *, #22057, .T. ) ;
#19967 = CARTESIAN_POINT ( 'NONE',  ( -10.07627163191000008, -18.75000000310999937, -7.601397897754999633 ) ) ;
#19968 = ORIENTED_EDGE ( 'NONE', *, *, #1247, .F. ) ;
#19969 = EDGE_CURVE ( 'NONE', #13072, #17378, #20493, .T. ) ;
#19970 = CARTESIAN_POINT ( 'NONE',  ( -3.412678419678000008, -78.64724969135635035, 0.4937240612773000636 ) ) ;
#19971 = CARTESIAN_POINT ( 'NONE',  ( 8.972094814454390388, -79.17629006715765172, 3.124824076624122871 ) ) ;
#19972 = ORIENTED_EDGE ( 'NONE', *, *, #27381, .T. ) ;
#19973 = CARTESIAN_POINT ( 'NONE',  ( 0.4636642495210216430, -82.75527458966378447, -1.160904140311521227 ) ) ;
#19974 = VERTEX_POINT ( 'NONE', #34046 ) ;
#19975 = CARTESIAN_POINT ( 'NONE',  ( -7.668949790015999746, -59.57129148919000272, 10.21381326473999884 ) ) ;
#19976 = ORIENTED_EDGE ( 'NONE', *, *, #6625, .F. ) ;
#19977 = CARTESIAN_POINT ( 'NONE',  ( 4.635655000267153270, -79.26679008495354140, -8.026958512551585656 ) ) ;
#19978 = CARTESIAN_POINT ( 'NONE',  ( -1.260816076409378761, -78.29616218522681947, -0.8268161317517029874 ) ) ;
#19979 = CARTESIAN_POINT ( 'NONE',  ( 11.15514985639044276, -79.79999999999998295, 3.879996556239171834 ) ) ;
#19980 = CARTESIAN_POINT ( 'NONE',  ( 12.70556836347999941, -25.22772277227999993, 2.424222353299999887E-09 ) ) ;
#19981 = CARTESIAN_POINT ( 'NONE',  ( 3.343750000583999960, -0.9062499994161000716, -3.925818329445000231E-08 ) ) ;
#19982 = CARTESIAN_POINT ( 'NONE',  ( -1.182190922889000184, -78.86528195922576856, -9.631881180458998770 ) ) ;
#19983 = CARTESIAN_POINT ( 'NONE',  ( -7.695020077040999773, -76.26927865530500128, 8.115451295621999961 ) ) ;
#19984 = CARTESIAN_POINT ( 'NONE',  ( 10.38093530541932985, -76.32946667606279334, -2.901028463810237490 ) ) ;
#19985 = CARTESIAN_POINT ( 'NONE',  ( -1.487911162517577823, -81.33517288243102428, 0.2674502543427375034 ) ) ;
#19986 = CARTESIAN_POINT ( 'NONE',  ( -7.653559502293999728, -60.09849137195000424, -10.01234990230000044 ) ) ;
#19987 = CARTESIAN_POINT ( 'NONE',  ( -5.529498250248094493, -78.67420770746792869, -7.421320449266156416 ) ) ;
#19988 = CARTESIAN_POINT ( 'NONE',  ( 4.120651084761334459, -76.54600812598258130, 11.01093787941378643 ) ) ;
#19989 = EDGE_CURVE ( 'NONE', #47619, #28634, #37438, .T. ) ;
#19990 = CARTESIAN_POINT ( 'NONE',  ( 0.3292142484335000563, -79.32296227407599076, -1.292352404326999826 ) ) ;
#19991 = CARTESIAN_POINT ( 'NONE',  ( -7.516303886515633970, -80.16556818807158891, -8.031330139908581245 ) ) ;
#19992 = CARTESIAN_POINT ( 'NONE',  ( -3.024915515467232474, -3.071593521866582410, 1.186391032666482825 ) ) ;
#19993 = CARTESIAN_POINT ( 'NONE',  ( 0.8348061542621000308, -80.96678455456799384, 3.662575701359999769 ) ) ;
#19994 = CARTESIAN_POINT ( 'NONE',  ( -7.318775999449999681, -79.58266715040700490, -9.761385579090999798 ) ) ;
#19995 = AXIS2_PLACEMENT_3D ( 'NONE', #34154, #56331, #32995 ) ;
#19996 = CARTESIAN_POINT ( 'NONE',  ( -8.368009042705715217, -78.04613955777109879, 6.748258816816721684 ) ) ;
#19997 = CARTESIAN_POINT ( 'NONE',  ( -0.4803308748150663110, -83.00644942323957309, 1.153985611485086160 ) ) ;
#19998 =( LENGTH_UNIT ( ) NAMED_UNIT ( * ) SI_UNIT ( .MILLI., .METRE. ) );
#19999 = CARTESIAN_POINT ( 'NONE',  ( -3.399999999999689937, -78.72609999968184979, -1.426627331148062801E-14 ) ) ;
#20000 = DIRECTION ( 'NONE',  ( 0.000000000000000000, 1.000000000000000000, 0.000000000000000000 ) ) ;
#20001 = CARTESIAN_POINT ( 'NONE',  ( 6.233047529871999615, -78.98050366622999263, 9.960502923565000444 ) ) ;
#20002 = CARTESIAN_POINT ( 'NONE',  ( -10.36221643470000053, -60.02123873632999818, -7.631895748967999715 ) ) ;
#20003 = CARTESIAN_POINT ( 'NONE',  ( 0.2613843059707509631, -3.500000000000000000, 3.291795858360297977 ) ) ;
#20004 = EDGE_CURVE ( 'NONE', #313, #26598, #55340, .T. ) ;
#20005 = CARTESIAN_POINT ( 'NONE',  ( 10.53101998748999968, -60.10639625617000092, 7.613962827198000660 ) ) ;
#20006 = B_SPLINE_CURVE_WITH_KNOTS ( 'NONE', 3,
 ( #4528, #423, #22528, #26357, #45272, #36104, #21648, #44972, #4229, #35800, #39939, #54121, #13662, #3645, #35499, #13069, #57660, #40538 ),
 .UNSPECIFIED., .F., .F.,
 ( 4, 2, 2, 2, 2, 2, 2, 2, 4 ),
 ( 0.000000000000000000, 0.1250000000000001110, 0.2500000000000001665, 0.3750000000000001665, 0.5000000000000001110, 0.6250000000000001110, 0.7500000000000001110, 0.8750000000000001110, 1.000000000000000000 ),
 .UNSPECIFIED. ) ;
#20008 = ADVANCED_FACE ( 'NONE', ( #52084 ), #20776, .F. ) ;
#20007 = CARTESIAN_POINT ( 'NONE',  ( 0.7554284705563509839, -80.56666666666664867, -1.310679582531386167 ) ) ;
#20009 = CARTESIAN_POINT ( 'NONE',  ( 12.77302471391999994, -24.72230123305000049, 1.481949986259999852 ) ) ;
#20010 = CARTESIAN_POINT ( 'NONE',  ( 5.542538650459465366, -77.61846143728747904, -9.237786168586172408 ) ) ;
#20011 = CARTESIAN_POINT ( 'NONE',  ( 11.67610687481217902, -78.43638509158282091, -1.539212210575771067 ) ) ;
#20012 = CARTESIAN_POINT ( 'NONE',  ( -4.399243655502999673, -79.75781822728644954, 10.05537673064999993 ) ) ;
#20013 = CARTESIAN_POINT ( 'NONE',  ( -11.96865137734000051, -76.26552026400000273, -1.496560055186000104 ) ) ;
#20014 = ORIENTED_EDGE ( 'NONE', *, *, #53083, .T. ) ;
#20015 = CARTESIAN_POINT ( 'NONE',  ( 2.260331847164999797, -82.87507450217398741, 3.456781180494999717 ) ) ;
#20016 = CARTESIAN_POINT ( 'NONE',  ( -4.413100828165999800, -80.04845022661349674, 10.26392002655999924 ) ) ;
#20017 = DIRECTION ( 'NONE',  ( 1.000000000000000000, 0.000000000000000000, 0.000000000000000000 ) ) ;
#20018 = CARTESIAN_POINT ( 'NONE',  ( 8.343860018000999190, -59.94999999967000548, -8.343860018000999190 ) ) ;
#20019 = CARTESIAN_POINT ( 'NONE',  ( 11.08595418830999968, -77.13951301121200288, -1.708721840212999998 ) ) ;
#20020 = CARTESIAN_POINT ( 'NONE',  ( -1.931086388578000079, -18.70221245812999911, -12.71798269385000069 ) ) ;
#20021 = CARTESIAN_POINT ( 'NONE',  ( -5.177883096403999907, -77.40958109976999424, -8.249196342081999589 ) ) ;
#20022 = CARTESIAN_POINT ( 'NONE',  ( -1.462746796095000024, -81.34738048770999796, -0.3322225316158000097 ) ) ;
#20023 = LINE ( 'NONE', #42163, #51977 ) ;
#20024 = CARTESIAN_POINT ( 'NONE',  ( -1.356492273396000092, -79.03756650451100541, -0.8757286844311999996 ) ) ;
#20025 = ORIENTED_EDGE ( 'NONE', *, *, #52839, .F. ) ;
#20026 = DIRECTION ( 'NONE',  ( 0.000000000000000000, 1.000000000000000000, -1.657933050107000062E-13 ) ) ;
#20027 = ADVANCED_FACE ( 'NONE', ( #49685 ), #53476, .F. ) ;
#20028 = CARTESIAN_POINT ( 'NONE',  ( -3.116622985464775564, -78.75135162752194162, -1.413773745829535411 ) ) ;
#20029 = ORIENTED_EDGE ( 'NONE', *, *, #26108, .T. ) ;
#20030 = CARTESIAN_POINT ( 'NONE',  ( -0.9612450871864000046, -78.69528584285799866, -0.9244371432244999909 ) ) ;
#20031 = CARTESIAN_POINT ( 'NONE',  ( 7.840491480036000382, -78.61915472700400187, 7.784894796889999746 ) ) ;
#20032 = CARTESIAN_POINT ( 'NONE',  ( 11.39907318373000145, -79.91618549011299422, -1.879061223299000050 ) ) ;
#20033 = ORIENTED_EDGE ( 'NONE', *, *, #10718, .T. ) ;
#20034 = CARTESIAN_POINT ( 'NONE',  ( 11.16396169635999946, -79.04136917884000013, 4.832020119862000307 ) ) ;
#20035 = CARTESIAN_POINT ( 'NONE',  ( -8.657507096519999834, -77.50120975171299165, 7.296561482783999075 ) ) ;
#20036 = CARTESIAN_POINT ( 'NONE',  ( -8.596529571091879873, -77.54793149518738460, 6.606441957186066638 ) ) ;
#20038 = ORIENTED_EDGE ( 'NONE', *, *, #50351, .T. ) ;
#20037 = AXIS2_PLACEMENT_3D ( 'NONE', #42636, #34042, #51505 ) ;
#20039 = ORIENTED_EDGE ( 'NONE', *, *, #24170, .F. ) ;
#20041 = ADVANCED_FACE ( 'NONE', ( #3631 ), #4510, .F. ) ;
#20040 = ORIENTED_EDGE ( 'NONE', *, *, #50103, .F. ) ;
#20042 = CARTESIAN_POINT ( 'NONE',  ( 0.8513071080735492568, -80.41589136472569521, 0.9149315643236480833 ) ) ;
#20043 = EDGE_CURVE ( 'NONE', #26509, #16529, #48026, .T. ) ;
#20044 = CARTESIAN_POINT ( 'NONE',  ( -0.7035745874731462735, -77.71981679028705514, -10.74957825944642487 ) ) ;
#20045 = CARTESIAN_POINT ( 'NONE',  ( 8.249323304235000265, -80.33519793320401448, -5.229696851825000437 ) ) ;
#20046 = ORIENTED_EDGE ( 'NONE', *, *, #47736, .T. ) ;
#20047 = CARTESIAN_POINT ( 'NONE',  ( -0.8504682047943638024, -2.496968858996786000, 3.168006968375890686 ) ) ;
#20048 = CARTESIAN_POINT ( 'NONE',  ( 10.60715898610999908, -79.30441252099899430, -2.581384170113000032 ) ) ;
#20049 = ORIENTED_EDGE ( 'NONE', *, *, #37762, .T. ) ;
#20050 = CARTESIAN_POINT ( 'NONE',  ( -12.77649732927999970, -25.30828417252000051, 0.06479631635393000300 ) ) ;
#20051 = CARTESIAN_POINT ( 'NONE',  ( 4.001451577097999923, -77.84924415034599576, 8.339717337904000161 ) ) ;
#20052 = B_SPLINE_CURVE_WITH_KNOTS ( 'NONE', 3,
 ( #25038, #12046, #39483, #2618, #33884, #30026, #11761, #25610, #38616, #56633, #16191, #43923, #3469, #29738, #21476, #57485, #12613, #31179, #4342, #21757, #49219, #8770, #9363, #14072, #32069, #538, #17929, #36219, #39761, #35918, #44489, #40051, #57775, #36509, #40656, #18516, #50110, #13485, #9654, #27642, #54239, #49520, #12894, #26762, #30895, #31776, #17330, #44790, #3757, #22936, #246, #58069, #53949, #49817, #27055, #35318, #27354, #53348, #48928, #45392, #22343, #40358, #9069, #8470, #4933 ),
 .UNSPECIFIED., .F., .F.,
 ( 4, 2, 2, 2, 2, 2, 2, 2, 2, 2, 2, 2, 2, 2, 2, 2, 1, 2, 2, 2, 2, 2, 2, 2, 2, 2, 2, 2, 2, 2, 2, 2, 4 ),
 ( 0.000000000000000000, 0.03125000000000000000, 0.06249999999999998612, 0.09374999999999998612, 0.1249999999999999861, 0.1562499999999999722, 0.1874999999999999722, 0.2187499999999999722, 0.2499999999999999722, 0.2812500000000000000, 0.3125000000000000000, 0.3437500000000000000, 0.3750000000000000000, 0.4062500000000000000, 0.4375000000000000000, 0.4687500000000000000, 0.5000000000000000000, 0.5312500000000000000, 0.5625000000000000000, 0.5937500000000000000, 0.6250000000000000000, 0.6562500000000000000, 0.6875000000000000000, 0.7187500000000000000, 0.7500000000000000000, 0.7812500000000000000, 0.8125000000000000000, 0.8437500000000000000, 0.8750000000000000000, 0.9062500000000000000, 0.9375000000000000000, 0.9687500000000000000, 1.000000000000000000 ),
 .UNSPECIFIED. ) ;
#20053 = CONICAL_SURFACE ( 'NONE', #19157, 10.04999999996000071, 0.7853981633972997312 ) ;
#20054 = DIRECTION ( 'NONE',  ( 0.000000000000000000, -1.000000000000000000, 0.000000000000000000 ) ) ;
#20055 = CARTESIAN_POINT ( 'NONE',  ( 11.70000000000000107, -79.79999999999999716, 0.000000000000000000 ) ) ;
#20056 = DIRECTION ( 'NONE',  ( 1.000000000000000000, 0.000000000000000000, 0.000000000000000000 ) ) ;
#20057 = AXIS2_PLACEMENT_3D ( 'NONE', #6487, #52237, #20930 ) ;
#20058 = CARTESIAN_POINT ( 'NONE',  ( -6.259101251364000085, -77.20009236341799408, 7.707182931745999888 ) ) ;
#20059 = CARTESIAN_POINT ( 'NONE',  ( -0.4698087411539742519, -78.74903415325783840, 1.463278444719919635 ) ) ;
#20060 = CARTESIAN_POINT ( 'NONE',  ( -4.014515848897613814, -81.66770834536960422, 0.5407614939776936858 ) ) ;
#20061 = CARTESIAN_POINT ( 'NONE',  ( 12.17088485526999975, -75.70997293883000623, 1.845041276493999849 ) ) ;
#20062 = CARTESIAN_POINT ( 'NONE',  ( -7.596835002782708735, -77.95208333333333428, -5.838193839761694370 ) ) ;
#20063 = CARTESIAN_POINT ( 'NONE',  ( 8.485281374238999419, -60.04999999966999980, -8.485281374238999419 ) ) ;
#20064 = CARTESIAN_POINT ( 'NONE',  ( 11.93255069029000026, -79.21413110817999836, -2.830763026309000008 ) ) ;
#20065 = CARTESIAN_POINT ( 'NONE',  ( 2.548493721447000038, -76.99225984930698985, 12.01365081398999912 ) ) ;
#20066 = DIRECTION ( 'NONE',  ( 0.000000000000000000, 1.000000000000000000, 0.000000000000000000 ) ) ;
#20067 = CARTESIAN_POINT ( 'NONE',  ( 10.30361667856515417, -77.84302199712344361, 6.183189858139286343 ) ) ;
#20068 = ORIENTED_EDGE ( 'NONE', *, *, #45244, .T. ) ;
#20069 = CARTESIAN_POINT ( 'NONE',  ( -1.289397738844999974, -81.47443067016000384, -0.2928510814055000355 ) ) ;
#20070 = CARTESIAN_POINT ( 'NONE',  ( -1.538071403319991814, -77.91458333333333997, -11.75000000000000355 ) ) ;
#20071 = DIRECTION ( 'NONE',  ( 0.000000000000000000, 0.000000000000000000, -1.000000000000000000 ) ) ;
#20072 = AXIS2_PLACEMENT_3D ( 'NONE', #37842, #34558, #38421 ) ;
#20073 = CARTESIAN_POINT ( 'NONE',  ( -0.3271848554491046945, -82.89583333333328596, 1.217465845835393301 ) ) ;
#20074 = CARTESIAN_POINT ( 'NONE',  ( -3.679349115619000354, -1.792405217095000003, 0.1044579997439999963 ) ) ;
#20075 = CARTESIAN_POINT ( 'NONE',  ( 4.484759669696999573, -77.35351546138099366, 11.18403784080000030 ) ) ;
#20076 = CARTESIAN_POINT ( 'NONE',  ( 7.282635111839001141, -77.57859895515098003, 6.467064367534000269 ) ) ;
#20078 = CARTESIAN_POINT ( 'NONE',  ( 4.977885330626823368, -77.86203852219340149, -9.897304379485548864 ) ) ;
#20077 = CARTESIAN_POINT ( 'NONE',  ( -7.250009772427842059, -76.12782158799809906, 9.252138825763349672 ) ) ;
#20079 = CARTESIAN_POINT ( 'NONE',  ( 1.242145130744999992, -82.29782237970999859, -0.5320213307544999770 ) ) ;
#20080 = CARTESIAN_POINT ( 'NONE',  ( -10.75000000000000000, -79.59999999999999432, 0.000000000000000000 ) ) ;
#20081 = ORIENTED_EDGE ( 'NONE', *, *, #21743, .T. ) ;
#20082 = CARTESIAN_POINT ( 'NONE',  ( 12.70610460582542167, -24.45512899795008011, 1.580683094056565485 ) ) ;
#20083 = DIRECTION ( 'NONE',  ( -1.000000000000000000, 0.000000000000000000, 0.000000000000000000 ) ) ;
#20084 = DIRECTION ( 'NONE',  ( 0.000000000000000000, -1.000000000000000000, 0.000000000000000000 ) ) ;
#20085 = CARTESIAN_POINT ( 'NONE',  ( -6.654586241810727998, -76.22057291693802483, -8.660536402383590016 ) ) ;
#20086 = CARTESIAN_POINT ( 'NONE',  ( -10.95938340363141528, -80.09357446033341432, 0.9416311679418450931 ) ) ;
#20087 = CARTESIAN_POINT ( 'NONE',  ( -7.768786981737000552, -79.62869298055800016, -5.571087248544999149 ) ) ;
#20088 = CARTESIAN_POINT ( 'NONE',  ( -0.8494789362751314910, -3.204387569124965474, -3.247320870830982198 ) ) ;
#20089 = CARTESIAN_POINT ( 'NONE',  ( -12.70457850616584317, -53.62128713286525539, -0.5106122237776331563 ) ) ;
#20090 = VERTEX_POINT ( 'NONE', #58233 ) ;
#20091 = AXIS2_PLACEMENT_3D ( 'NONE', #32459, #23621, #23336 ) ;
#20092 = CARTESIAN_POINT ( 'NONE',  ( 0.000000000000000000, 0.000000000000000000, 0.000000000000000000 ) ) ;
#20093 = CARTESIAN_POINT ( 'NONE',  ( -7.553623922565042115, -79.11961698824401878, -9.109432733142380556 ) ) ;
#20094 = CARTESIAN_POINT ( 'NONE',  ( 3.399999999999981704, -78.70000000000000284, 2.006589450846597789 ) ) ;
#20095 = ADVANCED_FACE ( 'NONE', ( #8639 ), #23418, .F. ) ;
#20096 = CARTESIAN_POINT ( 'NONE',  ( 1.347889543704216431, -77.31907281190599690, 11.99453198319526592 ) ) ;
#20098 = CARTESIAN_POINT ( 'NONE',  ( 0.05551074714531987336, -81.47208037662812785, 1.249630598122650982 ) ) ;
#20097 = CARTESIAN_POINT ( 'NONE',  ( -0.2293039177969000142, -82.26821515038699317, -1.215124277147999976 ) ) ;
#20099 = CARTESIAN_POINT ( 'NONE',  ( 14.00000000000000000, -72.39999999999999147, -1.714505518806294638E-15 ) ) ;
#20100 = CARTESIAN_POINT ( 'NONE',  ( -3.654181822837000215, -86.09999999943198645, 1.626946589673999854 ) ) ;
#20101 = CARTESIAN_POINT ( 'NONE',  ( 8.414570695956999913, -59.94999999967000548, 8.414570695956999913 ) ) ;
#20102 = CARTESIAN_POINT ( 'NONE',  ( 1.331074987945999988, -78.92186531869998589, 0.4986494974128999336 ) ) ;
#20103 = CARTESIAN_POINT ( 'NONE',  ( -1.980532758766000212, -22.76256650694000072, 12.80088938802999898 ) ) ;
#20104 = CARTESIAN_POINT ( 'NONE',  ( 0.7681833999686413783, -78.32291666666668561, 0.9995835529977274980 ) ) ;
#20105 = EDGE_CURVE ( 'NONE', #43036, #23138, #21220, .T. ) ;
#20106 = CARTESIAN_POINT ( 'NONE',  ( -5.809791519574999619, -79.13523967109999546, 7.851562197947999699 ) ) ;
#20107 = ORIENTED_EDGE ( 'NONE', *, *, #28451, .T. ) ;
#20108 = ORIENTED_EDGE ( 'NONE', *, *, #53953, .T. ) ;
#20109 = CARTESIAN_POINT ( 'NONE',  ( -8.872994237323272415, -77.86999999999999034, 3.510218210012938211 ) ) ;
#20110 = CARTESIAN_POINT ( 'NONE',  ( 5.096297253146042650, -78.76436718932042425, -9.465160375605314869 ) ) ;
#20111 = ORIENTED_EDGE ( 'NONE', *, *, #41247, .F. ) ;
#20112 = CARTESIAN_POINT ( 'NONE',  ( 7.961057357828999592, -17.46431744651999907, 9.783210913639999617 ) ) ;
#20113 = CARTESIAN_POINT ( 'NONE',  ( -9.438184056264791622, -79.39065464712832920, 1.083930077607391240 ) ) ;
#20114 = ADVANCED_FACE ( 'NONE', ( #37834 ), #40847, .F. ) ;
#20115 = CARTESIAN_POINT ( 'NONE',  ( -5.440694134380999358, -78.91922042627000167, -10.76505340543000067 ) ) ;
#20116 = LINE ( 'NONE', #47582, #1409 ) ;
#20117 = DIRECTION ( 'NONE',  ( 0.7071067811865475727, 0.000000000000000000, 0.7071067811865475727 ) ) ;
#20118 = CARTESIAN_POINT ( 'NONE',  ( 3.250000000000000000, -3.250000000000000000, 0.000000000000000000 ) ) ;
#20119 = CARTESIAN_POINT ( 'NONE',  ( -9.805641529082999241, -79.37424299324300137, -5.446788484474000214 ) ) ;
#20120 = EDGE_CURVE ( 'NONE', #14133, #27498, #38957, .T. ) ;
#20121 = ORIENTED_EDGE ( 'NONE', *, *, #44954, .F. ) ;
#20122 = CARTESIAN_POINT ( 'NONE',  ( 5.059105317731693141, -78.13973803206332036, 10.65395817999562667 ) ) ;
#20123 = EDGE_LOOP ( 'NONE', ( #819, #25250, #12664 ) ) ;
#20124 = CARTESIAN_POINT ( 'NONE',  ( 9.219793351069757392, -77.35649433367561301, 0.7464174168656269037 ) ) ;
#20125 = CARTESIAN_POINT ( 'NONE',  ( -1.776188306762000124, -77.60259568715798650, -10.89629776253999971 ) ) ;
#20126 = CARTESIAN_POINT ( 'NONE',  ( -6.884902925240382388, -78.42231923253098103, -8.855492064945991615 ) ) ;
#20127 = UNCERTAINTY_MEASURE_WITH_UNIT (LENGTH_MEASURE( 1.000000000000000082E-05 ), #10015, 'distance_accuracy_value', 'NONE');
#20128 = CARTESIAN_POINT ( 'NONE',  ( 1.481171800329999844, -77.81445905126490459, 0.3241480609735999940 ) ) ;
#20129 = AXIS2_PLACEMENT_3D ( 'NONE', #3164, #43898, #47185 ) ;
#20130 = DIRECTION ( 'NONE',  ( 0.000000000000000000, 1.000000000000000000, 0.000000000000000000 ) ) ;
#20131 = CARTESIAN_POINT ( 'NONE',  ( 0.4326115402657000342, -79.03523500932999468, -1.568920109259999807 ) ) ;
#20132 = CARTESIAN_POINT ( 'NONE',  ( -7.655542440091000600, -19.22180874373999870, 10.38645071870000081 ) ) ;
#20133 = VECTOR ( 'NONE', #43108, 1000.000000000000000 ) ;
#20134 = CARTESIAN_POINT ( 'NONE',  ( -10.20553722967999910, -78.52435544289399161, -4.233781229625999565 ) ) ;
#20135 = DIRECTION ( 'NONE',  ( 1.000000000000000000, 0.000000000000000000, 0.000000000000000000 ) ) ;
#20136 = CARTESIAN_POINT ( 'NONE',  ( 11.92746894621999942, -79.41036807549798482, 1.562891678063999867 ) ) ;
#20137 =( LENGTH_UNIT ( ) NAMED_UNIT ( * ) SI_UNIT ( .MILLI., .METRE. ) );
#20138 = CARTESIAN_POINT ( 'NONE',  ( 0.2486384805219999938, -85.03526194493599633, -3.535979362066000498 ) ) ;
#20139 = EDGE_LOOP ( 'NONE', ( #19143, #57628, #48005, #35440 ) ) ;
#20140 = CARTESIAN_POINT ( 'NONE',  ( -12.14769635903000200, -78.85631629717299518, 2.650188445066000043 ) ) ;
#20141 = CARTESIAN_POINT ( 'NONE',  ( 0.5947595261268000533, -80.98341720544999589, -1.595643580583000043 ) ) ;
#20142 = CARTESIAN_POINT ( 'NONE',  ( 9.329378798893031899, -79.30846558317799122, -5.387576131639663757 ) ) ;
#20143 = CARTESIAN_POINT ( 'NONE',  ( 11.81379047889000056, -77.39715825954098705, 1.987564636421000008 ) ) ;
#20144 = CARTESIAN_POINT ( 'NONE',  ( -8.385806979641005299, -53.91189752976736571, 9.298530586719172319 ) ) ;
#20145 = CARTESIAN_POINT ( 'NONE',  ( -0.6870218104159775407, -77.82969972257922109, -1.073419096667898032 ) ) ;
#20146 = CARTESIAN_POINT ( 'NONE',  ( -3.453171399369999950, -1.763032031398999999, -0.5706200895263999762 ) ) ;
#20147 = CARTESIAN_POINT ( 'NONE',  ( 4.598371993787000456, -78.85435584965399869, -8.567308531191999421 ) ) ;
#20148 = CARTESIAN_POINT ( 'NONE',  ( -5.004442145019999622, -77.15958109976958212, -7.972877152348999630 ) ) ;
#20149 = CARTESIAN_POINT ( 'NONE',  ( -10.60678368039263297, -76.58707232302387524, 1.749019199596896001 ) ) ;
#20150 = CARTESIAN_POINT ( 'NONE',  ( -7.585478157043000103, -77.52352982952599803, -8.010134550088000793 ) ) ;
#20151 = DIRECTION ( 'NONE',  ( -1.000000000000000000, 0.000000000000000000, 0.000000000000000000 ) ) ;
#20152 = CARTESIAN_POINT ( 'NONE',  ( 7.321105331825000562, -80.27520846168349067, 8.057475193947000847 ) ) ;
#20153 = CARTESIAN_POINT ( 'NONE',  ( 1.130902752456465654, -80.86209933428780516, -0.5870578767658550801 ) ) ;
#20154 = EDGE_LOOP ( 'NONE', ( #30537, #10486, #57741, #40085, #52824 ) ) ;
#20155 = CARTESIAN_POINT ( 'NONE',  ( 1.304222966381000104, -81.53240404768499161, 0.2785293583740000023 ) ) ;
#20156 = CARTESIAN_POINT ( 'NONE',  ( 1.814305421036000121, -61.08941969298000174, -12.78003582256000215 ) ) ;
#20157 = CARTESIAN_POINT ( 'NONE',  ( -8.595351952246861771, -80.54797288116316167, 6.605825225780209919 ) ) ;
#20158 = CARTESIAN_POINT ( 'NONE',  ( -3.244487197725999916, -76.86775418965099504, -10.73738397614000029 ) ) ;
#20159 = CARTESIAN_POINT ( 'NONE',  ( 8.867070753125000593, -78.56969597644598480, -6.468312982590000537 ) ) ;
#20160 = CARTESIAN_POINT ( 'NONE',  ( 10.45205659047000069, -56.03767314774999875, -7.651160337227000063 ) ) ;
#20161 = CARTESIAN_POINT ( 'NONE',  ( -3.887390283284898551, -83.13229165435031121, 1.138840507441416516 ) ) ;
#20162 = CARTESIAN_POINT ( 'NONE',  ( 8.006345619697000870, -77.19309101131499062, -8.693492320142999219 ) ) ;
#20163 = CARTESIAN_POINT ( 'NONE',  ( 7.050812550749764540, -78.52208679444892425, 9.402307432884422056 ) ) ;
#20164 = CARTESIAN_POINT ( 'NONE',  ( -10.20678250203529025, -61.03575784435037122, 7.770339463558867621 ) ) ;
#20165 = ORIENTED_EDGE ( 'NONE', *, *, #42080, .T. ) ;
#20166 = CARTESIAN_POINT ( 'NONE',  ( -1.171857579988537124, -80.07201495124374446, 0.4348164940204689022 ) ) ;
#20167 = CARTESIAN_POINT ( 'NONE',  ( 8.796335266379964324, -78.00208333333334565, 6.760013919724087827 ) ) ;
#20168 = AXIS2_PLACEMENT_3D ( 'NONE', #57602, #31597, #17163 ) ;
#20169 = CARTESIAN_POINT ( 'NONE',  ( 7.633478597807999755, -55.59901960186999759, -10.36292351976000070 ) ) ;
#20170 = CARTESIAN_POINT ( 'NONE',  ( 10.99934742197999960, -79.44654329274898430, 2.437886521773999782 ) ) ;
#20171 = CARTESIAN_POINT ( 'NONE',  ( -11.88151041292270094, -79.13151041431198962, -1.554433303865662142 ) ) ;
#20172 = CARTESIAN_POINT ( 'NONE',  ( 0.000000000000000000, -87.29999999999999716, 0.000000000000000000 ) ) ;
#20173 = CARTESIAN_POINT ( 'NONE',  ( 0.7681090888009013407, -78.92317030813214274, 0.9998401714662717987 ) ) ;
#20174 = CARTESIAN_POINT ( 'NONE',  ( -1.511181634424322739, -81.85134434412550775, -0.03904378459183766026 ) ) ;
#20175 = FACE_BOUND ( 'NONE', #33000, .T. ) ;
#20176 = AXIS2_PLACEMENT_3D ( 'NONE', #46660, #1782, #24490 ) ;
#20177 = CARTESIAN_POINT ( 'NONE',  ( -1.199500263597270244, -77.95208333333333428, -0.9218200799623728070 ) ) ;
#20178 = ORIENTED_EDGE ( 'NONE', *, *, #17808, .F. ) ;
#20179 = CARTESIAN_POINT ( 'NONE',  ( -0.8831554397796215206, -81.66311148394188990, -0.8841190442798870786 ) ) ;
#20180 = ADVANCED_FACE ( 'NONE', ( #42823 ), #30081, .T. ) ;
#20181 = CARTESIAN_POINT ( 'NONE',  ( 9.500000000000000000, -87.20000000000000284, 0.000000000000000000 ) ) ;
#20182 = ORIENTED_EDGE ( 'NONE', *, *, #48945, .F. ) ;
#20183 = ORIENTED_EDGE ( 'NONE', *, *, #53613, .T. ) ;
#20184 = CARTESIAN_POINT ( 'NONE',  ( -1.980584515756000030, -23.26485150094000076, -12.76303204340999997 ) ) ;
#20185 = EDGE_LOOP ( 'NONE', ( #55543, #15154 ) ) ;
#20186 = ORIENTED_EDGE ( 'NONE', *, *, #46847, .F. ) ;
#20187 = CARTESIAN_POINT ( 'NONE',  ( -0.9781264271453999903, -17.05968856123000066, 12.65967462879000038 ) ) ;
#20188 = CARTESIAN_POINT ( 'NONE',  ( -10.49924843836999777, -80.37932778397052402, -4.054558598941000014 ) ) ;
#20189 = DIRECTION ( 'NONE',  ( 1.000000000000000000, 0.000000000000000000, 0.000000000000000000 ) ) ;
#20190 = DIRECTION ( 'NONE',  ( 0.000000000000000000, -1.000000000000000000, 0.000000000000000000 ) ) ;
#20191 = CARTESIAN_POINT ( 'NONE',  ( -0.8547114690830001082, -79.07506332859900056, 9.761549055228000427 ) ) ;
#20192 = CARTESIAN_POINT ( 'NONE',  ( 3.340492633907115039, -76.26875000031391494, -10.28561997391731175 ) ) ;
#20193 = EDGE_CURVE ( 'NONE', #587, #23097, #11981, .T. ) ;
#20194 = CIRCLE ( 'NONE', #38088, 10.69999999999999929 ) ;
#20195 = VERTEX_POINT ( 'NONE', #16532 ) ;
#20196 = VERTEX_POINT ( 'NONE', #15659 ) ;
#20197 = CARTESIAN_POINT ( 'NONE',  ( -9.195808504226482327, -77.59150866904204236, 1.005241119271180095 ) ) ;
#20198 = CARTESIAN_POINT ( 'NONE',  ( -11.87139580924456261, -76.91341727770499404, -2.023209039049733704 ) ) ;
#20199 = PRODUCT_DEFINITION_SHAPE ( 'NONE', 'NONE',  #58415 ) ;
#20200 = DIRECTION ( 'NONE',  ( 0.000000000000000000, -1.000000000000000000, 0.000000000000000000 ) ) ;
#20201 = CARTESIAN_POINT ( 'NONE',  ( 8.553489385229999797, -79.05567299584799912, 4.133741566275999979 ) ) ;
#20202 = CARTESIAN_POINT ( 'NONE',  ( 9.500000000000000000, -77.64999999999999147, 0.000000000000000000 ) ) ;
#20203 = CARTESIAN_POINT ( 'NONE',  ( -6.606377239730330864, -76.57291666666665719, -8.596418555780440229 ) ) ;
#20204 = CARTESIAN_POINT ( 'NONE',  ( 11.68767212001978173, -76.67083333333333428, 3.140974612311388192 ) ) ;
#20205 = CARTESIAN_POINT ( 'NONE',  ( -0.9103895169571000201, -79.34438689399999589, -1.233764334031000054 ) ) ;
#20206 = VECTOR ( 'NONE', #28288, 999.9999999999998863 ) ;
#20207 = DIRECTION ( 'NONE',  ( 1.000000000000000000, 0.000000000000000000, 0.000000000000000000 ) ) ;
#20208 = CARTESIAN_POINT ( 'NONE',  ( -9.764531328947487765, -76.65264217124246215, 6.535287190017895043 ) ) ;
#20209 = CARTESIAN_POINT ( 'NONE',  ( 3.707796996315166016, -79.21874998086906317, -11.41868144588404377 ) ) ;
#20210 = CARTESIAN_POINT ( 'NONE',  ( -9.992014434659999722, -54.63915351680999777, 7.762970980286999279 ) ) ;
#20211 = CARTESIAN_POINT ( 'NONE',  ( -0.5353773281849999455, -78.62753667140100333, -9.784259853904000437 ) ) ;
#20212 = TOROIDAL_SURFACE ( 'NONE', #19283, 26.50000000000000000, 14.00000000000000000 ) ;
#20213 = CARTESIAN_POINT ( 'NONE',  ( -10.02842745654077561, -80.28333333334607858, -4.462749333579311362 ) ) ;
#20214 = EDGE_CURVE ( 'NONE', #16460, #521, #15593, .T. ) ;
#20215 = CARTESIAN_POINT ( 'NONE',  ( 1.799501877793999949, -23.28917723430000208, -12.60552511010000032 ) ) ;
#20217 = CARTESIAN_POINT ( 'NONE',  ( 1.798336774608999988, -18.80355501948000096, -12.61277771566000006 ) ) ;
#20216 = CARTESIAN_POINT ( 'NONE',  ( -0.9218200799623778030, -78.82708333333337691, 1.199500263597266914 ) ) ;
#20218 = CARTESIAN_POINT ( 'NONE',  ( 1.570796326794856590, -78.26458333333330586, 12.00000000000000711 ) ) ;
#20219 = CARTESIAN_POINT ( 'NONE',  ( -8.102049197848998574, -80.36951364748298943, 7.545907228784999532 ) ) ;
#20220 = FACE_OUTER_BOUND ( 'NONE', #16928, .T. ) ;
#20221 = CARTESIAN_POINT ( 'NONE',  ( 3.938171349113054998, -79.24333333333341045, -8.369041066855391620 ) ) ;
#20222 = CARTESIAN_POINT ( 'NONE',  ( -7.342331066867000544, -55.64999999967000122, -8.190859204290999784 ) ) ;
#20223 = EDGE_LOOP ( 'NONE', ( #35485, #15299, #51488, #31414 ) ) ;
#20224 = CARTESIAN_POINT ( 'NONE',  ( 0.000000000000000000, -76.00000000000000000, 0.000000000000000000 ) ) ;
#20225 = CARTESIAN_POINT ( 'NONE',  ( -1.666698456705999920, -55.60818260126999490, 12.50018138918999888 ) ) ;
#20226 = CARTESIAN_POINT ( 'NONE',  ( 1.159297299441395701, -78.38080567615219252, 0.4674996523628443534 ) ) ;
#20227 = CARTESIAN_POINT ( 'NONE',  ( 2.018311730614999799, -79.59891319606099103, -9.317554422237000367 ) ) ;
#20228 = CARTESIAN_POINT ( 'NONE',  ( -12.79971535682999928, -55.00965922235999983, 2.019101350716999921 ) ) ;
#20229 = FACE_OUTER_BOUND ( 'NONE', #52601, .T. ) ;
#20230 = CARTESIAN_POINT ( 'NONE',  ( -2.521418227633154263, -79.49383760258125164, 10.45011237715473129 ) ) ;
#20231 = CARTESIAN_POINT ( 'NONE',  ( -8.796335266379976758, -77.25208333333331723, -6.760013919724066511 ) ) ;
#20232 = CARTESIAN_POINT ( 'NONE',  ( -2.398287285836949501, -78.67389998729011324, 3.977573602256665009 ) ) ;
#20233 = CARTESIAN_POINT ( 'NONE',  ( 9.634437611857999073, -77.66019374448798374, 5.199262921030999962 ) ) ;
#20234 = CIRCLE ( 'NONE', #56967, 0.6000000000000008660 ) ;
#20235 = CARTESIAN_POINT ( 'NONE',  ( 4.205198518925999274, -76.79725762008598622, -10.19892346455999999 ) ) ;
#20236 = CARTESIAN_POINT ( 'NONE',  ( -1.124740126079791569, -82.06431169942482029, 0.5547021489710047826 ) ) ;
#20237 = CARTESIAN_POINT ( 'NONE',  ( 0.4286008670186999825, -79.47756961838999246, -1.472170099309999980 ) ) ;
#20238 = DIRECTION ( 'NONE',  ( 0.7071067811865475727, 0.000000000000000000, 0.7071067811865475727 ) ) ;
#20239 = CARTESIAN_POINT ( 'NONE',  ( -9.554796630153999715, -79.69035584965399721, -0.02401403847836000235 ) ) ;
#20240 = CARTESIAN_POINT ( 'NONE',  ( -9.250000000000000000, -79.49999999999998579, 1.813240672189999963E-14 ) ) ;
#20241 = CARTESIAN_POINT ( 'NONE',  ( 6.107111665684042734, -80.27352331620853931, -8.846533776856475129 ) ) ;
#20242 = CARTESIAN_POINT ( 'NONE',  ( -10.94712378871737535, -76.21666666663080036, 4.871360733705688340 ) ) ;
#20243 = CARTESIAN_POINT ( 'NONE',  ( 8.300970689365442468, -77.19166666666667709, 4.784380313523563188 ) ) ;
#20244 = CARTESIAN_POINT ( 'NONE',  ( -11.60111135005000094, -79.15519343212500303, -3.181408645392000523 ) ) ;
#20245 = EDGE_CURVE ( 'NONE', #48866, #18440, #23324, .T. ) ;
#20246 = AXIS2_PLACEMENT_3D ( 'NONE', #2245, #30525, #42676 ) ;
#20247 = DIRECTION ( 'NONE',  ( 0.000000000000000000, 1.000000000000000000, 0.000000000000000000 ) ) ;
#20248 = FACE_OUTER_BOUND ( 'NONE', #20154, .T. ) ;
#20249 = ORIENTED_EDGE ( 'NONE', *, *, #2462, .T. ) ;
#20250 = ADVANCED_FACE ( 'NONE', ( #2102 ), #52509, .F. ) ;
#20251 = CARTESIAN_POINT ( 'NONE',  ( -11.69669687464000063, -78.60749258035299647, 2.371241166392999755 ) ) ;
#20252 = VERTEX_POINT ( 'NONE', #38377 ) ;
#20253 = B_SPLINE_CURVE_WITH_KNOTS ( 'NONE', 3,
 ( #51978, #42532, #16244, #33939, #43692, #3247 ),
 .UNSPECIFIED., .F., .F.,
 ( 4, 1, 1, 4 ),
 ( 0.000000000000000000, 0.3333333333333000081, 0.6666666666667000474, 1.000000000000000000 ),
 .UNSPECIFIED. ) ;
#20254 = ORIENTED_EDGE ( 'NONE', *, *, #19101, .T. ) ;
#20255 = ORIENTED_EDGE ( 'NONE', *, *, #46971, .T. ) ;
#20256 = CARTESIAN_POINT ( 'NONE',  ( -2.027724787492000136, -80.41092258374798973, -2.910823306046000258 ) ) ;
#20257 = CARTESIAN_POINT ( 'NONE',  ( 5.194870660562412645, -79.22882422843130712, 7.960803537416587972 ) ) ;
#20258 = ORIENTED_EDGE ( 'NONE', *, *, #30663, .F. ) ;
#20260 = EDGE_CURVE ( 'NONE', #48350, #20090, #29686, .T. ) ;
#20259 = CARTESIAN_POINT ( 'NONE',  ( 0.7170858719455162067, -82.77394172231353764, -1.023701603912586133 ) ) ;
#20261 = ORIENTED_EDGE ( 'NONE', *, *, #54132, .F. ) ;
#20262 = CARTESIAN_POINT ( 'NONE',  ( -7.682331425181999407, -56.03513569577999931, 10.04115011118999945 ) ) ;
#20263 = ORIENTED_EDGE ( 'NONE', *, *, #42497, .F. ) ;
#20264 = DIRECTION ( 'NONE',  ( 1.000000000000000000, 0.000000000000000000, 0.000000000000000000 ) ) ;
#20265 = CARTESIAN_POINT ( 'NONE',  ( -1.304299203641290150, -78.79190939947621075, -0.7577321730552538659 ) ) ;
#20266 = CARTESIAN_POINT ( 'NONE',  ( 1.052500557283970073, -79.80000000000002558, -11.73283057634160720 ) ) ;
#20267 = CARTESIAN_POINT ( 'NONE',  ( -5.880916218342844282, -80.02142361888905953, 9.002827806299052327 ) ) ;
#20268 = CARTESIAN_POINT ( 'NONE',  ( 0.4140829508681878046, -86.17851879815596305, -3.934470707847995907 ) ) ;
#20269 = CARTESIAN_POINT ( 'NONE',  ( 7.486068761172999686, -75.95067068213799644, -8.059700645992000645 ) ) ;
#20270 = CARTESIAN_POINT ( 'NONE',  ( -1.250000000000000000, -77.64999999999999147, 0.000000000000000000 ) ) ;
#20271 = CARTESIAN_POINT ( 'NONE',  ( 1.180475833332838898, -81.15297854159264546, 0.9435589873242250514 ) ) ;
#20272 = AXIS2_PLACEMENT_3D ( 'NONE', #633, #50200, #8574 ) ;
#20273 = CARTESIAN_POINT ( 'NONE',  ( -9.877439518601001112, -76.85324162823199856, 5.094664542828000187 ) ) ;
#20274 = CARTESIAN_POINT ( 'NONE',  ( -7.891267276537118569, -78.64385383780864913, -4.825895275192899625 ) ) ;
#20275 = VECTOR ( 'NONE', #19922, 1000.000000000000114 ) ;
#20276 = LINE ( 'NONE', #29403, #10120 ) ;
#20277 = CARTESIAN_POINT ( 'NONE',  ( -12.56594317991999965, -60.04999999381999487, -1.750000000001000089 ) ) ;
#20278 = CARTESIAN_POINT ( 'NONE',  ( -3.585753949159999898, -80.00092549782598894, 0.1615739086348000064 ) ) ;
#20279 = CARTESIAN_POINT ( 'NONE',  ( 6.411492066225999764, -79.40708379888700108, 10.24266459616000091 ) ) ;
#20280 = CARTESIAN_POINT ( 'NONE',  ( -10.39983874692026866, -78.07962607350559381, 2.743425914733084614 ) ) ;
#20281 = CARTESIAN_POINT ( 'NONE',  ( -0.3505635783453250331, -82.99769806729025845, 1.207601184449180964 ) ) ;
#20282 = CARTESIAN_POINT ( 'NONE',  ( -10.13969151608854524, -76.24193945363813896, -5.960466986128117206 ) ) ;
#20283 = DIRECTION ( 'NONE',  ( -0.7592504788685168204, 0.04890177849162108403, 0.6489586476797148951 ) ) ;
#20284 = CARTESIAN_POINT ( 'NONE',  ( -0.8338927958969420962, -24.80053577746247129, 12.50366901602898650 ) ) ;
#20285 = AXIS2_PLACEMENT_3D ( 'NONE', #32888, #1931, #52090 ) ;
#20286 = CARTESIAN_POINT ( 'NONE',  ( 7.596835002782696300, -78.20208333333334849, 5.838193839761711246 ) ) ;
#20287 = CARTESIAN_POINT ( 'NONE',  ( -1.199500263597270022, -77.55208333333331439, -0.9218200799623730290 ) ) ;
#20288 = DIRECTION ( 'NONE',  ( 0.000000000000000000, 1.000000000000000000, 0.000000000000000000 ) ) ;
#20289 = CARTESIAN_POINT ( 'NONE',  ( 12.54715528150999937, -24.53180535391000205, 1.292252957172000061 ) ) ;
#20290 = EDGE_CURVE ( 'NONE', #37723, #89, #25201, .T. ) ;
#20291 = CARTESIAN_POINT ( 'NONE',  ( 10.47234974255967366, -77.67964032115997952, -2.795332386398399649 ) ) ;
#20292 = CARTESIAN_POINT ( 'NONE',  ( 11.37976048585989020, -78.42608585681624334, -3.047580145233151683 ) ) ;
#20293 = TOROIDAL_SURFACE ( 'NONE', #35335, 13.50000000000000000, 0.5000000000000000000 ) ;
#20294 = CARTESIAN_POINT ( 'NONE',  ( -0.5193979750644999172, -78.97123230597145493, -10.96331347381999954 ) ) ;
#20295 = CARTESIAN_POINT ( 'NONE',  ( -1.250000000000000000, -18.75000000000000000, 12.50000000000000000 ) ) ;
#20296 = VERTEX_POINT ( 'NONE', #30371 ) ;
#20297 = CARTESIAN_POINT ( 'NONE',  ( 3.614576546944999969, -82.67079877876498983, -1.331975541213999970 ) ) ;
#20298 = CARTESIAN_POINT ( 'NONE',  ( 3.647699722741000183, -86.02148118236299013, -1.624060551956000076 ) ) ;
#20299 = CARTESIAN_POINT ( 'NONE',  ( 8.470860587981800194, -78.31708216412036450, -3.718899516019706919 ) ) ;
#20300 = CARTESIAN_POINT ( 'NONE',  ( 0.000000000000000000, -74.99999999999998579, 0.000000000000000000 ) ) ;
#20301 = CARTESIAN_POINT ( 'NONE',  ( 10.34070037867000202, -78.12002135927799884, -4.346035695907999319 ) ) ;
#20302 = CARTESIAN_POINT ( 'NONE',  ( -17.49999986748943925, -13.07071424677999971, -0.002153571276233540773 ) ) ;
#20303 = CARTESIAN_POINT ( 'NONE',  ( 4.763371395742999503, -77.49485258715699842, -8.495292134120999705 ) ) ;
#20304 = CARTESIAN_POINT ( 'NONE',  ( 0.3142488045808999875, -82.82582186680899383, 4.160266772619999109 ) ) ;
#20305 = CARTESIAN_POINT ( 'NONE',  ( -8.999999998907000531, -3.999999998907000087, 1.966780300384000192E-09 ) ) ;
#20306 = CARTESIAN_POINT ( 'NONE',  ( 1.161710437675000041, -79.24177606238200156, -0.9743588931339001169 ) ) ;
#20307 = ORIENTED_EDGE ( 'NONE', *, *, #20837, .F. ) ;
#20308 = CARTESIAN_POINT ( 'NONE',  ( 0.000000000000000000, -23.75000000000000000, 11.79999999999999893 ) ) ;
#20309 = CYLINDRICAL_SURFACE ( 'NONE', #40339, 1.500000000000000000 ) ;
#20310 = ORIENTED_EDGE ( 'NONE', *, *, #24546, .F. ) ;
#20311 = CARTESIAN_POINT ( 'NONE',  ( 1.196963559360000096, -78.39177149676930867, -0.5880938590690999446 ) ) ;
#20312 = CARTESIAN_POINT ( 'NONE',  ( 12.53239398061000109, -59.56486430393999854, 1.667936688463999895 ) ) ;
#20313 = CIRCLE ( 'NONE', #34405, 1.000000000000000000 ) ;
#20314 = CARTESIAN_POINT ( 'NONE',  ( -8.838834764832000701, -18.75000000000000000, -8.838834764832000701 ) ) ;
#20315 = ORIENTED_EDGE ( 'NONE', *, *, #2345, .F. ) ;
#20316 = EDGE_CURVE ( 'NONE', #32447, #52628, #21983, .T. ) ;
#20317 = CARTESIAN_POINT ( 'NONE',  ( 11.54375705602000046, -77.98332587731398746, -3.837213001227999687 ) ) ;
#20318 = CARTESIAN_POINT ( 'NONE',  ( -9.771309935692000792, -78.01479567302799012, 5.719592689793999263 ) ) ;
#20319 = AXIS2_PLACEMENT_3D ( 'NONE', #16772, #26766, #40362 ) ;
#20320 = EDGE_LOOP ( 'NONE', ( #805, #16537, #43278, #38418 ) ) ;
#20321 = CARTESIAN_POINT ( 'NONE',  ( -0.4793197146253041496, -80.50639153267658799, 1.154396842167616954 ) ) ;
#20322 = CARTESIAN_POINT ( 'NONE',  ( 11.99999999999999822, -79.56041666666666856, 1.570796326794923203 ) ) ;
#20323 = CARTESIAN_POINT ( 'NONE',  ( 3.269429986698999979, -80.09785153581056250, 9.203886808668999109 ) ) ;
#20324 = ORIENTED_EDGE ( 'NONE', *, *, #55347, .F. ) ;
#20325 = EDGE_CURVE ( 'NONE', #237, #17178, #12383, .T. ) ;
#20326 = CARTESIAN_POINT ( 'NONE',  ( 8.500174178665998781, -78.26943148693000296, -6.849988769802000554 ) ) ;
#20327 = EDGE_LOOP ( 'NONE', ( #28807, #10219, #12647 ) ) ;
#20328 = CARTESIAN_POINT ( 'NONE',  ( -5.531768889155999958, -79.13776145859631583, -10.94525552207000096 ) ) ;
#20329 = EDGE_CURVE ( 'NONE', #18079, #4024, #50878, .T. ) ;
#20330 = CARTESIAN_POINT ( 'NONE',  ( 4.574312611392000072, -77.34484415034599181, 8.320643751074999983 ) ) ;
#20331 = CARTESIAN_POINT ( 'NONE',  ( 7.730439324435801396, -17.87809618957197699, -10.25198230928420173 ) ) ;
#20332 = CARTESIAN_POINT ( 'NONE',  ( -0.3926218265389256890, -78.29583333333334849, 1.460959015002472050 ) ) ;
#20333 = CARTESIAN_POINT ( 'NONE',  ( -11.75000000000000000, -77.20000000000000284, -1.435311119447000145E-14 ) ) ;
#20334 = CARTESIAN_POINT ( 'NONE',  ( -12.70305331333694632, -16.96853698854184600, -0.8727610012099511483 ) ) ;
#20335 = CARTESIAN_POINT ( 'NONE',  ( 0.1335152958906870024, -77.98161697419730842, -1.503794547195192788 ) ) ;
#20336 = CARTESIAN_POINT ( 'NONE',  ( 8.796335266379994522, -79.79791666666667993, -6.760013919724047859 ) ) ;
#20337 = CARTESIAN_POINT ( 'NONE',  ( -8.260136572111999698, -24.94034376567000066, 9.643347111174000119 ) ) ;
#20338 = CARTESIAN_POINT ( 'NONE',  ( 6.606377239730347739, -77.67708333333330017, -8.596418555780422466 ) ) ;
#20339 = CARTESIAN_POINT ( 'NONE',  ( -0.06116421237667998834, -79.84732046129099103, 4.171666818936000887 ) ) ;
#20340 = CARTESIAN_POINT ( 'NONE',  ( 8.082524092276875294, -77.79166666666667140, 4.658475568430836766 ) ) ;
#20341 = ADVANCED_FACE ( 'NONE', ( #8527 ), #27042, .F. ) ;
#20342 = CARTESIAN_POINT ( 'NONE',  ( 8.958641849996999085, -62.00112647771999974, -8.950065109854000056 ) ) ;
#20343 = CARTESIAN_POINT ( 'NONE',  ( 0.000000000000000000, -46.09579702914000165, 0.000000000000000000 ) ) ;
#20344 = CARTESIAN_POINT ( 'NONE',  ( -4.885220488697999741, -76.54144972795299395, 11.26753068192000029 ) ) ;
#20345 = CARTESIAN_POINT ( 'NONE',  ( 1.250000000000000000, -55.54999999966999980, 12.00000000000000000 ) ) ;
#20346 = CARTESIAN_POINT ( 'NONE',  ( -6.395896118064722025, -77.46943306756942604, 10.23033580516363195 ) ) ;
#20347 = DIRECTION ( 'NONE',  ( 0.7592504788685928707, 0.04890177849867949345, -0.6489586476790939473 ) ) ;
#20348 = TOROIDAL_SURFACE ( 'NONE', #27872, 9.799999999999998934, 0.2000000000000000111 ) ;
#20349 = VERTEX_POINT ( 'NONE', #44257 ) ;
#20350 = CARTESIAN_POINT ( 'NONE',  ( -0.8896385144511894660, -81.17505783692462273, 1.220758139846876977 ) ) ;
#20351 = CARTESIAN_POINT ( 'NONE',  ( -9.396085398178614767, -77.85208333333332575, -7.220923959705254802 ) ) ;
#20352 = FACE_OUTER_BOUND ( 'NONE', #50317, .T. ) ;
#20353 = DIRECTION ( 'NONE',  ( 0.7071067811865475727, 0.000000000000000000, 0.7071067811865475727 ) ) ;
#20354 = CARTESIAN_POINT ( 'NONE',  ( -1.937973738374999977, -3.211110789882000383, 3.350311810597999873 ) ) ;
#20355 = TOROIDAL_SURFACE ( 'NONE', #7166, 1.250000000000000000, 0.5000000000000000000 ) ;
#20356 = ADVANCED_FACE ( 'NONE', ( #12947 ), #3811, .F. ) ;
#20357 = CARTESIAN_POINT ( 'NONE',  ( -12.04425331849999914, -78.45234896019000814, -1.708359618215999909 ) ) ;
#20358 = CARTESIAN_POINT ( 'NONE',  ( 4.561861969681999973, -77.60702278427999090, 8.605179316909000065 ) ) ;
#20360 = CARTESIAN_POINT ( 'NONE',  ( -7.473530897346515545, -77.10494791667788661, 5.742368499590185138 ) ) ;
#20359 = CARTESIAN_POINT ( 'NONE',  ( -8.294246302884193511, -76.13736708880301762, 8.322727450349711731 ) ) ;
#20361 = CARTESIAN_POINT ( 'NONE',  ( 10.91653581620999880, -78.77708536617198831, 0.06787400445098999702 ) ) ;
#20362 = FACE_OUTER_BOUND ( 'NONE', #32319, .T. ) ;
#20363 = AXIS2_PLACEMENT_3D ( 'NONE', #9196, #40778, #44624 ) ;
#20364 = ORIENTED_EDGE ( 'NONE', *, *, #20214, .F. ) ;
#20365 = EDGE_CURVE ( 'NONE', #58179, #25083, #31763, .T. ) ;
#20366 = DIRECTION ( 'NONE',  ( 0.000000000000000000, -1.000000000000000000, 0.000000000000000000 ) ) ;
#20367 = CARTESIAN_POINT ( 'NONE',  ( -9.499121195477519208, -79.25069084405711806, -0.08246750231446209334 ) ) ;
#20368 = CARTESIAN_POINT ( 'NONE',  ( 0.000000000000000000, -80.49999999999998579, 0.000000000000000000 ) ) ;
#20369 = CARTESIAN_POINT ( 'NONE',  ( -2.047671225339077468E-06, -76.25353340279926329, -10.79679441329301959 ) ) ;
#20370 = DIRECTION ( 'NONE',  ( 0.000000000000000000, 1.000000000000000000, 0.000000000000000000 ) ) ;
#20371 = DIRECTION ( 'NONE',  ( 0.5721800009721869085, 0.8201280671257802357, 0.000000000000000000 ) ) ;
#20372 = CARTESIAN_POINT ( 'NONE',  ( -8.500000000000000000, -7.000000000000000000, 0.000000000000000000 ) ) ;
#20373 = CARTESIAN_POINT ( 'NONE',  ( -10.99999999999999822, -78.61041666666666572, -1.439896632895323325 ) ) ;
#20374 = ORIENTED_EDGE ( 'NONE', *, *, #36983, .F. ) ;
#20375 = CARTESIAN_POINT ( 'NONE',  ( 10.09881335831000015, -78.99010319720299833, -4.984770136353999348 ) ) ;
#20376 = CARTESIAN_POINT ( 'NONE',  ( 7.995769303601012012, -76.66150100378845877, 7.819579327592078855 ) ) ;
#20377 = FACE_OUTER_BOUND ( 'NONE', #33676, .T. ) ;
#20378 = CARTESIAN_POINT ( 'NONE',  ( -1.029292737021753279, -81.96672169472573444, -1.136050377789131538 ) ) ;
#20380 = CARTESIAN_POINT ( 'NONE',  ( -0.02778611078446202240, -81.47725253223261177, 1.249451979124360346 ) ) ;
#20379 = CARTESIAN_POINT ( 'NONE',  ( -0.9101267925792999591, -81.72247629319500106, -0.9551098530625999894 ) ) ;
#20381 = CARTESIAN_POINT ( 'NONE',  ( 10.75000000000000000, -79.75000000000000000, 0.000000000000000000 ) ) ;
#20382 = CARTESIAN_POINT ( 'NONE',  ( -9.141390146399626104, -76.99999999999998579, 1.754763298405772165 ) ) ;
#20383 = CARTESIAN_POINT ( 'NONE',  ( 1.249999986291000065, -76.30000000051599329, -0.6999999994844999796 ) ) ;
#20384 = CARTESIAN_POINT ( 'NONE',  ( 0.000000000000000000, -74.64999999999999147, 0.000000000000000000 ) ) ;
#20385 = PLANE ( 'NONE',  #52767 ) ;
#20386 = CARTESIAN_POINT ( 'NONE',  ( -13.86301033151605289, -9.638971321655001034, -0.1317488955328472711 ) ) ;
#20387 = ORIENTED_EDGE ( 'NONE', *, *, #49350, .F. ) ;
#20388 = VERTEX_POINT ( 'NONE', #13545 ) ;
#20389 = CARTESIAN_POINT ( 'NONE',  ( -3.243675144747000250, -77.43085259911799767, -12.16362487391999991 ) ) ;
#20390 = CARTESIAN_POINT ( 'NONE',  ( 5.081957869198564737, -78.76424439475270844, -9.472868843939814099 ) ) ;
#20391 = EDGE_CURVE ( 'NONE', #34093, #44548, #9130, .T. ) ;
#20392 = ORIENTED_EDGE ( 'NONE', *, *, #18116, .T. ) ;
#20393 = CARTESIAN_POINT ( 'NONE',  ( 10.52693198617999926, -18.57847693927000066, 7.606025555766000146 ) ) ;
#20394 = CONICAL_SURFACE ( 'NONE', #22278, 4.199999999630000147, 0.7853981633972997312 ) ;
#20395 = DIRECTION ( 'NONE',  ( 0.000000000000000000, 1.000000000000000000, 0.000000000000000000 ) ) ;
#20396 = CARTESIAN_POINT ( 'NONE',  ( 3.075537641221555596, -75.94583333333332575, -11.44417895085270587 ) ) ;
#20397 = AXIS2_PLACEMENT_3D ( 'NONE', #2743, #43767, #11606 ) ;
#20398 = CARTESIAN_POINT ( 'NONE',  ( 5.421352887295999956, -77.00873275214000557, 11.59375966951999892 ) ) ;
#20399 = VECTOR ( 'NONE', #30794, 1000.000000000000000 ) ;
#20400 = LINE ( 'NONE', #52275, #45743 ) ;
#20401 = FACE_OUTER_BOUND ( 'NONE', #51813, .T. ) ;
#20402 = CARTESIAN_POINT ( 'NONE',  ( 3.922208058606934333, -86.09999999999998010, 0.4502061935814848925 ) ) ;
#20403 = CARTESIAN_POINT ( 'NONE',  ( 0.9578316561262000262, -78.96569784821599569, -11.17589679220000143 ) ) ;
#20404 = COLOUR_RGB ( '', 0.31764706, 0.68627451, 0.89019608) ;
#20405 = ORIENTED_EDGE ( 'NONE', *, *, #54032, .T. ) ;
#20406 = CARTESIAN_POINT ( 'NONE',  ( 12.50000000000000000, -92.79999999999999716, 0.000000000000000000 ) ) ;
#20407 = EDGE_LOOP ( 'NONE', ( #42619, #12297, #19310, #46112, #47650, #51409, #6955, #27987, #17815 ) ) ;
#20408 = CARTESIAN_POINT ( 'NONE',  ( 9.249917852137487628, -77.35035757946567969, 0.04157983743616296135 ) ) ;
#20409 = CARTESIAN_POINT ( 'NONE',  ( -8.283402485401001769, -78.04793160847299305, -7.298588567667000149 ) ) ;
#20410 = LINE ( 'NONE', #38695, #2222 ) ;
#20411 = CARTESIAN_POINT ( 'NONE',  ( 12.00000000000000000, -78.14999999999999147, 0.000000000000000000 ) ) ;
#20412 = CARTESIAN_POINT ( 'NONE',  ( 1.407891339063999991, -78.86208320661400251, 0.1670362498605000023 ) ) ;
#20413 = DIRECTION ( 'NONE',  ( 0.000000000000000000, 1.000000000000000000, 2.042110567139000169E-13 ) ) ;
#20414 = ADVANCED_FACE ( 'NONE', ( #35677 ), #4036, .F. ) ;
#20415 = CARTESIAN_POINT ( 'NONE',  ( -11.90000000000000036, -21.00000000000000000, -0.6999999999999999556 ) ) ;
#20416 = CARTESIAN_POINT ( 'NONE',  ( -8.838834764832000701, -55.54999999966999980, -8.838834764832000701 ) ) ;
#20417 = B_SPLINE_CURVE_WITH_KNOTS ( 'NONE', 3,
 ( #56711, #7115, #2975, #20975, #25115, #16267, #24541, #37821 ),
 .UNSPECIFIED., .F., .F.,
 ( 4, 2, 2, 4 ),
 ( 0.000000000000000000, 0.5000000000000052180, 0.7500000000000025535, 1.000000000000000000 ),
 .UNSPECIFIED. ) ;
#20418 = CARTESIAN_POINT ( 'NONE',  ( -7.612971540276999960, -23.32452273707999879, 10.53003236233000095 ) ) ;
#20419 = CARTESIAN_POINT ( 'NONE',  ( 1.695617993698999904, -78.35580131689798122, 10.91800231797999921 ) ) ;
#20420 = EDGE_CURVE ( 'NONE', #30548, #39794, #10299, .T. ) ;
#20421 = DIRECTION ( 'NONE',  ( 0.000000000000000000, 1.000000000000000000, 0.000000000000000000 ) ) ;
#20422 = PRESENTATION_STYLE_ASSIGNMENT (( #2419 ) ) ;
#20423 = CARTESIAN_POINT ( 'NONE',  ( -3.318057126862000050, -86.14648452804499357, 0.9369146352647000908 ) ) ;
#20424 = VERTEX_POINT ( 'NONE', #55457 ) ;
#20425 = CARTESIAN_POINT ( 'NONE',  ( 1.647188161489999914, -81.60043415305999304, 0.4319573417677999849 ) ) ;
#20426 = LINE ( 'NONE', #6253, #27786 ) ;
#20427 = CARTESIAN_POINT ( 'NONE',  ( 8.547552837677239168, -79.29805100310200316, -6.557471810879811791 ) ) ;
#20428 = CARTESIAN_POINT ( 'NONE',  ( -3.085175050843000477, -78.10258993112499581, -11.57574012064000080 ) ) ;
#20429 = CARTESIAN_POINT ( 'NONE',  ( -7.756275637039999893, -17.77995361836999777, 10.15825999916999933 ) ) ;
#20430 = CARTESIAN_POINT ( 'NONE',  ( -0.8911338523900714792, -77.81379809819678428, -0.9115342124767401577 ) ) ;
#20431 = CARTESIAN_POINT ( 'NONE',  ( -0.2605338304268313143, -2.369161478775310137, -3.510605834263762492 ) ) ;
#20432 = CARTESIAN_POINT ( 'NONE',  ( 10.45146978769019519, -80.86920117642237926, 2.514705922069923716 ) ) ;
#20433 = CARTESIAN_POINT ( 'NONE',  ( -9.446372167179999835, -78.13301937267999620, 1.198511206093999970 ) ) ;
#20434 = CARTESIAN_POINT ( 'NONE',  ( 0.4376773866434802152, -81.25363771554175685, -1.170757306240687301 ) ) ;
#20435 = CARTESIAN_POINT ( 'NONE',  ( 2.927762776937000044, -77.60523885853200454, -10.63625589685999984 ) ) ;
#20436 = CARTESIAN_POINT ( 'NONE',  ( -1.662621324463000150, -81.13941687753749932, -10.78329382847999973 ) ) ;
#20437 = CARTESIAN_POINT ( 'NONE',  ( 1.207550169979716426, -80.92570526169950540, 0.4074191867525038813 ) ) ;
#20438 = ORIENTED_EDGE ( 'NONE', *, *, #43478, .T. ) ;
#20439 = EDGE_CURVE ( 'NONE', #57339, #26450, #28996, .T. ) ;
#20440 = DIRECTION ( 'NONE',  ( 0.000000000000000000, 1.000000000000000000, -1.776356839400000238E-14 ) ) ;
#20441 = DIRECTION ( 'NONE',  ( -1.000000000000000000, 0.000000000000000000, 0.000000000000000000 ) ) ;
#20442 = CARTESIAN_POINT ( 'NONE',  ( 1.798368564622000010, -59.99636757014000210, -12.61278090843000044 ) ) ;
#20443 = CARTESIAN_POINT ( 'NONE',  ( -8.150146600852252732, -55.38467666605728112, 7.387512494710395394 ) ) ;
#20444 = CARTESIAN_POINT ( 'NONE',  ( 4.275724345439000373, -76.92222687565399042, -10.36997068233999997 ) ) ;
#20445 = CARTESIAN_POINT ( 'NONE',  ( 6.083963560182000130, -78.54160362211398194, -9.135064530700001129 ) ) ;
#20446 = CARTESIAN_POINT ( 'NONE',  ( -0.5487783150233148666, -79.44506368774518990, -1.407050603238668041 ) ) ;
#20447 = CARTESIAN_POINT ( 'NONE',  ( -3.470841151267981317, -83.07447915372796388, 2.013464203440571421 ) ) ;
#20448 = CARTESIAN_POINT ( 'NONE',  ( 6.568955083609000489, -77.24824049629300760, -9.863814250127001415 ) ) ;
#20449 = CARTESIAN_POINT ( 'NONE',  ( 11.24815246472408425, -78.47207392326706099, 3.394727518005801414 ) ) ;
#20450 = DIRECTION ( 'NONE',  ( 0.4045626182452127795, -0.8201574091826254742, 0.4045626182452127795 ) ) ;
#20451 = ORIENTED_EDGE ( 'NONE', *, *, #24749, .F. ) ;
#20452 = AXIS2_PLACEMENT_3D ( 'NONE', #55807, #1504, #56673 ) ;
#20453 = CARTESIAN_POINT ( 'NONE',  ( -0.5576869831189765758, -80.01218415722107125, 1.118859008776958763 ) ) ;
#20454 = CARTESIAN_POINT ( 'NONE',  ( -3.630949683906000036, -75.80000000000001137, -11.17491406647000041 ) ) ;
#20455 = AXIS2_PLACEMENT_3D ( 'NONE', #38633, #11498, #29753 ) ;
#20456 = EDGE_CURVE ( 'NONE', #11044, #21614, #26162, .T. ) ;
#20457 = AXIS2_PLACEMENT_3D ( 'NONE', #25137, #33700, #16577 ) ;
#20458 = CARTESIAN_POINT ( 'NONE',  ( -0.5331530516160000177, -78.80041914309698825, -11.25365194899999999 ) ) ;
#20459 = CARTESIAN_POINT ( 'NONE',  ( 1.570796326794909881, -76.93541666666666856, -11.99999999999999822 ) ) ;
#20460 = CARTESIAN_POINT ( 'NONE',  ( -10.26699006316255591, -77.75833333333332575, 5.917523019358029934 ) ) ;
#20461 = CARTESIAN_POINT ( 'NONE',  ( -10.18499221076999994, -57.05022860182000244, 7.710118476618999850 ) ) ;
#20462 = VECTOR ( 'NONE', #20054, 1000.000000000000000 ) ;
#20463 = CARTESIAN_POINT ( 'NONE',  ( 1.023842844794183415, -82.03353868496313339, -1.111437593429350557 ) ) ;
#20464 = DIRECTION ( 'NONE',  ( 0.000000000000000000, -1.000000000000000000, 0.000000000000000000 ) ) ;
#20465 = CARTESIAN_POINT ( 'NONE',  ( -1.249633652174288123, -81.09028336531811476, 0.1639779393582905531 ) ) ;
#20466 = EDGE_LOOP ( 'NONE', ( #3023, #20756, #30666, #18658 ) ) ;
#20467 = CARTESIAN_POINT ( 'NONE',  ( 0.000000000000000000, -78.69999999999998863, 0.000000000000000000 ) ) ;
#20468 =( NAMED_UNIT ( * ) PLANE_ANGLE_UNIT ( ) SI_UNIT ( $, .RADIAN. ) );
#20469 = CARTESIAN_POINT ( 'NONE',  ( -12.72394223969999949, -23.22159774865999893, 1.930881086224999876 ) ) ;
#20470 = EDGE_LOOP ( 'NONE', ( #27925, #36255, #2681, #37220 ) ) ;
#20471 = VERTEX_POINT ( 'NONE', #14416 ) ;
#20472 = CARTESIAN_POINT ( 'NONE',  ( -1.343382297838000047E-14, -80.79999999999999716, 0.000000000000000000 ) ) ;
#20473 = EDGE_LOOP ( 'NONE', ( #37043, #14930, #2896, #48008, #857, #24604, #11760, #36463, #25754, #53486 ) ) ;
#20474 = EDGE_LOOP ( 'NONE', ( #33805, #18796, #55393, #34678 ) ) ;
#20475 = CARTESIAN_POINT ( 'NONE',  ( -8.593914503524631598, -81.00000000000001421, -6.616432748763715566 ) ) ;
#20476 = CARTESIAN_POINT ( 'NONE',  ( 0.1355484243948000267, -76.94742129968800270, 10.91590548763000079 ) ) ;
#20477 = CARTESIAN_POINT ( 'NONE',  ( -1.310679582531386611, -78.04166666666667140, -0.7554284705563495406 ) ) ;
#20478 = CARTESIAN_POINT ( 'NONE',  ( -9.676327351641999641, -79.20571332859898916, -1.545051445613999874 ) ) ;
#20479 = CARTESIAN_POINT ( 'NONE',  ( -1.794546681526326459, -78.20953827855916529, -9.074208611156969084 ) ) ;
#20480 = CARTESIAN_POINT ( 'NONE',  ( 0.000000000000000000, -75.09999999996229292, 0.000000000000000000 ) ) ;
#20481 = ORIENTED_EDGE ( 'NONE', *, *, #43456, .F. ) ;
#20482 = ORIENTED_EDGE ( 'NONE', *, *, #14602, .T. ) ;
#20483 = CARTESIAN_POINT ( 'NONE',  ( -7.483760668707474473, -77.55000130354729038, 5.436515708445330830 ) ) ;
#20484 = DIRECTION ( 'NONE',  ( 0.000000000000000000, -1.000000000000000000, 0.000000000000000000 ) ) ;
#20485 = CIRCLE ( 'NONE', #30820, 1.750000000000001332 ) ;
#20486 = CARTESIAN_POINT ( 'NONE',  ( -12.48409101790999998, -60.16970703802000031, -1.669510252625000080 ) ) ;
#20487 = CARTESIAN_POINT ( 'NONE',  ( -3.536681740116999872, -78.23483721851999917, 9.036735673663999435 ) ) ;
#20488 = CARTESIAN_POINT ( 'NONE',  ( -9.431564212231878130, -79.40938065491944542, -1.151173011385696165 ) ) ;
#20489 = CARTESIAN_POINT ( 'NONE',  ( -1.217465845835396188, -79.97916666666667140, 0.3271848554490955907 ) ) ;
#20490 = TOROIDAL_SURFACE ( 'NONE', #8088, 17.50000000000000000, 5.000000000000000000 ) ;
#20491 = CARTESIAN_POINT ( 'NONE',  ( -10.48543666025111776, -76.85833333333330586, 6.043427764450754580 ) ) ;
#20492 = CARTESIAN_POINT ( 'NONE',  ( -1.605277969432999940, -80.79704884152999966, -0.5682425234610001263 ) ) ;
#20493 = LINE ( 'NONE', #38490, #4424 ) ;
#20494 = CIRCLE ( 'NONE', #57221, 14.00000000000000000 ) ;
#20495 = AXIS2_PLACEMENT_3D ( 'NONE', #54654, #14193, #36636 ) ;
#20496 = CARTESIAN_POINT ( 'NONE',  ( -10.53494359612999887, -55.57285042800999264, 7.618393753177000072 ) ) ;
#20497 = CARTESIAN_POINT ( 'NONE',  ( -9.042797184480999562, -78.47666332859900251, -4.055650103703999143 ) ) ;
#20498 = CARTESIAN_POINT ( 'NONE',  ( 3.140974612311326908, -77.25416666666664867, 11.68767212001979772 ) ) ;
#20499 = CARTESIAN_POINT ( 'NONE',  ( 2.062670899361999766, -23.30639784948999704, -12.83044027760000105 ) ) ;
#20501 = CARTESIAN_POINT ( 'NONE',  ( 1.166929042523999982, -78.97544576573699260, -0.6456414311070999279 ) ) ;
#20500 = FACE_OUTER_BOUND ( 'NONE', #20931, .T. ) ;
#20502 = CARTESIAN_POINT ( 'NONE',  ( 1.243547092045970581, -78.93541666666665435, -9.500000000000000000 ) ) ;
#20503 = CARTESIAN_POINT ( 'NONE',  ( -8.564747023678000559, -80.00360881430898985, 6.787585331471000849 ) ) ;
#20504 = CARTESIAN_POINT ( 'NONE',  ( -0.6878299077642000547, -82.21297074961400142, -1.043738481606000024 ) ) ;
#20505 = CARTESIAN_POINT ( 'NONE',  ( -3.750250575282000121, -2.338355802843000486, 0.6493866540274000343 ) ) ;
#20506 = DIRECTION ( 'NONE',  ( 0.000000000000000000, 0.000000000000000000, -1.000000000000000000 ) ) ;
#20507 = ORIENTED_EDGE ( 'NONE', *, *, #24845, .T. ) ;
#20508 = DIRECTION ( 'NONE',  ( 0.7071067810866970005, -6.386274622742979319E-09, 0.7071067812863980340 ) ) ;
#20509 = ADVANCED_FACE ( 'NONE', ( #10012 ), #40328, .F. ) ;
#20510 = DIRECTION ( 'NONE',  ( 0.000000000000000000, 0.000000000000000000, -1.000000000000000000 ) ) ;
#20511 = CARTESIAN_POINT ( 'NONE',  ( -1.933650113858000230, -55.39213746940999528, 12.70909635752000177 ) ) ;
#20512 = CARTESIAN_POINT ( 'NONE',  ( 1.178220910110199249, -78.37735903784117397, 0.4169870122232715581 ) ) ;
#20513 = CARTESIAN_POINT ( 'NONE',  ( -9.063895419714999235, -79.48202256302897695, -2.955706763204999810 ) ) ;
#20514 = CARTESIAN_POINT ( 'NONE',  ( -8.098724780893656217, -77.04286527309800192, 7.103750973452154227 ) ) ;
#20515 = CARTESIAN_POINT ( 'NONE',  ( -9.237485228140851490, -79.37490541983250125, -3.012313834119925815 ) ) ;
#20516 = CARTESIAN_POINT ( 'NONE',  ( 1.194090705995999979, -61.24031658870000427, 12.43436538493000043 ) ) ;
#20517 = DIRECTION ( 'NONE',  ( -1.000000000000000000, 0.000000000000000000, 0.000000000000000000 ) ) ;
#20518 = CARTESIAN_POINT ( 'NONE',  ( 5.939680743703000668E-14, -6.000000000000000000, 0.000000000000000000 ) ) ;
#20519 = CARTESIAN_POINT ( 'NONE',  ( -0.03769866006636925920, -78.69999999999998863, 3.999822347433480640 ) ) ;
#20520 = CARTESIAN_POINT ( 'NONE',  ( -0.9587802219394000458, -77.48883549249599412, -10.90575368789999899 ) ) ;
#20521 = EDGE_CURVE ( 'NONE', #4032, #10285, #7329, .T. ) ;
#20522 = CARTESIAN_POINT ( 'NONE',  ( -7.719769492146999923, -76.57936687607200099, 7.579341418041000367 ) ) ;
#20523 = CARTESIAN_POINT ( 'NONE',  ( -5.505695391232999114, -78.72709514476063930, -8.014431902511001127 ) ) ;
#20524 = CARTESIAN_POINT ( 'NONE',  ( -2.431761726605123020, -1.043462501739716108, 2.188053907655647556 ) ) ;
#20525 = CARTESIAN_POINT ( 'NONE',  ( -3.831287612370999796, -76.80151196011908610, -8.693171758988999187 ) ) ;
#20526 = CARTESIAN_POINT ( 'NONE',  ( 2.769824414688999870, -79.15904415034599140, -8.825563591736999669 ) ) ;
#20527 = CARTESIAN_POINT ( 'NONE',  ( 10.71369944335146762, -77.37083333333333712, 2.879226727952103548 ) ) ;
#20528 = CARTESIAN_POINT ( 'NONE',  ( 8.058982427891788092, -80.29245933814496539, -7.115972638186089938 ) ) ;
#20529 = CONICAL_SURFACE ( 'NONE', #28049, 9.349999999968000353, 0.7853981633972997312 ) ;
#20530 = CARTESIAN_POINT ( 'NONE',  ( -11.97916666630055715, -76.27916666661793954, 1.256637064247476676 ) ) ;
#20531 = PLANE ( 'NONE',  #24758 ) ;
#20532 = CARTESIAN_POINT ( 'NONE',  ( 8.348735229153000148, -78.87821946291599318, 8.268078378528999295 ) ) ;
#20533 = CARTESIAN_POINT ( 'NONE',  ( 9.499999999999998224, -78.56041666666665435, 1.243547092045980129 ) ) ;
#20534 = CARTESIAN_POINT ( 'NONE',  ( -9.018305195942000196, -79.77230326501299373, 6.745675351750000104 ) ) ;
#20535 = TOROIDAL_SURFACE ( 'NONE', #29901, 1.250000000000000000, 0.5000000000000000000 ) ;
#20536 = ORIENTED_EDGE ( 'NONE', *, *, #15692, .F. ) ;
#20537 = CARTESIAN_POINT ( 'NONE',  ( -0.6484536763399982862, -25.12402982711039812, 12.70397497891742233 ) ) ;
#20538 = EDGE_CURVE ( 'NONE', #17898, #40041, #24085, .T. ) ;
#20539 = ORIENTED_EDGE ( 'NONE', *, *, #7468, .F. ) ;
#20540 = ORIENTED_EDGE ( 'NONE', *, *, #35582, .F. ) ;
#20541 = CARTESIAN_POINT ( 'NONE',  ( 3.031768397182069918, -3.499999999999999556, -1.753150493843362634 ) ) ;
#20542 = CIRCLE ( 'NONE', #54473, 3.399999999999999911 ) ;
#20543 = CARTESIAN_POINT ( 'NONE',  ( 9.396085398178630754, -77.49791666666665435, -7.220923959705230821 ) ) ;
#20544 = CARTESIAN_POINT ( 'NONE',  ( -3.235964442481000347, -78.68248402847228817, 1.036662180689999824 ) ) ;
#20545 = CARTESIAN_POINT ( 'NONE',  ( 9.031152101340357063, -79.17469186335426912, 2.946796958029828772 ) ) ;
#20546 = EDGE_LOOP ( 'NONE', ( #49967, #49588, #13246, #16467 ) ) ;
#20547 = CARTESIAN_POINT ( 'NONE',  ( 0.02044864296007851273, -82.72696752574205448, -1.249602587815580979 ) ) ;
#20548 = ORIENTED_EDGE ( 'NONE', *, *, #36363, .T. ) ;
#20549 = CARTESIAN_POINT ( 'NONE',  ( 3.236394086226999978, -2.780734372332999804, -1.046485274464999948 ) ) ;
#20550 = EDGE_LOOP ( 'NONE', ( #26679, #7018, #11474, #44448 ) ) ;
#20551 = CARTESIAN_POINT ( 'NONE',  ( 1.250000000000000000, -79.34999999999999432, 0.000000000000000000 ) ) ;
#20552 = CARTESIAN_POINT ( 'NONE',  ( 0.3438320055965143895, -78.89273934135498223, -1.494433517359873287 ) ) ;
#20553 = CARTESIAN_POINT ( 'NONE',  ( -5.576379918403213232, -79.79999999999998295, -10.46867297261899488 ) ) ;
#20554 = CARTESIAN_POINT ( 'NONE',  ( -9.416831372289546920, -80.06003372581248811, 5.217560844161510225 ) ) ;
#20555 = FACE_OUTER_BOUND ( 'NONE', #32926, .T. ) ;
#20556 = CARTESIAN_POINT ( 'NONE',  ( -4.028823909683901583, -86.31452042059395069, -0.3856585746546848936 ) ) ;
#20557 = CARTESIAN_POINT ( 'NONE',  ( 11.01994305158000031, -76.63805051245100231, -1.906499110313000234 ) ) ;
#20558 = CARTESIAN_POINT ( 'NONE',  ( 3.687685142782404224, -76.44819997255908106, 10.12799054552703382 ) ) ;
#20559 = CARTESIAN_POINT ( 'NONE',  ( -1.506676414812727183, -81.35541669807993514, -0.1142558127726139849 ) ) ;
#20560 = CARTESIAN_POINT ( 'NONE',  ( 7.516229220974000924, -76.00797436215698610, -8.092172198832999541 ) ) ;
#20561 = CARTESIAN_POINT ( 'NONE',  ( -1.799702852821704058, -78.70948991200978639, -9.073181958675275993 ) ) ;
#20562 = CARTESIAN_POINT ( 'NONE',  ( 1.313995274498999999, -80.41443998845899443, -0.2280190045613000038 ) ) ;
#20563 = CARTESIAN_POINT ( 'NONE',  ( -8.343860018000999190, -60.54999999966955926, -8.343860018000999190 ) ) ;
#20564 = CARTESIAN_POINT ( 'NONE',  ( 1.243547092045928615, -77.16458333333332575, 9.500000000000003553 ) ) ;
#20565 = CARTESIAN_POINT ( 'NONE',  ( 3.579475725212000192, -79.27942549782629555, 0.2666292237523999464 ) ) ;
#20566 = CARTESIAN_POINT ( 'NONE',  ( 4.732552697730000091, -79.16556358023599671, -11.24509117424000060 ) ) ;
#20567 = CARTESIAN_POINT ( 'NONE',  ( -10.54480093980093791, -78.08451164641000730, 2.090071665737717410 ) ) ;
#20568 = CARTESIAN_POINT ( 'NONE',  ( 0.2494208068312679105, -24.99288960763016831, -12.50614183112954336 ) ) ;
#20569 = DIRECTION ( 'NONE',  ( -1.000000000000000000, 0.000000000000000000, 0.000000000000000000 ) ) ;
#20570 = CARTESIAN_POINT ( 'NONE',  ( 3.544223523194999892, -82.50274735065200105, -0.05576259466792000269 ) ) ;
#20571 = CARTESIAN_POINT ( 'NONE',  ( -0.7681833999686477066, -80.42708333333334281, 0.9995835529977223910 ) ) ;
#20572 = CARTESIAN_POINT ( 'NONE',  ( 6.232755757386176043, -78.94717033289664698, 9.960036924250847079 ) ) ;
#20573 = CARTESIAN_POINT ( 'NONE',  ( 5.413904038987148226, -80.16666666666664298, -9.393203674808285442 ) ) ;
#20574 = EDGE_CURVE ( 'NONE', #456, #55491, #4988, .T. ) ;
#20575 = DIRECTION ( 'NONE',  ( 0.000000000000000000, -1.000000000000000000, 0.000000000000000000 ) ) ;
#20576 = CARTESIAN_POINT ( 'NONE',  ( 0.7341740840635999632, -80.80573051437600895, -1.113348630318000021 ) ) ;
#20577 = ADVANCED_FACE ( 'NONE', ( #25532 ), #16970, .F. ) ;
#20578 = CARTESIAN_POINT ( 'NONE',  ( -1.500000000000000222, -80.41041666666666288, -0.1963495408493622363 ) ) ;
#20579 = CARTESIAN_POINT ( 'NONE',  ( 0.000000000000000000, -75.15999999999999659, 0.000000000000000000 ) ) ;
#20580 = CARTESIAN_POINT ( 'NONE',  ( -10.25114915300409280, -77.97533825987605383, -3.311110282731340337 ) ) ;
#20581 = CARTESIAN_POINT ( 'NONE',  ( -7.223656224191105757, -78.27159733532405994, -9.395165950963319190 ) ) ;
#20582 = VECTOR ( 'NONE', #47031, 1000.000000000000114 ) ;
#20583 = CARTESIAN_POINT ( 'NONE',  ( 0.5222397221644492493, -25.16298219402098013, -12.70447686583673708 ) ) ;
#20584 = CARTESIAN_POINT ( 'NONE',  ( -6.672837361367000675, -75.65930287300999169, -9.910479691896998844 ) ) ;
#20585 = ORIENTED_EDGE ( 'NONE', *, *, #10925, .F. ) ;
#20586 = CARTESIAN_POINT ( 'NONE',  ( -9.421357847594000745, -80.29617642373133890, -6.176342950743000770 ) ) ;
#20587 = CARTESIAN_POINT ( 'NONE',  ( -4.505191439890000815, -80.18390435543939532, 10.47810291308999986 ) ) ;
#20588 = EDGE_CURVE ( 'NONE', #38869, #1755, #7152, .T. ) ;
#20589 = CARTESIAN_POINT ( 'NONE',  ( -11.00000000000000000, -18.25000000000000000, 0.000000000000000000 ) ) ;
#20590 = CARTESIAN_POINT ( 'NONE',  ( -12.78963794847000024, -78.58340606474000367, -0.3129899442943999688 ) ) ;
#20591 = CARTESIAN_POINT ( 'NONE',  ( 0.000000000000000000, -3.000000000000000000, -12.90000000000398472 ) ) ;
#20592 = CARTESIAN_POINT ( 'NONE',  ( 1.475792658273999969, -77.53030449881099173, -9.517102871385000995 ) ) ;
#20593 = CARTESIAN_POINT ( 'NONE',  ( 0.5021253177900999454, -82.03818896268001026, -1.588436081161999969 ) ) ;
#20594 = CARTESIAN_POINT ( 'NONE',  ( -1.575545371556065222, -79.98714921115445975, 10.63364149761491362 ) ) ;
#20595 = LINE ( 'NONE', #29434, #3783 ) ;
#20596 = EDGE_LOOP ( 'NONE', ( #40691, #33774, #27633, #36794, #16268 ) ) ;
#20597 = DIRECTION ( 'NONE',  ( 0.000000000000000000, -1.000000000000000000, 0.000000000000000000 ) ) ;
#20598 = CARTESIAN_POINT ( 'NONE',  ( -1.937220121396670214, -78.81741337217214038, -2.837945647007499961 ) ) ;
#20599 = ORIENTED_EDGE ( 'NONE', *, *, #34985, .F. ) ;
#20600 = CARTESIAN_POINT ( 'NONE',  ( -1.293339008660999934, -78.48638398745899281, -10.86347506762000137 ) ) ;
#20601 = CARTESIAN_POINT ( 'NONE',  ( 8.097906714174317955, -77.70861376145681731, -4.629560367825112266 ) ) ;
#20602 = CARTESIAN_POINT ( 'NONE',  ( 0.03580840776424319000, -80.72793405598493166, -1.249249415733939994 ) ) ;
#20603 = ORIENTED_EDGE ( 'NONE', *, *, #7583, .T. ) ;
#20604 = CARTESIAN_POINT ( 'NONE',  ( -11.29558555235000128, -78.05148038169298275, 0.7758774409984000586 ) ) ;
#20605 = ORIENTED_EDGE ( 'NONE', *, *, #24089, .T. ) ;
#20606 = VERTEX_POINT ( 'NONE', #21106 ) ;
#20607 = AXIS2_PLACEMENT_3D ( 'NONE', #20579, #56884, #38577 ) ;
#20608 = CARTESIAN_POINT ( 'NONE',  ( -0.8876925766968319920, -80.53848003073616724, 0.8795304379308518383 ) ) ;
#20609 = CARTESIAN_POINT ( 'NONE',  ( 1.247385803315000041, -61.27722255996999934, 12.50301438880000049 ) ) ;
#20610 = CARTESIAN_POINT ( 'NONE',  ( 3.269429986698999979, -79.97799869236203563, 9.203886808668999109 ) ) ;
#20611 = ORIENTED_EDGE ( 'NONE', *, *, #76, .F. ) ;
#20612 = CARTESIAN_POINT ( 'NONE',  ( 4.654517711782999889, -79.41335789300599401, 9.874757255799998745 ) ) ;
#20613 = B_SPLINE_CURVE_WITH_KNOTS ( 'NONE', 3,
 ( #43515, #21644, #34634, #3641, #39076, #16937, #39651, #29340, #26066, #20502, #25209, #3076, #7498, #25496, #34054, #16649, #11933, #29911 ),
 .UNSPECIFIED., .F., .F.,
 ( 4, 2, 2, 2, 2, 2, 2, 2, 4 ),
 ( 0.000000000000000000, 0.1250000000000000833, 0.2500000000000001665, 0.3750000000000002220, 0.5000000000000002220, 0.6250000000000002220, 0.7500000000000001110, 0.8750000000000001110, 1.000000000000000000 ),
 .UNSPECIFIED. ) ;
#20614 = VERTEX_POINT ( 'NONE', #39405 ) ;
#20615 = CARTESIAN_POINT ( 'NONE',  ( -12.02296678431999943, -78.53420637899631629, 2.418109797047000242 ) ) ;
#20616 = CARTESIAN_POINT ( 'NONE',  ( 9.136202122873999798, -77.28179415034600197, 2.585973524422000125 ) ) ;
#20617 = EDGE_CURVE ( 'NONE', #13297, #48890, #7822, .T. ) ;
#20618 = CARTESIAN_POINT ( 'NONE',  ( 0.000000000000000000, -3.500000000000000000, -8.500000000000000000 ) ) ;
#20619 = VECTOR ( 'NONE', #28973, 1000.000000000000114 ) ;
#20620 = CARTESIAN_POINT ( 'NONE',  ( 8.266608573609707022, -17.02766203690127966, -9.697383820329660509 ) ) ;
#20621 = DIRECTION ( 'NONE',  ( 0.7071067811865474617, 0.000000000000000000, 0.7071067811865474617 ) ) ;
#20622 = DIRECTION ( 'NONE',  ( 0.000000000000000000, -1.000000000000000000, 0.000000000000000000 ) ) ;
#20623 = DIRECTION ( 'NONE',  ( -1.000000000000000000, 0.000000000000000000, 0.000000000000000000 ) ) ;
#20624 = CARTESIAN_POINT ( 'NONE',  ( 0.9627474882855999727, -78.28140245315898937, -11.94107121277999894 ) ) ;
#20625 = CARTESIAN_POINT ( 'NONE',  ( 1.232251595443166980, -82.14947918407371219, -3.818482668381804501 ) ) ;
#20626 = CARTESIAN_POINT ( 'NONE',  ( 1.623944433304999935, -76.08352863036999736, -12.20239005717999881 ) ) ;
#20627 = CARTESIAN_POINT ( 'NONE',  ( -4.167886093573000217, -80.20807046129100115, 0.1878047563862999814 ) ) ;
#20628 = CARTESIAN_POINT ( 'NONE',  ( -0.1240611623467000046, -77.94466001420200030, -9.871970996624998662 ) ) ;
#20629 = CARTESIAN_POINT ( 'NONE',  ( 10.36292431360000066, -60.00096201600999990, -7.633479737330000070 ) ) ;
#20630 = CARTESIAN_POINT ( 'NONE',  ( -10.61911868076999887, -78.48968720768000651, -6.134606423928000041 ) ) ;
#20631 = CARTESIAN_POINT ( 'NONE',  ( 12.50000000000000000, -60.04999999657000131, 1.750000000000000000 ) ) ;
#20632 = DIRECTION ( 'NONE',  ( 1.000000000000000000, 0.000000000000000000, 0.000000000000000000 ) ) ;
#20633 = CARTESIAN_POINT ( 'NONE',  ( -7.374560639698971798, -77.87291666666668277, -9.596002108778163731 ) ) ;
#20634 = VERTEX_POINT ( 'NONE', #39112 ) ;
#20636 = EDGE_CURVE ( 'NONE', #32917, #23434, #4318, .T. ) ;
#20635 = CARTESIAN_POINT ( 'NONE',  ( 1.500158885365614037, -79.99082255360691818, -0.1727759592422631052 ) ) ;
#20637 = CARTESIAN_POINT ( 'NONE',  ( 7.418149392330000147, -77.15334168688949035, -5.919552685632999633 ) ) ;
#20638 = DIRECTION ( 'NONE',  ( -1.000000000000000000, 0.000000000000000000, 0.000000000000000000 ) ) ;
#20639 = CARTESIAN_POINT ( 'NONE',  ( 11.36512682855729750, -78.67683455540999660, 3.982123233433211063 ) ) ;
#20640 = CARTESIAN_POINT ( 'NONE',  ( -2.418807028576000384, -2.534049145665999703, -2.608992216514999907 ) ) ;
#20641 = CARTESIAN_POINT ( 'NONE',  ( 7.024610939158000278, -78.61512485273199502, -9.931634882699999167 ) ) ;
#20642 = CARTESIAN_POINT ( 'NONE',  ( -9.190938788893999956, -78.74397594943899037, 3.222784492720999872 ) ) ;
#20643 = AXIS2_PLACEMENT_3D ( 'NONE', #42858, #23960, #41979 ) ;
#20645 = CARTESIAN_POINT ( 'NONE',  ( -0.5931688960305999681, -78.65405146749098719, 1.178438064142999897 ) ) ;
#20644 = CARTESIAN_POINT ( 'NONE',  ( -9.730498664387607022, -76.15210458349736200, 6.585771582669669222 ) ) ;
#20646 = CARTESIAN_POINT ( 'NONE',  ( -0.6675286376147999690, -83.05589043469399257, 1.308112063971999861 ) ) ;
#20647 = CARTESIAN_POINT ( 'NONE',  ( -10.56288039171200488, -79.58526307256707355, 1.996919741384027835 ) ) ;
#20648 = ORIENTED_EDGE ( 'NONE', *, *, #26789, .T. ) ;
#20649 = CARTESIAN_POINT ( 'NONE',  ( 0.000000000000000000, -1.000000000000000000, 0.000000000000000000 ) ) ;
#20650 = CARTESIAN_POINT ( 'NONE',  ( -12.15598897987000093, -79.25941268769399528, -0.08388850244461000527 ) ) ;
#20651 = CARTESIAN_POINT ( 'NONE',  ( 9.425379270812129562, -79.01124851720528852, 1.342142796262536963 ) ) ;
#20652 = EDGE_CURVE ( 'NONE', #39067, #55619, #57693, .T. ) ;
#20653 = CARTESIAN_POINT ( 'NONE',  ( -1.881081600302069390, -79.78749999999999432, 11.88906204917373088 ) ) ;
#20654 = DIRECTION ( 'NONE',  ( 1.000000000000000000, 0.000000000000000000, 0.000000000000000000 ) ) ;
#20655 = DIRECTION ( 'NONE',  ( 0.000000000000000000, 1.000000000000000000, 0.000000000000000000 ) ) ;
#20656 = CARTESIAN_POINT ( 'NONE',  ( 3.149121100232000092, -79.92747424662198341, 9.026342880292000714 ) ) ;
#20657 = CARTESIAN_POINT ( 'NONE',  ( 7.660411364622000008, -18.80826384815000196, -10.01752038683000023 ) ) ;
#20658 = CARTESIAN_POINT ( 'NONE',  ( -5.539808784079886195, -78.68333333333332291, -9.611650271896841957 ) ) ;
#20659 = VERTEX_POINT ( 'NONE', #10892 ) ;
#20660 = CARTESIAN_POINT ( 'NONE',  ( 5.177840772445237327, -76.68658294577745949, 9.913027470100756133 ) ) ;
#20661 = AXIS2_PLACEMENT_3D ( 'NONE', #11914, #8336, #35182 ) ;
#20662 = CARTESIAN_POINT ( 'NONE',  ( 9.594300353386179481, -79.34959433123279382, 6.930735968784434320 ) ) ;
#20663 = CARTESIAN_POINT ( 'NONE',  ( 8.266198729306507786, -79.50520833333278858, -4.776057930729986190 ) ) ;
#20665 = CARTESIAN_POINT ( 'NONE',  ( 0.7780701227561770406, -81.42184096910574453, 0.9786064938539484892 ) ) ;
#20664 = CARTESIAN_POINT ( 'NONE',  ( 0.8866125316423000280, -81.47441317628999968, 0.9769768825355000796 ) ) ;
#20666 = EDGE_LOOP ( 'NONE', ( #43748, #17476, #47135, #50466, #24679 ) ) ;
#20667 = CARTESIAN_POINT ( 'NONE',  ( -0.7109705001964822246, -78.57228594746854355, 1.058387015174929280 ) ) ;
#20668 = CARTESIAN_POINT ( 'NONE',  ( 1.250000000000000000, -82.34999999999999432, 0.000000000000000000 ) ) ;
#20669 = CARTESIAN_POINT ( 'NONE',  ( 12.50385649911367558, -61.58436722984664158, 0.8579675320881684497 ) ) ;
#20670 = DIRECTION ( 'NONE',  ( -0.7071067811865475727, 0.000000000000000000, -0.7071067811865475727 ) ) ;
#20671 = DIRECTION ( 'NONE',  ( 0.000000000000000000, 0.000000000000000000, -1.000000000000000000 ) ) ;
#20672 = B_SPLINE_CURVE_WITH_KNOTS ( 'NONE', 3,
 ( #35911, #53944, #18225, #13478 ),
 .UNSPECIFIED., .F., .F.,
 ( 4, 4 ),
 ( 0.000000000000000000, 1.000000000000000000 ),
 .UNSPECIFIED. ) ;
#20673 = CARTESIAN_POINT ( 'NONE',  ( 6.728605944993000243, -79.39502093716299669, -7.080011783993000130 ) ) ;
#20674 = VERTEX_POINT ( 'NONE', #44128 ) ;
#20675 = VERTEX_POINT ( 'NONE', #24456 ) ;
#20676 = CARTESIAN_POINT ( 'NONE',  ( -1.955611496805000238, -76.87133267504599132, -12.31633344284000131 ) ) ;
#20677 = CARTESIAN_POINT ( 'NONE',  ( -5.302235804606764802, -78.68411842716731996, -9.360073049705164294 ) ) ;
#20678 = ORIENTED_EDGE ( 'NONE', *, *, #55095, .T. ) ;
#20679 = CARTESIAN_POINT ( 'NONE',  ( 7.659225706236999720, -18.31732796024000010, 9.963487823496000928 ) ) ;
#20680 = EDGE_CURVE ( 'NONE', #43698, #14636, #8605, .T. ) ;
#20681 = CARTESIAN_POINT ( 'NONE',  ( 10.99999999999999822, -77.46041666666667425, 1.439896632895345086 ) ) ;
#20682 = CIRCLE ( 'NONE', #39508, 2.299999999999999822 ) ;
#20683 = CARTESIAN_POINT ( 'NONE',  ( 1.811016405462537060, -54.73826444594539709, 12.71771640060721964 ) ) ;
#20684 = CARTESIAN_POINT ( 'NONE',  ( 11.60238327475000197, -76.95322811118001027, 5.404242916298000132 ) ) ;
#20685 = EDGE_CURVE ( 'NONE', #32066, #38434, #17703, .T. ) ;
#20686 = CARTESIAN_POINT ( 'NONE',  ( 7.646944885454000307, -59.99635956511999524, 10.19022188675999985 ) ) ;
#20687 = DIRECTION ( 'NONE',  ( 2.678911359553000079E-11, -1.000000000000000000, -2.678926851037000120E-11 ) ) ;
#20688 = DIRECTION ( 'NONE',  ( 0.000000000000000000, 1.000000000000000000, 0.000000000000000000 ) ) ;
#20689 = CARTESIAN_POINT ( 'NONE',  ( -5.268979267983999293, -78.74780710420199625, 9.902321347348999936 ) ) ;
#20690 = CARTESIAN_POINT ( 'NONE',  ( 1.249999999999999778, -81.26041666666667140, 0.1636246173744711763 ) ) ;
#20691 = ORIENTED_EDGE ( 'NONE', *, *, #15907, .F. ) ;
#20692 = LINE ( 'NONE', #52281, #19946 ) ;
#20693 = ORIENTED_EDGE ( 'NONE', *, *, #23477, .F. ) ;
#20694 = CARTESIAN_POINT ( 'NONE',  ( 3.218370493427320067, -77.25342817773334048, -8.672750898853246682 ) ) ;
#20695 = CARTESIAN_POINT ( 'NONE',  ( 0.6128924939060999000, -80.13674016633599706, 1.278445216313999877 ) ) ;
#20696 = VECTOR ( 'NONE', #30578, 1000.000000000000000 ) ;
#20697 = DIRECTION ( 'NONE',  ( -0.7071067811865475727, 0.000000000000000000, -0.7071067811865475727 ) ) ;
#20698 = CARTESIAN_POINT ( 'NONE',  ( -1.376714249866999973, -78.01290954478920980, 0.6352952275891999845 ) ) ;
#20699 = CARTESIAN_POINT ( 'NONE',  ( -7.639893274949090873, -60.18715751166916306, -10.11462445492871787 ) ) ;
#20700 = AXIS2_PLACEMENT_3D ( 'NONE', #17865, #35855, #53884 ) ;
#20701 = CARTESIAN_POINT ( 'NONE',  ( -0.5563122350442734065, -81.58886627922497325, -1.147641270936760716 ) ) ;
#20702 = CARTESIAN_POINT ( 'NONE',  ( -1.462188802161999979, -79.42500599778999515, -0.7147474581103999691 ) ) ;
#20703 = CARTESIAN_POINT ( 'NONE',  ( -5.869402599192000025, -78.36567021304000491, 10.46661899222999992 ) ) ;
#20704 = CARTESIAN_POINT ( 'NONE',  ( -2.948156184611000263, -78.88955604921899578, 10.64829886688000116 ) ) ;
#20705 = CARTESIAN_POINT ( 'NONE',  ( -11.60111135005000094, -79.17129902871758418, -3.181408645392000523 ) ) ;
#20706 = DIRECTION ( 'NONE',  ( -1.000000000000000000, 0.000000000000000000, 0.000000000000000000 ) ) ;
#20707 = CARTESIAN_POINT ( 'NONE',  ( -12.50000000000000000, -61.48359816765000119, -1.003641516062000250 ) ) ;
#20708 = ORIENTED_EDGE ( 'NONE', *, *, #35264, .T. ) ;
#20710 = EDGE_CURVE ( 'NONE', #3549, #52628, #18722, .T. ) ;
#20709 = CARTESIAN_POINT ( 'NONE',  ( -1.405367936307999832, -81.36885036431999652, -0.7351702954167999016 ) ) ;
#20711 = CARTESIAN_POINT ( 'NONE',  ( -1.240843214692000096, -81.55232256240998368, -0.5344114414419000036 ) ) ;
#20712 = LINE ( 'NONE', #52305, #29479 ) ;
#20713 = CARTESIAN_POINT ( 'NONE',  ( -4.743879332790999825, -78.59091760875300281, -11.00053059214000051 ) ) ;
#20714 = CARTESIAN_POINT ( 'NONE',  ( 5.285315739688693171, -77.00000000000001421, 7.652295706397369557 ) ) ;
#20715 = CARTESIAN_POINT ( 'NONE',  ( 0.7076411874954000591, -82.87108743283400258, -1.508144869335000138 ) ) ;
#20716 = CARTESIAN_POINT ( 'NONE',  ( 3.342812627361237521, -2.025386568323031433, 1.104663108944964556 ) ) ;
#20717 = CARTESIAN_POINT ( 'NONE',  ( 6.584508673715999905, -78.44585194988499666, 7.154582167228999978 ) ) ;
#20718 = CARTESIAN_POINT ( 'NONE',  ( -0.5444512524326000635, -77.76350959400299701, -9.506521396690999381 ) ) ;
#20719 = CARTESIAN_POINT ( 'NONE',  ( -0.6953472622417047333, -81.17859467677989471, -1.050534455880961060 ) ) ;
#20720 = CARTESIAN_POINT ( 'NONE',  ( 7.307192483546000261, -77.20994809191398645, -8.110505779365999146 ) ) ;
#20721 = CARTESIAN_POINT ( 'NONE',  ( 10.75000000000000355, -79.23958333333332860, -1.407171709420407035 ) ) ;
#20722 = CARTESIAN_POINT ( 'NONE',  ( -3.115648671636999989, -80.92463538950839563, 10.45640090600000072 ) ) ;
#20723 = CARTESIAN_POINT ( 'NONE',  ( 0.1243515176670834943, -80.78259192502341079, -1.268026773355690473 ) ) ;
#20724 = ORIENTED_EDGE ( 'NONE', *, *, #28645, .F. ) ;
#20725 = DIRECTION ( 'NONE',  ( 0.000000000000000000, 0.000000000000000000, -1.000000000000000000 ) ) ;
#20726 = CARTESIAN_POINT ( 'NONE',  ( 7.216714108252452853, -77.02036381975230483, 9.394814173648345701 ) ) ;
#20727 = CARTESIAN_POINT ( 'NONE',  ( -1.460729357734999789, -60.89091243169999501, -12.44211643244000065 ) ) ;
#20728 = CARTESIAN_POINT ( 'NONE',  ( 0.000000000000000000, -75.15999999999999659, 0.000000000000000000 ) ) ;
#20729 = EDGE_CURVE ( 'NONE', #4628, #56848, #39360, .T. ) ;
#20730 = CARTESIAN_POINT ( 'NONE',  ( 10.29113596735999892, -77.54866276469599029, 4.462133020506000136 ) ) ;
#20731 = CARTESIAN_POINT ( 'NONE',  ( -3.548303639235999896, -79.46865131509198932, -10.38621961377000069 ) ) ;
#20732 = CARTESIAN_POINT ( 'NONE',  ( 9.835223439032999337, -24.08138927656000305, -7.760980897158999525 ) ) ;
#20733 = EDGE_CURVE ( 'NONE', #58285, #53612, #3960, .T. ) ;
#20734 = CARTESIAN_POINT ( 'NONE',  ( 4.019001026802343723, -83.98020833014430764, 0.5171148167050576561 ) ) ;
#20735 = CARTESIAN_POINT ( 'NONE',  ( -2.462645637647999930, -77.18535259911799074, -11.90051400241999957 ) ) ;
#20736 = CARTESIAN_POINT ( 'NONE',  ( 11.74786300771494219, -78.44881845960851763, 0.3511192646659174188 ) ) ;
#20737 = CARTESIAN_POINT ( 'NONE',  ( 4.009346575041191407, -79.10969738753867375, -8.520289397331099579 ) ) ;
#20738 = ORIENTED_EDGE ( 'NONE', *, *, #45034, .F. ) ;
#20739 = CARTESIAN_POINT ( 'NONE',  ( -1.250000000000000000, -77.71666666666666856, 0.000000000000000000 ) ) ;
#20740 = CARTESIAN_POINT ( 'NONE',  ( -9.611650271896857944, -78.15833333333333144, 5.539808784079855997 ) ) ;
#20741 = CARTESIAN_POINT ( 'NONE',  ( -2.205131412320000095, -78.13389367123097884, 10.93750404997000025 ) ) ;
#20742 = CARTESIAN_POINT ( 'NONE',  ( 7.919595949288999570, -55.65000000488999632, 8.768124086549999419 ) ) ;
#20743 = CARTESIAN_POINT ( 'NONE',  ( -11.75000000000000711, -77.78958333333332575, 1.538071403319954955 ) ) ;
#20744 = CARTESIAN_POINT ( 'NONE',  ( -7.686918321195999937, -58.55560170965000566, -10.48771805380999922 ) ) ;
#20745 = VECTOR ( 'NONE', #52617, 1000.000000000000000 ) ;
#20746 = CARTESIAN_POINT ( 'NONE',  ( -1.528577347423822896, -82.33719591969246210, 0.2446291273937655775 ) ) ;
#20747 = CARTESIAN_POINT ( 'NONE',  ( 0.5145317771005305518, -79.75915092270044227, -1.139023839920036529 ) ) ;
#20748 = ADVANCED_FACE ( 'NONE', ( #32271 ), #8686, .T. ) ;
#20749 = VERTEX_POINT ( 'NONE', #49735 ) ;
#20750 = CARTESIAN_POINT ( 'NONE',  ( 1.667961430005999945, -20.25111654322000021, 12.58335110166999904 ) ) ;
#20751 = CARTESIAN_POINT ( 'NONE',  ( -9.250000000000000000, -78.99999999999998579, 0.000000000000000000 ) ) ;
#20752 = VERTEX_POINT ( 'NONE', #54729 ) ;
#20753 = ORIENTED_EDGE ( 'NONE', *, *, #20888, .F. ) ;
#20754 = CARTESIAN_POINT ( 'NONE',  ( -12.54976795928000044, -53.75224499974000025, 0.05636009750359999987 ) ) ;
#20755 = VERTEX_POINT ( 'NONE', #49438 ) ;
#20756 = ORIENTED_EDGE ( 'NONE', *, *, #26342, .T. ) ;
#20757 = CARTESIAN_POINT ( 'NONE',  ( 10.19019669286999985, -23.19643762568000156, 7.646965578493999161 ) ) ;
#20758 = CARTESIAN_POINT ( 'NONE',  ( 8.060704535212000366, -77.76451158974199984, -7.362092663522999736 ) ) ;
#20759 = DIRECTION ( 'NONE',  ( 0.9999999930530777403, 0.000000000000000000, 0.0001178721535675973718 ) ) ;
#20760 = EDGE_CURVE ( 'NONE', #3286, #15875, #5062, .T. ) ;
#20761 = CARTESIAN_POINT ( 'NONE',  ( -9.170454433240001535, -79.22593667140100138, 3.758088286126999744 ) ) ;
#20762 = CARTESIAN_POINT ( 'NONE',  ( 1.809879502519539995, -78.24079858881482608, -9.071132683527801888 ) ) ;
#20763 = CARTESIAN_POINT ( 'NONE',  ( 6.349001246031294343, -76.28437500015692763, -8.735174149410413591 ) ) ;
#20764 = EDGE_LOOP ( 'NONE', ( #41481, #2123, #44770, #44487, #22336 ) ) ;
#20765 = CONICAL_SURFACE ( 'NONE', #49043, 1.099999997149000430, 0.7853981633972997312 ) ;
#20766 = EDGE_LOOP ( 'NONE', ( #29737, #48110, #44713, #7660, #46781 ) ) ;
#20767 = CARTESIAN_POINT ( 'NONE',  ( -7.047464712085933947, -77.54400991620123307, 5.991240863339566403 ) ) ;
#20768 = CARTESIAN_POINT ( 'NONE',  ( -1.471932811527529195, -79.01769483858601006, -0.3335056313496183034 ) ) ;
#20769 = DIRECTION ( 'NONE',  ( -0.9999999999998321343, 0.000000000000000000, -5.794540613806191565E-07 ) ) ;
#20770 = CARTESIAN_POINT ( 'NONE',  ( 4.545264886168000729, -77.66636063594098971, 8.573871732259998879 ) ) ;
#20771 = CARTESIAN_POINT ( 'NONE',  ( 1.592434616855211038, -86.12610001270965654, 3.669353075276090781 ) ) ;
#20772 = CARTESIAN_POINT ( 'NONE',  ( -9.250000000000000000, -77.50056085624700586, -0.06519332902036732713 ) ) ;
#20773 = CARTESIAN_POINT ( 'NONE',  ( 0.7681833999686413783, -79.82291666666668561, 0.9995835529977274980 ) ) ;
#20774 = CARTESIAN_POINT ( 'NONE',  ( -7.179058446792000225, -79.93980297709798322, -8.667882172381000672 ) ) ;
#20775 = CARTESIAN_POINT ( 'NONE',  ( -0.8549356769920000154, -79.78634392611000692, -1.335470596990000036 ) ) ;
#20776 = PLANE ( 'NONE',  #18597 ) ;
#20777 = CARTESIAN_POINT ( 'NONE',  ( 1.021232999834709165, -79.43413075375887900, -1.113201301497944717 ) ) ;
#20778 = CARTESIAN_POINT ( 'NONE',  ( -5.708830652390999738, -77.86696332859899883, 8.101181774151999804 ) ) ;
#20779 = DIRECTION ( 'NONE',  ( -1.000000000000000000, 0.000000000000000000, 0.000000000000000000 ) ) ;
#20780 = CARTESIAN_POINT ( 'NONE',  ( 1.799502287743000029, -23.30716934606000024, -12.60413652831999975 ) ) ;
#20781 = CIRCLE ( 'NONE', #4769, 0.8000000000000011546 ) ;
#20783 = CARTESIAN_POINT ( 'NONE',  ( 1.576170184332999824, -17.83913032783999952, -12.55466896104999996 ) ) ;
#20782 = CARTESIAN_POINT ( 'NONE',  ( 7.919595949288999570, -55.65000000893999754, 9.050966798898000931 ) ) ;
#20784 = CARTESIAN_POINT ( 'NONE',  ( 11.75000000000000000, -75.95000000000000284, 0.000000000000000000 ) ) ;
#20785 = CARTESIAN_POINT ( 'NONE',  ( -0.2814639899600999695, -80.05216315943599170, -11.06814981317999980 ) ) ;
#20786 = CARTESIAN_POINT ( 'NONE',  ( -8.190859204290999784, -55.64999999967000122, -7.342331066867000544 ) ) ;
#20787 = CARTESIAN_POINT ( 'NONE',  ( 1.271520795309928120, -1.404249853560488814, -3.289139988056414943 ) ) ;
#20788 = EDGE_LOOP ( 'NONE', ( #3930, #36929 ) ) ;
#20789 = CARTESIAN_POINT ( 'NONE',  ( 7.102903299382745672, -80.31775757425651818, 8.111946779019859832 ) ) ;
#20790 = DIRECTION ( 'NONE',  ( 0.000000000000000000, -1.000000000000000000, 0.000000000000000000 ) ) ;
#20791 = CARTESIAN_POINT ( 'NONE',  ( 0.8550973397286725231, -78.41513696957164825, 0.9116979360512381669 ) ) ;
#20792 = CARTESIAN_POINT ( 'NONE',  ( -1.611853968441999907, -2.220016836959000539, -3.270131938172000208 ) ) ;
#20793 = CARTESIAN_POINT ( 'NONE',  ( 3.376184802135000051, -79.73959606308299897, 9.032146306647000245 ) ) ;
#20794 = CARTESIAN_POINT ( 'NONE',  ( -10.75000000000000000, -77.10000000000000853, 0.000000000000000000 ) ) ;
#20795 = CARTESIAN_POINT ( 'NONE',  ( 9.549999999999998934, -79.99999999999998579, 0.000000000000000000 ) ) ;
#20796 = CARTESIAN_POINT ( 'NONE',  ( -0.9218200799623716968, -80.07291666666667140, -1.199500263597270910 ) ) ;
#20797 = CARTESIAN_POINT ( 'NONE',  ( 0.000000000000000000, -5.899999999999999467, 0.000000000000000000 ) ) ;
#20798 = CARTESIAN_POINT ( 'NONE',  ( 2.879226727952094222, -77.34583333333328881, -10.71369944335146940 ) ) ;
#20799 = DIRECTION ( 'NONE',  ( 1.205461585547979389E-11, 1.868136279038964309E-07, -0.9999999999999824585 ) ) ;
#20800 = CARTESIAN_POINT ( 'NONE',  ( 2.961948693619000039, -77.45351946037798996, -10.65246418773999970 ) ) ;
#20801 = CARTESIAN_POINT ( 'NONE',  ( 7.853292460675339370, -76.38309044374258860, -8.740604184407734678 ) ) ;
#20802 = CARTESIAN_POINT ( 'NONE',  ( 10.27624888046999985, -77.92720206157000007, -4.318947732659999872 ) ) ;
#20803 = DIRECTION ( 'NONE',  ( 0.000000000000000000, 0.000000000000000000, -1.000000000000000000 ) ) ;
#20804 = CARTESIAN_POINT ( 'NONE',  ( 0.4193126674068999860, -78.47530136235999976, -1.609880760976999836 ) ) ;
#20805 = CARTESIAN_POINT ( 'NONE',  ( -2.880544446985999762, -76.87051800811249791, -9.112186890989001142 ) ) ;
#20806 = DIRECTION ( 'NONE',  ( -1.000000000000000000, 0.000000000000000000, 0.000000000000000000 ) ) ;
#20807 = CARTESIAN_POINT ( 'NONE',  ( -1.735649827337248263, -0.8020833187308676893, -3.013068263282779213 ) ) ;
#20808 = CARTESIAN_POINT ( 'NONE',  ( 6.913388667549481781, -80.28076439126193975, -8.232022196888907573 ) ) ;
#20809 = CARTESIAN_POINT ( 'NONE',  ( -8.803761571656083973, -16.78431590349724445, -9.164326402687485995 ) ) ;
#20810 = ADVANCED_FACE ( 'NONE', ( #454 ), #20535, .F. ) ;
#20811 = VERTEX_POINT ( 'NONE', #165 ) ;
#20812 = CARTESIAN_POINT ( 'NONE',  ( -11.95950202284999975, -78.98973269472499226, 1.295167635372999948 ) ) ;
#20813 = CARTESIAN_POINT ( 'NONE',  ( 1.249999999999999778, -81.76041666666665719, 0.1636246173744711763 ) ) ;
#20814 = CARTESIAN_POINT ( 'NONE',  ( 6.907293935673000540, -79.14586737597099386, 8.895125352942999442 ) ) ;
#20815 = EDGE_LOOP ( 'NONE', ( #4714, #37482, #55598, #10311 ) ) ;
#20816 = CARTESIAN_POINT ( 'NONE',  ( -0.2678032735367172346, -25.21432775288745276, 12.70526550769160323 ) ) ;
#20817 = AXIS2_PLACEMENT_3D ( 'NONE', #282, #18260, #54275 ) ;
#20818 = VERTEX_POINT ( 'NONE', #22851 ) ;
#20819 = ORIENTED_EDGE ( 'NONE', *, *, #11193, .F. ) ;
#20820 = AXIS2_PLACEMENT_3D ( 'NONE', #37679, #42703, #28220 ) ;
#20821 = CARTESIAN_POINT ( 'NONE',  ( 3.321932689531000182, -77.19999999999998863, 10.22385755016999909 ) ) ;
#20822 = CARTESIAN_POINT ( 'NONE',  ( -5.917523019358058356, -77.38333333333329733, -10.26699006316253282 ) ) ;
#20823 = EDGE_CURVE ( 'NONE', #54925, #19957, #13396, .T. ) ;
#20824 = CARTESIAN_POINT ( 'NONE',  ( 2.185729144939000168, -82.22094444544498515, -2.793620395780000099 ) ) ;
#20825 = CARTESIAN_POINT ( 'NONE',  ( 7.446016869863558263, -79.20295307825982434, 5.901058708005812115 ) ) ;
#20826 = ORIENTED_EDGE ( 'NONE', *, *, #29733, .T. ) ;
#20827 = CARTESIAN_POINT ( 'NONE',  ( 0.4179219924009388576, -82.75223496485374142, -1.178037307492067365 ) ) ;
#20828 = CARTESIAN_POINT ( 'NONE',  ( -11.75000000000000000, -78.20000000000000284, 1.702919296826999607E-14 ) ) ;
#20829 = ORIENTED_EDGE ( 'NONE', *, *, #36869, .F. ) ;
#20830 = CARTESIAN_POINT ( 'NONE',  ( -6.053718295315133169, -79.62010282387937821, -7.393039598043110949 ) ) ;
#20831 = CARTESIAN_POINT ( 'NONE',  ( 0.8643672385586788076, -79.07759423480628413, 1.266515284944065511 ) ) ;
#20832 = DIRECTION ( 'NONE',  ( -9.149080738879000281E-11, 1.000000000000000000, 8.583834452030000788E-10 ) ) ;
#20833 = CARTESIAN_POINT ( 'NONE',  ( -4.881323669191630188, -80.01262565301878738, 9.577793144389749713 ) ) ;
#20834 = DIRECTION ( 'NONE',  ( 1.000000000000000000, 0.000000000000000000, 0.000000000000000000 ) ) ;
#20835 = CARTESIAN_POINT ( 'NONE',  ( -1.504090147229564911, -86.39318692614398287, -3.294327671531883439 ) ) ;
#20837 = EDGE_CURVE ( 'NONE', #31027, #19156, #25246, .T. ) ;
#20836 = CARTESIAN_POINT ( 'NONE',  ( -10.85772169724999969, -76.82108137906500644, 1.763485056683000041 ) ) ;
#20838 = CARTESIAN_POINT ( 'NONE',  ( -5.917523019358107206, -77.21666666666666856, 10.26699006316250795 ) ) ;
#20839 = CARTESIAN_POINT ( 'NONE',  ( -10.71369944335148361, -78.67916666666667425, 2.879226727952040044 ) ) ;
#20840 = EDGE_CURVE ( 'NONE', #3891, #46308, #36136, .T. ) ;
#20841 = CARTESIAN_POINT ( 'NONE',  ( 11.14347266599000008, -76.08322018812400245, 1.380835503201000014 ) ) ;
#20842 = CARTESIAN_POINT ( 'NONE',  ( 0.000000000000000000, -77.40000000000736691, 0.000000000000000000 ) ) ;
#20843 = B_SPLINE_CURVE_WITH_KNOTS ( 'NONE', 3,
 ( #4658, #30117, #3278, #53959, #13496, #49533, #43726, #9079, #22355, #40369, #18241, #34545, #30407, #48165, #7696, #27066, #4945, #16562 ),
 .UNSPECIFIED., .F., .F.,
 ( 4, 2, 2, 2, 2, 2, 2, 2, 4 ),
 ( 0.000000000000000000, 0.1249999999999999445, 0.2499999999999998890, 0.3749999999999999445, 0.5000000000000000000, 0.6250000000000000000, 0.7500000000000001110, 0.8750000000000000000, 1.000000000000000000 ),
 .UNSPECIFIED. ) ;
#20844 = MECHANICAL_DESIGN_GEOMETRIC_PRESENTATION_REPRESENTATION (  '', ( #12365 ), #3850 ) ;
#20845 = CARTESIAN_POINT ( 'NONE',  ( -10.89688518808336148, -80.11107775181403667, -1.501841381199422898 ) ) ;
#20846 = CARTESIAN_POINT ( 'NONE',  ( -0.3037430299689138358, -2.982705603859970633, 3.237211740786743785 ) ) ;
#20847 = CARTESIAN_POINT ( 'NONE',  ( -0.05507133005142999388, -79.52378455456849338, 3.756105593829000000 ) ) ;
#20848 = CARTESIAN_POINT ( 'NONE',  ( -6.217680906644530658, -78.02424479843827498, 8.769644482899945359 ) ) ;
#20849 = LINE ( 'NONE', #2568, #10045 ) ;
#20850 = CARTESIAN_POINT ( 'NONE',  ( -8.096452064242996016, -59.58578169018998949, 13.15643568217000769 ) ) ;
#20851 = CARTESIAN_POINT ( 'NONE',  ( -3.512414921358999909, -83.22424735065199286, 0.4773942860886000172 ) ) ;
#20852 = CARTESIAN_POINT ( 'NONE',  ( -8.587885547135288178, -76.25922932029355650, -8.019350720283787481 ) ) ;
#20853 = CARTESIAN_POINT ( 'NONE',  ( 10.55911395186000057, -22.78461666469000235, 7.642160924865000204 ) ) ;
#20854 = CARTESIAN_POINT ( 'NONE',  ( -9.389195554442999025, -61.51043214172000262, -8.194863653299998774 ) ) ;
#20855 = CARTESIAN_POINT ( 'NONE',  ( 1.384588047529715649, -79.16581540243207371, 11.96733435986142347 ) ) ;
#20856 = CARTESIAN_POINT ( 'NONE',  ( 10.35845616728999907, -60.09778595451999905, 7.627487606627999739 ) ) ;
#20857 = B_SPLINE_CURVE_WITH_KNOTS ( 'NONE', 3,
 ( #40613, #211, #27016, #53907, #22893, #54491, #40904, #8728, #36180, #50066, #31136, #23186, #31732, #49479, #4001, #13734, #49175, #18473 ),
 .UNSPECIFIED., .F., .F.,
 ( 4, 2, 2, 2, 2, 2, 2, 2, 4 ),
 ( 0.000000000000000000, 0.06250000000000185962, 0.1250000000000037192, 0.2500000000000024980, 0.5000000000000000000, 0.7499999999999974465, 0.8124999999999968914, 0.8749999999999962252, 1.000000000000000000 ),
 .UNSPECIFIED. ) ;
#20858 = TOROIDAL_SURFACE ( 'NONE', #53867, 26.50000000000000000, 14.00000000000000000 ) ;
#20859 = CARTESIAN_POINT ( 'NONE',  ( -0.09713983013762964025, -79.11964965042942310, -1.537455523586755080 ) ) ;
#20860 = CARTESIAN_POINT ( 'NONE',  ( -3.346450045594000056, -76.91303030157000364, 12.57540552286999791 ) ) ;
#20861 = EDGE_CURVE ( 'NONE', #48338, #15598, #38824, .T. ) ;
#20862 = AXIS2_PLACEMENT_3D ( 'NONE', #42019, #24001, #55595 ) ;
#20863 = PRESENTATION_STYLE_ASSIGNMENT (( #42733 ) ) ;
#20864 = LINE ( 'NONE', #8156, #50890 ) ;
#20865 = CARTESIAN_POINT ( 'NONE',  ( 4.394064475695000027, -76.23537712840000324, -11.55491662800999997 ) ) ;
#20866 = VERTEX_POINT ( 'NONE', #37295 ) ;
#20867 = CARTESIAN_POINT ( 'NONE',  ( -2.895922040489999905, -80.14568799371318164, 10.88681414971999928 ) ) ;
#20868 = CARTESIAN_POINT ( 'NONE',  ( 0.000000000000000000, -76.00000000000000000, 0.000000000000000000 ) ) ;
#20869 = CARTESIAN_POINT ( 'NONE',  ( -1.137100204128000058, -81.28336096009799405, -0.6517852884778999600 ) ) ;
#20870 = CARTESIAN_POINT ( 'NONE',  ( 10.61187473961000016, -78.96149350880999407, -6.572462896270000243 ) ) ;
#20871 = CARTESIAN_POINT ( 'NONE',  ( 0.000000000000000000, -72.89999999999999147, 0.000000000000000000 ) ) ;
#20872 = CARTESIAN_POINT ( 'NONE',  ( -6.424145201942000227, -78.32617171442198867, 7.175205111309999495 ) ) ;
#20873 = CARTESIAN_POINT ( 'NONE',  ( 3.805616469024999837, -82.37863818301799768, -1.402376157695000014 ) ) ;
#20874 = CARTESIAN_POINT ( 'NONE',  ( -1.846742135806079599, -79.98920618438151564, 10.59049653823865178 ) ) ;
#20875 = DIRECTION ( 'NONE',  ( 0.000000000000000000, -1.000000000000000000, 9.237395726959999468E-14 ) ) ;
#20876 = ORIENTED_EDGE ( 'NONE', *, *, #50835, .F. ) ;
#20877 = CARTESIAN_POINT ( 'NONE',  ( 10.07294373702136170, -77.32156161217383783, -3.779831308317421534 ) ) ;
#20878 = CARTESIAN_POINT ( 'NONE',  ( 6.919235075806907886, -78.90838314311494628, 6.169169527640317341 ) ) ;
#20879 = CARTESIAN_POINT ( 'NONE',  ( -2.382488120207371107, -78.79697025342967720, -2.465198065420734164 ) ) ;
#20880 = ORIENTED_EDGE ( 'NONE', *, *, #2040, .T. ) ;
#20881 = CARTESIAN_POINT ( 'NONE',  ( -4.969435546850999863, -78.45829163312599519, -9.746410964130999943 ) ) ;
#20882 = CARTESIAN_POINT ( 'NONE',  ( 12.64502302235999842, -56.02870851050000311, 1.799490220168999954 ) ) ;
#20883 = CARTESIAN_POINT ( 'NONE',  ( 1.820702833782999797, -80.10534472691198005, 11.29565607131000071 ) ) ;
#20884 = ORIENTED_EDGE ( 'NONE', *, *, #12944, .F. ) ;
#20885 = ORIENTED_EDGE ( 'NONE', *, *, #43896, .T. ) ;
#20886 = ORIENTED_EDGE ( 'NONE', *, *, #22557, .F. ) ;
#20887 = CARTESIAN_POINT ( 'NONE',  ( -0.4467308992050549321, -80.50409186563182118, 1.167926343017146484 ) ) ;
#20888 = EDGE_CURVE ( 'NONE', #28211, #604, #45891, .T. ) ;
#20889 = CARTESIAN_POINT ( 'NONE',  ( 11.75000000000000000, -77.95000000000000284, 2.316376715183999699E-14 ) ) ;
#20890 = CARTESIAN_POINT ( 'NONE',  ( -8.448510849392999233, -79.58832679327100834, 4.901364000006999788 ) ) ;
#20891 = B_SPLINE_CURVE_WITH_KNOTS ( 'NONE', 3,
 ( #5105, #23104, #22522, #10121 ),
 .UNSPECIFIED., .F., .F.,
 ( 4, 4 ),
 ( 0.000000000000000000, 1.000000000000000000 ),
 .UNSPECIFIED. ) ;
#20892 = EDGE_LOOP ( 'NONE', ( #27105, #14130, #9061, #7876 ) ) ;
#20893 = CARTESIAN_POINT ( 'NONE',  ( 12.43640296263000167, -53.88252466098000326, -0.05222744260233999625 ) ) ;
#20894 = EDGE_CURVE ( 'NONE', #24677, #31891, #39545, .T. ) ;
#20895 = VERTEX_POINT ( 'NONE', #19887 ) ;
#20896 = VECTOR ( 'NONE', #34824, 999.9999999999998863 ) ;
#20897 = CARTESIAN_POINT ( 'NONE',  ( 11.81418954875000082, -78.82161355975632944, 3.289986436736999753 ) ) ;
#20898 = CARTESIAN_POINT ( 'NONE',  ( 2.148673102446170713, -79.00321104920828930, -3.720415885850087534 ) ) ;
#20899 = AXIS2_PLACEMENT_3D ( 'NONE', #24956, #42396, #50680 ) ;
#20900 = CARTESIAN_POINT ( 'NONE',  ( 9.788022091658000079, -54.27120090369999872, 7.956349397036000859 ) ) ;
#20901 = CARTESIAN_POINT ( 'NONE',  ( 9.689263856525805352, -17.02111184948868328, -8.274777959192654464 ) ) ;
#20902 = CARTESIAN_POINT ( 'NONE',  ( 1.199500263597268246, -78.20208333333333428, 0.9218200799623752495 ) ) ;
#20903 = CARTESIAN_POINT ( 'NONE',  ( -8.998590793623751694, -79.01817913613845690, 3.687657890823406337 ) ) ;
#20904 = CARTESIAN_POINT ( 'NONE',  ( -8.328265577977349565, -80.29148630941537590, 7.504971905104131480 ) ) ;
#20905 = EDGE_CURVE ( 'NONE', #4925, #4724, #46479, .T. ) ;
#20906 = CARTESIAN_POINT ( 'NONE',  ( -11.00000000000000000, -78.59999999999999432, 0.000000000000000000 ) ) ;
#20907 = CARTESIAN_POINT ( 'NONE',  ( -3.989720889280234051, -81.72552084601404943, -0.4276727937140968883 ) ) ;
#20908 = CARTESIAN_POINT ( 'NONE',  ( -7.618394338636999663, -23.22713821270000167, 10.53494418059000104 ) ) ;
#20909 = CARTESIAN_POINT ( 'NONE',  ( 11.75000000000000000, -78.54999999999999716, 0.000000000000000000 ) ) ;
#20910 = CARTESIAN_POINT ( 'NONE',  ( 4.658475568430798575, -77.83333333333332860, 8.082524092276898386 ) ) ;
#20911 = CARTESIAN_POINT ( 'NONE',  ( 10.53562597590999950, -60.00558297591999946, -7.620013358898000355 ) ) ;
#20912 = CARTESIAN_POINT ( 'NONE',  ( -11.38660623898999980, -78.97827941498000826, -4.554589311945999697 ) ) ;
#20913 = CARTESIAN_POINT ( 'NONE',  ( -11.38972971424999869, -76.52882083631500620, -4.593112662244999811 ) ) ;
#20914 = CARTESIAN_POINT ( 'NONE',  ( -7.356278612544759454, -60.10416868444603722, -8.178338515874420622 ) ) ;
#20915 = CARTESIAN_POINT ( 'NONE',  ( 3.229154007622224931, -78.40340539145115883, 11.62820000353926986 ) ) ;
#20916 = DIRECTION ( 'NONE',  ( 1.000000000000000000, 0.000000000000000000, 0.000000000000000000 ) ) ;
#20917 = STYLED_ITEM ( 'NONE', ( #22772 ), #1805 ) ;
#20918 = B_SPLINE_CURVE_WITH_KNOTS ( 'NONE', 3,
 ( #40683, #32383, #14101, #5529 ),
 .UNSPECIFIED., .F., .F.,
 ( 4, 4 ),
 ( 0.000000000000000000, 1.000000000000000000 ),
 .UNSPECIFIED. ) ;
#20919 = CARTESIAN_POINT ( 'NONE',  ( 1.248378436199009789, -80.95238111698088801, -0.8512954593689909810 ) ) ;
#20920 = CARTESIAN_POINT ( 'NONE',  ( 12.59651352883999920, -60.19056208351000237, -1.801710201210000140 ) ) ;
#20921 = FACE_OUTER_BOUND ( 'NONE', #33270, .T. ) ;
#20922 = CYLINDRICAL_SURFACE ( 'NONE', #8738, 0.5000000000000006661 ) ;
#20923 = ADVANCED_FACE ( 'NONE', ( #46188 ), #37881, .F. ) ;
#20924 = CARTESIAN_POINT ( 'NONE',  ( 1.977932612850999972, -2.640452063625000179, -2.957236955477999807 ) ) ;
#20925 = CARTESIAN_POINT ( 'NONE',  ( 6.482586803565999922, -77.67906724646599059, -10.15735398655000132 ) ) ;
#20926 = CARTESIAN_POINT ( 'NONE',  ( -9.173272937381000247, -77.24698761531298885, 2.837265496132999942 ) ) ;
#20928 = CARTESIAN_POINT ( 'NONE',  ( -0.9052918118899000444, -78.30676310382339977, -0.9596938812619000281 ) ) ;
#20927 = CARTESIAN_POINT ( 'NONE',  ( 0.03141490047175235500, -75.80000000000001137, 12.11027917007127463 ) ) ;
#20929 = CARTESIAN_POINT ( 'NONE',  ( -1.260823269212999920, -83.24552555368300943, -0.6699510868867000202 ) ) ;
#20930 = DIRECTION ( 'NONE',  ( -0.9999548435846228323, 0.000000000000000000, -0.009503199022040218977 ) ) ;
#20931 = EDGE_LOOP ( 'NONE', ( #30599, #45864, #51413 ) ) ;
#20932 = CARTESIAN_POINT ( 'NONE',  ( -0.3271848554490991434, -82.10416666666665719, -1.217465845835395299 ) ) ;
#20933 = CARTESIAN_POINT ( 'NONE',  ( -11.45393214452999864, -79.28604631854099694, -4.072167004989999839 ) ) ;
#20934 = CARTESIAN_POINT ( 'NONE',  ( -1.329807244621280971, -79.13613989625301315, 9.426744174562156076 ) ) ;
#20935 = CARTESIAN_POINT ( 'NONE',  ( -5.198192873473606035, -79.99999999999998579, -7.810577683091829648 ) ) ;
#20936 = CARTESIAN_POINT ( 'NONE',  ( -3.250000000000000000, -2.000000000000000000, 0.000000000000000000 ) ) ;
#20937 = CARTESIAN_POINT ( 'NONE',  ( -0.6280215140811999941, -0.7428930985899000472, -3.647896628088999726 ) ) ;
#20938 = CARTESIAN_POINT ( 'NONE',  ( 4.128286005151000637, -78.98296321443997670, 8.744818112003999389 ) ) ;
#20939 = CARTESIAN_POINT ( 'NONE',  ( -3.140974612311352221, -78.00416666666664867, -11.68767212001979061 ) ) ;
#20940 = CARTESIAN_POINT ( 'NONE',  ( -12.70253230845862724, -53.82944272754753001, -0.9891673677568084688 ) ) ;
#20941 = ORIENTED_EDGE ( 'NONE', *, *, #13103, .T. ) ;
#20942 = EDGE_CURVE ( 'NONE', #50158, #29213, #9864, .T. ) ;
#20943 = CARTESIAN_POINT ( 'NONE',  ( -1.499934128473817241, -81.90004407876089942, 2.109063419893342596E-06 ) ) ;
#20944 = CARTESIAN_POINT ( 'NONE',  ( -2.463227758765337505, -79.15794654540887620, -11.57512065399542855 ) ) ;
#20945 = CARTESIAN_POINT ( 'NONE',  ( 0.000000000000000000, -77.70312499986998489, 0.000000000000000000 ) ) ;
#20946 = CARTESIAN_POINT ( 'NONE',  ( -10.53003236235000095, -60.12452273675999947, -7.612971540294999784 ) ) ;
#20947 = CARTESIAN_POINT ( 'NONE',  ( 0.3704480504712000521, -79.97245295876999194, -1.624200486671999899 ) ) ;
#20948 = VECTOR ( 'NONE', #861, 1000.000000000000114 ) ;
#20949 = VERTEX_POINT ( 'NONE', #51193 ) ;
#20950 = DIRECTION ( 'NONE',  ( 0.000000000000000000, 0.000000000000000000, -1.000000000000000000 ) ) ;
#20951 = LINE ( 'NONE', #38376, #48674 ) ;
#20952 = CARTESIAN_POINT ( 'NONE',  ( 1.799502287691000069, -55.49283319101999723, -12.60413670417000098 ) ) ;
#20953 = CIRCLE ( 'NONE', #54927, 4.100000000000000533 ) ;
#20954 = CARTESIAN_POINT ( 'NONE',  ( 3.176667715697470307, -79.80173575882605519, 10.50602662186070013 ) ) ;
#20955 = ADVANCED_FACE ( 'NONE', ( #10444 ), #38171, .F. ) ;
#20956 = CARTESIAN_POINT ( 'NONE',  ( 12.70259395223311039, -54.06112126473090740, -1.314575638816234182 ) ) ;
#20957 = EDGE_LOOP ( 'NONE', ( #36796, #45150, #13322, #1909, #51379 ) ) ;
#20958 = ORIENTED_EDGE ( 'NONE', *, *, #4029, .T. ) ;
#20959 = CARTESIAN_POINT ( 'NONE',  ( -9.126129491359000312, -77.19919458148599745, 8.498837978755000577 ) ) ;
#20960 = CARTESIAN_POINT ( 'NONE',  ( -2.423311762192682739, -78.70718521568076653, -10.49559937800138698 ) ) ;
#20961 = ADVANCED_FACE ( 'NONE', ( #6005 ), #46776, .F. ) ;
#20962 = ORIENTED_EDGE ( 'NONE', *, *, #29182, .T. ) ;
#20963 = CARTESIAN_POINT ( 'NONE',  ( 9.523369619462000557, -17.18054357685999989, 8.220347091616000412 ) ) ;
#20964 = B_SPLINE_CURVE_WITH_KNOTS ( 'NONE', 3,
 ( #20668, #56397, #38667, #2101, #46981, #38090, #6509, #43392, #25377, #56112, #30080, #2951, #24809, #48131, #15948, #7663, #47564, #24519 ),
 .UNSPECIFIED., .F., .F.,
 ( 4, 2, 2, 2, 2, 2, 2, 2, 4 ),
 ( 0.000000000000000000, 0.1250000000000000555, 0.2500000000000001110, 0.3750000000000001110, 0.5000000000000001110, 0.6250000000000000000, 0.7500000000000000000, 0.8750000000000000000, 1.000000000000000000 ),
 .UNSPECIFIED. ) ;
#20965 = CARTESIAN_POINT ( 'NONE',  ( 0.000000000000000000, -2.660000000000000142, 0.000000000000000000 ) ) ;
#20966 = CARTESIAN_POINT ( 'NONE',  ( 1.217390015638971645, -53.98106975037926958, 12.70229597936534560 ) ) ;
#20967 = CARTESIAN_POINT ( 'NONE',  ( -1.316656843623999817, -78.28533949426000049, -12.73088833989999991 ) ) ;
#20968 = CARTESIAN_POINT ( 'NONE',  ( 10.47045947498260965, -79.82917641337841985, -2.813952884208940741 ) ) ;
#20969 = DIRECTION ( 'NONE',  ( -1.000000000000000000, 0.000000000000000000, 0.000000000000000000 ) ) ;
#20970 = CARTESIAN_POINT ( 'NONE',  ( -0.4871519710311427165, -86.09999999999998010, 3.917790784212549227 ) ) ;
#20971 = CARTESIAN_POINT ( 'NONE',  ( 10.05828973332000054, -79.04740687722198800, -4.964767691657000270 ) ) ;
#20972 = CARTESIAN_POINT ( 'NONE',  ( 5.215253922439524459, -79.92783438175399624, 7.639483251372545247 ) ) ;
#20973 = ADVANCED_FACE ( 'NONE', ( #27846 ), #41733, .T. ) ;
#20974 = ORIENTED_EDGE ( 'NONE', *, *, #53205, .T. ) ;
#20975 = CARTESIAN_POINT ( 'NONE',  ( 7.709154088362968338, -54.87253195859279487, -9.998702477015203982 ) ) ;
#20976 = EDGE_LOOP ( 'NONE', ( #42411, #50167, #3741, #41092 ) ) ;
#20977 = CARTESIAN_POINT ( 'NONE',  ( 9.478197642333000772, -79.91626286943099444, 6.090377947633999867 ) ) ;
#20978 = CARTESIAN_POINT ( 'NONE',  ( 7.489645613629919652, -77.30016879572562516, -5.428330277087084710 ) ) ;
#20979 = CARTESIAN_POINT ( 'NONE',  ( 0.9925657212695000453, -80.48402853000399659, -1.012359935335999994 ) ) ;
#20980 = CARTESIAN_POINT ( 'NONE',  ( -1.499999999971000086, -77.75000000002998490, -1.761798912373000190E-09 ) ) ;
#20981 = AXIS2_PLACEMENT_3D ( 'NONE', #51141, #46726, #5091 ) ;
#20982 = CARTESIAN_POINT ( 'NONE',  ( -4.647153543919563923, -78.25890117452027539, 10.20909265806945676 ) ) ;
#20983 = CARTESIAN_POINT ( 'NONE',  ( -1.232249204661999942, -77.57215499870638098, 0.4974159524616000305 ) ) ;
#20984 = DIRECTION ( 'NONE',  ( 0.000000000000000000, 1.000000000000000000, 0.000000000000000000 ) ) ;
#20985 = CARTESIAN_POINT ( 'NONE',  ( 2.813789756862229652, -80.85416666666665719, 10.47020627418440064 ) ) ;
#20986 = CARTESIAN_POINT ( 'NONE',  ( -12.50000000000000000, -61.48359816765000119, -1.003641516062000250 ) ) ;
#20987 = LINE ( 'NONE', #39569, #47976 ) ;
#20988 = CARTESIAN_POINT ( 'NONE',  ( -7.642160924865000204, -22.78461666469000235, 10.55911395186000057 ) ) ;
#20989 = CARTESIAN_POINT ( 'NONE',  ( 8.348568777154000031, -78.25112293168498923, -7.051780313135000533 ) ) ;
#20990 = CARTESIAN_POINT ( 'NONE',  ( 10.04115011118000211, -22.76486430425999785, -7.682331425175999762 ) ) ;
#20991 = VECTOR ( 'NONE', #55849, 1000.000000000000000 ) ;
#20992 = PLANE ( 'NONE',  #19654 ) ;
#20993 = CARTESIAN_POINT ( 'NONE',  ( 2.269106295766999856E-14, -92.56607767729998670, 0.000000000000000000 ) ) ;
#20994 = ORIENTED_EDGE ( 'NONE', *, *, #29485, .T. ) ;
#20995 = CARTESIAN_POINT ( 'NONE',  ( 0.6196687357644999894, -82.48466316460299197, -1.586136063883000213 ) ) ;
#20996 = CARTESIAN_POINT ( 'NONE',  ( 1.195983586496999873, -79.65738863544999049, -0.8522763136304999376 ) ) ;
#20997 = CARTESIAN_POINT ( 'NONE',  ( -3.235440615655987617, -2.008688020932666518, -0.3548227715288363449 ) ) ;
#20998 = CARTESIAN_POINT ( 'NONE',  ( 11.95248949435000085, -78.75369350129598445, 0.8087524912306001124 ) ) ;
#20999 = CARTESIAN_POINT ( 'NONE',  ( -12.72966282071492472, -18.23110224986362837, 1.931329623869561862 ) ) ;
#21000 = CARTESIAN_POINT ( 'NONE',  ( -1.140431633367790853, -79.21314104385653820, 0.5695704127092841018 ) ) ;
#21001 = CARTESIAN_POINT ( 'NONE',  ( -3.412661197378369593, -2.269647688907610927, -0.8619490756354352134 ) ) ;
#21002 = CARTESIAN_POINT ( 'NONE',  ( 5.279327442448000340, -79.30233528321798531, -7.780650776298999816 ) ) ;
#21003 = CARTESIAN_POINT ( 'NONE',  ( -6.351606481687999128, -78.07617171442198867, 7.094185741421999758 ) ) ;
#21004 = CARTESIAN_POINT ( 'NONE',  ( -0.4230197004537654126, -81.19773207085326305, -1.184957207720425343 ) ) ;
#21005 = CARTESIAN_POINT ( 'NONE',  ( 11.52686684160662267, -75.96526634729282534, 2.278194760864160173 ) ) ;
#21006 = CARTESIAN_POINT ( 'NONE',  ( -0.4619891075108225054, -82.05471047325586653, 1.187616552076537602 ) ) ;
#21007 = ORIENTED_EDGE ( 'NONE', *, *, #204, .F. ) ;
#21008 = AXIS2_PLACEMENT_3D ( 'NONE', #25355, #12077, #30058 ) ;
#21009 = DIRECTION ( 'NONE',  ( -1.000000000000000000, 0.000000000000000000, 0.000000000000000000 ) ) ;
#21010 = CARTESIAN_POINT ( 'NONE',  ( -11.75000000000000000, -77.20000000000000284, -1.435311119447000145E-14 ) ) ;
#21011 = CARTESIAN_POINT ( 'NONE',  ( -0.5999999999999999778, -23.15000000000999947, 11.79999999999999893 ) ) ;
#21012 = CARTESIAN_POINT ( 'NONE',  ( -2.347024683480479545, -78.48547955770027329, -3.892553587101836410 ) ) ;
#21013 = CARTESIAN_POINT ( 'NONE',  ( 0.5021253177900999454, -81.97897263881000640, -1.588436081161999969 ) ) ;
#21014 = CARTESIAN_POINT ( 'NONE',  ( -0.5193979750644999172, -78.99108129143698420, -10.96331347381999954 ) ) ;
#21015 = CARTESIAN_POINT ( 'NONE',  ( 10.48774103545000003, -57.04527981721000174, -7.686941364801000098 ) ) ;
#21016 = CARTESIAN_POINT ( 'NONE',  ( -10.75651041663249607, -80.44348958333230826, 1.407171709692736083 ) ) ;
#21017 = CARTESIAN_POINT ( 'NONE',  ( 4.610941639127999814, -76.73255973945900621, -11.24387672497000068 ) ) ;
#21018 = CARTESIAN_POINT ( 'NONE',  ( 0.000000000000000000, -75.10000000284179578, 7.200000000000000178 ) ) ;
#21019 = CARTESIAN_POINT ( 'NONE',  ( 1.980584515756000030, -60.06485150062000145, 12.76303204342999997 ) ) ;
#21020 = ORIENTED_EDGE ( 'NONE', *, *, #19809, .T. ) ;
#21021 = EDGE_CURVE ( 'NONE', #55921, #18184, #28724, .T. ) ;
#21022 = CARTESIAN_POINT ( 'NONE',  ( -11.01515889844999840, -78.63675832436199187, 0.6066373079611000474 ) ) ;
#21023 = CARTESIAN_POINT ( 'NONE',  ( -1.159815416435145519, -80.06983562126566767, 0.4658135504333426047 ) ) ;
#21024 = CARTESIAN_POINT ( 'NONE',  ( 9.249999999999996447, -78.23958333333334281, -1.210822168571094481 ) ) ;
#21025 = CARTESIAN_POINT ( 'NONE',  ( -10.07307375010999984, -78.71614208009899016, -5.046000355766999235 ) ) ;
#21026 = CARTESIAN_POINT ( 'NONE',  ( -10.48543666025109111, -76.84166666666665435, -6.043427764450793660 ) ) ;
#21027 = CARTESIAN_POINT ( 'NONE',  ( 5.896171905175000560, -77.86999999999999034, 7.127247495676000355 ) ) ;
#21028 = LINE ( 'NONE', #11607, #56689 ) ;
#21029 = VECTOR ( 'NONE', #58382, 1000.000000000000000 ) ;
#21030 = CARTESIAN_POINT ( 'NONE',  ( 0.9049231439593581339, -83.02548565174980411, -1.211648235339166657 ) ) ;
#21031 = PRODUCT_DEFINITION_SHAPE ( 'NONE', 'NONE',  #54603 ) ;
#21032 = CARTESIAN_POINT ( 'NONE',  ( 0.1863217586117132951, -79.73704994264652157, -1.236983196908801208 ) ) ;
#21033 = DIRECTION ( 'NONE',  ( -1.000000000000000000, 0.000000000000000000, 0.000000000000000000 ) ) ;
#21034 = CYLINDRICAL_SURFACE ( 'NONE', #23563, 12.90000000000000036 ) ;
#21035 = AXIS2_PLACEMENT_3D ( 'NONE', #2892, #2613, #3752 ) ;
#21036 = FACE_OUTER_BOUND ( 'NONE', #20139, .T. ) ;
#21037 = ORIENTED_EDGE ( 'NONE', *, *, #53131, .T. ) ;
#21038 = ORIENTED_EDGE ( 'NONE', *, *, #31373, .F. ) ;
#21039 = CARTESIAN_POINT ( 'NONE',  ( -12.77306291382000047, -53.74129324268999852, -1.041150512314999999 ) ) ;
#21040 = EDGE_CURVE ( 'NONE', #28137, #50285, #43129, .T. ) ;
#21041 = VERTEX_POINT ( 'NONE', #5423 ) ;
#21042 = VERTEX_POINT ( 'NONE', #6591 ) ;
#21043 = CARTESIAN_POINT ( 'NONE',  ( -10.75000000000000000, -81.00000000000000000, 2.851355842494999902E-13 ) ) ;
#21044 = CARTESIAN_POINT ( 'NONE',  ( 9.410240357728000049, -76.86571227068199619, 5.533781925607000218 ) ) ;
#21045 = ITEM_DEFINED_TRANSFORMATION ( 'NONE', 'NONE', #7490,  #43526 ) ;
#21046 = AXIS2_PLACEMENT_3D ( 'NONE', #18201, #45947, #54211 ) ;
#21047 = CARTESIAN_POINT ( 'NONE',  ( -5.875581754031000692, -79.18238667140099096, 7.981103691720999649 ) ) ;
#21048 = CARTESIAN_POINT ( 'NONE',  ( 2.039250879084999912, -79.83786543273089364, -11.02993955029000084 ) ) ;
#21049 = ADVANCED_FACE ( 'NONE', ( #14567 ), #30866, .F. ) ;
#21050 = ORIENTED_EDGE ( 'NONE', *, *, #42314, .T. ) ;
#21051 = VERTEX_POINT ( 'NONE', #20181 ) ;
#21052 = CARTESIAN_POINT ( 'NONE',  ( -4.872763204610360610, -77.51918167194213538, 7.863451525103128503 ) ) ;
#21053 = CARTESIAN_POINT ( 'NONE',  ( -9.808193611224998776, -77.77159370546399941, 5.067887917229000116 ) ) ;
#21054 = EDGE_CURVE ( 'NONE', #9689, #51555, #56192, .T. ) ;
#21055 = CARTESIAN_POINT ( 'NONE',  ( -12.78037829250999913, -61.09316779356999660, -1.812823010630000065 ) ) ;
#21056 = CARTESIAN_POINT ( 'NONE',  ( -3.907230163516999699, -77.92217509810099330, -8.882807090995999744 ) ) ;
#21057 = CARTESIAN_POINT ( 'NONE',  ( 4.614362421890539245, -86.09999999999978115, 0.5296543453899439369 ) ) ;
#21058 = CARTESIAN_POINT ( 'NONE',  ( 8.792818914745540226, -62.02696626405479208, 9.175540344916807811 ) ) ;
#21059 = CARTESIAN_POINT ( 'NONE',  ( 10.75000000000000000, -76.75000000000000000, 0.000000000000000000 ) ) ;
#21060 = CARTESIAN_POINT ( 'NONE',  ( -4.017143116098000455, -80.27389229980698815, 10.51352533724000082 ) ) ;
#21061 = CARTESIAN_POINT ( 'NONE',  ( -0.5415696896749999656, -80.67073041130998945, 1.614471809804999936 ) ) ;
#21062 = CARTESIAN_POINT ( 'NONE',  ( 0.000000000000000000, -78.69999999999998863, 0.000000000000000000 ) ) ;
#21063 = EDGE_LOOP ( 'NONE', ( #48000, #24281, #34613, #23870 ) ) ;
#21064 = CARTESIAN_POINT ( 'NONE',  ( -10.15836276337999955, -76.54404187781499047, 3.905545731297999978 ) ) ;
#21065 = CARTESIAN_POINT ( 'NONE',  ( 9.418360348373997937, -78.27913667140100529, 2.704229673158000224 ) ) ;
#21066 = FACE_OUTER_BOUND ( 'NONE', #55832, .T. ) ;
#21067 = CARTESIAN_POINT ( 'NONE',  ( -10.18949731070999931, -18.78470987703000006, -7.645392562261999814 ) ) ;
#21069 = CARTESIAN_POINT ( 'NONE',  ( -0.005523896503903000417, -16.93036543774000080, -12.55021156880999911 ) ) ;
#21068 = CARTESIAN_POINT ( 'NONE',  ( 7.678667886039000301, -58.55736537918999574, 10.59548767697000038 ) ) ;
#21070 = EDGE_CURVE ( 'NONE', #49814, #55458, #41445, .T. ) ;
#21071 = CARTESIAN_POINT ( 'NONE',  ( -9.369164850722000892, -60.04999999966999980, 7.601397897754999633 ) ) ;
#21072 = CARTESIAN_POINT ( 'NONE',  ( -8.182545292233999845, -80.43338938826599360, 7.620877899251000009 ) ) ;
#21073 = CARTESIAN_POINT ( 'NONE',  ( -9.563148796606999014, -77.27913032869298604, 5.948121522994000543 ) ) ;
#21074 = CARTESIAN_POINT ( 'NONE',  ( -12.50745077485999879, -53.80005551680000053, 2.011910316382000212E-09 ) ) ;
#21075 = CARTESIAN_POINT ( 'NONE',  ( 5.448459039171999585, -81.05765812071879850, -9.476848501824999715 ) ) ;
#21076 = ORIENTED_EDGE ( 'NONE', *, *, #36998, .T. ) ;
#21077 = CARTESIAN_POINT ( 'NONE',  ( -1.456717367586000012E-14, -79.29999999999999716, 0.000000000000000000 ) ) ;
#21078 = VECTOR ( 'NONE', #20347, 1000.000000000000114 ) ;
#21079 = CARTESIAN_POINT ( 'NONE',  ( -1.500000000000000000, -77.50000000000000000, 0.000000000000000000 ) ) ;
#21080 = CARTESIAN_POINT ( 'NONE',  ( 7.686918321221999584, -20.24439829127999957, -10.48771805383000100 ) ) ;
#21081 = CARTESIAN_POINT ( 'NONE',  ( 2.732748911140999937, -3.323893098590000150, -2.413281231417000239 ) ) ;
#21082 = CARTESIAN_POINT ( 'NONE',  ( -11.14038684213999986, -78.18901912946698474, 1.307628137226999998 ) ) ;
#21083 = CARTESIAN_POINT ( 'NONE',  ( -12.66322081666000088, -53.61838367289999496, 0.1487102037790999920 ) ) ;
#21084 = CARTESIAN_POINT ( 'NONE',  ( -0.7554284705563480973, -80.08333333333332860, -1.310679582531387277 ) ) ;
#21085 = CARTESIAN_POINT ( 'NONE',  ( -1.636761686205420396, -3.083333333333333925, -2.839805762151339508 ) ) ;
#21086 = B_SPLINE_CURVE_WITH_KNOTS ( 'NONE', 3,
 ( #44881, #43725, #21269, #13572, #4136, #53738 ),
 .UNSPECIFIED., .F., .F.,
 ( 4, 2, 4 ),
 ( 0.000000000000000000, 0.5000000000000000000, 1.000000000000000000 ),
 .UNSPECIFIED. ) ;
#21087 = AXIS2_PLACEMENT_3D ( 'NONE', #17133, #18242, #36522 ) ;
#21088 = DIRECTION ( 'NONE',  ( 1.000000000000000000, 0.000000000000000000, 0.000000000000000000 ) ) ;
#21089 = EDGE_CURVE ( 'NONE', #8528, #47767, #19011, .T. ) ;
#21090 = AXIS2_PLACEMENT_3D ( 'NONE', #43967, #48404, #40103 ) ;
#21091 = DIRECTION ( 'NONE',  ( 0.000000000000000000, 1.000000000000000000, 0.000000000000000000 ) ) ;
#21092 = CARTESIAN_POINT ( 'NONE',  ( 1.918267526783000054, -77.23179811450799548, 10.77842959370000031 ) ) ;
#21093 = CARTESIAN_POINT ( 'NONE',  ( 9.768846781487011910, -76.40261481437684665, -6.528746261247764693 ) ) ;
#21094 = CARTESIAN_POINT ( 'NONE',  ( -8.595972950985999006, -77.76378400355899601, -7.096749227412000316 ) ) ;
#21095 = CARTESIAN_POINT ( 'NONE',  ( 1.250000000000000000, -81.84999999999999432, 0.000000000000000000 ) ) ;
#21096 = LINE ( 'NONE', #3101, #40617 ) ;
#21097 = CARTESIAN_POINT ( 'NONE',  ( 7.764258067048000811, -77.01038689586449948, 5.767450660628000492 ) ) ;
#21098 = CARTESIAN_POINT ( 'NONE',  ( 7.396918292183172206, -78.30208333333331439, 5.684557159767955170 ) ) ;
#21099 = CARTESIAN_POINT ( 'NONE',  ( 1.496667148433702188, -3.438256644742763601, 2.927442453955206414 ) ) ;
#21100 = CARTESIAN_POINT ( 'NONE',  ( -3.746558969565879416, -80.19711350692230667, -10.07601878856429423 ) ) ;
#21101 = DIRECTION ( 'NONE',  ( 0.000000000000000000, -1.000000000000000000, 0.000000000000000000 ) ) ;
#21102 = CARTESIAN_POINT ( 'NONE',  ( -10.36746145411166431, -18.23400545010064633, -7.635225828759649502 ) ) ;
#21103 = CARTESIAN_POINT ( 'NONE',  ( 8.348735229153000148, -78.81043090964000442, 8.268078378528999295 ) ) ;
#21104 = CARTESIAN_POINT ( 'NONE',  ( 0.7681833999686413783, -81.82291666666667140, 0.9995835529977274980 ) ) ;
#21105 = CARTESIAN_POINT ( 'NONE',  ( -2.860041384466000203, -78.92797663195699442, -10.89284755413000028 ) ) ;
#21106 = CARTESIAN_POINT ( 'NONE',  ( -13.86363636363000218, -46.43897132165000130, -1.277887489420000009E-05 ) ) ;
#21107 = VERTEX_POINT ( 'NONE', #52912 ) ;
#21108 = DIRECTION ( 'NONE',  ( 0.5721800015181066623, -0.8201280667449074580, 0.000000000000000000 ) ) ;
#21109 = ORIENTED_EDGE ( 'NONE', *, *, #6751, .T. ) ;
#21110 = ORIENTED_EDGE ( 'NONE', *, *, #56057, .T. ) ;
#21111 = FACE_OUTER_BOUND ( 'NONE', #46044, .T. ) ;
#21112 = ORIENTED_EDGE ( 'NONE', *, *, #19590, .T. ) ;
#21113 = CIRCLE ( 'NONE', #13561, 10.69999999999999929 ) ;
#21114 = CARTESIAN_POINT ( 'NONE',  ( 1.665357644511999968, -79.76473784880299434, 3.129146085054999471 ) ) ;
#21115 = CARTESIAN_POINT ( 'NONE',  ( -3.652956595797749895, -79.30607455077640111, 8.769390947670537173 ) ) ;
#21116 = ORIENTED_EDGE ( 'NONE', *, *, #12574, .F. ) ;
#21117 = CARTESIAN_POINT ( 'NONE',  ( 0.1997943094379295570, -82.73830915514584206, -1.234411186249315673 ) ) ;
#21118 = ORIENTED_EDGE ( 'NONE', *, *, #47517, .F. ) ;
#21119 = CARTESIAN_POINT ( 'NONE',  ( 7.396918292183175758, -79.69791666666667140, -5.684557159767951617 ) ) ;
#21120 = ORIENTED_EDGE ( 'NONE', *, *, #460, .F. ) ;
#21121 = FACE_OUTER_BOUND ( 'NONE', #45595, .T. ) ;
#21122 = CARTESIAN_POINT ( 'NONE',  ( -10.98521938008736853, -18.65929923595803785, 0.5702549022851668425 ) ) ;
#21123 = CARTESIAN_POINT ( 'NONE',  ( -10.21779526337023114, -80.07488518645870101, 3.340465863513364830 ) ) ;
#21124 = CARTESIAN_POINT ( 'NONE',  ( -8.190859204290999784, -59.94999999967000548, 7.342331066867000544 ) ) ;
#21125 = CARTESIAN_POINT ( 'NONE',  ( 0.4401343155876301094, -86.39318692614396866, -4.182001622060982804 ) ) ;
#21126 = CARTESIAN_POINT ( 'NONE',  ( 2.076475668830000121, -76.19403282933799915, 10.98918251355999942 ) ) ;
#21127 = FACE_OUTER_BOUND ( 'NONE', #8924, .T. ) ;
#21128 = CARTESIAN_POINT ( 'NONE',  ( -3.592030622028691056, -77.25518602892395847, 8.980398724672147281 ) ) ;
#21129 = CARTESIAN_POINT ( 'NONE',  ( 7.863749243303001180, -76.77047704070999146, 7.690468382148999638 ) ) ;
#21130 = CARTESIAN_POINT ( 'NONE',  ( -8.447183166110368902, -78.63346764869346828, -3.773792821381649620 ) ) ;
#21131 = CARTESIAN_POINT ( 'NONE',  ( 0.000000000000000000, -75.15999999999999659, 0.000000000000000000 ) ) ;
#21132 = CARTESIAN_POINT ( 'NONE',  ( 2.252478813166476801, -2.914525471928731459, 2.342577926442860559 ) ) ;
#21133 = CARTESIAN_POINT ( 'NONE',  ( 3.301590336738000175, -82.16542549782599281, -1.408153524787000066 ) ) ;
#21134 = CARTESIAN_POINT ( 'NONE',  ( -7.477182751274228600, -78.03619407845222611, 7.725621107446211333 ) ) ;
#21135 = EDGE_CURVE ( 'NONE', #37236, #23864, #57052, .T. ) ;
#21136 = DIRECTION ( 'NONE',  ( 0.000000000000000000, 0.000000000000000000, -1.000000000000000000 ) ) ;
#21137 = CARTESIAN_POINT ( 'NONE',  ( -0.8560878949168587715, -80.98146821848625621, 10.71577390680143971 ) ) ;
#21138 = CARTESIAN_POINT ( 'NONE',  ( 3.437452679404000122, -83.99694503318799832, 0.8749179571431999758 ) ) ;
#21139 = CARTESIAN_POINT ( 'NONE',  ( -1.209804193477999945, -2.381925387468999400, -3.608664049297999998 ) ) ;
#21140 = CARTESIAN_POINT ( 'NONE',  ( -1.247385801055000076, -17.52277743740000204, 12.50301438876999960 ) ) ;
#21141 = CARTESIAN_POINT ( 'NONE',  ( -8.533826143255001995, -61.80526450216999734, -9.213084459936000670 ) ) ;
#21142 = EDGE_CURVE ( 'NONE', #37515, #48410, #2626, .T. ) ;
#21143 = CARTESIAN_POINT ( 'NONE',  ( 4.784380313523522332, -78.23333333333333428, 8.300970689365462007 ) ) ;
#21144 = CARTESIAN_POINT ( 'NONE',  ( -0.5935892672256000147, -82.08982011648200228, 1.194249225580000129 ) ) ;
#21145 = CARTESIAN_POINT ( 'NONE',  ( -12.66313295597999833, -16.82196533882000011, 0.06049275240485999655 ) ) ;
#21146 = CARTESIAN_POINT ( 'NONE',  ( 11.79660191402999914, -76.83668768631000034, 5.494707494196000575 ) ) ;
#21147 = AXIS2_PLACEMENT_3D ( 'NONE', #57091, #24931, #24644 ) ;
#21148 = CARTESIAN_POINT ( 'NONE',  ( -10.96673197750000206, -78.31274657044698984, -0.4413686857046000278 ) ) ;
#21149 = CARTESIAN_POINT ( 'NONE',  ( -12.50745077494999968, -61.79994448255000350, -2.661703094427999907E-09 ) ) ;
#21150 = CARTESIAN_POINT ( 'NONE',  ( 8.559075968402000356, -75.76731679589001089, -8.919964875508998858 ) ) ;
#21151 = VERTEX_POINT ( 'NONE', #44056 ) ;
#21152 = ADVANCED_FACE ( 'NONE', ( #21036 ), #3532, .F. ) ;
#21153 = CARTESIAN_POINT ( 'NONE',  ( 4.537811113640745297, -80.09166625100542092, 10.16818905941867968 ) ) ;
#21154 = CARTESIAN_POINT ( 'NONE',  ( 5.865376297750441863E-14, -72.84999999994899156, 13.94999999994999840 ) ) ;
#21155 = CARTESIAN_POINT ( 'NONE',  ( 12.83677138650999972, -60.02737696024999536, 2.062839765282999949 ) ) ;
#21156 = CARTESIAN_POINT ( 'NONE',  ( -1.806885568419999810, -79.19518329857000083, -12.66522665019000016 ) ) ;
#21157 = CARTESIAN_POINT ( 'NONE',  ( 9.596002108778174389, -79.09791666666666288, -7.374560639698961140 ) ) ;
#21158 = CARTESIAN_POINT ( 'NONE',  ( 6.852546780225999612, -78.64586191736599119, -6.611579150008999761 ) ) ;
#21159 = CARTESIAN_POINT ( 'NONE',  ( 3.472269588435000109, -82.33855471126298653, -1.985374575346000370 ) ) ;
#21160 = CARTESIAN_POINT ( 'NONE',  ( 4.030751681420186472, -79.94461808928627988, 9.966766518696916322 ) ) ;
#21161 = CARTESIAN_POINT ( 'NONE',  ( 0.3985939703966000502, -79.13679175127299459, -1.564707112294000169 ) ) ;
#21162 = ORIENTED_EDGE ( 'NONE', *, *, #45263, .F. ) ;
#21163 = DIRECTION ( 'NONE',  ( 0.000000000000000000, -1.000000000000000000, 0.000000000000000000 ) ) ;
#21164 = CARTESIAN_POINT ( 'NONE',  ( 10.99999999999999822, -78.93958333333334565, -1.439896632895356188 ) ) ;
#21165 = CARTESIAN_POINT ( 'NONE',  ( -3.926077803139174982, -78.72584796626247794, -0.8615687731491100676 ) ) ;
#21166 = EDGE_CURVE ( 'NONE', #29378, #40036, #43174, .T. ) ;
#21167 = ORIENTED_EDGE ( 'NONE', *, *, #38310, .F. ) ;
#21168 = CARTESIAN_POINT ( 'NONE',  ( 7.763360352781000451, -78.68303046778699184, 7.708310604078000061 ) ) ;
#21169 = EDGE_CURVE ( 'NONE', #22103, #51194, #48800, .T. ) ;
#21170 = CARTESIAN_POINT ( 'NONE',  ( -7.555116226631051646, -55.11315380193744318, -7.995796640820927337 ) ) ;
#21171 = CARTESIAN_POINT ( 'NONE',  ( -7.101555135103000183, -80.37802629438799329, -8.827926690876999771 ) ) ;
#21172 = ORIENTED_EDGE ( 'NONE', *, *, #7016, .T. ) ;
#21173 = CARTESIAN_POINT ( 'NONE',  ( -4.771559678803999560, -78.78373690646100158, -11.06471824780000013 ) ) ;
#21174 = ORIENTED_EDGE ( 'NONE', *, *, #43404, .T. ) ;
#21175 = ORIENTED_EDGE ( 'NONE', *, *, #17963, .F. ) ;
#21176 = CARTESIAN_POINT ( 'NONE',  ( 0.7505680871121789277, -80.42410011460410146, 1.001643424464033760 ) ) ;
#21177 = DIRECTION ( 'NONE',  ( 0.000000000000000000, -1.000000000000000000, 0.000000000000000000 ) ) ;
#21178 = CARTESIAN_POINT ( 'NONE',  ( -7.479908383216000267, -79.68574476804501217, -6.281056869080000382 ) ) ;
#21179 = CIRCLE ( 'NONE', #54198, 5.000000000000000000 ) ;
#21180 = ORIENTED_EDGE ( 'NONE', *, *, #43097, .F. ) ;
#21181 = CARTESIAN_POINT ( 'NONE',  ( 12.66314509266000066, -53.62135249290999894, -0.04032083120558000583 ) ) ;
#21182 = EDGE_LOOP ( 'NONE', ( #3400, #38315, #527, #938, #50027, #41643 ) ) ;
#21183 = CARTESIAN_POINT ( 'NONE',  ( -9.393849266501053563, -80.64169200378464097, -5.414091273218729405 ) ) ;
#21184 = VECTOR ( 'NONE', #49667, 1000.000000000000000 ) ;
#21185 = CARTESIAN_POINT ( 'NONE',  ( 3.485499217011998940, -78.91452042059378869, -2.057048905967550745 ) ) ;
#21186 = CARTESIAN_POINT ( 'NONE',  ( 10.52693198617000014, -55.37847693893999690, 7.606025555747000233 ) ) ;
#21187 = DIRECTION ( 'NONE',  ( 0.000000000000000000, 1.000000000000000000, 0.000000000000000000 ) ) ;
#21188 = CARTESIAN_POINT ( 'NONE',  ( 1.460959015002472494, -78.17083333333334849, 0.3926218265389232465 ) ) ;
#21189 = FACE_OUTER_BOUND ( 'NONE', #51989, .T. ) ;
#21190 = CIRCLE ( 'NONE', #37211, 0.5999999999999999778 ) ;
#21191 = CARTESIAN_POINT ( 'NONE',  ( 0.000000000000000000, -76.75499999999999545, 0.000000000000000000 ) ) ;
#21192 = CARTESIAN_POINT ( 'NONE',  ( 0.6217590130341388299, -78.00838734090868343, -1.375229810813027198 ) ) ;
#21193 = CARTESIAN_POINT ( 'NONE',  ( 8.823651773949475086, -78.82575552834812527, -2.782417521243436109 ) ) ;
#21194 = CARTESIAN_POINT ( 'NONE',  ( -7.633089125616000281, -23.39007426303999893, 10.18115018432999896 ) ) ;
#21195 = FACE_OUTER_BOUND ( 'NONE', #57199, .T. ) ;
#21196 = CARTESIAN_POINT ( 'NONE',  ( 5.838193839761703252, -78.07708333333333428, -7.596835002782702517 ) ) ;
#21197 = CARTESIAN_POINT ( 'NONE',  ( -12.77649734584999841, -16.69171487512999974, -0.06478328530401999963 ) ) ;
#21198 = CARTESIAN_POINT ( 'NONE',  ( 1.439896632895286466, -77.96458333333332291, 11.00000000000000711 ) ) ;
#21199 = CARTESIAN_POINT ( 'NONE',  ( 2.548493721447000038, -76.85668274275499812, 12.01365081398999912 ) ) ;
#21200 = CARTESIAN_POINT ( 'NONE',  ( 4.784380313523522332, -78.73333333333332007, 8.300970689365462007 ) ) ;
#21201 = DIRECTION ( 'NONE',  ( 1.000000000000000000, 0.000000000000000000, 0.000000000000000000 ) ) ;
#21202 = CARTESIAN_POINT ( 'NONE',  ( -1.497746365902677956, -80.73982606612976554, 0.1936102584281759742 ) ) ;
#21203 = CARTESIAN_POINT ( 'NONE',  ( -2.794222306786000143, -77.12148308212269399, -8.839119250891998902 ) ) ;
#21204 = CARTESIAN_POINT ( 'NONE',  ( 1.603441158369999897, -79.16745489434200067, 0.1902368389766999901 ) ) ;
#21205 = CARTESIAN_POINT ( 'NONE',  ( -12.50000000000000000, -60.04999999725999515, 1.750000000000000000 ) ) ;
#21206 = CARTESIAN_POINT ( 'NONE',  ( -3.020029971748000364, -3.012862276481999668, -1.880661267551000160 ) ) ;
#21207 = CARTESIAN_POINT ( 'NONE',  ( 11.88669912479000068, -78.20818512137599043, 2.586293583890999948 ) ) ;
#21208 = CARTESIAN_POINT ( 'NONE',  ( 1.500000000000000000, -80.75000000000000000, 0.000000000000000000 ) ) ;
#21210 = CARTESIAN_POINT ( 'NONE',  ( -7.836763323857902641, -17.69488832272180900, 9.850488778970195369 ) ) ;
#21209 = DIRECTION ( 'NONE',  ( 0.6562721000481037681, -0.7545243075597046767, 7.874481590556048732E-10 ) ) ;
#21211 = CARTESIAN_POINT ( 'NONE',  ( 0.6000739755967000599, -82.55077418747099216, 1.467756090344000119 ) ) ;
#21212 = CARTESIAN_POINT ( 'NONE',  ( -8.033734583472570634, -79.54227913950597895, 7.144481850731994932 ) ) ;
#21213 = EDGE_LOOP ( 'NONE', ( #57245, #37021, #28993, #20165 ) ) ;
#21214 = EDGE_CURVE ( 'NONE', #25466, #2738, #55780, .T. ) ;
#21215 = DIRECTION ( 'NONE',  ( 1.000000000000000000, 0.000000000000000000, 0.000000000000000000 ) ) ;
#21216 = CARTESIAN_POINT ( 'NONE',  ( 11.77121427762000039, -79.45802193175599371, 2.535895762643999962 ) ) ;
#21217 = CIRCLE ( 'NONE', #37232, 0.5000000000000001110 ) ;
#21218 = CARTESIAN_POINT ( 'NONE',  ( -9.509637957782862472, -79.24022236790916907, 1.167149435952707259 ) ) ;
#21219 = B_SPLINE_CURVE_WITH_KNOTS ( 'NONE', 3,
 ( #52530, #7081, #25082, #12087, #48401, #34211, #51685, #33645, #38657, #24798, #25651, #20940, #39231, #20089, #15648, #16232 ),
 .UNSPECIFIED., .F., .F.,
 ( 4, 2, 2, 2, 2, 2, 2, 4 ),
 ( 0.000000000000000000, 0.2499999999999956701, 0.3749999999999965028, 0.4374999999999968914, 0.4999999999999973355, 0.6249999999999980016, 0.7499999999999987788, 1.000000000000000000 ),
 .UNSPECIFIED. ) ;
#21220 = B_SPLINE_CURVE_WITH_KNOTS ( 'NONE', 3,
 ( #10700, #1847, #24263, #46429, #9522, #5664, #1266, #50268, #41687, #28676, #36670, #5959, #54686, #15103, #41980, #27509 ),
 .UNSPECIFIED., .F., .F.,
 ( 4, 2, 2, 2, 2, 2, 2, 4 ),
 ( 0.000000000000000000, 0.2500000000000092704, 0.3750000000000126565, 0.5000000000000160982, 0.6250000000000195399, 0.6875000000000184297, 0.7500000000000172085, 1.000000000000000000 ),
 .UNSPECIFIED. ) ;
#21221 = CARTESIAN_POINT ( 'NONE',  ( -6.977995179411893290, -79.99999999999998579, -6.220662632887979271 ) ) ;
#21222 = CARTESIAN_POINT ( 'NONE',  ( -7.605690822197999523, -60.22565082124000213, 10.52682217037000001 ) ) ;
#21223 = CARTESIAN_POINT ( 'NONE',  ( -3.110062099568999816, -0.6770460165488999538, -2.005045321468000186 ) ) ;
#21224 = CARTESIAN_POINT ( 'NONE',  ( 1.497466954355000102, -79.56970617083499064, 9.665433974424999519 ) ) ;
#21225 = FACE_OUTER_BOUND ( 'NONE', #57477, .T. ) ;
#21226 = CARTESIAN_POINT ( 'NONE',  ( -4.658475568430814562, -79.08333333333332860, -8.082524092276884176 ) ) ;
#21227 = VERTEX_POINT ( 'NONE', #47351 ) ;
#21228 = CARTESIAN_POINT ( 'NONE',  ( -12.70249541834471074, -53.83496187168930902, 0.9988462571234606457 ) ) ;
#21229 = AXIS2_PLACEMENT_3D ( 'NONE', #49548, #48664, #26211 ) ;
#21230 = CARTESIAN_POINT ( 'NONE',  ( -3.587712099295000012, -1.710945589986999860, 1.801380527025000067 ) ) ;
#21231 = CARTESIAN_POINT ( 'NONE',  ( 8.185149126674000186, -79.55108667140099499, 5.079755422656999642 ) ) ;
#21232 = LINE ( 'NONE', #16814, #53524 ) ;
#21233 = CARTESIAN_POINT ( 'NONE',  ( 3.407095545933000569, -78.62148120184447464, 0.000000000000000000 ) ) ;
#21234 = VECTOR ( 'NONE', #48863, 1000.000000000000114 ) ;
#21235 = CARTESIAN_POINT ( 'NONE',  ( 0.2617232932829000047, -79.46717923788999371, -1.644907507304999905 ) ) ;
#21236 = EDGE_CURVE ( 'NONE', #19368, #7896, #23352, .T. ) ;
#21237 = ORIENTED_EDGE ( 'NONE', *, *, #1578, .T. ) ;
#21238 = CARTESIAN_POINT ( 'NONE',  ( -4.670305506034999610, -77.01883941971439640, -9.783521845360001024 ) ) ;
#21239 = CARTESIAN_POINT ( 'NONE',  ( -8.561416052707739865, -77.00000000000000000, 3.586226970955711302 ) ) ;
#21240 = DIRECTION ( 'NONE',  ( -1.000000000000000000, 0.000000000000000000, 0.000000000000000000 ) ) ;
#21241 = CARTESIAN_POINT ( 'NONE',  ( -10.75040831495720361, -78.58963204257108259, 1.407120353455911133 ) ) ;
#21242 = CARTESIAN_POINT ( 'NONE',  ( -9.358268528169000788, -79.23265764587299032, -2.797054701638000296 ) ) ;
#21243 = ORIENTED_EDGE ( 'NONE', *, *, #6554, .T. ) ;
#21244 = VERTEX_POINT ( 'NONE', #20751 ) ;
#21245 = CARTESIAN_POINT ( 'NONE',  ( -7.768219623894999870, -76.83034993674100122, -9.755575312415000866 ) ) ;
#21246 = CARTESIAN_POINT ( 'NONE',  ( 4.370112803705837656, -78.75831584482018854, -9.822244704776046831 ) ) ;
#21247 = CARTESIAN_POINT ( 'NONE',  ( 0.2826255412215000207, -78.50241276046999417, 1.393030722100999874 ) ) ;
#21248 = VERTEX_POINT ( 'NONE', #43480 ) ;
#21249 = ADVANCED_FACE ( 'NONE', ( #25461 ), #57771, .F. ) ;
#21250 = CARTESIAN_POINT ( 'NONE',  ( -9.454379850511999805, -77.68278084965399444, 0.8787206290761000460 ) ) ;
#21251 = CARTESIAN_POINT ( 'NONE',  ( 0.000000000000000000, -75.67500000000001137, 0.000000000000000000 ) ) ;
#21252 = CARTESIAN_POINT ( 'NONE',  ( -12.50000000000000000, -51.86282895648000135, 0.000000000000000000 ) ) ;
#21253 = CARTESIAN_POINT ( 'NONE',  ( -3.040431873813000063, -78.64994354880001026, 12.26916943822000050 ) ) ;
#21254 = CARTESIAN_POINT ( 'NONE',  ( 6.329984427696999205, -78.07728428553903655, 9.260097609460000712 ) ) ;
#21255 = DIRECTION ( 'NONE',  ( 0.000000000000000000, 1.000000000000000000, 0.000000000000000000 ) ) ;
#21256 = DIRECTION ( 'NONE',  ( 0.8090169943750002979, 0.000000000000000000, -0.5877852522924001955 ) ) ;
#21257 = CARTESIAN_POINT ( 'NONE',  ( -2.710423231297999891, -79.79610400554300043, 10.88447134676999895 ) ) ;
#21258 = VECTOR ( 'NONE', #24353, 1000.000000000000000 ) ;
#21259 = CARTESIAN_POINT ( 'NONE',  ( -1.037716418681747577, -79.98405221576109625, 9.192368781140272560 ) ) ;
#21260 = ORIENTED_EDGE ( 'NONE', *, *, #13124, .F. ) ;
#21261 = CARTESIAN_POINT ( 'NONE',  ( -1.196791375131569746, -82.25000000000000000, -0.4167097060225089522 ) ) ;
#21262 = ORIENTED_EDGE ( 'NONE', *, *, #2042, .T. ) ;
#21263 = CARTESIAN_POINT ( 'NONE',  ( 9.101894997447999458, -78.82066105045699089, -6.639611571546000235 ) ) ;
#21264 = CARTESIAN_POINT ( 'NONE',  ( 4.311764069688931222, -77.26360251928231548, -8.183661215609575379 ) ) ;
#21265 = CARTESIAN_POINT ( 'NONE',  ( -0.8374915928969000056, -80.80902028819700433, -0.9453856285906999668 ) ) ;
#21266 = DIRECTION ( 'NONE',  ( 0.000000000000000000, -1.000000000000000000, 0.000000000000000000 ) ) ;
#21267 = CARTESIAN_POINT ( 'NONE',  ( -11.14658556052672367, -76.84470657150592388, 0.7341312425827495325 ) ) ;
#21268 = CARTESIAN_POINT ( 'NONE',  ( -1.391953914337000109, -78.11789385589818835, -0.2693022098514999962 ) ) ;
#21269 = CARTESIAN_POINT ( 'NONE',  ( 12.50657384757278479, -53.82752583170963590, -0.3552644803360501813 ) ) ;
#21270 = DIRECTION ( 'NONE',  ( 0.7071067811865474617, 0.000000000000000000, -0.7071067811865474617 ) ) ;
#21271 = CARTESIAN_POINT ( 'NONE',  ( -12.71798280854999952, -18.70221404512000163, -1.931086388455000025 ) ) ;
#21272 = CARTESIAN_POINT ( 'NONE',  ( -1.160437014136601830, -79.13041490960291924, -0.4645391383290830012 ) ) ;
#21273 = CARTESIAN_POINT ( 'NONE',  ( -10.99582742793000101, -79.54337123098800078, 1.892981466416000069 ) ) ;
#21274 = CARTESIAN_POINT ( 'NONE',  ( -7.000686966495000441, -76.94891167140099242, 6.253505135046999897 ) ) ;
#21275 = CARTESIAN_POINT ( 'NONE',  ( 10.24996238026999862, -21.75171076523999858, -7.705119999407000542 ) ) ;
#21276 = CARTESIAN_POINT ( 'NONE',  ( -5.092641036025000290, -79.55978622973557890, 10.89826376711000044 ) ) ;
#21277 = CYLINDRICAL_SURFACE ( 'NONE', #28524, 9.250000000000000000 ) ;
#21278 = CARTESIAN_POINT ( 'NONE',  ( -8.596418555780466875, -77.94791666666667140, 6.606377239730298001 ) ) ;
#21279 = EDGE_LOOP ( 'NONE', ( #44264, #36364, #10824, #54336, #32000 ) ) ;
#21280 = CARTESIAN_POINT ( 'NONE',  ( -7.330094131514235833, -77.20000000000001705, 8.056329451334999447 ) ) ;
#21281 = CARTESIAN_POINT ( 'NONE',  ( 1.291435174072999903, -79.59407194668000329, -0.9202965842325999679 ) ) ;
#21282 = DIRECTION ( 'NONE',  ( 0.000000000000000000, -0.9701425001453282126, -0.2425356250363475685 ) ) ;
#21283 = CARTESIAN_POINT ( 'NONE',  ( 3.249499231398999655, -78.64517623960099968, -11.53069031867000049 ) ) ;
#21284 = CARTESIAN_POINT ( 'NONE',  ( -12.70610308059024440, -17.54479009146447765, 1.580620443413589982 ) ) ;
#21285 = CARTESIAN_POINT ( 'NONE',  ( -1.271334513670838939, -79.24494429262146866, 0.08715925150112330266 ) ) ;
#21286 = CARTESIAN_POINT ( 'NONE',  ( -10.44638973513362856, -76.35792952211139095, 6.036140669651893553 ) ) ;
#21287 = CARTESIAN_POINT ( 'NONE',  ( -7.401612602209000968, -79.12609805011500441, -6.305503003149000030 ) ) ;
#21288 = CARTESIAN_POINT ( 'NONE',  ( -7.476203163627999970, -77.13115727064058547, -5.719923538308999689 ) ) ;
#21289 = CARTESIAN_POINT ( 'NONE',  ( -1.667269374601999976, -55.59060116482999803, -12.49858097728999873 ) ) ;
#21290 = CYLINDRICAL_SURFACE ( 'NONE', #36581, 1.750000000000001332 ) ;
#21291 = CARTESIAN_POINT ( 'NONE',  ( 11.32560461271045149, -75.97108467502835083, 3.151449499211164351 ) ) ;
#21292 = CARTESIAN_POINT ( 'NONE',  ( -1.273526288746646973, -81.14832600764039228, 0.03013355673499748880 ) ) ;
#21293 = ORIENTED_EDGE ( 'NONE', *, *, #4233, .F. ) ;
#21294 = CARTESIAN_POINT ( 'NONE',  ( -8.971989909486167036, -78.64261696927431444, 7.658931699842775664 ) ) ;
#21295 = EDGE_CURVE ( 'NONE', #12596, #51331, #49752, .T. ) ;
#21296 = PLANE ( 'NONE',  #2189 ) ;
#21297 = CARTESIAN_POINT ( 'NONE',  ( 5.985848557435999417, -79.99298052329480413, -10.45156471383000074 ) ) ;
#21298 = DIRECTION ( 'NONE',  ( 1.000000000000000000, 0.000000000000000000, 0.000000000000000000 ) ) ;
#21299 = ADVANCED_FACE ( 'NONE', ( #40782, #17468 ), #17177, .T. ) ;
#21300 = CARTESIAN_POINT ( 'NONE',  ( 10.55657102546000026, -78.59778833077898241, -3.003801718854000047 ) ) ;
#21301 = CARTESIAN_POINT ( 'NONE',  ( 3.599999993293999889, -0.2000000067061999953, 5.600095136020000205E-09 ) ) ;
#21302 = CARTESIAN_POINT ( 'NONE',  ( 12.18980338489999937, -76.24977255369199725, -1.398660325409999849 ) ) ;
#21303 = CARTESIAN_POINT ( 'NONE',  ( 3.417874729156432867, -78.54962478900189637, 11.24133698585978891 ) ) ;
#21304 = LINE ( 'NONE', #15723, #10771 ) ;
#21305 = ORIENTED_EDGE ( 'NONE', *, *, #56889, .T. ) ;
#21306 = CARTESIAN_POINT ( 'NONE',  ( 11.08725735368000009, -79.46710299282599976, 1.152095891907999992 ) ) ;
#21307 = CARTESIAN_POINT ( 'NONE',  ( 4.213602390902059902, -77.33743496812297735, 8.266346695140056156 ) ) ;
#21308 = CARTESIAN_POINT ( 'NONE',  ( -7.601397897754999633, -60.04999999725999515, 10.07627163191000008 ) ) ;
#21309 = ADVANCED_FACE ( 'NONE', ( #31025 ), #31798, .F. ) ;
#21310 = CARTESIAN_POINT ( 'NONE',  ( -9.757422770562000025, -79.13752739508899481, 5.632196307135999724 ) ) ;
#21311 = CARTESIAN_POINT ( 'NONE',  ( -3.075537641221584018, -77.69583333333332575, 11.44417895085269876 ) ) ;
#21312 = DIRECTION ( 'NONE',  ( 0.000000000000000000, 1.000000000000000000, 0.000000000000000000 ) ) ;
#21313 = CARTESIAN_POINT ( 'NONE',  ( -1.193682973855900498, -81.90195388324707437, -0.9265664831431897897 ) ) ;
#21314 = CARTESIAN_POINT ( 'NONE',  ( 0.2287542621979772872, -79.73975884029870542, -1.229773590461207267 ) ) ;
#21315 = AXIS2_PLACEMENT_3D ( 'NONE', #36252, #18258, #46013 ) ;
#21316 = DIRECTION ( 'NONE',  ( 0.000000000000000000, -1.000000000000000000, 0.000000000000000000 ) ) ;
#21317 = VECTOR ( 'NONE', #41423, 1000.000000000000114 ) ;
#21318 = CARTESIAN_POINT ( 'NONE',  ( -12.70299718804919742, -61.82583482774937522, -0.8845454260942260394 ) ) ;
#21319 = SURFACE_SIDE_STYLE ('',( #24889 ) ) ;
#21320 = DIRECTION ( 'NONE',  ( 0.000000000000000000, -1.000000000000000000, 0.000000000000000000 ) ) ;
#21321 = ORIENTED_EDGE ( 'NONE', *, *, #10634, .F. ) ;
#21322 = CONICAL_SURFACE ( 'NONE', #44085, 13.89999999994999946, 0.7853981633972997312 ) ;
#21323 = ORIENTED_EDGE ( 'NONE', *, *, #37170, .T. ) ;
#21324 = FACE_OUTER_BOUND ( 'NONE', #58208, .T. ) ;
#21325 = EDGE_LOOP ( 'NONE', ( #41210, #16407, #1892, #40818 ) ) ;
#21326 = CARTESIAN_POINT ( 'NONE',  ( 11.03890801094999929, -78.76613151614000685, -5.342433469444999972 ) ) ;
#21327 = EDGE_LOOP ( 'NONE', ( #19130, #42947, #45243 ) ) ;
#21328 = CARTESIAN_POINT ( 'NONE',  ( -9.538057720467248757, -80.99999999999997158, -5.099884920957399537 ) ) ;
#21329 = CARTESIAN_POINT ( 'NONE',  ( 10.89987286286000057, -77.81898427574600419, -0.6067434084558999130 ) ) ;
#21330 = CARTESIAN_POINT ( 'NONE',  ( -0.5414817640998000892, -78.87753667140100333, -9.895821147420001296 ) ) ;
#21331 = CARTESIAN_POINT ( 'NONE',  ( 5.986115112277999195, -80.09630838701978917, 9.486000076385000312 ) ) ;
#21332 = ORIENTED_EDGE ( 'NONE', *, *, #25946, .T. ) ;
#21333 = VERTEX_POINT ( 'NONE', #8319 ) ;
#21334 = B_SPLINE_CURVE_WITH_KNOTS ( 'NONE', 3,
 ( #49406, #13364, #133, #58253, #4821, #31362, #44376, #49105, #22820, #31951, #49996, #18401, #8955, #54419, #39655, #26939, #21930, #57955 ),
 .UNSPECIFIED., .F., .F.,
 ( 4, 2, 2, 2, 2, 2, 2, 2, 4 ),
 ( 0.000000000000000000, 0.1249999999999999722, 0.2499999999999999445, 0.3749999999999998890, 0.4999999999999998890, 0.6249999999999998890, 0.7499999999999997780, 0.8749999999999998890, 1.000000000000000000 ),
 .UNSPECIFIED. ) ;
#21335 = CARTESIAN_POINT ( 'NONE',  ( -5.453704473740694780, -77.52520987146617415, 7.471219652258522359 ) ) ;
#21336 = CARTESIAN_POINT ( 'NONE',  ( -0.5999999999999999778, -5.000000000000000000, -4.000000000000000000 ) ) ;
#21337 = CARTESIAN_POINT ( 'NONE',  ( 2.486604901413172808, -77.54583333333330586, -9.252740428348992907 ) ) ;
#21338 = EDGE_CURVE ( 'NONE', #21810, #33522, #11110, .T. ) ;
#21339 = CARTESIAN_POINT ( 'NONE',  ( -12.83677138650999972, -60.02737696024999536, -2.062839765282999949 ) ) ;
#21340 = CARTESIAN_POINT ( 'NONE',  ( 9.703485699160999900, -77.58108914855399973, 0.1143444355825999903 ) ) ;
#21341 = CARTESIAN_POINT ( 'NONE',  ( 7.627487606607999737, -18.70221404512000163, 10.35845616727999996 ) ) ;
#21342 = CARTESIAN_POINT ( 'NONE',  ( 0.000000000000000000, -55.54999999966999980, 12.50000000000000000 ) ) ;
#21343 = CARTESIAN_POINT ( 'NONE',  ( 6.365665562422999635, -78.73050366622999263, 10.17242851768000023 ) ) ;
#21344 = CARTESIAN_POINT ( 'NONE',  ( -1.635010352784000087, -80.48269812649999722, -10.62493487727000030 ) ) ;
#21345 = CARTESIAN_POINT ( 'NONE',  ( 12.54715396801999994, -17.46815137273999952, -1.292200816715999956 ) ) ;
#21346 = PLANE ( 'NONE',  #49708 ) ;
#21347 = B_SPLINE_CURVE_WITH_KNOTS ( 'NONE', 3,
 ( #32936, #29387, #6965, #24686 ),
 .UNSPECIFIED., .F., .F.,
 ( 4, 4 ),
 ( 0.000000000000000000, 1.000000000000000000 ),
 .UNSPECIFIED. ) ;
#21348 = VERTEX_POINT ( 'NONE', #13321 ) ;
#21349 = CARTESIAN_POINT ( 'NONE',  ( -8.478741751108000102, -53.92187496570999627, 9.108230428579000559 ) ) ;
#21350 = CARTESIAN_POINT ( 'NONE',  ( -9.690626710582000314, -78.25169696010699738, -7.043281791253000357 ) ) ;
#21351 = CARTESIAN_POINT ( 'NONE',  ( -8.194873807832001589, -17.28956116771000140, -9.389185139535999980 ) ) ;
#21353 = CARTESIAN_POINT ( 'NONE',  ( 7.601397897754999633, -18.75000000240999753, 10.07627163191000008 ) ) ;
#21352 = CARTESIAN_POINT ( 'NONE',  ( 7.613962827161000035, -55.49360374314999689, 10.53101998745000145 ) ) ;
#21354 = CARTESIAN_POINT ( 'NONE',  ( 4.635796264669566291, -79.43347470810225275, 8.027154431640754595 ) ) ;
#21355 = DIRECTION ( 'NONE',  ( 0.009503199022040095811, 0.000000000000000000, -0.9999548435846228323 ) ) ;
#21356 = CARTESIAN_POINT ( 'NONE',  ( 2.866472250631999952, -78.17792964775300391, 10.89115702734000024 ) ) ;
#21357 = CARTESIAN_POINT ( 'NONE',  ( 0.2424258809980906204, -3.499999999999999556, 3.292477318001853170 ) ) ;
#21358 = CARTESIAN_POINT ( 'NONE',  ( -8.288807259790001325, -80.88254031229138263, -7.615077709626000058 ) ) ;
#21359 = CONICAL_SURFACE ( 'NONE', #41173, 10.80312499997999964, 0.7853981633972997312 ) ;
#21360 = ORIENTED_EDGE ( 'NONE', *, *, #41212, .T. ) ;
#21361 = CARTESIAN_POINT ( 'NONE',  ( -3.172909266784524451, -3.500000000000001332, -1.019795895214234083 ) ) ;
#21362 = CARTESIAN_POINT ( 'NONE',  ( -2.061613410425999771, -55.59429985491999560, 12.83797036852999796 ) ) ;
#21363 = DIRECTION ( 'NONE',  ( 0.000000000000000000, 0.7071067811866525998, -0.7071067811864425456 ) ) ;
#21364 = VECTOR ( 'NONE', #49401, 1000.000000000000000 ) ;
#21365 = CARTESIAN_POINT ( 'NONE',  ( -1.820775719418999739, -3.635837631243000079, 3.058566008963000016 ) ) ;
#21366 = EDGE_CURVE ( 'NONE', #15598, #43389, #8909, .T. ) ;
#21367 = CARTESIAN_POINT ( 'NONE',  ( -3.818323177486000031, -79.42900767078099022, 8.616648607789999303 ) ) ;
#21368 = CARTESIAN_POINT ( 'NONE',  ( -12.44209697057999975, -54.71557297424000410, 1.464771213333999844 ) ) ;
#21369 = CARTESIAN_POINT ( 'NONE',  ( -5.299999999999999822, -75.00000000000000000, 0.000000000000000000 ) ) ;
#21370 = CARTESIAN_POINT ( 'NONE',  ( -0.005119011379994000376, -61.73813862155999743, 12.43705489347999915 ) ) ;
#21371 = CARTESIAN_POINT ( 'NONE',  ( 12.70556836352000118, -62.02772277195000328, 2.424222323408999617E-09 ) ) ;
#21372 = CARTESIAN_POINT ( 'NONE',  ( 2.266462915304999992, -85.26849735065199809, -3.506101190763999842 ) ) ;
#21373 = CARTESIAN_POINT ( 'NONE',  ( 9.611650271896843734, -77.40833333333328881, -5.539808784079876425 ) ) ;
#21374 = CARTESIAN_POINT ( 'NONE',  ( -5.101716603136247308, -77.04332471689124873, -10.93886256472661778 ) ) ;
#21375 = ADVANCED_FACE ( 'NONE', ( #26319 ), #46002, .F. ) ;
#21376 = CARTESIAN_POINT ( 'NONE',  ( 8.298649457567281118, -76.38737123282477626, -8.318302812671584334 ) ) ;
#21377 = CARTESIAN_POINT ( 'NONE',  ( 0.1369776181910999924, -77.01514836410099463, 11.03100047655000004 ) ) ;
#21378 = CARTESIAN_POINT ( 'NONE',  ( -0.07104694739953303084, -81.98010065232054444, 1.247827375486972645 ) ) ;
#21379 = CARTESIAN_POINT ( 'NONE',  ( -1.327657890597083279, -1.010175696052641348, 2.983557525922736708 ) ) ;
#21380 = ADVANCED_FACE ( 'NONE', ( #44634 ), #36348, .T. ) ;
#21381 = CARTESIAN_POINT ( 'NONE',  ( 9.670530767802999250, -76.95816816192808574, -0.1674091926992999912 ) ) ;
#21382 = CARTESIAN_POINT ( 'NONE',  ( -9.554796630153999715, -79.51004415034600470, -0.02401403847836000235 ) ) ;
#21383 = CARTESIAN_POINT ( 'NONE',  ( -0.8982906067046061427, -0.8151041484501103662, -3.345820488051431507 ) ) ;
#21384 = CARTESIAN_POINT ( 'NONE',  ( -4.634473952174339217, -80.18982139357595429, -9.715902795605705577 ) ) ;
#21385 = B_SPLINE_CURVE_WITH_KNOTS ( 'NONE', 3,
 ( #18386, #13941, #31937, #23095, #50269, #49980, #9523, #45551, #18679, #41106, #54971, #697, #27801, #45847, #983, #18967, #10991, #56435 ),
 .UNSPECIFIED., .F., .F.,
 ( 4, 2, 2, 2, 2, 2, 2, 2, 4 ),
 ( 0.000000000000000000, 0.06249999999999567013, 0.1249999999999913403, 0.2499999999999929501, 0.4999999999999955591, 0.7499999999999991118, 0.8125000000000019984, 0.8750000000000048850, 1.000000000000000000 ),
 .UNSPECIFIED. ) ;
#21386 = CARTESIAN_POINT ( 'NONE',  ( -11.99999999994999911, -76.29999999994899440, 3.078392110872999642E-09 ) ) ;
#21387 = CARTESIAN_POINT ( 'NONE',  ( 6.031068391564602393, -75.80000000000002558, 10.45132295220961538 ) ) ;
#21388 = CARTESIAN_POINT ( 'NONE',  ( 9.785129497364000173, -79.26670666393400211, -6.997026981537000090 ) ) ;
#21389 = DIRECTION ( 'NONE',  ( 0.000000000000000000, 0.000000000000000000, -1.000000000000000000 ) ) ;
#21390 = CARTESIAN_POINT ( 'NONE',  ( -9.845147265217999433, -79.36375811998600227, -5.468732932272000191 ) ) ;
#21391 = CARTESIAN_POINT ( 'NONE',  ( -10.98384481689545034, -23.22882187213843963, -0.5959944459583164100 ) ) ;
#21392 = ORIENTED_EDGE ( 'NONE', *, *, #1146, .T. ) ;
#21393 = CARTESIAN_POINT ( 'NONE',  ( -0.5222397221919125032, -25.16298219400451686, 12.70447686583787572 ) ) ;
#21394 = ORIENTED_EDGE ( 'NONE', *, *, #26460, .T. ) ;
#21395 = CARTESIAN_POINT ( 'NONE',  ( 10.12290050122000018, -55.54999999974999980, -7.648026767069000087 ) ) ;
#21396 = CIRCLE ( 'NONE', #34583, 12.90000000000000036 ) ;
#21397 = VERTEX_POINT ( 'NONE', #17768 ) ;
#21398 = CARTESIAN_POINT ( 'NONE',  ( 1.800092392015347098, -3.500000000000000000, -3.095232311630156108 ) ) ;
#21399 = PRODUCT_DEFINITION ( 'UNKNOWN', '', #30089, #43990 ) ;
#21400 = DIRECTION ( 'NONE',  ( 0.000000000000000000, 0.000000000000000000, 1.000000000000000000 ) ) ;
#21401 = CIRCLE ( 'NONE', #56269, 1.749999999999997780 ) ;
#21402 = B_SPLINE_SURFACE_WITH_KNOTS ( 'NONE', 3, 3, ( 
 ( #36449, #50923, #54478, #37324 ),
 ( #14594, #18746, #14013, #32011 ),
 ( #50340, #9891, #9598, #45627 ),
 ( #769, #27873, #45918, #5453 ),
 ( #37032, #55046, #57864, #29829 ),
 ( #17418, #35404, #16853, #25415 ),
 ( #3279, #21271, #57570, #16279 ),
 ( #34259, #52291, #39278, #44289 ) ),
 .UNSPECIFIED., .F., .F., .F.,
 ( 4, 1, 1, 1, 1, 4 ),
 ( 4, 4 ),
 ( -0.01200407347463999970, 0.000000000000000000, 0.3333333333333000081, 0.6666666666667000474, 1.000000000000000000, 1.011997855551999947 ),
 ( -0.3559705542741000150, 1.355970554273999928 ),
 .UNSPECIFIED. ) ;
#21403 = CARTESIAN_POINT ( 'NONE',  ( -3.062358763434999798, -80.25731627376899269, 1.872352532395999969 ) ) ;
#21404 = CARTESIAN_POINT ( 'NONE',  ( 0.7542767905157096164, -79.26850739209180574, 9.471697596554010445 ) ) ;
#21405 = VERTEX_POINT ( 'NONE', #9201 ) ;
#21406 = CARTESIAN_POINT ( 'NONE',  ( 9.070041738308999513, -79.31372763096999279, 8.129404524763000239 ) ) ;
#21407 = AXIS2_PLACEMENT_3D ( 'NONE', #14293, #34532, #49003 ) ;
#21408 = VERTEX_POINT ( 'NONE', #35457 ) ;
#21409 = ORIENTED_EDGE ( 'NONE', *, *, #37501, .T. ) ;
#21410 = DIRECTION ( 'NONE',  ( 0.000000000000000000, -1.000000000000000000, 0.000000000000000000 ) ) ;
#21411 = CIRCLE ( 'NONE', #49712, 9.950000000000001066 ) ;
#21412 = CARTESIAN_POINT ( 'NONE',  ( 3.708203932500000022, -75.80000000000001137, 11.41267819554000162 ) ) ;
#21413 = EDGE_CURVE ( 'NONE', #40983, #49519, #22621, .T. ) ;
#21414 = CARTESIAN_POINT ( 'NONE',  ( -3.411549236729638945, -80.00087276832812222, 10.19443305130964283 ) ) ;
#21415 = DIRECTION ( 'NONE',  ( -4.762495317921000031E-11, 1.000000000000000000, -4.762546956201999894E-11 ) ) ;
#21416 = CARTESIAN_POINT ( 'NONE',  ( 0.4236117777057033518, -86.31452042059397911, -4.025010272438366954 ) ) ;
#21417 = DIRECTION ( 'NONE',  ( 1.000000000000000000, 0.000000000000000000, 0.000000000000000000 ) ) ;
#21418 = B_SPLINE_CURVE_WITH_KNOTS ( 'NONE', 3,
 ( #327, #17718, #4725, #14148, #40736, #23015, #31261, #617, #28012, #29, #45765, #18305, #35702, #18600, #36589 ),
 .UNSPECIFIED., .F., .F.,
 ( 4, 1, 1, 1, 1, 1, 1, 1, 1, 1, 1, 1, 4 ),
 ( 0.000000000000000000, 0.05991653944398223075, 0.1464624072683559930, 0.2330082750926717738, 0.3195541429170455361, 0.4061000107414192706, 0.4926458785657931161, 0.5791917463901669061, 0.6657376142143087705, 0.7522834820388564214, 0.8388293498634040724, 0.9253752176879519453, 1.000000000000000000 ),
 .UNSPECIFIED. ) ;
#21419 = CARTESIAN_POINT ( 'NONE',  ( -1.349038754591999956, -78.12242034399000090, -13.04399231589999886 ) ) ;
#21420 = EDGE_CURVE ( 'NONE', #36179, #13579, #50822, .T. ) ;
#21421 = CARTESIAN_POINT ( 'NONE',  ( 11.69353635062999963, -78.11477256742000463, 5.202647212677000255 ) ) ;
#21422 = CARTESIAN_POINT ( 'NONE',  ( 1.521043722421000055, -76.59490344678600593, -10.89349724765000005 ) ) ;
#21423 = CARTESIAN_POINT ( 'NONE',  ( -1.276771495430000038E-14, -69.50420297070000686, 0.000000000000000000 ) ) ;
#21424 = CARTESIAN_POINT ( 'NONE',  ( 8.631763462862000580, -77.22223667140100645, -4.015524064286999817 ) ) ;
#21425 = CARTESIAN_POINT ( 'NONE',  ( 0.6322386839596000341, -82.41796443320698984, -3.912314205455000415 ) ) ;
#21426 = DIRECTION ( 'NONE',  ( 0.000000000000000000, -1.000000000000000000, 0.000000000000000000 ) ) ;
#21427 = CARTESIAN_POINT ( 'NONE',  ( 2.056655112429589760, -2.920778328515915678, 2.518430561230568632 ) ) ;
#21428 = CARTESIAN_POINT ( 'NONE',  ( 3.537250157901000058, -79.48030496681158752, 0.2634839111148000179 ) ) ;
#21429 = CARTESIAN_POINT ( 'NONE',  ( -13.94827586207000003, -33.10361340872000113, -8.082385102019000922E-06 ) ) ;
#21430 = CARTESIAN_POINT ( 'NONE',  ( 1.483688553140142252, -80.96438982575540422, 10.64694122786772468 ) ) ;
#21431 = CARTESIAN_POINT ( 'NONE',  ( -2.845754477180000297, -83.10399735065199422, 2.113443956577000016 ) ) ;
#21432 = CARTESIAN_POINT ( 'NONE',  ( -1.568660613942000071, -1.839195589987000057, -3.467930652269000102 ) ) ;
#21433 = CARTESIAN_POINT ( 'NONE',  ( -1.260553452884753955, -79.73788096563870909, 0.1933511446621866969 ) ) ;
#21434 = CARTESIAN_POINT ( 'NONE',  ( 10.47020627418437932, -80.22916666666665719, -2.813789756862290492 ) ) ;
#21435 = CARTESIAN_POINT ( 'NONE',  ( -9.797890753601748770, -79.25056356931708024, 7.009672782845666639 ) ) ;
#21436 = CARTESIAN_POINT ( 'NONE',  ( -0.7068627984950999199, -81.09756764886000724, 1.130893941374999878 ) ) ;
#21437 = CARTESIAN_POINT ( 'NONE',  ( -12.68625206996000010, -18.23580249185999946, -1.886949102778999965 ) ) ;
#21438 = CARTESIAN_POINT ( 'NONE',  ( 12.72558241036999860, -23.20131830507999737, 1.930284820930999956 ) ) ;
#21439 = CARTESIAN_POINT ( 'NONE',  ( -11.00000000000000000, -79.69999999999998863, 0.000000000000000000 ) ) ;
#21440 = CARTESIAN_POINT ( 'NONE',  ( 1.217390015642369372, -24.81893024925991753, -12.70229597941076172 ) ) ;
#21441 = CARTESIAN_POINT ( 'NONE',  ( 10.18629808814000093, -76.37939569223999570, 7.004515126288999305 ) ) ;
#21442 = ORIENTED_EDGE ( 'NONE', *, *, #12940, .F. ) ;
#21443 = DIRECTION ( 'NONE',  ( 0.000000000000000000, -1.000000000000000000, 0.000000000000000000 ) ) ;
#21444 = CARTESIAN_POINT ( 'NONE',  ( 3.451879464910999840, -85.80681307243298761, -1.536875756006000016 ) ) ;
#21445 = AXIS2_PLACEMENT_3D ( 'NONE', #50026, #8988, #44408 ) ;
#21446 = ADVANCED_FACE ( 'NONE', ( #23360 ), #19603, .F. ) ;
#21447 = CARTESIAN_POINT ( 'NONE',  ( 12.54981857179000038, -61.84836586168999872, -0.03768635776142000016 ) ) ;
#21448 = CARTESIAN_POINT ( 'NONE',  ( -1.799475295154000065, -21.75083378359999742, -12.69619287811000063 ) ) ;
#21449 = CARTESIAN_POINT ( 'NONE',  ( -0.1527179957142000277, -78.26932405616399535, 9.629635879864999026 ) ) ;
#21450 = AXIS2_PLACEMENT_3D ( 'NONE', #56808, #33261, #52383 ) ;
#21451 = ADVANCED_FACE ( 'NONE', ( #41658 ), #54941, .F. ) ;
#21452 = CARTESIAN_POINT ( 'NONE',  ( -3.894423402048999616, -83.23150571593399150, -1.504352435119000075 ) ) ;
#21453 = CARTESIAN_POINT ( 'NONE',  ( -2.804788745061338240, -79.99636019303807188, 10.37822998189701806 ) ) ;
#21454 = CARTESIAN_POINT ( 'NONE',  ( -1.034826241750000264, -80.48209164690899797, 1.108174957742000144 ) ) ;
#21455 = ORIENTED_EDGE ( 'NONE', *, *, #51033, .T. ) ;
#21456 = CARTESIAN_POINT ( 'NONE',  ( -12.70556836347999941, -16.77227722772000007, 1.774192816106000118E-09 ) ) ;
#21457 = CARTESIAN_POINT ( 'NONE',  ( 1.097898070916953239, -82.12630208333071380, 0.8448041534256599538 ) ) ;
#21458 = AXIS2_PLACEMENT_3D ( 'NONE', #392, #31331, #4787 ) ;
#21459 = CARTESIAN_POINT ( 'NONE',  ( -3.065563091283566521, -78.78445349890496630, -2.577180195798276063 ) ) ;
#21460 = ORIENTED_EDGE ( 'NONE', *, *, #52626, .T. ) ;
#21461 = CARTESIAN_POINT ( 'NONE',  ( -10.62234821842000088, -78.85158459378298801, 2.617925641156000349 ) ) ;
#21462 = CARTESIAN_POINT ( 'NONE',  ( -10.45204383623999966, -59.56256649442000395, 7.651147548074000326 ) ) ;
#21463 = DIRECTION ( 'NONE',  ( 0.000000000000000000, 0.000000000000000000, -1.000000000000000000 ) ) ;
#21464 = ORIENTED_EDGE ( 'NONE', *, *, #46109, .T. ) ;
#21465 = CARTESIAN_POINT ( 'NONE',  ( 0.4919088493939999807, -77.63064477680499920, 12.15485731165999894 ) ) ;
#21466 = EDGE_LOOP ( 'NONE', ( #29889, #44934, #55744, #21965, #41871 ) ) ;
#21467 = ORIENTED_EDGE ( 'NONE', *, *, #24749, .T. ) ;
#21468 = EDGE_CURVE ( 'NONE', #51903, #46323, #24327, .T. ) ;
#21469 = CARTESIAN_POINT ( 'NONE',  ( -1.629367637659999923, -18.31736356602000271, 12.46114270826000059 ) ) ;
#21470 = CARTESIAN_POINT ( 'NONE',  ( 0.000000000000000000, -74.64999999999999147, 0.000000000000000000 ) ) ;
#21471 = LINE ( 'NONE', #26462, #49661 ) ;
#21472 = B_SPLINE_SURFACE_WITH_KNOTS ( 'NONE', 3, 3, ( 
 ( #34317, #7472, #11622, #25762, #43782, #33745, #7180, #43203, #29311, #12191, #56777, #3334, #29597, #47361, #30470, #21616, #47653, #21329, #16339, #20758, #8041, #11333, #52921, #2473, #42915, #25468, #34028, #34892, #34606, #48499, #48225, #56487, #16909, #7757, #51781, #39339, #52353, #43488, #25180, #57345, #12468, #6891, #2757, #38759, #24897, #26039, #11904, #44064, #3049, #20476, #3612, #39622, #21044, #57630, #39047, #57061, #16044, #52067, #36356, #44342, #3895, #49368, #13036, #49959, #13625, #27489, #12754 ),
 ( #13330, #5076, #48784, #23071, #53796, #31034, #35767, #8620, #41085, #17185, #44936, #40502, #39907, #21898, #98, #22192, #44643, #17777, #30750, #4196, #31623, #58215, #18073, #36067, #54087, #27195, #49666, #26605, #45235, #8328, #9209, #4782, #57920, #22784, #40792, #387, #56700, #15799, #24943, #7807, #57107, #48271, #11385, #47698, #29360, #30228, #56249, #43252, #34939, #21377, #39098, #56535, #56827, #25808, #25519, #2236, #43836, #20235, #47409, #3383, #2808, #16096, #12521, #52682, #39392, #7228, #20522 ),
 ( #38520, #47984, #8095, #29932, #7522, #11954, #38809, #12237, #57399, #30518, #48548, #43535, #38229, #25232, #3099, #34076, #33788, #11671, #20802, #51830, #6940, #42963, #2520, #16673, #21094, #52112, #16957, #34654, #29646, #26090, #16381, #34366, #52400, #21665, #9265, #31969, #13974, #44694, #17833, #17529, #4249, #26959, #35820, #22246, #49722, #40849, #22547, #40558, #441, #150, #26374, #57677, #9558, #53850, #50012, #44989, #54438, #49423, #27250, #44116, #39671, #18419, #30801, #3945, #13382, #31382, #8973 ),
 ( #40257, #18127, #35222, #31085, #53252, #12802, #58270, #4840, #17235, #3665, #4545, #57973, #36122, #44393, #48833, #8376, #54138, #13678, #21948, #39960, #31676, #49122, #13087, #45290, #35520, #8672, #22835, #26661, #36410, #53549, #41719, #37574, #10431, #1017, #55590, #15442, #46463, #28416, #1882, #15140, #42313, #50302, #10145, #41137, #9851, #33135, #23997, #51178, #36702, #14554, #54717, #10735, #23128, #28122, #19876, #46763, #5991, #23419, #23709, #28711, #50885, #27542, #6285, #45585, #14260, #24300, #46172 ) ),
 .UNSPECIFIED., .F., .F., .F.,
 ( 4, 4 ),
 ( 4, 1, 1, 1, 1, 1, 1, 1, 1, 1, 1, 1, 1, 1, 1, 1, 1, 1, 1, 1, 1, 1, 1, 1, 1, 1, 1, 1, 1, 1, 1, 1, 1, 1, 1, 1, 1, 1, 1, 1, 1, 1, 1, 1, 1, 1, 1, 1, 1, 1, 1, 1, 1, 1, 1, 1, 1, 1, 1, 1, 1, 1, 1, 1, 4 ),
 ( -0.1772706441294000235, 1.177270644128999955 ),
 ( -0.02000000000000000042, -0.003749999999999999861, 0.01250000000000000069, 0.02875000000000000125, 0.04499999999999999833, 0.06124999999999999889, 0.07749999999999999944, 0.09375000000000000000, 0.1100000000000000006, 0.1262500000000000011, 0.1424999999999999878, 0.1587500000000000022, 0.1749999999999999889, 0.1912500000000000033, 0.2074999999999999900, 0.2237500000000000044, 0.2399999999999999911, 0.2562499999999999778, 0.2725000000000000200, 0.2887500000000000067, 0.3049999999999999933, 0.3212499999999999800, 0.3375000000000000222, 0.3537500000000000089, 0.3699999999999999956, 0.3862499999999999822, 0.4025000000000000244, 0.4187500000000000111, 0.4349999999999999978, 0.4512499999999999845, 0.4675000000000000266, 0.4837500000000000133, 0.5000000000000000000, 0.5162499999999999867, 0.5324999999999999734, 0.5487499999999999600, 0.5649999999999999467, 0.5812500000000000444, 0.5975000000000000311, 0.6137500000000000178, 0.6300000000000000044, 0.6462499999999999911, 0.6624999999999999778, 0.6787499999999999645, 0.6949999999999999512, 0.7112500000000000488, 0.7275000000000000355, 0.7437500000000000222, 0.7600000000000000089, 0.7762499999999999956, 0.7924999999999999822, 0.8087499999999999689, 0.8249999999999999556, 0.8412500000000000533, 0.8575000000000000400, 0.8737500000000000266, 0.8900000000000000133, 0.9062500000000000000, 0.9224999999999999867, 0.9387499999999999734, 0.9549999999999999600, 0.9712499999999999467, 0.9875000000000000444, 1.003749999999999920, 1.020000000000000018 ),
 .UNSPECIFIED. ) ;
#21473 = EDGE_LOOP ( 'NONE', ( #10749, #11910, #23157, #57518, #12582, #54157 ) ) ;
#21474 = CARTESIAN_POINT ( 'NONE',  ( 12.70556836343000029, -53.57227722738999631, -1.774194422348999890E-09 ) ) ;
#21475 = ORIENTED_EDGE ( 'NONE', *, *, #55835, .F. ) ;
#21476 = CARTESIAN_POINT ( 'NONE',  ( 0.4727252345235593567, -79.49457189493710985, 1.183769161397306258 ) ) ;
#21477 = CARTESIAN_POINT ( 'NONE',  ( -0.03487147506507188438, -79.00321104920828930, -3.699835669024340579 ) ) ;
#21478 = CARTESIAN_POINT ( 'NONE',  ( 8.652389292562999046, -53.53734871844999788, 9.414476472778000371 ) ) ;
#21479 = LINE ( 'NONE', #25615, #43071 ) ;
#21480 = DIRECTION ( 'NONE',  ( 0.000000000000000000, -1.000000000000000000, 0.000000000000000000 ) ) ;
#21481 = EDGE_CURVE ( 'NONE', #4986, #25253, #1237, .T. ) ;
#21482 = CARTESIAN_POINT ( 'NONE',  ( 12.70255466323004967, -61.54616562044007111, -1.306323829481652821 ) ) ;
#21483 = CARTESIAN_POINT ( 'NONE',  ( 0.9109609374202407572, -78.02623425204966168, -1.202808138275179184 ) ) ;
#21484 = CARTESIAN_POINT ( 'NONE',  ( -10.12290050256999940, -18.75000002239000096, -7.648026768411000376 ) ) ;
#21485 = CARTESIAN_POINT ( 'NONE',  ( -10.35410175339000105, -23.40399325350999860, 7.619715687203000520 ) ) ;
#21486 = CARTESIAN_POINT ( 'NONE',  ( -3.743366236640000455, -80.25300264934799088, -1.848461251573999986 ) ) ;
#21487 = CARTESIAN_POINT ( 'NONE',  ( 8.149610418757999852, -77.55328667140099697, 5.375310761231999912 ) ) ;
#21488 = CARTESIAN_POINT ( 'NONE',  ( -12.43570956085999946, -17.12016029981999665, 0.4384071701242000518 ) ) ;
#21489 = VECTOR ( 'NONE', #15221, 1000.000000000000114 ) ;
#21490 = CARTESIAN_POINT ( 'NONE',  ( 11.00000000000000000, -77.84999999999999432, 0.000000000000000000 ) ) ;
#21491 = CARTESIAN_POINT ( 'NONE',  ( 5.459501886381000091, -76.15997619157100473, -11.00074850082999767 ) ) ;
#21492 = CARTESIAN_POINT ( 'NONE',  ( -8.190859204290999784, -59.94999999967000548, -7.342331066867000544 ) ) ;
#21493 = CARTESIAN_POINT ( 'NONE',  ( 2.362319013936999834, -1.467935987230000183, -3.378608031078000007 ) ) ;
#21494 = CARTESIAN_POINT ( 'NONE',  ( -0.6295237254636235624, -78.58333333333331439, -1.092232985442822990 ) ) ;
#21495 = CARTESIAN_POINT ( 'NONE',  ( -1.091678962010041332, -80.91005275380919670, -1.044836448518165595 ) ) ;
#21496 = CARTESIAN_POINT ( 'NONE',  ( 2.265947762240999808, -77.10112295295309082, -9.216051757218000517 ) ) ;
#21497 = CARTESIAN_POINT ( 'NONE',  ( -0.7259747304966001069, -78.82016653067499590, 1.442281046339000117 ) ) ;
#21498 = CARTESIAN_POINT ( 'NONE',  ( 1.405334850312945250, -24.31492947779451796, 12.50716844834712660 ) ) ;
#21499 = CARTESIAN_POINT ( 'NONE',  ( -3.306807500130999777, -3.438473948318000240, 1.312446816095000024 ) ) ;
#21500 = CARTESIAN_POINT ( 'NONE',  ( 0.9868626873424000134, -78.00481147984399399, -12.24017488508000007 ) ) ;
#21501 = CARTESIAN_POINT ( 'NONE',  ( 0.3926218265389159190, -80.85416666666667140, 1.460959015002474715 ) ) ;
#21503 = CARTESIAN_POINT ( 'NONE',  ( -0.9509180703096998810, -78.80288933763399939, -0.9145055679095001056 ) ) ;
#21502 = DIRECTION ( 'NONE',  ( 1.000000000000000000, 0.000000000000000000, 0.000000000000000000 ) ) ;
#21504 = CARTESIAN_POINT ( 'NONE',  ( 1.307088170492999968, -81.35043415305999304, 0.3427697847655999941 ) ) ;
#21505 = CARTESIAN_POINT ( 'NONE',  ( -8.125470958442424063, -79.54330210541110091, 7.039620741617721222 ) ) ;
#21506 = ORIENTED_EDGE ( 'NONE', *, *, #1465, .F. ) ;
#21507 = CARTESIAN_POINT ( 'NONE',  ( -12.00000000000000000, -78.89999999999999147, -1.868256502752000067E-14 ) ) ;
#21508 = CARTESIAN_POINT ( 'NONE',  ( 7.657575756372000164, -79.51128919345099177, 9.292673803815999278 ) ) ;
#21509 = B_SPLINE_CURVE_WITH_KNOTS ( 'NONE', 3,
 ( #49989, #27226, #416, #18686, #9535, #50566, #50277, #49399, #9827, #14238, #27518, #14529, #18394, #36968, #44966, #4520, #4222, #27809 ),
 .UNSPECIFIED., .F., .F.,
 ( 4, 2, 2, 2, 2, 2, 2, 2, 4 ),
 ( 0.000000000000000000, 0.1249999999999999722, 0.2499999999999999445, 0.3749999999999998890, 0.4999999999999998890, 0.6249999999999998890, 0.7499999999999997780, 0.8749999999999998890, 1.000000000000000000 ),
 .UNSPECIFIED. ) ;
#21510 = CARTESIAN_POINT ( 'NONE',  ( -4.833288342901160384, -79.16736403866717353, 8.201749509104971025 ) ) ;
#21511 = DIRECTION ( 'NONE',  ( 0.000000000000000000, -1.000000000000000000, 0.000000000000000000 ) ) ;
#21512 = CARTESIAN_POINT ( 'NONE',  ( -8.796335266380006956, -79.04791666666669414, 6.760013919724027431 ) ) ;
#21513 = CARTESIAN_POINT ( 'NONE',  ( -3.526725475056999848, -1.050894741108000074, -0.2894248236847000166 ) ) ;
#21514 = CARTESIAN_POINT ( 'NONE',  ( -7.948284285155000184, -79.75644446212498906, -5.699806846671999772 ) ) ;
#21515 = CARTESIAN_POINT ( 'NONE',  ( 12.66314513616999982, -25.17864743362000013, 0.04033065750139999683 ) ) ;
#21516 = CARTESIAN_POINT ( 'NONE',  ( -9.369164850722000892, -55.54999999966999980, -7.601397897754999633 ) ) ;
#21517 = VERTEX_POINT ( 'NONE', #28355 ) ;
#21518 = CARTESIAN_POINT ( 'NONE',  ( 12.57042253521000141, -62.90094976977999863, 0.000000000000000000 ) ) ;
#21519 = CARTESIAN_POINT ( 'NONE',  ( 6.190793678633999875, -79.50046001420199104, -7.521868196643000992 ) ) ;
#21520 = VECTOR ( 'NONE', #34645, 1000.000000000000000 ) ;
#21521 = CARTESIAN_POINT ( 'NONE',  ( -2.589715347022274017, -1.653783639445655762, -2.004944695761151863 ) ) ;
#21522 = DIRECTION ( 'NONE',  ( 1.000000000000000000, 0.000000000000000000, 0.000000000000000000 ) ) ;
#21523 = CARTESIAN_POINT ( 'NONE',  ( -1.603789611582999930, -80.41062457329998381, -0.4506860216877000558 ) ) ;
#21524 = EDGE_LOOP ( 'NONE', ( #2108, #43138, #57427, #47556 ) ) ;
#21525 = DIRECTION ( 'NONE',  ( 0.000000000000000000, -0.1122098755727947705, -0.9936845293270585300 ) ) ;
#21526 = CARTESIAN_POINT ( 'NONE',  ( 9.298485322489097982, -61.68812323674666231, -8.385852789353158698 ) ) ;
#21527 = DIRECTION ( 'NONE',  ( 0.000000000000000000, 1.000000000000000000, 0.000000000000000000 ) ) ;
#21528 = STYLED_ITEM ( 'NONE', ( #20422 ), #17297 ) ;
#21529 = ADVANCED_FACE ( 'NONE', ( #24524 ), #27119, .T. ) ;
#21530 = CARTESIAN_POINT ( 'NONE',  ( -0.7999999997951999786, -18.85000000927000130, 11.99999999979999821 ) ) ;
#21531 = CARTESIAN_POINT ( 'NONE',  ( -7.765024210398999926, -54.70905971351000119, -9.830784063398999351 ) ) ;
#21532 =( LENGTH_UNIT ( ) NAMED_UNIT ( * ) SI_UNIT ( .MILLI., .METRE. ) );
#21533 = CARTESIAN_POINT ( 'NONE',  ( -8.448510849392999233, -79.28831818069899384, 4.901364000006999788 ) ) ;
#21534 = ORIENTED_EDGE ( 'NONE', *, *, #23830, .T. ) ;
#21535 = ORIENTED_EDGE ( 'NONE', *, *, #37817, .F. ) ;
#21536 = CARTESIAN_POINT ( 'NONE',  ( 1.330647945963000067, -76.69316330962899997, 12.51808036622999865 ) ) ;
#21537 = CARTESIAN_POINT ( 'NONE',  ( 0.7999999997951999786, -18.85000000927000130, -11.99999999979999821 ) ) ;
#21538 = CARTESIAN_POINT ( 'NONE',  ( -1.375956693795999941, -77.66350764398998763, -0.3562251950211999807 ) ) ;
#21539 = ORIENTED_EDGE ( 'NONE', *, *, #15617, .F. ) ;
#21540 = CARTESIAN_POINT ( 'NONE',  ( 9.426477049435000310, -77.43058084965399246, -1.139727483088999849 ) ) ;
#21541 = DIRECTION ( 'NONE',  ( -1.000000000000000000, 0.000000000000000000, 0.000000000000000000 ) ) ;
#21542 = CARTESIAN_POINT ( 'NONE',  ( -5.917523019358058356, -75.88333333333329733, -10.26699006316253282 ) ) ;
#21543 = CARTESIAN_POINT ( 'NONE',  ( 11.54974070075000014, -78.53893426687999124, 5.138670156068000594 ) ) ;
#21544 = PRODUCT_DEFINITION_CONTEXT ( 'detailed design', #8898, 'design' ) ;
#21545 = CARTESIAN_POINT ( 'NONE',  ( 10.29113596735999892, -77.53255742550288687, 4.462133020506000136 ) ) ;
#21547 = EDGE_CURVE ( 'NONE', #35878, #1239, #56510, .T. ) ;
#21546 = DIRECTION ( 'NONE',  ( -0.7071067811865475727, 0.000000000000000000, 0.7071067811865475727 ) ) ;
#21548 = CARTESIAN_POINT ( 'NONE',  ( -0.4881686207923673915, -86.17851879815599148, 3.925966920820173733 ) ) ;
#21549 = DIRECTION ( 'NONE',  ( 0.7071067811865475727, 0.000000000000000000, -0.7071067811865475727 ) ) ;
#21550 = CARTESIAN_POINT ( 'NONE',  ( 7.624341764923000753, -18.73514850530999709, 10.42531124853000080 ) ) ;
#21551 = CARTESIAN_POINT ( 'NONE',  ( -0.8502109015516584600, -82.25000000000000000, -0.9397329394915318046 ) ) ;
#21552 = ORIENTED_EDGE ( 'NONE', *, *, #42573, .T. ) ;
#21553 = CARTESIAN_POINT ( 'NONE',  ( -7.208482872893000604, -79.55106226310599027, 8.658331769851001170 ) ) ;
#21554 = CARTESIAN_POINT ( 'NONE',  ( 9.249971803402324610, -77.34340569116132258, -0.7721083477804356887 ) ) ;
#21555 = DIRECTION ( 'NONE',  ( 0.000000000000000000, -1.000000000000000000, 0.000000000000000000 ) ) ;
#21556 = CARTESIAN_POINT ( 'NONE',  ( 9.579193661067593624, -77.09808761060168081, -7.313663711862215422 ) ) ;
#21557 = CARTESIAN_POINT ( 'NONE',  ( -1.100846539600000007, -79.19859309350199794, -0.6190985795237999856 ) ) ;
#21558 = AXIS2_PLACEMENT_3D ( 'NONE', #45052, #4605, #40011 ) ;
#21559 = CARTESIAN_POINT ( 'NONE',  ( -9.500094076791862463, -79.39994338716823563, -4.328536937075411965E-07 ) ) ;
#21560 = CARTESIAN_POINT ( 'NONE',  ( -3.422254106058401746, -78.35090439325858824, 11.58678479484117219 ) ) ;
#21561 = EDGE_CURVE ( 'NONE', #17250, #38390, #9232, .T. ) ;
#21562 = CARTESIAN_POINT ( 'NONE',  ( 0.000000000000000000, -75.09999999979599750, -4.899999999795999983 ) ) ;
#21563 = CARTESIAN_POINT ( 'NONE',  ( 8.838834764832000701, -55.54999999966999980, 8.838834764832000701 ) ) ;
#21564 = CARTESIAN_POINT ( 'NONE',  ( -9.242272388666000538, -79.00961649866798098, 6.250760013846000440 ) ) ;
#21565 = CARTESIAN_POINT ( 'NONE',  ( 10.38646360831000059, -19.22204592323999961, -7.655555357453000198 ) ) ;
#21566 = CARTESIAN_POINT ( 'NONE',  ( 11.00000000000000000, -76.04999999999999716, -1.235102163740000267E-09 ) ) ;
#21567 = CARTESIAN_POINT ( 'NONE',  ( 0.5573607202496000390, -79.08816791445418914, -4.134721415477000228 ) ) ;
#21568 = EDGE_CURVE ( 'NONE', #54597, #33739, #31841, .T. ) ;
#21569 = CARTESIAN_POINT ( 'NONE',  ( 1.407171709420391936, -77.86458333333330017, 10.75000000000000178 ) ) ;
#21570 = VERTEX_POINT ( 'NONE', #46401 ) ;
#21571 = CARTESIAN_POINT ( 'NONE',  ( -1.491081270832000039, -81.78991179838999415, 0.8224925373206000145 ) ) ;
#21572 = CARTESIAN_POINT ( 'NONE',  ( -1.223477145616999939, -79.91002549588999671, 0.8121269926547999285 ) ) ;
#21573 = CARTESIAN_POINT ( 'NONE',  ( 9.249827694200002171, -79.25056085624731850, 0.06519332901358350363 ) ) ;
#21574 = CARTESIAN_POINT ( 'NONE',  ( -3.545645331619000196, -77.46501628338398859, 11.44309676683000099 ) ) ;
#21575 = CARTESIAN_POINT ( 'NONE',  ( -8.130813118348999780, -54.11476110100999648, 9.546856411314999846 ) ) ;
#21576 = CARTESIAN_POINT ( 'NONE',  ( -1.510823314100999903, -83.28820597566100048, -0.3534059060544000319 ) ) ;
#21577 = VECTOR ( 'NONE', #23159, 1000.000000000000000 ) ;
#21578 = CARTESIAN_POINT ( 'NONE',  ( 10.14226539039000130, -78.37076856562599403, 6.290465419776000822 ) ) ;
#21579 = CARTESIAN_POINT ( 'NONE',  ( -0.8481231068849000021, -78.95189805011500539, 9.686304223355000076 ) ) ;
#21580 = CARTESIAN_POINT ( 'NONE',  ( 1.288488638075999893, -54.26435060599999360, -12.54709296479000002 ) ) ;
#21581 = CARTESIAN_POINT ( 'NONE',  ( 9.770627950922811777, -75.99681967017289708, 6.526574872315616282 ) ) ;
#21582 = CARTESIAN_POINT ( 'NONE',  ( 1.592434616855533891, -86.09999999999999432, 3.669353075276593046 ) ) ;
#21583 = VERTEX_POINT ( 'NONE', #36640 ) ;
#21584 = LINE ( 'NONE', #3580, #6709 ) ;
#21585 = CARTESIAN_POINT ( 'NONE',  ( -12.00000000000000000, -23.25000000000000000, 1.750000000000000000 ) ) ;
#21586 = CARTESIAN_POINT ( 'NONE',  ( -11.56229308710999959, -79.35377338295398886, -4.110692102696999584 ) ) ;
#21587 = DIRECTION ( 'NONE',  ( 0.7071067811865475727, 0.000000000000000000, 0.7071067811865475727 ) ) ;
#21588 = CARTESIAN_POINT ( 'NONE',  ( 10.71556987377000070, -79.69750836675898142, 2.374990294079000197 ) ) ;
#21589 = CARTESIAN_POINT ( 'NONE',  ( -1.208267226945607176, -17.17409317850119876, 12.70228502423926997 ) ) ;
#21590 = EDGE_CURVE ( 'NONE', #51311, #12545, #40926, .T. ) ;
#21591 = CARTESIAN_POINT ( 'NONE',  ( -11.42709289613000045, -75.91791632114400556, 3.432315517540000194 ) ) ;
#21592 = DIRECTION ( 'NONE',  ( 0.000000000000000000, -1.000000000000000000, 0.000000000000000000 ) ) ;
#21593 = CARTESIAN_POINT ( 'NONE',  ( 9.046072084723403961, -76.79619834608396900, 5.940455828180382980 ) ) ;
#21594 = B_SPLINE_CURVE_WITH_KNOTS ( 'NONE', 3,
 ( #31802, #32670, #849, #23255, #18833, #27955 ),
 .UNSPECIFIED., .F., .F.,
 ( 4, 1, 1, 4 ),
 ( 0.000000000000000000, 0.3333333311589000147, 0.6666666623179000606, 0.9999999934768000198 ),
 .UNSPECIFIED. ) ;
#21595 = ORIENTED_EDGE ( 'NONE', *, *, #30291, .T. ) ;
#21596 = CARTESIAN_POINT ( 'NONE',  ( -5.360806944915999850, -79.79393910884799368, -9.773246618612999370 ) ) ;
#21597 = CARTESIAN_POINT ( 'NONE',  ( 0.3859961575645005083, -79.95043709814795818, 1.188828431463626822 ) ) ;
#21598 = CARTESIAN_POINT ( 'NONE',  ( 2.879226727952094222, -77.74583333333333712, -10.71369944335146940 ) ) ;
#21599 = MECHANICAL_DESIGN_GEOMETRIC_PRESENTATION_REPRESENTATION (  '', ( #46405 ), #50873 ) ;
#21600 = CARTESIAN_POINT ( 'NONE',  ( 7.338671297540000360, -79.06094136420898622, 8.404493039061998516 ) ) ;
#21601 = CARTESIAN_POINT ( 'NONE',  ( -11.79999999999999893, -18.84999999999000053, 0.5999999999999999778 ) ) ;
#21602 = DIRECTION ( 'NONE',  ( 0.000000000000000000, 1.000000000000000000, 0.000000000000000000 ) ) ;
#21603 = CARTESIAN_POINT ( 'NONE',  ( -10.99071003982055572, -23.54576790506902029, 0.4528411669630135195 ) ) ;
#21604 = CARTESIAN_POINT ( 'NONE',  ( 10.13881649148000008, -76.90783510652001098, -5.938594122520999719 ) ) ;
#21605 = DIRECTION ( 'NONE',  ( 0.000000000000000000, -0.8191989531316462569, -0.5735094377497330642 ) ) ;
#21606 = CARTESIAN_POINT ( 'NONE',  ( -9.369164850722000892, -60.04999999966999980, 7.601397897754999633 ) ) ;
#21607 = CARTESIAN_POINT ( 'NONE',  ( -11.75000000000000000, -76.30000000000001137, 1.487410190129999909E-14 ) ) ;
#21608 = ORIENTED_EDGE ( 'NONE', *, *, #26417, .F. ) ;
#21609 = EDGE_LOOP ( 'NONE', ( #30934, #8540, #12752, #48497 ) ) ;
#21610 = CARTESIAN_POINT ( 'NONE',  ( 10.57259517296283491, -78.83558926200460348, -1.944988004412892657 ) ) ;
#21611 = AXIS2_PLACEMENT_3D ( 'NONE', #20518, #2232, #21088 ) ;
#21612 = ORIENTED_EDGE ( 'NONE', *, *, #40072, .T. ) ;
#21613 = CARTESIAN_POINT ( 'NONE',  ( -3.359581381603320871, -79.84641223401524712, -8.956518138560074505 ) ) ;
#21614 = VERTEX_POINT ( 'NONE', #55827 ) ;
#21615 = CARTESIAN_POINT ( 'NONE',  ( -10.47544694528181886, -81.00000000000000000, -2.552740764969549936 ) ) ;
#21616 = CARTESIAN_POINT ( 'NONE',  ( 8.827997450462000018, -77.87345696174899956, 6.421979991006000255 ) ) ;
#21617 = AXIS2_PLACEMENT_3D ( 'NONE', #46488, #46783, #6012 ) ;
#21619 = EDGE_CURVE ( 'NONE', #29817, #16042, #34512, .T. ) ;
#21618 = CARTESIAN_POINT ( 'NONE',  ( 8.188916213828999702, -78.92418998579800871, 5.175217742376999830 ) ) ;
#21620 = CARTESIAN_POINT ( 'NONE',  ( -6.539419588528526894, -78.16268753938295788, -6.541902902125212194 ) ) ;
#21621 = CARTESIAN_POINT ( 'NONE',  ( -1.780884232981000181, -79.87841764300529235, -11.07459082487999957 ) ) ;
#21622 = ORIENTED_EDGE ( 'NONE', *, *, #6279, .T. ) ;
#21624 = ORIENTED_EDGE ( 'NONE', *, *, #28194, .F. ) ;
#21623 = ADVANCED_FACE ( 'NONE', ( #33659 ), #11819, .T. ) ;
#21625 = CARTESIAN_POINT ( 'NONE',  ( -4.757657419345691530, -77.51803282916795013, 7.934074630878104273 ) ) ;
#21626 = DIRECTION ( 'NONE',  ( 0.000000000000000000, 1.000000000000000000, 0.000000000000000000 ) ) ;
#21627 = CARTESIAN_POINT ( 'NONE',  ( -1.199500263597274685, -77.94791666666668561, 0.9218200799623673669 ) ) ;
#21628 = CARTESIAN_POINT ( 'NONE',  ( 7.658860137760000519, -78.63277082632598081, 5.959242465009999989 ) ) ;
#21629 = CARTESIAN_POINT ( 'NONE',  ( 3.757989199629302668, -86.12610001270964233, 2.729540522067530173 ) ) ;
#21630 = CARTESIAN_POINT ( 'NONE',  ( -4.588273267446388637, -79.48450841110565079, -8.321223633674817322 ) ) ;
#21631 = CARTESIAN_POINT ( 'NONE',  ( -12.00000000000000000, -18.75000000000000000, 1.250000000000000000 ) ) ;
#21632 = CARTESIAN_POINT ( 'NONE',  ( -8.744140569415000286, -80.25535053947399433, 7.086030162020000134 ) ) ;
#21633 = CARTESIAN_POINT ( 'NONE',  ( 12.54901566180999950, -16.99264670699999868, -0.4731578885118999933 ) ) ;
#21634 = DIRECTION ( 'NONE',  ( 0.000000000000000000, 0.000000000000000000, 1.000000000000000000 ) ) ;
#21635 = ADVANCED_FACE ( 'NONE', ( #29515 ), #25096, .F. ) ;
#21636 = CARTESIAN_POINT ( 'NONE',  ( -9.009247259181922374, -78.52083333333334281, -2.421167930323344653 ) ) ;
#21637 = ORIENTED_EDGE ( 'NONE', *, *, #21880, .T. ) ;
#21638 = CARTESIAN_POINT ( 'NONE',  ( 7.547699635377999705, -79.68694304294899666, -9.585476548908999916 ) ) ;
#21639 = DIRECTION ( 'NONE',  ( 0.000000000000000000, 1.000000000000000000, 0.000000000000000000 ) ) ;
#21640 = CYLINDRICAL_SURFACE ( 'NONE', #43723, 12.90000000000000036 ) ;
#21641 = CARTESIAN_POINT ( 'NONE',  ( -10.31988039474999930, -17.71085245535000396, -7.753829094184000681 ) ) ;
#21643 = CARTESIAN_POINT ( 'NONE',  ( -2.061649843245999758, -18.79438692412999856, -12.83797346714000120 ) ) ;
#21642 = CARTESIAN_POINT ( 'NONE',  ( 7.668936932637000048, -59.57152778012000027, 10.21380041493999968 ) ) ;
#21644 = CARTESIAN_POINT ( 'NONE',  ( -9.499999999999998224, -78.81041666666666856, -1.243547092045960367 ) ) ;
#21645 = CARTESIAN_POINT ( 'NONE',  ( 10.24996238027999951, -58.55171076491000548, -7.705119999413000187 ) ) ;
#21646 = CARTESIAN_POINT ( 'NONE',  ( -1.626826133776999786E-14, -74.80000000000001137, 0.000000000000000000 ) ) ;
#21647 = CARTESIAN_POINT ( 'NONE',  ( 9.181220278661999856, -77.52425741570898765, -6.522205052974000772 ) ) ;
#21648 = CARTESIAN_POINT ( 'NONE',  ( -1.636761686205434385, -1.916666666666666741, 2.839805762151331958 ) ) ;
#21649 = CARTESIAN_POINT ( 'NONE',  ( 10.99999999999999822, -79.96041666666779690, 1.439896632895345086 ) ) ;
#21650 = ORIENTED_EDGE ( 'NONE', *, *, #44862, .T. ) ;
#21651 = DIRECTION ( 'NONE',  ( -0.9999548435846228323, 0.000000000000000000, -0.009503199022040118363 ) ) ;
#21652 = CARTESIAN_POINT ( 'NONE',  ( 1.933504092460999857, -55.39593152692000189, 12.70940235704999921 ) ) ;
#21653 = CARTESIAN_POINT ( 'NONE',  ( -12.80900240953000058, -21.75365779208000205, 1.930989144707000005 ) ) ;
#21654 = CARTESIAN_POINT ( 'NONE',  ( 1.881026021997999953, -2.552403522605000141, 3.308707285175000123 ) ) ;
#21655 = CARTESIAN_POINT ( 'NONE',  ( 4.013660496580000903, -78.35243718747800301, -10.47417304634999979 ) ) ;
#21656 = CIRCLE ( 'NONE', #27300, 12.80000000000000071 ) ;
#21657 = DIRECTION ( 'NONE',  ( 0.000000000000000000, -0.7071067811866525998, -0.7071067811864425456 ) ) ;
#21658 = CARTESIAN_POINT ( 'NONE',  ( -9.199999999999999289, -77.00000000000000000, 0.000000000000000000 ) ) ;
#21659 = CARTESIAN_POINT ( 'NONE',  ( -0.8520291216319383354, -1.997329406447212685, 3.167964011321702689 ) ) ;
#21660 = CARTESIAN_POINT ( 'NONE',  ( 9.722718241315000398, -60.04999999966999980, -7.954951288349001004 ) ) ;
#21661 = AXIS2_PLACEMENT_3D ( 'NONE', #2957, #29226, #2105 ) ;
#21662 = CARTESIAN_POINT ( 'NONE',  ( -3.978328889313999639, -86.23049735065200139, 0.4349952100312000081 ) ) ;
#21663 = DIRECTION ( 'NONE',  ( 1.000000000000000000, 0.000000000000000000, 0.000000000000000000 ) ) ;
#21664 = CARTESIAN_POINT ( 'NONE',  ( 7.287274196408028537, -76.77647172171292311, 9.625134870786519414 ) ) ;
#21665 = CARTESIAN_POINT ( 'NONE',  ( 8.145565103785999739, -77.51865691654299440, 7.609492079688000565 ) ) ;
#21666 = CARTESIAN_POINT ( 'NONE',  ( 0.6719893610791689564, -81.92997134543871596, 1.053977402048356549 ) ) ;
#21667 = CARTESIAN_POINT ( 'NONE',  ( 1.264115560106999991, -78.59429962090999311, -0.8953837640199000525 ) ) ;
#21668 = LINE ( 'NONE', #56538, #16027 ) ;
#21669 = CARTESIAN_POINT ( 'NONE',  ( -6.053394164830000257, -79.58024415034599031, -7.392643757108000813 ) ) ;
#21670 = CARTESIAN_POINT ( 'NONE',  ( 1.997276839918477265, -2.677083333333333481, -2.598917237794082791 ) ) ;
#21671 = CARTESIAN_POINT ( 'NONE',  ( -1.946241567991743304, -80.21069342602670815, -10.57240121655948606 ) ) ;
#21672 = EDGE_CURVE ( 'NONE', #57688, #57178, #56692, .T. ) ;
#21673 = CARTESIAN_POINT ( 'NONE',  ( -2.813789756862251856, -77.10416666666665719, -10.47020627418439709 ) ) ;
#21674 = CARTESIAN_POINT ( 'NONE',  ( -10.18249594443699735, -17.70907903275769613, -7.792385963400852766 ) ) ;
#21675 = ORIENTED_EDGE ( 'NONE', *, *, #6996, .F. ) ;
#21676 = CARTESIAN_POINT ( 'NONE',  ( 11.43764105185000091, -79.76670709676099591, 2.691257544168000226 ) ) ;
#21677 = CARTESIAN_POINT ( 'NONE',  ( -1.092232985442824100, -81.95833333333330017, 0.6295237254636200097 ) ) ;
#21678 = CARTESIAN_POINT ( 'NONE',  ( -4.036005110416000186, -79.22757640497698617, 10.51402051105999824 ) ) ;
#21679 = CARTESIAN_POINT ( 'NONE',  ( -7.103581178201927138, -77.53231073429024889, 8.098573607620954462 ) ) ;
#21680 = VERTEX_POINT ( 'NONE', #20386 ) ;
#21681 = AXIS2_PLACEMENT_3D ( 'NONE', #56296, #19698, #11718 ) ;
#21682 = CARTESIAN_POINT ( 'NONE',  ( 1.308715794696073020, -24.74404499195298968, 12.70256747357037419 ) ) ;
#21683 = ORIENTED_EDGE ( 'NONE', *, *, #50667, .T. ) ;
#21684 = DIRECTION ( 'NONE',  ( 0.000000000000000000, -1.000000000000000000, 0.000000000000000000 ) ) ;
#21685 = ORIENTED_EDGE ( 'NONE', *, *, #3610, .T. ) ;
#21686 = DIRECTION ( 'NONE',  ( 0.000000000000000000, -1.000000000000000000, 0.000000000000000000 ) ) ;
#21687 = CARTESIAN_POINT ( 'NONE',  ( -10.74525019809999904, -79.05928543398199793, 1.927424232126999870 ) ) ;
#21688 = CARTESIAN_POINT ( 'NONE',  ( -1.756145855908000097, -80.00523869776598929, 3.079110751715000038 ) ) ;
#21689 = CARTESIAN_POINT ( 'NONE',  ( -5.670780713235441972, -79.32583130080989520, 7.622161873721389647 ) ) ;
#21690 = VERTEX_POINT ( 'NONE', #2390 ) ;
#21691 = CARTESIAN_POINT ( 'NONE',  ( 10.36935812844000004, -78.07876026662599145, -2.835297515976000327 ) ) ;
#21692 = CARTESIAN_POINT ( 'NONE',  ( -12.04891275065999956, -78.43148691446999976, -1.977722186035000274 ) ) ;
#21694 = ORIENTED_EDGE ( 'NONE', *, *, #11702, .T. ) ;
#21693 = EDGE_CURVE ( 'NONE', #13579, #51686, #25670, .T. ) ;
#21695 = DIRECTION ( 'NONE',  ( 0.000000000000000000, 1.000000000000000000, 0.000000000000000000 ) ) ;
#21696 = CARTESIAN_POINT ( 'NONE',  ( 8.485281374238999419, -60.74999999967048581, 8.485281374238999419 ) ) ;
#21697 = B_SPLINE_CURVE_WITH_KNOTS ( 'NONE', 3,
 ( #12710, #35721, #49027, #26561, #44892, #3569 ),
 .UNSPECIFIED., .F., .F.,
 ( 4, 1, 1, 4 ),
 ( 0.000000000000000000, 0.3333333333333000081, 0.6666666666667000474, 1.000000000000000000 ),
 .UNSPECIFIED. ) ;
#21698 = CARTESIAN_POINT ( 'NONE',  ( -1.319155384867000125, -80.21015088913199520, 0.1959724986398999891 ) ) ;
#21699 = AXIS2_PLACEMENT_3D ( 'NONE', #27993, #54594, #50170 ) ;
#21700 = CARTESIAN_POINT ( 'NONE',  ( -9.312149464823921363, -77.13785053516166101, -0.06563382585331917207 ) ) ;
#21701 = VECTOR ( 'NONE', #14560, 1000.000000000000000 ) ;
#21702 = CARTESIAN_POINT ( 'NONE',  ( -3.488504142081042314, -86.36264283715695456, 1.632650329933101885 ) ) ;
#21703 = CARTESIAN_POINT ( 'NONE',  ( 3.281627333226164289, -85.82424546584941538, 1.435836378473854591 ) ) ;
#21704 = CARTESIAN_POINT ( 'NONE',  ( -10.63665183518000035, -77.95590642111000079, 7.669898027128999374 ) ) ;
#21705 = CARTESIAN_POINT ( 'NONE',  ( 12.30436613475999863, -78.05926792646000933, -3.523071432600000108 ) ) ;
#21706 = CARTESIAN_POINT ( 'NONE',  ( -10.56721085596999998, -77.01377769904699733, 1.716300984214999881 ) ) ;
#21707 = ADVANCED_FACE ( 'NONE', ( #7956 ), #53548, .T. ) ;
#21708 = CARTESIAN_POINT ( 'NONE',  ( -8.719367347793284040, -78.62710504220744667, -3.087874295618068476 ) ) ;
#21709 = CARTESIAN_POINT ( 'NONE',  ( 0.6588992274324999565, -82.30157348994899280, -4.077290543664999767 ) ) ;
#21710 = CARTESIAN_POINT ( 'NONE',  ( 12.56594317989000054, -23.24999999414999863, 1.750000000001000089 ) ) ;
#21711 = CARTESIAN_POINT ( 'NONE',  ( -0.1776184920840612746, -2.979648444064375123, 3.245463997345638063 ) ) ;
#21712 = CARTESIAN_POINT ( 'NONE',  ( -1.756256933393999908, -79.89225264934799497, 3.079046179090000113 ) ) ;
#21713 = CARTESIAN_POINT ( 'NONE',  ( -9.469606800734000629, -79.65752053325199711, 5.597012331546999953 ) ) ;
#21714 = CARTESIAN_POINT ( 'NONE',  ( -1.429395846838289241, -80.98573564870306996, 10.65686433594883198 ) ) ;
#21715 = LINE ( 'NONE', #13139, #22183 ) ;
#21716 = CARTESIAN_POINT ( 'NONE',  ( -0.3113020967593000399, -2.664182682366000421, 3.793306396812999637 ) ) ;
#21717 = CARTESIAN_POINT ( 'NONE',  ( 10.75503897980323309, -77.20000000000001705, -0.4084248854891507352 ) ) ;
#21718 = ORIENTED_EDGE ( 'NONE', *, *, #45175, .F. ) ;
#21719 = CARTESIAN_POINT ( 'NONE',  ( -7.619712170668999640, -60.20404510030000012, -10.35409959312000083 ) ) ;
#21720 = CARTESIAN_POINT ( 'NONE',  ( -3.250000000000000000, -1.000000000000000000, 1.223542571470000149E-13 ) ) ;
#21721 = CARTESIAN_POINT ( 'NONE',  ( -1.234140985588999984, -81.19095428981999873, 0.5054425604136000283 ) ) ;
#21722 = CIRCLE ( 'NONE', #13241, 9.599999999999999645 ) ;
#21723 = CARTESIAN_POINT ( 'NONE',  ( -12.66314509270999977, -16.82135249322999826, 0.04032083120557000688 ) ) ;
#21724 = CARTESIAN_POINT ( 'NONE',  ( 0.000000000000000000, -18.75000000000000000, -12.50000000000000000 ) ) ;
#21725 = CARTESIAN_POINT ( 'NONE',  ( 1.001315002179000047, -24.68522411714000242, -12.50000000000000000 ) ) ;
#21726 = CARTESIAN_POINT ( 'NONE',  ( -6.753896588641000065, -75.57222202327999128, -10.03086863324999989 ) ) ;
#21727 = ORIENTED_EDGE ( 'NONE', *, *, #9620, .T. ) ;
#21728 = CARTESIAN_POINT ( 'NONE',  ( 0.000000000000000000, -74.64999999999999147, 0.000000000000000000 ) ) ;
#21729 = CARTESIAN_POINT ( 'NONE',  ( 12.82230166705999963, -60.22260937973999972, 2.065916748305000272 ) ) ;
#21730 = CARTESIAN_POINT ( 'NONE',  ( 7.653559502277999194, -18.70150862776000267, -10.01234990228999955 ) ) ;
#21731 = CIRCLE ( 'NONE', #16234, 0.5000000000000004441 ) ;
#21732 = CARTESIAN_POINT ( 'NONE',  ( 7.201320854070999644, -77.70084747358500010, 6.394856364399000626 ) ) ;
#21733 = CARTESIAN_POINT ( 'NONE',  ( 0.2050755927455000238, -85.82581675399998744, 4.167486983637000542 ) ) ;
#21734 = CARTESIAN_POINT ( 'NONE',  ( -1.552587846661832138, -79.98697443929660267, 10.63702038836880881 ) ) ;
#21735 = CARTESIAN_POINT ( 'NONE',  ( -1.499766830043999910, -80.03557803647899505, 0.2228039671692000068 ) ) ;
#21736 = VERTEX_POINT ( 'NONE', #52770 ) ;
#21737 = ADVANCED_FACE ( 'NONE', ( #57770 ), #44785, .F. ) ;
#21738 = DIRECTION ( 'NONE',  ( 3.342393029126999711E-11, -1.000000000000000000, 3.127660138207999783E-09 ) ) ;
#21739 = CARTESIAN_POINT ( 'NONE',  ( 11.00000000000000000, -78.94999999999998863, -1.064824513673000067E-14 ) ) ;
#21740 = VECTOR ( 'NONE', #27666, 1000.000000000000114 ) ;
#21741 = CARTESIAN_POINT ( 'NONE',  ( -3.437187628289029018, -78.85171435493609238, 6.874375256578015403 ) ) ;
#21742 = ORIENTED_EDGE ( 'NONE', *, *, #38273, .T. ) ;
#21743 = EDGE_CURVE ( 'NONE', #19957, #57178, #7261, .T. ) ;
#21744 = ORIENTED_EDGE ( 'NONE', *, *, #50835, .T. ) ;
#21745 = CARTESIAN_POINT ( 'NONE',  ( 10.82226978776999893, -79.13250813710999410, 1.601965348215999896 ) ) ;
#21746 = DIRECTION ( 'NONE',  ( 0.000000000000000000, 1.000000000000000000, 0.000000000000000000 ) ) ;
#21747 = CARTESIAN_POINT ( 'NONE',  ( -10.67332088312999971, -80.27238938826599224, -4.121781213195999882 ) ) ;
#21748 = ORIENTED_EDGE ( 'NONE', *, *, #33712, .T. ) ;
#21749 = EDGE_LOOP ( 'NONE', ( #13450, #56131, #33950, #27774 ) ) ;
#21750 = ORIENTED_EDGE ( 'NONE', *, *, #54901, .T. ) ;
#21751 = CARTESIAN_POINT ( 'NONE',  ( 1.537484947575329830, -78.06258978500997614, 11.74336395611926243 ) ) ;
#21752 = CARTESIAN_POINT ( 'NONE',  ( 0.000000000000000000, -77.69999999999998863, 0.000000000000000000 ) ) ;
#21753 = VERTEX_POINT ( 'NONE', #13181 ) ;
#21754 = CARTESIAN_POINT ( 'NONE',  ( -8.022734517049746273E-06, -82.01564364893640402, -1.484164386985079798 ) ) ;
#21756 = EDGE_CURVE ( 'NONE', #42409, #27527, #44484, .T. ) ;
#21755 = ORIENTED_EDGE ( 'NONE', *, *, #37094, .T. ) ;
#21757 = CARTESIAN_POINT ( 'NONE',  ( -1.193476013507506650, -79.62178374976105033, 0.4454124431937202533 ) ) ;
#21758 = CARTESIAN_POINT ( 'NONE',  ( -3.819913647775994292, -78.99318692756679638, -2.158384532486305574 ) ) ;
#21759 = CARTESIAN_POINT ( 'NONE',  ( 7.645398650953000086, -55.58468617124000133, 10.18948982067999864 ) ) ;
#21760 = CARTESIAN_POINT ( 'NONE',  ( -7.691893942719999266, -21.75453807238000081, -10.42272502862000039 ) ) ;
#21761 = DIRECTION ( 'NONE',  ( 0.000000000000000000, -1.000000000000000000, 0.000000000000000000 ) ) ;
#21762 = DIRECTION ( 'NONE',  ( 0.000000000000000000, 1.000000000000000000, 0.000000000000000000 ) ) ;
#21763 = CARTESIAN_POINT ( 'NONE',  ( 7.654537165486999584, -60.08056535122999975, -10.01332852690999964 ) ) ;
#21764 = EDGE_CURVE ( 'NONE', #35060, #47903, #57736, .T. ) ;
#21765 = CARTESIAN_POINT ( 'NONE',  ( -10.18499221075000172, -21.74977139925000102, -7.710118476595999581 ) ) ;
#21766 = DIRECTION ( 'NONE',  ( 0.000000000000000000, 1.000000000000000000, 0.000000000000000000 ) ) ;
#21767 = VECTOR ( 'NONE', #28069, 1000.000000000000000 ) ;
#21768 = EDGE_CURVE ( 'NONE', #18144, #48697, #48924, .T. ) ;
#21769 = CARTESIAN_POINT ( 'NONE',  ( 1.621859418500000150, -80.61375264934798679, -3.846969171540000065 ) ) ;
#21770 = CIRCLE ( 'NONE', #6750, 1.000000000000000000 ) ;
#21771 = CARTESIAN_POINT ( 'NONE',  ( -9.021895076917001433, -77.22568667140099308, 3.730351835827999896 ) ) ;
#21772 = CARTESIAN_POINT ( 'NONE',  ( 1.250000000000000000, -83.24999999999998579, 0.000000000000000000 ) ) ;
#21773 = CARTESIAN_POINT ( 'NONE',  ( 10.45204383622999877, -22.76256649475000060, -7.651147548059999970 ) ) ;
#21774 = CARTESIAN_POINT ( 'NONE',  ( -0.6669403506045999963, -76.11899345326600042, -12.26286337364000012 ) ) ;
#21775 = CARTESIAN_POINT ( 'NONE',  ( 0.5437984056370208652, -79.97105364439701702, 11.05137384886682916 ) ) ;
#21776 = CARTESIAN_POINT ( 'NONE',  ( -3.420836093188877935, -78.44788026401511161, 11.58194243861089134 ) ) ;
#21777 = CARTESIAN_POINT ( 'NONE',  ( -0.1636246173744726473, -80.88541666666665719, 1.249999999999999112 ) ) ;
#21778 = CARTESIAN_POINT ( 'NONE',  ( -1.417852237051780540, -79.87761815572260105, -0.5262009856692363430 ) ) ;
#21779 = CARTESIAN_POINT ( 'NONE',  ( 8.827998080066999265, -77.24332679464099272, -3.176622877762000030 ) ) ;
#21780 = CARTESIAN_POINT ( 'NONE',  ( -1.308462286196999891, -79.31053370013900405, 0.7661340681064999769 ) ) ;
#21781 = LINE ( 'NONE', #22069, #50261 ) ;
#21782 = CARTESIAN_POINT ( 'NONE',  ( -9.053955183288000086, -77.07376637690499876, -6.099285168125999412 ) ) ;
#21783 = CARTESIAN_POINT ( 'NONE',  ( -10.88187945745999841, -78.41175121120100755, -5.690384754473000406 ) ) ;
#21784 = DIRECTION ( 'NONE',  ( -1.000000000000000000, 0.000000000000000000, -2.582636882130999866E-11 ) ) ;
#21785 = EDGE_CURVE ( 'NONE', #15969, #13888, #43919, .T. ) ;
#21787 = CARTESIAN_POINT ( 'NONE',  ( -7.970415440364950754, -17.47707676838395230, 9.713035532436663289 ) ) ;
#21786 = DIRECTION ( 'NONE',  ( 0.000000000000000000, -1.000000000000000000, 0.000000000000000000 ) ) ;
#21788 = CARTESIAN_POINT ( 'NONE',  ( -0.6004489902433000070, -82.23482063826000399, -1.340115349862999850 ) ) ;
#21789 = CARTESIAN_POINT ( 'NONE',  ( -5.015684137145860255, -79.51374401593871255, 9.508478352445903781 ) ) ;
#21790 = ORIENTED_EDGE ( 'NONE', *, *, #57492, .T. ) ;
#21791 = CARTESIAN_POINT ( 'NONE',  ( -10.04115011120000034, -19.23513569609999863, -7.682331425195999763 ) ) ;
#21792 = CARTESIAN_POINT ( 'NONE',  ( 5.072393583102999592, -79.09961090260800631, 11.04742415471000072 ) ) ;
#21793 = CARTESIAN_POINT ( 'NONE',  ( 6.689487621035000053, -80.75012225428049817, -8.802461778990000596 ) ) ;
#21794 = AXIS2_PLACEMENT_3D ( 'NONE', #45302, #35532, #26969 ) ;
#21795 = CARTESIAN_POINT ( 'NONE',  ( 9.736961952457013680, -79.69999999999997442, 7.076710841379813210 ) ) ;
#21796 = CARTESIAN_POINT ( 'NONE',  ( -9.966224254750001066, -60.46904904752999954, 7.657729124028000101 ) ) ;
#21797 = CARTESIAN_POINT ( 'NONE',  ( -3.195973530103000115, -0.6111989345079000824, 0.8317538331999000389 ) ) ;
#21798 = CARTESIAN_POINT ( 'NONE',  ( 7.637074688270999445, -78.94561555618199122, 5.932176574774000066 ) ) ;
#21799 = CARTESIAN_POINT ( 'NONE',  ( 12.83675988120999989, -23.22754371161000009, -2.062832873794000044 ) ) ;
#21800 = CARTESIAN_POINT ( 'NONE',  ( -1.667936688463999895, -59.56486430393999854, 12.53239398061000109 ) ) ;
#21801 = ORIENTED_EDGE ( 'NONE', *, *, #56263, .F. ) ;
#21802 = B_SPLINE_CURVE_WITH_KNOTS ( 'NONE', 3,
 ( #48795, #26338, #44356, #3910, #21912, #39921, #28378, #5659, #10105, #1262, #14516, #33097, #27505, #36954, #49975, #23383, #18379, #32508 ),
 .UNSPECIFIED., .F., .F.,
 ( 4, 2, 2, 2, 2, 2, 2, 2, 4 ),
 ( 0.000000000000000000, 0.1249999999999999722, 0.2500000000000000000, 0.3750000000000000000, 0.5000000000000001110, 0.6250000000000001110, 0.7500000000000000000, 0.8750000000000000000, 1.000000000000000000 ),
 .UNSPECIFIED. ) ;
#21803 = EDGE_CURVE ( 'NONE', #30548, #2165, #21471, .T. ) ;
#21804 = CYLINDRICAL_SURFACE ( 'NONE', #54088, 1.750000000000001332 ) ;
#21805 = CARTESIAN_POINT ( 'NONE',  ( 9.298485322488877713, -24.88812323703113805, -8.385852789304612642 ) ) ;
#21806 = CARTESIAN_POINT ( 'NONE',  ( -12.52785477537235082, -18.20586572947692972, 1.668513103013892884 ) ) ;
#21807 = EDGE_CURVE ( 'NONE', #19884, #17378, #58065, .T. ) ;
#21808 = CARTESIAN_POINT ( 'NONE',  ( -10.35747145890000098, -55.48415267986000288, -7.626500777218999438 ) ) ;
#21809 = CARTESIAN_POINT ( 'NONE',  ( 3.124641504234999534, -85.31342953870898782, -1.679633349223000005 ) ) ;
#21810 = VERTEX_POINT ( 'NONE', #5792 ) ;
#21811 = DIRECTION ( 'NONE',  ( -1.000000000000000000, 0.000000000000000000, 0.000000000000000000 ) ) ;
#21812 = AXIS2_PLACEMENT_3D ( 'NONE', #52568, #42267, #38979 ) ;
#21813 = CARTESIAN_POINT ( 'NONE',  ( 11.79999999999999893, -18.84999999999000053, -0.5999999999999999778 ) ) ;
#21814 = DIRECTION ( 'NONE',  ( 1.000000000000000000, 3.441642669434999888E-11, 0.000000000000000000 ) ) ;
#21815 = ORIENTED_EDGE ( 'NONE', *, *, #29875, .F. ) ;
#21816 = AXIS2_PLACEMENT_3D ( 'NONE', #29296, #47345, #48209 ) ;
#21817 = CARTESIAN_POINT ( 'NONE',  ( 1.668607604520048415, -55.00618368707859673, 12.52787843847549887 ) ) ;
#21818 = CARTESIAN_POINT ( 'NONE',  ( -10.15833271780000047, -54.58011549179999378, -7.756208840337999177 ) ) ;
#21819 = CARTESIAN_POINT ( 'NONE',  ( 9.226480760116999136, -79.00070664722298375, -2.263195259622999611 ) ) ;
#21820 = VERTEX_POINT ( 'NONE', #5499 ) ;
#21821 = ORIENTED_EDGE ( 'NONE', *, *, #12057, .T. ) ;
#21822 = CARTESIAN_POINT ( 'NONE',  ( 8.182584713298000523, -77.00851930215799257, 9.253818538989998288 ) ) ;
#21823 = CARTESIAN_POINT ( 'NONE',  ( -10.45676550743384858, -78.61867176466869012, -2.493575623787820827 ) ) ;
#21824 = EDGE_LOOP ( 'NONE', ( #13469, #13992, #674 ) ) ;
#21825 = CARTESIAN_POINT ( 'NONE',  ( 10.19022281666000040, -18.80366258888000175, 7.646946378508999942 ) ) ;
#21826 = CARTESIAN_POINT ( 'NONE',  ( -5.159130208082606472, -77.43030033517193544, -8.219319990131634057 ) ) ;
#21827 = CARTESIAN_POINT ( 'NONE',  ( 0.5801429252975863760, -80.26374239380967879, -1.107237889240993534 ) ) ;
#21828 = CARTESIAN_POINT ( 'NONE',  ( -12.92190527446000026, -78.08724936260999527, -0.9418163832602000074 ) ) ;
#21829 = CARTESIAN_POINT ( 'NONE',  ( -9.457500717944000712, -78.29517502955388863, -6.031068363571000290 ) ) ;
#21830 = CARTESIAN_POINT ( 'NONE',  ( -0.4924802140953842278, -86.25171435493598437, 3.960641768741265611 ) ) ;
#21831 = CARTESIAN_POINT ( 'NONE',  ( 10.12058791103999944, -79.68715863353600071, 4.836508133599999759 ) ) ;
#21832 = CARTESIAN_POINT ( 'NONE',  ( 3.393132750703385270, -79.94520027180968214, 8.605390363453048863 ) ) ;
#21833 = CARTESIAN_POINT ( 'NONE',  ( 0.000000000000000000, -1.355252715606880543E-17, -3.800000000000270717 ) ) ;
#21834 =( GEOMETRIC_REPRESENTATION_CONTEXT ( 3 ) GLOBAL_UNCERTAINTY_ASSIGNED_CONTEXT ( ( #33682 ) ) GLOBAL_UNIT_ASSIGNED_CONTEXT ( ( #11401, #38245, #47428 ) ) REPRESENTATION_CONTEXT ( 'NONE', 'WORKASPACE' ) );
#21835 = ORIENTED_EDGE ( 'NONE', *, *, #25244, .F. ) ;
#21836 = CARTESIAN_POINT ( 'NONE',  ( 10.24618685648000138, -78.90493811345498898, 4.684505231889000143 ) ) ;
#21837 = CARTESIAN_POINT ( 'NONE',  ( -2.699182493562976681, -77.20154682869322471, -8.848940700691480643 ) ) ;
#21838 = CARTESIAN_POINT ( 'NONE',  ( -0.2315393795184000070, -80.13098110198900770, 1.298828366650000010 ) ) ;
#21839 = CARTESIAN_POINT ( 'NONE',  ( 1.750000000001000089, -60.04999998641999781, -12.56594318054000148 ) ) ;
#21840 = CARTESIAN_POINT ( 'NONE',  ( 1.317981885658178198, -3.004763700841414753, -3.265141604934490793 ) ) ;
#21841 = CARTESIAN_POINT ( 'NONE',  ( -1.112867702664867675, -80.60286633726140337, -0.8764124957829881879 ) ) ;
#21842 = DIRECTION ( 'NONE',  ( -1.894056205636980548E-11, 1.538484108169980264E-07, 0.9999999999999882316 ) ) ;
#21843 = CARTESIAN_POINT ( 'NONE',  ( -10.75000000000000000, -80.44999999999998863, 5.225043809877999334E-10 ) ) ;
#21844 = CARTESIAN_POINT ( 'NONE',  ( 8.456503675551001464, -78.36349234901598493, 7.278678959607000287 ) ) ;
#21845 = CARTESIAN_POINT ( 'NONE',  ( -7.529844411733000342, -77.43398998579799297, -6.173647680939999383 ) ) ;
#21846 = CARTESIAN_POINT ( 'NONE',  ( 10.53101990620000095, -23.30639784948999704, -7.613962745608000127 ) ) ;
#21847 = CARTESIAN_POINT ( 'NONE',  ( -5.413904038987160661, -79.58333333333330017, -9.393203674808278336 ) ) ;
#21848 = CARTESIAN_POINT ( 'NONE',  ( -11.20683111097000051, -79.75336693180456393, -0.4743912329535999728 ) ) ;
#21849 = ORIENTED_EDGE ( 'NONE', *, *, #11702, .F. ) ;
#21850 = CARTESIAN_POINT ( 'NONE',  ( -1.339567984323000172, -82.99025183280099327, -0.6016691479808000675 ) ) ;
#21851 = CARTESIAN_POINT ( 'NONE',  ( 1.258195058187999926, -81.29968570196999167, 0.4928692076250000276 ) ) ;
#21852 = DIRECTION ( 'NONE',  ( 0.000000000000000000, 1.000000000000000000, 0.000000000000000000 ) ) ;
#21853 = AXIS2_PLACEMENT_3D ( 'NONE', #9594, #32875, #42350 ) ;
#21854 = DIRECTION ( 'NONE',  ( 0.2425356250363094601, 0.9701425001453377606, 4.828652960331188457E-10 ) ) ;
#21855 = CARTESIAN_POINT ( 'NONE',  ( -9.397813699260852971, -80.00762368868254271, 5.554579860211124931 ) ) ;
#21856 = CARTESIAN_POINT ( 'NONE',  ( -1.510823314100999903, -83.22898965179099662, -0.3534059060544000319 ) ) ;
#21857 = CARTESIAN_POINT ( 'NONE',  ( -5.666254562607999645, -77.99095814969300022, 10.50376416711000083 ) ) ;
#21858 = CARTESIAN_POINT ( 'NONE',  ( 4.495978696100999983, -78.02690584965399978, 8.621246072682998474 ) ) ;
#21859 = CARTESIAN_POINT ( 'NONE',  ( -4.441436338936000539, -78.79379552517198704, -8.545575054271999704 ) ) ;
#21861 = EDGE_CURVE ( 'NONE', #52710, #37361, #40945, .T. ) ;
#21860 = CARTESIAN_POINT ( 'NONE',  ( -0.5154756746322000094, -53.66759400203999775, -12.66205448068000017 ) ) ;
#21862 = B_SPLINE_CURVE_WITH_KNOTS ( 'NONE', 3,
 ( #46858, #51571, #11128, #1984, #19979, #6386, #37966, #24690, #47151, #16413, #44148, #29677, #25837, #43567, #26128, #7262, #2836, #12552, #48015, #12834, #52715, #57429, #45242, #7550, #25262, #16990, #34970, #31631 ),
 .UNSPECIFIED., .F., .F.,
 ( 4, 2, 1, 2, 2, 1, 2, 2, 2, 2, 2, 2, 2, 2, 4 ),
 ( 0.000000000000000000, 0.1249999999999998612, 0.1874999999999997502, 0.2187499999999996669, 0.2499999999999996114, 0.3124999999999996114, 0.3437499999999996114, 0.3749999999999995559, 0.4999999999999996669, 0.5624999999999996669, 0.6249999999999997780, 0.6874999999999997780, 0.7499999999999997780, 0.8749999999999998890, 1.000000000000000000 ),
 .UNSPECIFIED. ) ;
#21863 = CARTESIAN_POINT ( 'NONE',  ( 9.772926403074635004, -75.99679253653761180, 6.523134133395031675 ) ) ;
#21864 = CARTESIAN_POINT ( 'NONE',  ( 3.654181830570652156, -86.07389998728979208, -1.626946572303435534 ) ) ;
#21865 = ORIENTED_EDGE ( 'NONE', *, *, #5001, .T. ) ;
#21866 = CARTESIAN_POINT ( 'NONE',  ( 9.009247259181915268, -78.77083333333334281, 2.421167930323361972 ) ) ;
#21867 = CARTESIAN_POINT ( 'NONE',  ( -1.310679582531389276, -79.35833333333332007, 0.7554284705563443225 ) ) ;
#21868 = EDGE_CURVE ( 'NONE', #48419, #36474, #53566, .T. ) ;
#21869 = CARTESIAN_POINT ( 'NONE',  ( 8.485281374238999419, -55.54999999966999980, 8.485281374238999419 ) ) ;
#21870 = CARTESIAN_POINT ( 'NONE',  ( 1.431241028886999889, -81.47764180916999521, -0.8524881072380000591 ) ) ;
#21871 = CARTESIAN_POINT ( 'NONE',  ( 9.632126701410999914, -79.21993834310299576, 5.261763182588000021 ) ) ;
#21872 = CARTESIAN_POINT ( 'NONE',  ( 6.673790874065899104, -80.33932291666529579, 8.685525953824821954 ) ) ;
#21873 = CARTESIAN_POINT ( 'NONE',  ( -5.277198993124000204, -76.03111453605899328, -11.20659448217999987 ) ) ;
#21874 = CARTESIAN_POINT ( 'NONE',  ( -9.469606800734000629, -79.65752053325199711, 5.597012331546999953 ) ) ;
#21875 = CARTESIAN_POINT ( 'NONE',  ( 0.5928849308894093006, -77.96093750004841638, 1.162612760383189947 ) ) ;
#21876 = VERTEX_POINT ( 'NONE', #6084 ) ;
#21877 = CARTESIAN_POINT ( 'NONE',  ( 8.767647372505999570, -80.01182985286258997, 6.883540450345000394 ) ) ;
#21878 = CARTESIAN_POINT ( 'NONE',  ( 1.150057798432680745, -79.88230094492989508, 0.4893180354286167377 ) ) ;
#21879 = CARTESIAN_POINT ( 'NONE',  ( 10.71369944335147473, -77.82916666666666572, -2.879226727952063580 ) ) ;
#21880 = EDGE_CURVE ( 'NONE', #4894, #35836, #50976, .T. ) ;
#21881 = CARTESIAN_POINT ( 'NONE',  ( 9.386754667005000385, -79.53851138786500030, 6.031619700400000283 ) ) ;
#21882 = CARTESIAN_POINT ( 'NONE',  ( 0.000000000000000000, -76.14999999999999147, -10.90000000000000036 ) ) ;
#21883 = DIRECTION ( 'NONE',  ( 0.000000000000000000, 1.000000000000000000, 0.000000000000000000 ) ) ;
#21884 = CARTESIAN_POINT ( 'NONE',  ( 8.480197680338001476, -78.51225130393000029, -8.881555409017000358 ) ) ;
#21885 = EDGE_CURVE ( 'NONE', #20606, #47713, #5357, .T. ) ;
#21886 = CARTESIAN_POINT ( 'NONE',  ( -1.423904377723695935, -61.10512805135450520, 12.50677628660337248 ) ) ;
#21887 = CARTESIAN_POINT ( 'NONE',  ( 5.413904038987143785, -78.33333333333332860, 9.393203674808290771 ) ) ;
#21888 = EDGE_CURVE ( 'NONE', #33386, #20388, #25168, .T. ) ;
#21889 = DIRECTION ( 'NONE',  ( 0.000000000000000000, -1.000000000000000000, 0.000000000000000000 ) ) ;
#21890 = EDGE_LOOP ( 'NONE', ( #4407, #10513, #38400, #22188, #46992 ) ) ;
#21891 = VERTEX_POINT ( 'NONE', #23509 ) ;
#21892 = CARTESIAN_POINT ( 'NONE',  ( 10.59031137979719084, -78.83631738623206786, -1.847091933338027125 ) ) ;
#21893 = AXIS2_PLACEMENT_3D ( 'NONE', #7053, #11206, #11776 ) ;
#21894 = ORIENTED_EDGE ( 'NONE', *, *, #36182, .T. ) ;
#21895 = CARTESIAN_POINT ( 'NONE',  ( 2.624826629463999694, -78.90983510652000632, 11.97953966613999910 ) ) ;
#21896 = ORIENTED_EDGE ( 'NONE', *, *, #28267, .T. ) ;
#21897 = CARTESIAN_POINT ( 'NONE',  ( 9.414507962619001802, -25.26263135926000203, 8.652357372777000677 ) ) ;
#21898 = CARTESIAN_POINT ( 'NONE',  ( 2.807878695492000087, -77.99565671216601004, 10.66853090226000056 ) ) ;
#21899 = CARTESIAN_POINT ( 'NONE',  ( -9.595602112029999020, -78.14028998579800600, -1.328770664336999863 ) ) ;
#21900 = CARTESIAN_POINT ( 'NONE',  ( -6.395610860418600829, -78.16440346101558134, -6.682817714148057142 ) ) ;
#21901 = AXIS2_PLACEMENT_3D ( 'NONE', #2413, #30405, #7982 ) ;
#21902 = CARTESIAN_POINT ( 'NONE',  ( -11.04065564778000130, -79.18419320068699108, 1.980412446595999798 ) ) ;
#21903 = CARTESIAN_POINT ( 'NONE',  ( -0.3229108565016139409, -79.49587948166266926, 1.210510340675584162 ) ) ;
#21904 = VERTEX_POINT ( 'NONE', #36504 ) ;
#21905 = VERTEX_POINT ( 'NONE', #1105 ) ;
#21906 = CARTESIAN_POINT ( 'NONE',  ( -0.2651902714627518143, -77.47745245132422554, 9.246255095149187753 ) ) ;
#21907 = CARTESIAN_POINT ( 'NONE',  ( 2.604371601988999974, -77.45349661881098768, -10.72853197743999942 ) ) ;
#21908 = CARTESIAN_POINT ( 'NONE',  ( -9.500000000000000000, -77.39999999999999147, 0.000000000000000000 ) ) ;
#21909 = CARTESIAN_POINT ( 'NONE',  ( -5.351292223237999579, -77.81193504899798086, 8.095330809056001442 ) ) ;
#21910 = VECTOR ( 'NONE', #29509, 1000.000000000000000 ) ;
#21911 = CARTESIAN_POINT ( 'NONE',  ( -2.203951651292999969, -75.80714300465999145, 12.77594201493999826 ) ) ;
#21912 = CARTESIAN_POINT ( 'NONE',  ( 2.663461512100961048, -2.200631673208123917, -1.905539629302623217 ) ) ;
#21913 = CARTESIAN_POINT ( 'NONE',  ( 8.610991514451539430, -53.62512235746365263, -9.355860133842407222 ) ) ;
#21914 = CARTESIAN_POINT ( 'NONE',  ( -9.459258931978000717, -79.82843986952799753, 5.442530770145999952 ) ) ;
#21915 = VECTOR ( 'NONE', #42008, 1000.000000000000000 ) ;
#21916 = CARTESIAN_POINT ( 'NONE',  ( 12.77562786370999959, -16.73761952138000098, -0.5426593252874999385 ) ) ;
#21917 = CARTESIAN_POINT ( 'NONE',  ( -9.516272955293000990, -24.82538765621999843, -8.227498559427999680 ) ) ;
#21918 = CARTESIAN_POINT ( 'NONE',  ( -11.73895145468623724, -76.69513831007681404, 0.6305574448010526911 ) ) ;
#21919 = EDGE_LOOP ( 'NONE', ( #13043, #7034, #1223, #1673 ) ) ;
#21920 = CARTESIAN_POINT ( 'NONE',  ( -7.458578474212999687, -79.44721302158100684, -9.947846520260998915 ) ) ;
#21921 = CARTESIAN_POINT ( 'NONE',  ( -7.943801774140000660, -54.36598212437999678, 9.641153612765998915 ) ) ;
#21922 = CARTESIAN_POINT ( 'NONE',  ( 11.70594025892000012, -78.46873148349699534, 2.546964289010999583 ) ) ;
#21923 = CARTESIAN_POINT ( 'NONE',  ( -7.758899961888999997, -17.69918178096000005, -10.31442855573999928 ) ) ;
#21925 = DIRECTION ( 'NONE',  ( 0.000000000000000000, 1.000000000000000000, 0.000000000000000000 ) ) ;
#21924 = CARTESIAN_POINT ( 'NONE',  ( -2.420948490244752449, -78.49585695048426714, 9.008675488125174269 ) ) ;
#21926 = CARTESIAN_POINT ( 'NONE',  ( 3.576074390006000137, -86.31452044229999387, -1.592170899227999925 ) ) ;
#21927 = CARTESIAN_POINT ( 'NONE',  ( 10.21380041493999968, -59.57152778012000027, -7.668936932637000048 ) ) ;
#21928 = CARTESIAN_POINT ( 'NONE',  ( -0.6878299077642000547, -82.24743426901200394, -1.043738481606000024 ) ) ;
#21929 = CARTESIAN_POINT ( 'NONE',  ( 1.639991984446999895, -77.96003890373799550, -11.14201017990999887 ) ) ;
#21930 = CARTESIAN_POINT ( 'NONE',  ( -12.00000000000000355, -78.28958333333331154, 1.570796326794848596 ) ) ;
#21931 = CARTESIAN_POINT ( 'NONE',  ( -10.99999999999000089, -80.20000000002698926, -2.639066790267999940E-09 ) ) ;
#21932 = EDGE_LOOP ( 'NONE', ( #41224, #42831, #39045, #15813, #40746, #57038, #5569 ) ) ;
#21933 = CARTESIAN_POINT ( 'NONE',  ( 1.638701331945049633, -1.434920423400078304, 2.842861795934006786 ) ) ;
#21934 = CARTESIAN_POINT ( 'NONE',  ( -1.691611010928999903, -54.56917308736999672, 12.66722148965999928 ) ) ;
#21935 = DIRECTION ( 'NONE',  ( 0.000000000000000000, -1.000000000000000000, 0.000000000000000000 ) ) ;
#21936 = CARTESIAN_POINT ( 'NONE',  ( -2.342185844934999928, -3.569198934507999965, 2.328138035414999862 ) ) ;
#21937 = CARTESIAN_POINT ( 'NONE',  ( -0.08960567475284000882, -79.89657020290799494, 9.424340550334999733 ) ) ;
#21938 = VECTOR ( 'NONE', #28827, 1000.000000000000114 ) ;
#21939 = FACE_OUTER_BOUND ( 'NONE', #40280, .T. ) ;
#21940 = CARTESIAN_POINT ( 'NONE',  ( 5.399973277016593798, -77.19999999999998863, 9.364213316283096944 ) ) ;
#21941 = DIRECTION ( 'NONE',  ( 0.000000000000000000, 0.000000000000000000, -1.000000000000000000 ) ) ;
#21942 = CARTESIAN_POINT ( 'NONE',  ( 12.49989298250000047, -18.80773379996000116, 1.666426105558000081 ) ) ;
#21943 = CARTESIAN_POINT ( 'NONE',  ( 0.2031981210172000007, -86.00157450217399457, 4.125184445905999198 ) ) ;
#21944 = DIRECTION ( 'NONE',  ( 0.000000000000000000, 0.000000000000000000, -1.000000000000000000 ) ) ;
#21945 = EDGE_CURVE ( 'NONE', #24388, #21041, #54233, .T. ) ;
#21946 = CARTESIAN_POINT ( 'NONE',  ( 11.03313870319343160, -76.66973052364008367, -4.907352434147976616 ) ) ;
#21947 = B_SPLINE_SURFACE_WITH_KNOTS ( 'NONE', 3, 3, ( 
 ( #14686, #1726, #50737, #33275 ),
 ( #14981, #19719, #21447, #47480 ),
 ( #12018, #38586, #16736, #47760 ),
 ( #56892, #43899, #25008, #56601 ),
 ( #34430, #52460, #38872, #29999 ),
 ( #39737, #39456, #16161, #57460 ),
 ( #34718, #11734, #39161, #57747 ),
 ( #57170, #3165, #48053, #3443 ),
 ( #21729, #44182, #52748, #11449 ),
 ( #21155, #29712, #51891, #12302 ),
 ( #30292, #34139, #35005, #25872 ) ),
 .UNSPECIFIED., .F., .F., .F.,
 ( 4, 1, 1, 1, 1, 1, 1, 1, 4 ),
 ( 4, 4 ),
 ( -0.01994534136800000038, 0.000000000000000000, 0.1666666666667000196, 0.3333333333333000081, 0.5000000000000000000, 0.6666666666667000474, 0.8333333333333000637, 1.000000000000000000, 1.020519780480000138 ),
 ( -0.3582002740342999925, 1.358566136078000142 ),
 .UNSPECIFIED. ) ;
#21948 = CARTESIAN_POINT ( 'NONE',  ( 10.38236180178000012, -77.99492912598299199, -4.363545344708000151 ) ) ;
#21949 = CARTESIAN_POINT ( 'NONE',  ( 0.6503206246681177971, -81.93155565340288149, 1.067516121945689900 ) ) ;
#21950 = CARTESIAN_POINT ( 'NONE',  ( 0.1140339002500000004, -79.26247845825999150, 1.544894080918999713 ) ) ;
#21951 = CARTESIAN_POINT ( 'NONE',  ( 2.632967082928999947, -77.18321148114229402, 9.306700570505000769 ) ) ;
#21952 = DIRECTION ( 'NONE',  ( 0.000000000000000000, -1.000000000000000000, 0.000000000000000000 ) ) ;
#21953 = CARTESIAN_POINT ( 'NONE',  ( 2.799999999999999822, -76.00000000000000000, 0.000000000000000000 ) ) ;
#21954 = CARTESIAN_POINT ( 'NONE',  ( -4.109693089787123554, -80.19415985813694192, -9.933173281240437191 ) ) ;
#21955 = CARTESIAN_POINT ( 'NONE',  ( -12.52134121557681468, -23.92745484923118937, -1.618935178668596375 ) ) ;
#21956 = CARTESIAN_POINT ( 'NONE',  ( 3.113304451009999863, -78.49783470746899638, -10.55022916317000181 ) ) ;
#21957 = CIRCLE ( 'NONE', #15365, 1.500000000000000000 ) ;
#21958 = CONICAL_SURFACE ( 'NONE', #54968, 12.94999999994000106, 0.7853981633972997312 ) ;
#21959 = CARTESIAN_POINT ( 'NONE',  ( -1.047413957980333654, -80.85330312658089724, -0.8248344856773377476 ) ) ;
#21960 = FACE_OUTER_BOUND ( 'NONE', #38102, .T. ) ;
#21961 = ADVANCED_FACE ( 'NONE', ( #533 ), #54381, .F. ) ;
#21962 = CARTESIAN_POINT ( 'NONE',  ( 5.768896245881999896, -78.65561320193899064, 9.672321370914000127 ) ) ;
#21963 = CARTESIAN_POINT ( 'NONE',  ( -12.50000000000000000, -55.55000000278000272, 1.750000000000000000 ) ) ;
#21964 = VERTEX_POINT ( 'NONE', #24092 ) ;
#21965 = ORIENTED_EDGE ( 'NONE', *, *, #1941, .T. ) ;
#21966 = CARTESIAN_POINT ( 'NONE',  ( -1.364447001127000014, -80.56986782673699565, -0.3974066121187999623 ) ) ;
#21967 = ORIENTED_EDGE ( 'NONE', *, *, #4247, .F. ) ;
#21968 = CARTESIAN_POINT ( 'NONE',  ( 1.749899258081075271, -55.41283151199909440, 12.55433901288162168 ) ) ;
#21969 = ORIENTED_EDGE ( 'NONE', *, *, #57125, .F. ) ;
#21970 = CARTESIAN_POINT ( 'NONE',  ( 3.165411199172025292, -1.270833333333332815, 0.8506806241676674318 ) ) ;
#21971 = CARTESIAN_POINT ( 'NONE',  ( 11.44417895085271475, -77.52916666666665435, -3.075537641221520069 ) ) ;
#21972 = CARTESIAN_POINT ( 'NONE',  ( 8.677112325477001065, -79.94410278844959805, 6.812460760216000111 ) ) ;
#21973 = CARTESIAN_POINT ( 'NONE',  ( 2.019183793707000074, -23.78720277242999970, -12.79944116704999857 ) ) ;
#21974 = CARTESIAN_POINT ( 'NONE',  ( 0.5726238964369999573, -82.30157348994899280, -3.543415898539000075 ) ) ;
#21975 = CARTESIAN_POINT ( 'NONE',  ( -6.028334951382167795, -79.32967556650831398, 7.344047846277041103 ) ) ;
#21976 = ORIENTED_EDGE ( 'NONE', *, *, #58164, .F. ) ;
#21977 = CARTESIAN_POINT ( 'NONE',  ( -10.79754810891999917, -77.36671284630264722, -2.301543980132999767 ) ) ;
#21978 = CARTESIAN_POINT ( 'NONE',  ( 12.30892827549999957, -78.74849350881000021, -1.105470418167000091 ) ) ;
#21979 = ORIENTED_EDGE ( 'NONE', *, *, #48239, .F. ) ;
#21980 = ORIENTED_EDGE ( 'NONE', *, *, #55969, .F. ) ;
#21981 = CARTESIAN_POINT ( 'NONE',  ( 7.685661446562000343, -79.50000000000000000, -5.583959896778000420 ) ) ;
#21982 = VECTOR ( 'NONE', #33771, 1000.000000000000000 ) ;
#21983 = B_SPLINE_CURVE_WITH_KNOTS ( 'NONE', 3,
 ( #53708, #35083, #8830, #26242, #40414, #57831, #52828, #57540 ),
 .UNSPECIFIED., .F., .F.,
 ( 4, 2, 2, 4 ),
 ( 0.000000000000000000, 0.5000000000000000000, 0.7500000000000000000, 1.000000000000000000 ),
 .UNSPECIFIED. ) ;
#21984 = EDGE_CURVE ( 'NONE', #5753, #34724, #33626, .T. ) ;
#21985 = CARTESIAN_POINT ( 'NONE',  ( 0.9788970803261000109, -79.95624916642501034, -0.9057243817226000582 ) ) ;
#21986 = CARTESIAN_POINT ( 'NONE',  ( 9.690463944985998168, -78.45531731672599562, -0.5153813127049999832 ) ) ;
#21987 = CARTESIAN_POINT ( 'NONE',  ( 0.4757506811368034660, -86.31452044229999387, -4.520415813425825213 ) ) ;
#21988 = CARTESIAN_POINT ( 'NONE',  ( -1.469278768180998673, -86.01430711258555561, 3.096351707814453125 ) ) ;
#21989 = CARTESIAN_POINT ( 'NONE',  ( 5.759449073023001020, -78.34443890784000075, 11.78163922240000083 ) ) ;
#21990 = CARTESIAN_POINT ( 'NONE',  ( -8.971242061857001460, -76.80658961653000461, -8.906291659541000882 ) ) ;
#21991 = AXIS2_PLACEMENT_3D ( 'NONE', #25119, #7979, #25692 ) ;
#21992 = CARTESIAN_POINT ( 'NONE',  ( 8.020449964080999194, -76.26883820092800192, 7.526900779542000208 ) ) ;
#21993 = CARTESIAN_POINT ( 'NONE',  ( -9.216383265370728495, -78.60684264245168151, -0.7874879489689852186 ) ) ;
#21994 = CARTESIAN_POINT ( 'NONE',  ( 7.689575839419000580, -77.30706167140100149, 5.612681836884999775 ) ) ;
#21995 = CARTESIAN_POINT ( 'NONE',  ( -10.53003236230999917, -55.47547726255000100, 7.612971540256999958 ) ) ;
#21996 = CARTESIAN_POINT ( 'NONE',  ( -0.003967600564047823151, -2.975581622302581497, 3.249709392134530805 ) ) ;
#21997 = CARTESIAN_POINT ( 'NONE',  ( 0.5726387496589999682, -81.92492549782599554, -3.543412413248999915 ) ) ;
#21998 = AXIS2_PLACEMENT_3D ( 'NONE', #50001, #27530, #19278 ) ;
#21999 = CARTESIAN_POINT ( 'NONE',  ( 6.252156853421744209, -77.46842338808832551, -10.30345392412948158 ) ) ;
#22000 = CARTESIAN_POINT ( 'NONE',  ( -1.258323786088432650, -80.98444689146701592, 10.67706056211495813 ) ) ;
#22001 = CARTESIAN_POINT ( 'NONE',  ( 3.862060628231000159, -80.74883687878880778, 10.58270681924999934 ) ) ;
#22002 = CARTESIAN_POINT ( 'NONE',  ( -3.804208684430999909, -3.285148731141000145, -0.1186911049137999996 ) ) ;
#22003 = CARTESIAN_POINT ( 'NONE',  ( 1.274727678800788633, -79.49935659990086378, -0.01038921198208550382 ) ) ;
#22004 = VECTOR ( 'NONE', #23633, 1000.000000000000000 ) ;
#22005 = VERTEX_POINT ( 'NONE', #45975 ) ;
#22006 = CARTESIAN_POINT ( 'NONE',  ( 0.000000000000000000, -23.15000000000000213, -11.89999999977000122 ) ) ;
#22007 = CARTESIAN_POINT ( 'NONE',  ( 7.648026768019999366, -23.24999998419999869, 10.12290050217000115 ) ) ;
#22008 = CARTESIAN_POINT ( 'NONE',  ( -0.7068627984950999199, -81.14134166643898993, 1.130893941374999878 ) ) ;
#22009 = CARTESIAN_POINT ( 'NONE',  ( 3.324778437932995434, -79.05333333333332746, -8.934722022349857795 ) ) ;
#22010 = CARTESIAN_POINT ( 'NONE',  ( -3.201433918554999813, -77.87744717221998769, 12.61309089657999927 ) ) ;
#22011 = CARTESIAN_POINT ( 'NONE',  ( -8.618369191482001312, -79.53576001420199759, 4.042276274071999076 ) ) ;
#22012 = CARTESIAN_POINT ( 'NONE',  ( 12.60413652832999887, -18.69283065396999888, -1.799502287743000029 ) ) ;
#22013 = VERTEX_POINT ( 'NONE', #19091 ) ;
#22014 = EDGE_CURVE ( 'NONE', #48012, #3043, #22931, .T. ) ;
#22015 = CARTESIAN_POINT ( 'NONE',  ( -10.06692933811712365, -55.09657286937044063, 7.655995045256465126 ) ) ;
#22016 = CARTESIAN_POINT ( 'NONE',  ( 1.975443078346000192, -77.04017089215798819, 11.09968961003999866 ) ) ;
#22017 = EDGE_CURVE ( 'NONE', #47194, #52418, #54529, .T. ) ;
#22018 = CARTESIAN_POINT ( 'NONE',  ( -0.2109498265882999990, -82.12980651837901291, 1.293563445978999971 ) ) ;
#22019 = CARTESIAN_POINT ( 'NONE',  ( 11.68767212001979239, -79.12916666666667709, -3.140974612311342451 ) ) ;
#22020 = CARTESIAN_POINT ( 'NONE',  ( -6.639445101857000431, -78.02053767652898841, -6.825550891425999467 ) ) ;
#22021 = CARTESIAN_POINT ( 'NONE',  ( -1.831926221770999952, -85.94606716926699619, 3.748911303548999818 ) ) ;
#22022 = CARTESIAN_POINT ( 'NONE',  ( -1.667936697358999965, -59.56462890159999546, -12.53241208775999915 ) ) ;
#22023 = CARTESIAN_POINT ( 'NONE',  ( -0.6219878248318000402, -79.63867704943100989, -1.382777385570999940 ) ) ;
#22024 = ORIENTED_EDGE ( 'NONE', *, *, #31524, .T. ) ;
#22025 = CARTESIAN_POINT ( 'NONE',  ( 1.900435629933197923, -77.23927092607918610, -10.60415385166746027 ) ) ;
#22026 = CARTESIAN_POINT ( 'NONE',  ( 8.485281374238999419, -18.75000000000000000, 8.485281374238999419 ) ) ;
#22027 = CARTESIAN_POINT ( 'NONE',  ( -2.821716789433580619, -78.79507810614309449, -2.832896129789050921 ) ) ;
#22028 = VERTEX_POINT ( 'NONE', #18226 ) ;
#22029 = ORIENTED_EDGE ( 'NONE', *, *, #16899, .F. ) ;
#22030 = CARTESIAN_POINT ( 'NONE',  ( -10.53745838584999994, -79.85354523164899376, 2.317267403318000074 ) ) ;
#22031 = VECTOR ( 'NONE', #18068, 999.9999999999998863 ) ;
#22032 = CARTESIAN_POINT ( 'NONE',  ( -11.75000000000000000, -76.04999999999999716, -3.652443742841000169E-09 ) ) ;
#22033 = EDGE_CURVE ( 'NONE', #47003, #35953, #8483, .T. ) ;
#22034 = CARTESIAN_POINT ( 'NONE',  ( 8.837556037038000412, -79.93830006555698731, -7.266664171576000086 ) ) ;
#22035 = ORIENTED_EDGE ( 'NONE', *, *, #16973, .T. ) ;
#22036 = CARTESIAN_POINT ( 'NONE',  ( 10.24006772854000147, -78.48531443679999597, 6.351124671173999481 ) ) ;
#22037 = ORIENTED_EDGE ( 'NONE', *, *, #17446, .F. ) ;
#22038 = ORIENTED_EDGE ( 'NONE', *, *, #17635, .F. ) ;
#22039 = CIRCLE ( 'NONE', #21087, 13.00000000000000000 ) ;
#22040 = CARTESIAN_POINT ( 'NONE',  ( 12.00000000000000000, -76.64999999999999147, 0.000000000000000000 ) ) ;
#22041 = CARTESIAN_POINT ( 'NONE',  ( -1.490118887467393627, -0.9426324846354789955, -3.733870388342663826 ) ) ;
#22042 = VERTEX_POINT ( 'NONE', #14642 ) ;
#22043 = CARTESIAN_POINT ( 'NONE',  ( 1.461448385607039491, -81.67104446236695026, 0.3928510776231207702 ) ) ;
#22044 = VERTEX_POINT ( 'NONE', #49812 ) ;
#22045 = CARTESIAN_POINT ( 'NONE',  ( 0.000000000000000000, -75.15999999999999659, 0.000000000000000000 ) ) ;
#22046 = CARTESIAN_POINT ( 'NONE',  ( -3.444390624473297358, -78.77851879815550262, -1.946200917927129570 ) ) ;
#22047 = FACE_OUTER_BOUND ( 'NONE', #20223, .T. ) ;
#22048 = CARTESIAN_POINT ( 'NONE',  ( 12.00000000000000000, -77.54999999999999716, 0.000000000000000000 ) ) ;
#22049 = CARTESIAN_POINT ( 'NONE',  ( -7.220923959705292994, -78.72708333333336839, 9.396085398178589898 ) ) ;
#22050 = CIRCLE ( 'NONE', #16437, 0.6999999999999999556 ) ;
#22051 = CARTESIAN_POINT ( 'NONE',  ( -10.86788298907000083, -77.68455751383611130, -5.040355520269000245 ) ) ;
#22052 = CARTESIAN_POINT ( 'NONE',  ( 8.872594700925422018, -78.82720320433729455, -2.619895919442627008 ) ) ;
#22053 = CARTESIAN_POINT ( 'NONE',  ( -9.966224254735001509, -23.66904904784999886, 7.657729124005999921 ) ) ;
#22054 = CARTESIAN_POINT ( 'NONE',  ( -1.500000000000000000, -79.90000000000000568, 0.000000000000000000 ) ) ;
#22055 = CIRCLE ( 'NONE', #25863, 9.000000000000000000 ) ;
#22056 = CARTESIAN_POINT ( 'NONE',  ( -2.068479106922999744, -79.89225264934799497, 3.626429920131999829 ) ) ;
#22057 = EDGE_CURVE ( 'NONE', #52539, #6658, #35240, .T. ) ;
#22058 = CARTESIAN_POINT ( 'NONE',  ( 5.787933236233000045, -76.93448667140100383, -7.442428143219999903 ) ) ;
#22059 = CARTESIAN_POINT ( 'NONE',  ( 1.217465845835393967, -83.27083333333331439, 0.3271848554491025851 ) ) ;
#22060 = FACE_OUTER_BOUND ( 'NONE', #7356, .T. ) ;
#22061 = CARTESIAN_POINT ( 'NONE',  ( -0.5154756746315999338, -25.13240599763000205, 12.66205448072999928 ) ) ;
#22062 = CARTESIAN_POINT ( 'NONE',  ( 1.281522546595510681, -81.47967980706110325, -0.3373344656957449339 ) ) ;
#22063 = CARTESIAN_POINT ( 'NONE',  ( -12.05000000000000071, -74.80000000000001137, 0.000000000000000000 ) ) ;
#22064 = CARTESIAN_POINT ( 'NONE',  ( 3.591303024676000266, -1.295096044169000038, -0.4777876730464000188 ) ) ;
#22065 = VECTOR ( 'NONE', #7014, 1000.000000000000114 ) ;
#22066 = CARTESIAN_POINT ( 'NONE',  ( -0.4440249787718509311, -80.74810222861310649, 1.446726180314430010 ) ) ;
#22067 = CARTESIAN_POINT ( 'NONE',  ( -0.7735775726147171572, -78.52788082791856539, 0.9939198430596817291 ) ) ;
#22068 = CARTESIAN_POINT ( 'NONE',  ( 0.000000000000000000, -0.1000000007601000024, -10.29999999923999887 ) ) ;
#22069 = CARTESIAN_POINT ( 'NONE',  ( 1.250000000000000000, -80.25000000000000000, 0.000000000000000000 ) ) ;
#22070 = CARTESIAN_POINT ( 'NONE',  ( 2.778581917921999711, -78.38111084099200809, 10.55721783972000161 ) ) ;
#22071 = CARTESIAN_POINT ( 'NONE',  ( -9.108185712014998714, -77.81490627187800158, 8.236305738405000909 ) ) ;
#22072 = DIRECTION ( 'NONE',  ( 0.000000000000000000, 0.000000000000000000, -1.000000000000000000 ) ) ;
#22074 = CARTESIAN_POINT ( 'NONE',  ( -0.1190996060027000036, -77.91562118112170765, -1.412746526842000083 ) ) ;
#22073 = DIRECTION ( 'NONE',  ( 0.000000000000000000, 0.000000000000000000, -1.000000000000000000 ) ) ;
#22075 = CARTESIAN_POINT ( 'NONE',  ( 1.517511648408000013, -81.98249872513999037, -0.7726417995267998995 ) ) ;
#22076 = VERTEX_POINT ( 'NONE', #6523 ) ;
#22077 = CARTESIAN_POINT ( 'NONE',  ( 4.484526869169065399, -78.74462836071080574, 11.18137712903838299 ) ) ;
#22078 = CARTESIAN_POINT ( 'NONE',  ( 9.798978774566998950, -80.78509494028411098, -5.119823760639000909 ) ) ;
#22079 = EDGE_CURVE ( 'NONE', #17474, #41507, #31693, .T. ) ;
#22080 = DIRECTION ( 'NONE',  ( 1.000000000000000000, 0.000000000000000000, 0.000000000000000000 ) ) ;
#22081 = DIRECTION ( 'NONE',  ( 0.000000000000000000, -1.000000000000000000, 0.000000000000000000 ) ) ;
#22082 = CARTESIAN_POINT ( 'NONE',  ( -4.000000000000000000, -75.00000000000001421, -0.5999999999999999778 ) ) ;
#22083 = CARTESIAN_POINT ( 'NONE',  ( 8.584722543520001636, -79.11501084750798896, 4.148835967969999317 ) ) ;
#22084 = CARTESIAN_POINT ( 'NONE',  ( -0.6004213309738001270, -0.6558122488618000068, -3.487579485068999841 ) ) ;
#22085 = CARTESIAN_POINT ( 'NONE',  ( 5.850913721802999845, -79.38296787954499223, -7.837718406031999763 ) ) ;
#22086 = CARTESIAN_POINT ( 'NONE',  ( -8.838834764832000701, -60.04999999966999980, -8.838834764832000701 ) ) ;
#22087 = CARTESIAN_POINT ( 'NONE',  ( -2.062670899361999766, -60.10639784916000394, 12.83044027763000017 ) ) ;
#22088 = ORIENTED_EDGE ( 'NONE', *, *, #43438, .F. ) ;
#22089 = DIRECTION ( 'NONE',  ( 1.000000000000000000, 0.000000000000000000, 0.000000000000000000 ) ) ;
#22090 = CYLINDRICAL_SURFACE ( 'NONE', #27831, 1.250000000000000000 ) ;
#22091 = CARTESIAN_POINT ( 'NONE',  ( -0.5458445578339461424, -1.713104424745484300, -3.230288565804697143 ) ) ;
#22092 = CARTESIAN_POINT ( 'NONE',  ( -10.04115011118999945, -56.03513569577999931, -7.682331425181999407 ) ) ;
#22093 = B_SPLINE_CURVE_WITH_KNOTS ( 'NONE', 3,
 ( #38153, #56175, #8595, #22169, #54357, #21875, #40768, #3589, #362, #49639 ),
 .UNSPECIFIED., .F., .F.,
 ( 4, 2, 2, 2, 4 ),
 ( 0.000000000000000000, 0.2500000000000000000, 0.5000000000000000000, 0.7500000000000000000, 1.000000000000000000 ),
 .UNSPECIFIED. ) ;
#22094 = CARTESIAN_POINT ( 'NONE',  ( 1.863042131308999982, -85.67417953870899794, 3.018880368111999779 ) ) ;
#22095 = CARTESIAN_POINT ( 'NONE',  ( -1.570796326794885012, -76.91458333333332575, -12.00000000000000178 ) ) ;
#22096 = CONICAL_SURFACE ( 'NONE', #4202, 2.399999999383999771, 0.7853981633972997312 ) ;
#22097 = ADVANCED_FACE ( 'NONE', ( #33080 ), #41181, .T. ) ;
#22098 = EDGE_LOOP ( 'NONE', ( #33962, #20611, #42835, #20876, #16759, #41356, #9637, #50462, #31883, #455 ) ) ;
#22099 = CARTESIAN_POINT ( 'NONE',  ( -12.55432891850757748, -55.41272687720891099, 1.749897736046110541 ) ) ;
#22100 = CARTESIAN_POINT ( 'NONE',  ( 11.67628222315400599, -77.93643586021261171, -1.539162911442760517 ) ) ;
#22101 = DIRECTION ( 'NONE',  ( 0.7071067811865475727, 0.000000000000000000, -0.7071067811865475727 ) ) ;
#22102 = EDGE_CURVE ( 'NONE', #10870, #25466, #9238, .T. ) ;
#22103 = VERTEX_POINT ( 'NONE', #7105 ) ;
#22104 = VERTEX_POINT ( 'NONE', #57553 ) ;
#22105 = CARTESIAN_POINT ( 'NONE',  ( -12.58335110165999993, -57.05111654290000445, 1.667961430005999945 ) ) ;
#22106 = CARTESIAN_POINT ( 'NONE',  ( -7.647736468613000049, -55.07704514418999509, -10.13404651203999940 ) ) ;
#22107 = VECTOR ( 'NONE', #5418, 1000.000000000000000 ) ;
#22108 = CARTESIAN_POINT ( 'NONE',  ( 6.653382217586999658, -79.58521449586598351, 7.150748904218000135 ) ) ;
#22109 = EDGE_LOOP ( 'NONE', ( #14740, #7958 ) ) ;
#22110 = VERTEX_POINT ( 'NONE', #29524 ) ;
#22111 = CARTESIAN_POINT ( 'NONE',  ( -3.720841153849000271, -77.09048477876800121, 11.77893002587000026 ) ) ;
#22112 = CARTESIAN_POINT ( 'NONE',  ( -10.44660810894644598, -78.61899168769637924, -2.535882402899716670 ) ) ;
#22113 = CARTESIAN_POINT ( 'NONE',  ( 0.06588118243728999235, -79.39804249476999587, -1.568452433177999872 ) ) ;
#22114 = EDGE_LOOP ( 'NONE', ( #56234, #9653, #7319, #27481 ) ) ;
#22115 = CARTESIAN_POINT ( 'NONE',  ( -8.383077572658999443, -77.65125584965400662, 4.458862939031999595 ) ) ;
#22116 = CARTESIAN_POINT ( 'NONE',  ( 5.091979538295729135, -78.68094881684694997, 8.261087832219587312 ) ) ;
#22117 = EDGE_CURVE ( 'NONE', #3901, #22275, #34524, .T. ) ;
#22118 = CARTESIAN_POINT ( 'NONE',  ( 0.2449793097989906576, -80.24093316106807094, -1.227248574985329688 ) ) ;
#22119 = CARTESIAN_POINT ( 'NONE',  ( -8.110204649352999340, -78.42570409358999939, 9.400142180594000862 ) ) ;
#22120 = CARTESIAN_POINT ( 'NONE',  ( 11.01642476344999899, -77.01506690846845515, 2.111041454437999842 ) ) ;
#22121 = DIRECTION ( 'NONE',  ( -1.000000000000000000, 0.000000000000000000, 1.929499587357000000E-14 ) ) ;
#22122 = CARTESIAN_POINT ( 'NONE',  ( 3.274617103212424940, -86.31452042059399332, 2.378452838117018242 ) ) ;
#22123 = CARTESIAN_POINT ( 'NONE',  ( -6.206245474241999460, -79.82334034854498839, 9.343480492029000217 ) ) ;
#22124 = CARTESIAN_POINT ( 'NONE',  ( 5.428802703023839271, -79.92556352659003949, 7.489012433513578593 ) ) ;
#22125 = CARTESIAN_POINT ( 'NONE',  ( 10.25203062049729041, -17.87822876371741998, 7.730397977284573230 ) ) ;
#22126 = ORIENTED_EDGE ( 'NONE', *, *, #32128, .T. ) ;
#22127 = CARTESIAN_POINT ( 'NONE',  ( -9.757422770562000025, -79.57915461743898788, 5.632196307135999724 ) ) ;
#22128 = CARTESIAN_POINT ( 'NONE',  ( -3.151328970204000157, -76.15639898940999331, -11.89977497056000111 ) ) ;
#22129 = CARTESIAN_POINT ( 'NONE',  ( -1.606812318740999945, -79.90019517812399386, 0.1592736582230999953 ) ) ;
#22130 = B_SPLINE_SURFACE_WITH_KNOTS ( 'NONE', 3, 3, ( 
 ( #13797, #46003, #23828, #5527 ),
 ( #6118, #40680, #18251, #31799 ),
 ( #27376, #1132, #22962, #32096 ),
 ( #18541, #40972, #14098, #9678 ),
 ( #5248, #23253, #41262, #36823 ),
 ( #54838, #14381, #32381, #19704 ),
 ( #20005, #20856, #38575, #42727 ),
 ( #52170, #25285, #37989, #33557 ) ),
 .UNSPECIFIED., .F., .F., .F.,
 ( 4, 1, 1, 1, 1, 4 ),
 ( 4, 4 ),
 ( -0.01200407345748999953, 0.000000000000000000, 0.3333333333333000081, 0.6666666666667000474, 1.000000000000000000, 1.011997855551999947 ),
 ( -0.3559705542741999906, 1.355970554273999928 ),
 .UNSPECIFIED. ) ;
#22132 = EDGE_CURVE ( 'NONE', #16033, #18435, #42286, .T. ) ;
#22131 = CARTESIAN_POINT ( 'NONE',  ( 0.8816674349947000167, -77.97481505010179603, 0.9814419191067000892 ) ) ;
#22133 = CARTESIAN_POINT ( 'NONE',  ( -3.554945896888052737, -3.345802747932901777, 0.1544303516782937480 ) ) ;
#22134 = DIRECTION ( 'NONE',  ( 0.9999999999998321343, 0.000000000000000000, 5.794540611356191117E-07 ) ) ;
#22135 = CARTESIAN_POINT ( 'NONE',  ( -12.17466003208999936, -76.69120375783900556, 1.612538369963999907 ) ) ;
#22136 = CARTESIAN_POINT ( 'NONE',  ( 0.000000000000000000, -75.15999999999999659, 0.000000000000000000 ) ) ;
#22137 = EDGE_CURVE ( 'NONE', #47867, #35763, #34817, .T. ) ;
#22138 = CARTESIAN_POINT ( 'NONE',  ( -9.646812774837000504, -76.86848998579799286, 1.323497712265999882 ) ) ;
#22139 = CARTESIAN_POINT ( 'NONE',  ( 10.53003236233000095, -18.67547726287999765, -7.612971540274999782 ) ) ;
#22140 = CARTESIAN_POINT ( 'NONE',  ( 6.233047529871999615, -78.98050366622999263, 9.960502923565000444 ) ) ;
#22141 = FACE_OUTER_BOUND ( 'NONE', #54725, .T. ) ;
#22142 = AXIS2_PLACEMENT_3D ( 'NONE', #33499, #24065, #41491 ) ;
#22143 = CARTESIAN_POINT ( 'NONE',  ( -2.099388381696000338E-14, -0.1000000000000002554, -12.80000000000033467 ) ) ;
#22144 = VERTEX_POINT ( 'NONE', #43705 ) ;
#22145 = CARTESIAN_POINT ( 'NONE',  ( -0.7427769915940999335, -81.97954691737999156, -1.400956470667000131 ) ) ;
#22146 = CIRCLE ( 'NONE', #55161, 14.00000000000000000 ) ;
#22147 = CARTESIAN_POINT ( 'NONE',  ( -1.250000000000000000, -78.60000000000000853, 0.000000000000000000 ) ) ;
#22148 = CYLINDRICAL_SURFACE ( 'NONE', #25741, 14.00000000000000000 ) ;
#22149 = CARTESIAN_POINT ( 'NONE',  ( -7.624341766629000539, -55.53514853726999689, 10.42531125022999916 ) ) ;
#22150 = DIRECTION ( 'NONE',  ( 0.000000000000000000, 0.8191944460894733382, -0.5735158755397804509 ) ) ;
#22151 = CARTESIAN_POINT ( 'NONE',  ( -11.44451898095999987, -78.09947541138799920, -3.385038809382000302 ) ) ;
#22152 = CARTESIAN_POINT ( 'NONE',  ( -5.505695391233000002, -78.64704805011498934, -8.014431902511001127 ) ) ;
#22153 = CARTESIAN_POINT ( 'NONE',  ( 4.459991035765999534, -77.47927130271399676, 8.413017068390001185 ) ) ;
#22154 = CARTESIAN_POINT ( 'NONE',  ( -10.10713367717059796, -24.46653151341558896, -7.860990029285546576 ) ) ;
#22155 = CARTESIAN_POINT ( 'NONE',  ( 11.73168449440016481, -75.95508173438524580, 0.7621015541101189283 ) ) ;
#22156 = CARTESIAN_POINT ( 'NONE',  ( 5.472379214682000281, -80.19337520226639526, -9.446080217779000421 ) ) ;
#22157 = CARTESIAN_POINT ( 'NONE',  ( 1.577629893833666808, -85.94828561723799965, 3.635239426043249011 ) ) ;
#22158 = ORIENTED_EDGE ( 'NONE', *, *, #3718, .F. ) ;
#22159 = CARTESIAN_POINT ( 'NONE',  ( -1.250000000000000000, -79.51887984502333495, -0.2965639121358008001 ) ) ;
#22160 = CARTESIAN_POINT ( 'NONE',  ( -3.168364096407636499, -2.122297881318587542, -0.8517483099742300112 ) ) ;
#22161 = AXIS2_PLACEMENT_3D ( 'NONE', #54694, #5389, #23397 ) ;
#22162 = CARTESIAN_POINT ( 'NONE',  ( -11.21736175386999967, -79.85981236905720948, -4.975459846704000100 ) ) ;
#22163 = CARTESIAN_POINT ( 'NONE',  ( -0.03413113949348758891, -78.40681307385639798, -3.621286655835656898 ) ) ;
#22164 = CARTESIAN_POINT ( 'NONE',  ( 0.3958579896396000608, -81.41448259405999011, -1.618315812554999900 ) ) ;
#22165 = CARTESIAN_POINT ( 'NONE',  ( -9.438868967565998247, -79.47276953209699002, -5.601050722391000214 ) ) ;
#22166 = CARTESIAN_POINT ( 'NONE',  ( -10.75000000000000000, -80.44999999999998863, 5.225043809877999334E-10 ) ) ;
#22167 = CARTESIAN_POINT ( 'NONE',  ( -6.570942521484999688, -76.52164013402300213, -10.50046416013000083 ) ) ;
#22168 = CARTESIAN_POINT ( 'NONE',  ( 5.939518926465330750, -78.53233929404970581, 10.13791247079975832 ) ) ;
#22169 = CARTESIAN_POINT ( 'NONE',  ( 1.075291064028265797, -77.93750000007800338, 0.7806521200495090129 ) ) ;
#22170 = VERTEX_POINT ( 'NONE', #29805 ) ;
#22171 = CARTESIAN_POINT ( 'NONE',  ( -10.17265785211000129, -78.60952198136099867, 4.268344714933999917 ) ) ;
#22172 = CARTESIAN_POINT ( 'NONE',  ( 1.120846582852062401, -79.88692784018829229, 0.5535639178212069522 ) ) ;
#22173 = CARTESIAN_POINT ( 'NONE',  ( 10.17807092908048539, -75.79999999999999716, -6.222892922246035852 ) ) ;
#22174 = CARTESIAN_POINT ( 'NONE',  ( -2.375990622215050418, -78.54828561723800817, 3.940594454193545371 ) ) ;
#22175 = CARTESIAN_POINT ( 'NONE',  ( -11.08844420678000020, -78.75192546654999148, -1.240163186867999867 ) ) ;
#22176 = DIRECTION ( 'NONE',  ( 0.000000000000000000, 0.000000000000000000, -1.000000000000000000 ) ) ;
#22177 = CARTESIAN_POINT ( 'NONE',  ( 0.6451515509158406436, -81.68939381893659402, 1.369045774478446553 ) ) ;
#22178 = EDGE_CURVE ( 'NONE', #9689, #47619, #23969, .T. ) ;
#22179 = CARTESIAN_POINT ( 'NONE',  ( 11.82394432951000063, -79.05483761240600415, -3.315134025842000121 ) ) ;
#22180 = CARTESIAN_POINT ( 'NONE',  ( 10.12290050253000118, -23.24999997822999731, -7.648026768374000639 ) ) ;
#22181 = DIRECTION ( 'NONE',  ( 0.000000000000000000, -1.000000000000000000, 0.000000000000000000 ) ) ;
#22182 = CARTESIAN_POINT ( 'NONE',  ( -12.71005379442735084, -61.09489531480230085, -1.687596143085857481 ) ) ;
#22183 = VECTOR ( 'NONE', #31132, 1000.000000000000000 ) ;
#22184 = DIRECTION ( 'NONE',  ( 1.000000000000000000, 0.000000000000000000, 0.000000000000000000 ) ) ;
#22185 = EDGE_LOOP ( 'NONE', ( #22776, #32556, #32355, #47660, #54660 ) ) ;
#22186 = ORIENTED_EDGE ( 'NONE', *, *, #43462, .T. ) ;
#22187 = CARTESIAN_POINT ( 'NONE',  ( 10.72009390921250649, -78.84356995979068472, -0.8762394021455865989 ) ) ;
#22188 = ORIENTED_EDGE ( 'NONE', *, *, #38962, .T. ) ;
#22189 = FACE_OUTER_BOUND ( 'NONE', #7504, .T. ) ;
#22190 = VERTEX_POINT ( 'NONE', #21252 ) ;
#22191 = CARTESIAN_POINT ( 'NONE',  ( 7.660411271047999904, -23.19173735492000077, 10.01752031414999955 ) ) ;
#22192 = CARTESIAN_POINT ( 'NONE',  ( 8.921077980507002181, -77.94118402616200569, 6.489691983999000158 ) ) ;
#22193 = ADVANCED_FACE ( 'NONE', ( #12398 ), #17708, .T. ) ;
#22194 = CARTESIAN_POINT ( 'NONE',  ( 8.137215171343429532, -55.34844303568876711, -7.401770473315444576 ) ) ;
#22195 = CARTESIAN_POINT ( 'NONE',  ( 9.310971084499998440, -78.40158998579799743, 2.673395725080999874 ) ) ;
#22196 = ADVANCED_FACE ( 'NONE', ( #35991 ), #36453, .F. ) ;
#22197 = CARTESIAN_POINT ( 'NONE',  ( -9.022067442310994778, -78.11871138684033156, -2.130921441519212145 ) ) ;
#22198 = CARTESIAN_POINT ( 'NONE',  ( -8.382198119002001846, -79.82394495700170012, -7.453647783897999979 ) ) ;
#22199 = CARTESIAN_POINT ( 'NONE',  ( 0.9981636088842267274, -79.40219188384969584, 0.7561152057269426852 ) ) ;
#22200 = ORIENTED_EDGE ( 'NONE', *, *, #30527, .F. ) ;
#22201 = ORIENTED_EDGE ( 'NONE', *, *, #56456, .F. ) ;
#22202 = CARTESIAN_POINT ( 'NONE',  ( -0.09048081827621948237, -77.47593987896340195, 9.249522775818471487 ) ) ;
#22203 = CARTESIAN_POINT ( 'NONE',  ( 10.77519778174000109, -77.17117949372459407, -1.228540277667999892 ) ) ;
#22204 = CARTESIAN_POINT ( 'NONE',  ( -1.460959015002474937, -77.97916666666665719, 0.3926218265389144757 ) ) ;
#22205 = CARTESIAN_POINT ( 'NONE',  ( 9.259046916275000427, -78.66464992286799429, 2.905298533503999803 ) ) ;
#22206 = CARTESIAN_POINT ( 'NONE',  ( -2.150406028006000003, -75.63298130519999063, 12.46554692171000056 ) ) ;
#22207 = CARTESIAN_POINT ( 'NONE',  ( -9.363446672522654168, -79.41312937742843303, -1.604998447536725603 ) ) ;
#22208 = LINE ( 'NONE', #3347, #23298 ) ;
#22209 = CARTESIAN_POINT ( 'NONE',  ( -2.179156891764956416, -79.40744640124135856, -9.282072619734307750 ) ) ;
#22210 = EDGE_CURVE ( 'NONE', #19028, #43389, #29609, .T. ) ;
#22211 = CARTESIAN_POINT ( 'NONE',  ( 12.66315144086999922, -16.82197088188999601, 0.06064144874956999692 ) ) ;
#22212 = DIRECTION ( 'NONE',  ( 0.000000000000000000, -1.000000000000000000, 0.000000000000000000 ) ) ;
#22213 = CARTESIAN_POINT ( 'NONE',  ( -6.277317685251144752, -79.23269343647702101, 7.157620870793346413 ) ) ;
#22214 = VERTEX_POINT ( 'NONE', #32717 ) ;
#22215 = CARTESIAN_POINT ( 'NONE',  ( 6.596971017208000276, -79.20390260564799689, 10.53897607326000063 ) ) ;
#22216 = CARTESIAN_POINT ( 'NONE',  ( 0.000000000000000000, -87.20000000000000284, 0.000000000000000000 ) ) ;
#22217 = CARTESIAN_POINT ( 'NONE',  ( -5.561497340033285219, -78.01840227481952184, 9.199883782775010843 ) ) ;
#22218 = CARTESIAN_POINT ( 'NONE',  ( -3.545645331619000196, -77.60059338993599454, 11.44309676683000099 ) ) ;
#22219 = CARTESIAN_POINT ( 'NONE',  ( -10.19022281666000040, -18.80366258888000175, -7.646946378508999942 ) ) ;
#22221 = CARTESIAN_POINT ( 'NONE',  ( -0.8537148449481999357, -17.29501854091000013, -12.43377424872999981 ) ) ;
#22220 = CARTESIAN_POINT ( 'NONE',  ( -1.247385803317999864, -61.27722255996999934, -12.50301438880000049 ) ) ;
#22222 = CARTESIAN_POINT ( 'NONE',  ( 3.241578942234999872, -86.36264282632899381, -1.443243930775000239 ) ) ;
#22223 = CARTESIAN_POINT ( 'NONE',  ( 6.596840968109408898, -80.92259746458073266, 8.494723663472855790 ) ) ;
#22224 = CARTESIAN_POINT ( 'NONE',  ( 10.04116292115999975, -56.03537109808000594, -7.682344222575999915 ) ) ;
#22225 = CARTESIAN_POINT ( 'NONE',  ( -2.486604901413152824, -78.40416666666666856, -9.252740428349003565 ) ) ;
#22226 = CARTESIAN_POINT ( 'NONE',  ( -9.340344124447998553, -76.87058518366599458, -6.292213870087999261 ) ) ;
#22227 = CARTESIAN_POINT ( 'NONE',  ( 0.000000000000000000, -77.40000000000736691, 0.000000000000000000 ) ) ;
#22228 = CARTESIAN_POINT ( 'NONE',  ( -1.697681976669999981, -81.00396274871158653, -11.01068734798000115 ) ) ;
#22229 = DIRECTION ( 'NONE',  ( 0.000000000000000000, 1.000000000000000000, 0.000000000000000000 ) ) ;
#22230 = EDGE_CURVE ( 'NONE', #521, #16460, #13400, .T. ) ;
#22231 = CARTESIAN_POINT ( 'NONE',  ( 1.698401934078999975, -54.57985954063000378, 12.66748707609000135 ) ) ;
#22232 = VECTOR ( 'NONE', #27087, 1000.000000000000000 ) ;
#22233 = DIRECTION ( 'NONE',  ( 1.000000000000000000, 0.000000000000000000, 0.000000000000000000 ) ) ;
#22234 = CARTESIAN_POINT ( 'NONE',  ( 1.655866326982999848, -1.964893323557999949, -3.604003584276000094 ) ) ;
#22235 = CARTESIAN_POINT ( 'NONE',  ( -8.608637500484000782, -79.48745298729599540, 3.836350400429999752 ) ) ;
#22236 = CARTESIAN_POINT ( 'NONE',  ( 10.68101746380904515, -76.86058654510705423, 1.407256982417045332 ) ) ;
#22237 = CARTESIAN_POINT ( 'NONE',  ( 9.408852130907261468, -77.30624999999999147, -5.763669873574839286 ) ) ;
#22238 = CARTESIAN_POINT ( 'NONE',  ( -1.761265949705000056, -60.50858218752999562, 12.57448205046000034 ) ) ;
#22239 = CARTESIAN_POINT ( 'NONE',  ( 12.72394144137000005, -18.77839271500000251, 1.930881231431999856 ) ) ;
#22240 = VECTOR ( 'NONE', #50278, 1000.000000000000000 ) ;
#22241 = CARTESIAN_POINT ( 'NONE',  ( 0.2895459579014000306, -85.28007450217398855, -4.120032362860000852 ) ) ;
#22242 = CARTESIAN_POINT ( 'NONE',  ( -11.55514622889111465, -76.05000000000001137, 2.460715416399694266 ) ) ;
#22243 = VECTOR ( 'NONE', #46693, 1000.000000000000114 ) ;
#22244 = CARTESIAN_POINT ( 'NONE',  ( -10.97571145796055703, -76.91879331913770557, 5.030464531489157842 ) ) ;
#22245 = CARTESIAN_POINT ( 'NONE',  ( -6.042059545598000625, -78.58551785422000080, 10.44717322784999958 ) ) ;
#22246 = CARTESIAN_POINT ( 'NONE',  ( -9.936460025306999455, -77.24629348652399585, -5.051867252445999767 ) ) ;
#22247 = CARTESIAN_POINT ( 'NONE',  ( 0.5893919561240600347, -81.93594225748110205, 1.102503278612346316 ) ) ;
#22248 = CARTESIAN_POINT ( 'NONE',  ( -0.7373102530955000233, -77.91848566455999503, -1.491280593247999997 ) ) ;
#22249 = CARTESIAN_POINT ( 'NONE',  ( 7.764258067048000811, -77.19129567287669147, 5.767450660628000492 ) ) ;
#22250 = CARTESIAN_POINT ( 'NONE',  ( -1.355824619571554868, -82.71355153832641349, 0.6688378176153790822 ) ) ;
#22251 = CARTESIAN_POINT ( 'NONE',  ( -3.250000000000001332, -2.510416666666666075, -0.4254240051736181139 ) ) ;
#22252 = CARTESIAN_POINT ( 'NONE',  ( -1.229427629842215985, -80.21594462373234080, -10.68102437834389207 ) ) ;
#22253 = DIRECTION ( 'NONE',  ( 0.000000000000000000, -0.7071067811866525998, -0.7071067811864425456 ) ) ;
#22254 = CARTESIAN_POINT ( 'NONE',  ( 0.9578449722871110739, -78.98171181572377009, -11.17605216401635637 ) ) ;
#22255 = CARTESIAN_POINT ( 'NONE',  ( 0.4857358544503080355, -81.75688173250232182, -1.151682746447475036 ) ) ;
#22256 = CARTESIAN_POINT ( 'NONE',  ( 9.611650271896843734, -79.39166666666663730, 5.539808784079872872 ) ) ;
#22257 = CARTESIAN_POINT ( 'NONE',  ( 2.188076007269000200, -78.68284954493999805, 11.04745617521000156 ) ) ;
#22258 = CARTESIAN_POINT ( 'NONE',  ( 1.217465845835394855, -80.22916666666665719, -0.3271848554490981997 ) ) ;
#22259 = ORIENTED_EDGE ( 'NONE', *, *, #35924, .F. ) ;
#22260 = ORIENTED_EDGE ( 'NONE', *, *, #15752, .T. ) ;
#22261 = CARTESIAN_POINT ( 'NONE',  ( 0.1045857360044000067, -80.86178450267699702, 1.611296339591000049 ) ) ;
#22262 = ORIENTED_EDGE ( 'NONE', *, *, #39759, .T. ) ;
#22263 = SURFACE_STYLE_FILL_AREA ( #13402 ) ;
#22264 = VERTEX_POINT ( 'NONE', #10610 ) ;
#22265 = B_SPLINE_CURVE_WITH_KNOTS ( 'NONE', 3,
 ( #28418, #51762, #56182, #21026, #38452, #11313, #39033, #33727, #22095, #20459, #35672, #34013, #7740, #52049, #29294, #29868, #17683, #56469 ),
 .UNSPECIFIED., .F., .F.,
 ( 4, 2, 2, 2, 2, 2, 2, 2, 4 ),
 ( 0.000000000000000000, 0.1250000000000000000, 0.2500000000000000000, 0.3750000000000000000, 0.5000000000000000000, 0.6250000000000000000, 0.7500000000000000000, 0.8750000000000000000, 1.000000000000000000 ),
 .UNSPECIFIED. ) ;
#22266 = EDGE_CURVE ( 'NONE', #31399, #42913, #6456, .T. ) ;
#22267 = CARTESIAN_POINT ( 'NONE',  ( 0.000000000000000000, -75.20000000000000284, -5.100000000000000533 ) ) ;
#22268 = CARTESIAN_POINT ( 'NONE',  ( 10.97276992925000094, -79.39937592841299363, 1.140199307644999882 ) ) ;
#22269 = CARTESIAN_POINT ( 'NONE',  ( 0.005523896503950999348, -25.06963456225999920, -12.55021156880999911 ) ) ;
#22270 = CARTESIAN_POINT ( 'NONE',  ( -3.752697076307999868, -80.49395764150798982, 0.1692192794638000264 ) ) ;
#22271 = CARTESIAN_POINT ( 'NONE',  ( -1.413089197430621669, -79.28666837594398942, 9.394211990193552353 ) ) ;
#22272 = ORIENTED_EDGE ( 'NONE', *, *, #58090, .F. ) ;
#22273 = CARTESIAN_POINT ( 'NONE',  ( 7.083715465317824922, -78.28195011990158036, -8.166873904374831739 ) ) ;
#22274 = CARTESIAN_POINT ( 'NONE',  ( -1.301498323113999822, -79.03504199407001352, -12.14058299385000161 ) ) ;
#22275 = VERTEX_POINT ( 'NONE', #42484 ) ;
#22276 = ORIENTED_EDGE ( 'NONE', *, *, #13019, .T. ) ;
#22277 = CARTESIAN_POINT ( 'NONE',  ( -0.9820397338569999413, -80.70308451575900222, -0.7733679338621000099 ) ) ;
#22278 = AXIS2_PLACEMENT_3D ( 'NONE', #58397, #32102, #49554 ) ;
#22279 = CARTESIAN_POINT ( 'NONE',  ( 0.9336649615752000697, -80.45237540023499889, -0.9522845488933000535 ) ) ;
#22280 = CARTESIAN_POINT ( 'NONE',  ( -5.681372509047000641, -78.28477434195299622, -7.867192369580999767 ) ) ;
#22281 = CARTESIAN_POINT ( 'NONE',  ( 2.689222434189590061, -86.17851881763698429, -3.776835788994612475 ) ) ;
#22282 = CARTESIAN_POINT ( 'NONE',  ( 2.452186592920638120, -85.87062192719187692, 2.534882777327113867 ) ) ;
#22283 = AXIS2_PLACEMENT_3D ( 'NONE', #8434, #32028, #18475 ) ;
#22284 = CONICAL_SURFACE ( 'NONE', #41134, 12.84999999993999964, 0.7853981633972997312 ) ;
#22285 = CARTESIAN_POINT ( 'NONE',  ( 5.554616340558999887, -77.67073543972999516, 11.53062854294000061 ) ) ;
#22286 = ADVANCED_FACE ( 'NONE', ( #5869 ), #41892, .F. ) ;
#22287 = CARTESIAN_POINT ( 'NONE',  ( -0.5136231202413000796, -80.98605406588998790, 1.249846006485000105 ) ) ;
#22288 = CARTESIAN_POINT ( 'NONE',  ( -1.910682550011000291, -76.63754856920999714, -10.71539657768000176 ) ) ;
#22289 = CIRCLE ( 'NONE', #43082, 0.5000000000000004441 ) ;
#22290 = CARTESIAN_POINT ( 'NONE',  ( -5.088691759813757095E-08, -76.94999999999998863, -9.499908983443795307 ) ) ;
#22291 = CARTESIAN_POINT ( 'NONE',  ( 3.894762958177000023, -81.21931966961800242, 1.374530897864000067 ) ) ;
#22292 = CARTESIAN_POINT ( 'NONE',  ( -10.24996238027999951, -58.55171076491000548, 7.705119999413000187 ) ) ;
#22293 = CARTESIAN_POINT ( 'NONE',  ( 3.262409307125078595, -76.84669750786996190, -11.36051482961531001 ) ) ;
#22294 = CARTESIAN_POINT ( 'NONE',  ( -1.208787279847999940, -81.80467549782599690, -3.379731224302000125 ) ) ;
#22295 = CARTESIAN_POINT ( 'NONE',  ( 10.76566337430111275, -77.51291972185832435, -5.417667412981278297 ) ) ;
#22296 = CARTESIAN_POINT ( 'NONE',  ( -0.9849936891751999157, -81.01971605282150790, -11.22225356808999841 ) ) ;
#22297 = EDGE_CURVE ( 'NONE', #2251, #16536, #52829, .T. ) ;
#22298 = CARTESIAN_POINT ( 'NONE',  ( -2.963791440107999886, -3.228697272162000420, 2.387889716789000083 ) ) ;
#22299 = CARTESIAN_POINT ( 'NONE',  ( -1.258250795308458070, -80.26263457026050219, -0.2016572651531162164 ) ) ;
#22300 = ORIENTED_EDGE ( 'NONE', *, *, #11460, .T. ) ;
#22301 = CARTESIAN_POINT ( 'NONE',  ( 11.00000000000000000, -78.44999999999998863, 0.000000000000000000 ) ) ;
#22302 = EDGE_CURVE ( 'NONE', #25015, #11513, #15609, .T. ) ;
#22303 = CARTESIAN_POINT ( 'NONE',  ( 5.865376297750809157E-14, -72.79999999999999716, 13.89999999999999858 ) ) ;
#22304 = CARTESIAN_POINT ( 'NONE',  ( -1.127489577578000057, -80.71720420293900133, -0.5989559841152000130 ) ) ;
#22305 = CARTESIAN_POINT ( 'NONE',  ( -2.178743964827522639, -79.00666666666666060, -9.280974303042503593 ) ) ;
#22306 = CARTESIAN_POINT ( 'NONE',  ( -3.129814719915999799, -78.37698894087999690, 12.62985940900000159 ) ) ;
#22307 = CARTESIAN_POINT ( 'NONE',  ( 5.728183583606999640, -79.68258667140098339, -7.739857582846999762 ) ) ;
#22308 = CARTESIAN_POINT ( 'NONE',  ( 12.69619287811000063, -21.75083378359999742, -1.799475295154000065 ) ) ;
#22309 = EDGE_LOOP ( 'NONE', ( #47716, #58190, #815, #19203 ) ) ;
#22310 = CARTESIAN_POINT ( 'NONE',  ( -8.813891479040833588, -25.01010130368336348, -8.872963530600353366 ) ) ;
#22311 = CARTESIAN_POINT ( 'NONE',  ( -10.73206714754000046, -77.15440972681939513, 3.453790258818999703 ) ) ;
#22312 = CARTESIAN_POINT ( 'NONE',  ( 0.8666632585819999957, -81.42443521981201116, -0.9832170324100000247 ) ) ;
#22313 = CARTESIAN_POINT ( 'NONE',  ( 7.640030139758000161, -18.69283065396999888, -10.18491068059999805 ) ) ;
#22314 = CARTESIAN_POINT ( 'NONE',  ( 1.459128634122999868, -77.59418023959399591, -9.409639786240999726 ) ) ;
#22316 = CARTESIAN_POINT ( 'NONE',  ( 2.627446458840999810, -1.635584759237999952, 3.037392460054000320 ) ) ;
#22315 = CARTESIAN_POINT ( 'NONE',  ( -4.095405198877999808, -84.54268354761398996, -0.5349483391501999030 ) ) ;
#22317 = CARTESIAN_POINT ( 'NONE',  ( -1.931043762602999925, -56.02180874340999850, -12.75761570867999950 ) ) ;
#22318 = CARTESIAN_POINT ( 'NONE',  ( 0.2296925013217000211, -80.18441590662199303, -1.498727297740999775 ) ) ;
#22319 = ADVANCED_FACE ( 'NONE', ( #51927 ), #12049, .F. ) ;
#22320 = ORIENTED_EDGE ( 'NONE', *, *, #10858, .F. ) ;
#22321 = CIRCLE ( 'NONE', #54369, 1.749999999999998890 ) ;
#22322 = CARTESIAN_POINT ( 'NONE',  ( -2.739655911418338530, -77.20466484327231171, -10.39613826528414364 ) ) ;
#22323 = CARTESIAN_POINT ( 'NONE',  ( 1.460959015002474493, -79.12916666666669130, -0.3926218265389176953 ) ) ;
#22324 = CARTESIAN_POINT ( 'NONE',  ( 3.548349909811001179, -78.96264282632948550, 7.096699819622030780 ) ) ;
#22325 = ORIENTED_EDGE ( 'NONE', *, *, #11767, .T. ) ;
#22326 = AXIS2_PLACEMENT_3D ( 'NONE', #51806, #6629, #24637 ) ;
#22327 = ORIENTED_EDGE ( 'NONE', *, *, #35924, .T. ) ;
#22328 = CARTESIAN_POINT ( 'NONE',  ( 11.77452260639999970, -79.96011154630718920, 1.259536412044000020 ) ) ;
#22329 = DIRECTION ( 'NONE',  ( -1.000000000000000000, 7.077902766859999560E-11, 7.077871680614999346E-11 ) ) ;
#22330 = DIRECTION ( 'NONE',  ( 0.000000000000000000, 0.000000000000000000, -1.000000000000000000 ) ) ;
#22331 = AXIS2_PLACEMENT_3D ( 'NONE', #5231, #36514, #45691 ) ;
#22332 = EDGE_LOOP ( 'NONE', ( #29736, #31461, #15353, #4299 ) ) ;
#22333 = CARTESIAN_POINT ( 'NONE',  ( 11.77424395174999994, -78.45818512137599043, 2.561825723684000078 ) ) ;
#22334 = VECTOR ( 'NONE', #3541, 1000.000000000000000 ) ;
#22335 = ORIENTED_EDGE ( 'NONE', *, *, #48851, .T. ) ;
#22336 = ORIENTED_EDGE ( 'NONE', *, *, #7254, .F. ) ;
#22337 = CARTESIAN_POINT ( 'NONE',  ( 7.553727747492950506, -60.48581381148435554, 7.997114030238977378 ) ) ;
#22338 = CARTESIAN_POINT ( 'NONE',  ( 11.92322513370752191, -76.63885875642324663, -1.571131804317056568 ) ) ;
#22339 = CARTESIAN_POINT ( 'NONE',  ( 8.944729675425000082, -80.03290621929455995, 3.923329690209000908 ) ) ;
#22340 = ORIENTED_EDGE ( 'NONE', *, *, #2907, .T. ) ;
#22341 = DIRECTION ( 'NONE',  ( 0.7071067811865474617, 0.000000000000000000, -0.7071067811865474617 ) ) ;
#22342 = ORIENTED_EDGE ( 'NONE', *, *, #15656, .F. ) ;
#22343 = CARTESIAN_POINT ( 'NONE',  ( -1.203536965665374270, -80.62357710649452258, 0.4181554378093583768 ) ) ;
#22344 = CARTESIAN_POINT ( 'NONE',  ( -3.992195106911536673, -78.77851881763731967, 0.07526069398394277798 ) ) ;
#22345 = CYLINDRICAL_SURFACE ( 'NONE', #7622, 1.750000000000001332 ) ;
#22346 = CARTESIAN_POINT ( 'NONE',  ( -7.627487606607999737, -18.70221404512000163, -10.35845616727999996 ) ) ;
#22347 = CARTESIAN_POINT ( 'NONE',  ( 8.250583883964464960, -79.55729166666260710, 4.756314483000303461 ) ) ;
#22348 = EDGE_CURVE ( 'NONE', #55096, #11974, #29174, .T. ) ;
#22349 = CARTESIAN_POINT ( 'NONE',  ( -1.405334848770694034, -54.48507051970170068, 12.50716844827185348 ) ) ;
#22350 = CARTESIAN_POINT ( 'NONE',  ( 7.678690995210999404, -58.55648180022999583, -10.59551070212999946 ) ) ;
#22351 = LINE ( 'NONE', #39770, #29362 ) ;
#22352 = EDGE_CURVE ( 'NONE', #39723, #17474, #15900, .T. ) ;
#22353 = DIRECTION ( 'NONE',  ( 0.000000000000000000, -1.000000000000000000, 0.000000000000000000 ) ) ;
#22354 = CARTESIAN_POINT ( 'NONE',  ( -1.178447680628000205, -80.55308451575899653, -0.9280415206345000723 ) ) ;
#22355 = CARTESIAN_POINT ( 'NONE',  ( 1.439896632895286466, -78.46458333333332291, 11.00000000000000711 ) ) ;
#22356 = TOROIDAL_SURFACE ( 'NONE', #706, 9.799999999999998934, 0.2000000000000000111 ) ;
#22357 = CARTESIAN_POINT ( 'NONE',  ( 3.277247998812000240, -80.73400264934798543, -2.586357541886000089 ) ) ;
#22358 = CARTESIAN_POINT ( 'NONE',  ( 8.737261393354000205, -77.04368667140099092, 4.355473623822999407 ) ) ;
#22359 = CARTESIAN_POINT ( 'NONE',  ( -12.43647099681000157, -17.08193128089000012, -0.03491583288330000340 ) ) ;
#22360 = CARTESIAN_POINT ( 'NONE',  ( 10.45205659049000069, -19.23767314807999895, -7.651160337241000420 ) ) ;
#22361 = CARTESIAN_POINT ( 'NONE',  ( 1.288488638074000159, -24.53564939367999997, 12.54709296483000003 ) ) ;
#22362 = CARTESIAN_POINT ( 'NONE',  ( -8.137215171344100995, -60.25155696365447255, -7.401770473314702059 ) ) ;
#22363 = CARTESIAN_POINT ( 'NONE',  ( -1.454020682123249530, -80.00000000000000000, 9.185157777585660099 ) ) ;
#22364 = CARTESIAN_POINT ( 'NONE',  ( -3.095372243593999873, -1.512137290291999836, 1.882642529173000012 ) ) ;
#22365 = CARTESIAN_POINT ( 'NONE',  ( 9.539544502573999551, -79.40450095943377562, 0.5400218831817873433 ) ) ;
#22366 = ADVANCED_FACE ( 'NONE', ( #48083 ), #25614, .F. ) ;
#22367 = VECTOR ( 'NONE', #52984, 1000.000000000000000 ) ;
#22368 = CARTESIAN_POINT ( 'NONE',  ( -1.511213184804566678, -80.84932130686019036, -0.0005575924518816717133 ) ) ;
#22369 = CARTESIAN_POINT ( 'NONE',  ( 12.43410103870000150, -61.24137177736000126, -1.192638008239000014 ) ) ;
#22370 = CARTESIAN_POINT ( 'NONE',  ( -1.431457626485999945, -78.86977915405600470, 0.7470896798747000966 ) ) ;
#22371 = CONICAL_SURFACE ( 'NONE', #19566, 2.399999999383999771, 0.7853981633972997312 ) ;
#22372 = FACE_BOUND ( 'NONE', #9867, .T. ) ;
#22373 = CARTESIAN_POINT ( 'NONE',  ( 2.897215155706000189, -77.67296592294499646, -10.52527958449999979 ) ) ;
#22374 = CARTESIAN_POINT ( 'NONE',  ( -12.11185258877999971, -77.44856428951000282, -1.133824260204999934 ) ) ;
#22375 = FACE_OUTER_BOUND ( 'NONE', #6152, .T. ) ;
#22376 = AXIS2_PLACEMENT_3D ( 'NONE', #42188, #37747, #15016 ) ;
#22377 = CARTESIAN_POINT ( 'NONE',  ( 2.813789756862274505, -79.14583333333331439, -10.47020627418438821 ) ) ;
#22379 = CARTESIAN_POINT ( 'NONE',  ( -0.2558648464975999959, -78.90787364874299215, -1.394486488214999875 ) ) ;
#22378 = CARTESIAN_POINT ( 'NONE',  ( -11.00000000000000000, -78.19999999999998863, 0.000000000000000000 ) ) ;
#22380 = ORIENTED_EDGE ( 'NONE', *, *, #24024, .F. ) ;
#22381 = CARTESIAN_POINT ( 'NONE',  ( 2.727581927295000153, -84.07371544543099162, -2.582955461952999965 ) ) ;
#22382 = CARTESIAN_POINT ( 'NONE',  ( -8.708695699441999949, -79.68326480666600276, -8.148281476810998569 ) ) ;
#22383 = CARTESIAN_POINT ( 'NONE',  ( -5.726205896150999841, -80.22331365663170288, -9.593452009017001458 ) ) ;
#22384 = CARTESIAN_POINT ( 'NONE',  ( 0.000000000000000000, -73.00000000000001421, 0.000000000000000000 ) ) ;
#22385 = CARTESIAN_POINT ( 'NONE',  ( 0.000000000000000000, -87.25000000009099210, 0.000000000000000000 ) ) ;
#22386 = CARTESIAN_POINT ( 'NONE',  ( -9.302864017704999711, -76.88107005692299367, -6.266965030821000759 ) ) ;
#22387 = CARTESIAN_POINT ( 'NONE',  ( -9.788011744299998540, -61.32881292732000134, 7.956359616248999345 ) ) ;
#22388 = CARTESIAN_POINT ( 'NONE',  ( 0.000000000000000000, -55.54999999966999980, 12.00000000000000000 ) ) ;
#22389 = CARTESIAN_POINT ( 'NONE',  ( -3.476885736642000069, -0.7853606339641999723, 0.9048613863073000640 ) ) ;
#22390 = CARTESIAN_POINT ( 'NONE',  ( -10.71931710301092266, -76.33463918441997009, -4.979328733251163541 ) ) ;
#22391 = CARTESIAN_POINT ( 'NONE',  ( 12.43356840162999966, -24.71269674488000234, -0.8410229959428999758 ) ) ;
#22392 = CARTESIAN_POINT ( 'NONE',  ( -1.930989179114000143, -58.55453807205000061, 12.80896991324999945 ) ) ;
#22393 = VERTEX_POINT ( 'NONE', #38041 ) ;
#22394 = CARTESIAN_POINT ( 'NONE',  ( 0.7833523767573993268, -80.66795188156623908, -1.316067733153899688 ) ) ;
#22395 = CARTESIAN_POINT ( 'NONE',  ( -8.658543215228000633, -79.65891332859899876, 3.968578621617999680 ) ) ;
#22396 = CARTESIAN_POINT ( 'NONE',  ( 10.75000000000000000, -80.84999999999999432, -1.053639850055999980E-14 ) ) ;
#22397 = CARTESIAN_POINT ( 'NONE',  ( -0.8906226101088000613, -79.46323634664999247, -1.206976125017999779 ) ) ;
#22398 = CARTESIAN_POINT ( 'NONE',  ( -12.75761570869000039, -59.57819125629999490, -1.931043762602999925 ) ) ;
#22399 = EDGE_LOOP ( 'NONE', ( #53870, #50560, #36642, #40832, #48003 ) ) ;
#22400 = CARTESIAN_POINT ( 'NONE',  ( -9.599999999916001059, -90.40000000008399184, 6.531558194539000517E-10 ) ) ;
#22401 = CARTESIAN_POINT ( 'NONE',  ( 10.26605847043819075, -77.90552223423264877, -5.914160144501205529 ) ) ;
#22402 = CARTESIAN_POINT ( 'NONE',  ( 3.250000000000000000, -1.250000000000000000, 0.000000000000000000 ) ) ;
#22403 = ORIENTED_EDGE ( 'NONE', *, *, #49041, .T. ) ;
#22404 = EDGE_CURVE ( 'NONE', #40525, #2165, #43755, .T. ) ;
#22405 = ORIENTED_EDGE ( 'NONE', *, *, #48848, .F. ) ;
#22406 = CARTESIAN_POINT ( 'NONE',  ( -9.213130513665999999, -53.79475660653999824, -8.533779407502999348 ) ) ;
#22407 = FILL_AREA_STYLE_COLOUR ( '', #47341 ) ;
#22408 = CARTESIAN_POINT ( 'NONE',  ( -7.545891804452000251, -79.77540805456798978, 6.201630566990999682 ) ) ;
#22409 = ORIENTED_EDGE ( 'NONE', *, *, #3204, .F. ) ;
#22410 = VECTOR ( 'NONE', #31397, 1000.000000000000000 ) ;
#22411 = ORIENTED_EDGE ( 'NONE', *, *, #50295, .F. ) ;
#22412 = CARTESIAN_POINT ( 'NONE',  ( 11.09583276434000076, -76.40801663978099612, 5.154565694333999915 ) ) ;
#22413 = CARTESIAN_POINT ( 'NONE',  ( -0.2078880262912795873, -79.31385681300682222, -1.400979628114630060 ) ) ;
#22414 = CARTESIAN_POINT ( 'NONE',  ( -1.640079623176999846, -78.26202514954999856, 0.1643931535720999926 ) ) ;
#22415 = ORIENTED_EDGE ( 'NONE', *, *, #40204, .T. ) ;
#22416 = CARTESIAN_POINT ( 'NONE',  ( -4.342561293556999935, -77.65714805011499777, -8.443909622126001935 ) ) ;
#22417 = AXIS2_PLACEMENT_3D ( 'NONE', #56161, #15710, #47321 ) ;
#22418 = CARTESIAN_POINT ( 'NONE',  ( 0.7058627945297136774, -80.27327360843820259, -1.031809627508295302 ) ) ;
#22419 = CARTESIAN_POINT ( 'NONE',  ( 11.91901974179999968, -77.27860818038000446, 5.468333046474000980 ) ) ;
#22420 = CARTESIAN_POINT ( 'NONE',  ( 11.19180402071999936, -77.50532108250102681, 0.7494220128532999015 ) ) ;
#22421 = CARTESIAN_POINT ( 'NONE',  ( 1.356394222569207386, -86.17851879815597727, 3.125459129807984571 ) ) ;
#22422 = CARTESIAN_POINT ( 'NONE',  ( -4.019809786096000259, -79.30584983151099721, 10.47183077952999852 ) ) ;
#22423 = CARTESIAN_POINT ( 'NONE',  ( 8.230920277480567648, -79.88818024824762176, 4.220077749870753792 ) ) ;
#22424 = CARTESIAN_POINT ( 'NONE',  ( -5.016174693291526765, -80.03806740382935914, -9.911088353662746542 ) ) ;
#22425 = ORIENTED_EDGE ( 'NONE', *, *, #29942, .F. ) ;
#22426 = CARTESIAN_POINT ( 'NONE',  ( 0.000000000000000000, -0.6500000000000000222, 0.000000000000000000 ) ) ;
#22427 = EDGE_CURVE ( 'NONE', #38110, #5279, #44352, .T. ) ;
#22428 = CARTESIAN_POINT ( 'NONE',  ( -6.282410744257000523, -75.96962114363998353, 10.58616248715999930 ) ) ;
#22429 = CARTESIAN_POINT ( 'NONE',  ( 0.6980205241115000625, -80.24748354179199339, 1.456015547280999911 ) ) ;
#22430 = CARTESIAN_POINT ( 'NONE',  ( 0.6216730717741000278, -78.32210341376939766, -1.163652956044999964 ) ) ;
#22431 = CARTESIAN_POINT ( 'NONE',  ( 0.4088352756822764000, -2.714880510813482584, 3.556394378621883234 ) ) ;
#22432 = DIRECTION ( 'NONE',  ( 0.000000000000000000, 0.000000000000000000, -1.000000000000000000 ) ) ;
#22433 = CARTESIAN_POINT ( 'NONE',  ( -0.6669403506045999963, -76.32235911309500409, -12.26286337364000012 ) ) ;
#22434 = DIRECTION ( 'NONE',  ( -0.7026410690473252618, -0.1122098755728027641, 0.7026410690473252618 ) ) ;
#22435 = CARTESIAN_POINT ( 'NONE',  ( 4.927379535269999167, -77.61086332859899528, -8.272319949952999352 ) ) ;
#22436 = CARTESIAN_POINT ( 'NONE',  ( 10.65724243470759269, -77.26040116651306278, -5.779895665056474563 ) ) ;
#22437 = CARTESIAN_POINT ( 'NONE',  ( -1.250000000000000000, -83.09999999999999432, 0.000000000000000000 ) ) ;
#22438 = CARTESIAN_POINT ( 'NONE',  ( 7.910349975595998728, -79.56271253079168559, 7.952639426948999279 ) ) ;
#22439 = B_SPLINE_SURFACE_WITH_KNOTS ( 'NONE', 3, 3, ( 
 ( #1267, #5381, #14521, #27510 ),
 ( #54687, #41400, #1551, #55262 ),
 ( #19542, #10398, #37540, #23675 ),
 ( #19256, #32514, #14810, #50558 ),
 ( #23388, #15105, #28678, #46730 ),
 ( #10111, #28383, #36377, #46141 ),
 ( #32226, #54403, #10701, #32806 ),
 ( #24264, #37250, #33102, #42280 ) ),
 .UNSPECIFIED., .F., .F., .F.,
 ( 4, 1, 1, 1, 1, 4 ),
 ( 4, 4 ),
 ( -0.01200407345746999990, 0.000000000000000000, 0.3333333333333000081, 0.6666666666667000474, 1.000000000000000000, 1.011997855551999947 ),
 ( -0.3559705542741999906, 1.355970554273999928 ),
 .UNSPECIFIED. ) ;
#22440 = EDGE_CURVE ( 'NONE', #7885, #56550, #38092, .T. ) ;
#22441 = VERTEX_POINT ( 'NONE', #15513 ) ;
#22442 = CARTESIAN_POINT ( 'NONE',  ( 1.424157265477999923, -83.17957200447399657, 0.6972603243668999973 ) ) ;
#22443 = CARTESIAN_POINT ( 'NONE',  ( -12.57042253521000141, -52.69905023022000279, 0.000000000000000000 ) ) ;
#22444 = DIRECTION ( 'NONE',  ( -1.000000000000000000, 0.000000000000000000, 0.000000000000000000 ) ) ;
#22445 = CARTESIAN_POINT ( 'NONE',  ( 6.444980599754999595, -77.66852088434498569, -10.09843005143000028 ) ) ;
#22446 = CARTESIAN_POINT ( 'NONE',  ( 7.709155920968100872, -23.92747430419191090, 9.998700314111166776 ) ) ;
#22447 = CARTESIAN_POINT ( 'NONE',  ( -0.6811744818814000624, -82.36187082071000987, -1.520282978132999840 ) ) ;
#22448 = CARTESIAN_POINT ( 'NONE',  ( 3.237243043699999934, -78.72344966613400175, -11.48719983142999901 ) ) ;
#22449 = CARTESIAN_POINT ( 'NONE',  ( -9.631455446501000495, -78.08089805011499607, -1.333735528292999906 ) ) ;
#22450 = CARTESIAN_POINT ( 'NONE',  ( -9.108272167377998940, -77.16660918229489141, -2.776672910959999907 ) ) ;
#22451 = CARTESIAN_POINT ( 'NONE',  ( 9.199999999999999289, -76.00000000000000000, 0.000000000000000000 ) ) ;
#22452 = CARTESIAN_POINT ( 'NONE',  ( 4.507156365786499919, -76.04314103804109948, 10.85083221517958663 ) ) ;
#22453 = CARTESIAN_POINT ( 'NONE',  ( 10.21235917355000034, -80.24784788827008697, -3.857859667932999947 ) ) ;
#22454 = CARTESIAN_POINT ( 'NONE',  ( -8.485281374238999419, 0.000000000000000000, 8.485281374238999419 ) ) ;
#22455 = ORIENTED_EDGE ( 'NONE', *, *, #42244, .T. ) ;
#22456 = CARTESIAN_POINT ( 'NONE',  ( 6.055527902613000002, -78.11999999999999034, 7.319875806370000682 ) ) ;
#22457 = DIRECTION ( 'NONE',  ( 0.7026410690473252618, 0.1122098755728027641, -0.7026410690473252618 ) ) ;
#22458 = CARTESIAN_POINT ( 'NONE',  ( -1.807666384373000090, -79.87198619718679993, -12.02113240485999945 ) ) ;
#22459 = CARTESIAN_POINT ( 'NONE',  ( 3.778552491320999795, -78.40681307243319509, -2.230001151765018008 ) ) ;
#22460 = CARTESIAN_POINT ( 'NONE',  ( 3.303001513109999898, -79.07947657143998299, -10.46681410869999951 ) ) ;
#22461 = CARTESIAN_POINT ( 'NONE',  ( 10.99999999999999645, -79.33958333333332291, -1.439896632895355522 ) ) ;
#22462 = CARTESIAN_POINT ( 'NONE',  ( 10.20634188032000012, -76.21203981538700134, -6.810150128040000084 ) ) ;
#22463 = LINE ( 'NONE', #361, #23638 ) ;
#22464 = DIRECTION ( 'NONE',  ( 0.000000000000000000, 0.000000000000000000, -1.000000000000000000 ) ) ;
#22465 = ORIENTED_EDGE ( 'NONE', *, *, #54547, .F. ) ;
#22466 = CARTESIAN_POINT ( 'NONE',  ( -7.362671760698999535, -79.27644859181400250, -8.369328833011000057 ) ) ;
#22467 = CARTESIAN_POINT ( 'NONE',  ( 0.9312054229806641104, -79.90880812854101123, 0.8360461126382245922 ) ) ;
#22468 = VECTOR ( 'NONE', #31570, 1000.000000000000000 ) ;
#22469 = CARTESIAN_POINT ( 'NONE',  ( 8.424622201753786399, -75.79999999999998295, -8.402754719800665129 ) ) ;
#22471 = CARTESIAN_POINT ( 'NONE',  ( 8.305672835130092579, -76.38744052775911086, -8.311290054389553816 ) ) ;
#22470 = CARTESIAN_POINT ( 'NONE',  ( -1.115376533724000030, -80.69714874331999965, -0.5925211750962999790 ) ) ;
#22472 = B_SPLINE_CURVE_WITH_KNOTS ( 'NONE', 3,
 ( #31601, #57900, #8310, #49644 ),
 .UNSPECIFIED., .F., .F.,
 ( 4, 4 ),
 ( 0.000000000000000000, 1.000000000000000000 ),
 .UNSPECIFIED. ) ;
#22473 = CARTESIAN_POINT ( 'NONE',  ( 9.088959790636000236, -78.01048704979598369, -6.010253266999000310 ) ) ;
#22474 = CARTESIAN_POINT ( 'NONE',  ( -7.229432123683867673, -76.43333333333332291, 8.035240866938302418 ) ) ;
#22475 = CARTESIAN_POINT ( 'NONE',  ( 0.08826574687577952438, -81.71975954240951978, 1.508524260310913689 ) ) ;
#22476 = CARTESIAN_POINT ( 'NONE',  ( 0.9868626873424000134, -78.45799267308299818, -12.24017488508000007 ) ) ;
#22477 = ADVANCED_FACE ( 'NONE', ( #19650 ), #2550, .T. ) ;
#22478 = CARTESIAN_POINT ( 'NONE',  ( -9.250000000000007105, -79.98958333333334281, 1.210822168571027868 ) ) ;
#22479 = ADVANCED_FACE ( 'NONE', ( #51544 ), #47126, .F. ) ;
#22480 = CARTESIAN_POINT ( 'NONE',  ( -8.861449449424648961, -79.64887384436650564, 6.625956105248707928 ) ) ;
#22481 =( NAMED_UNIT ( * ) PLANE_ANGLE_UNIT ( ) SI_UNIT ( $, .RADIAN. ) );
#22482 = DIRECTION ( 'NONE',  ( 0.7071067811865475727, 0.000000000000000000, 0.7071067811865475727 ) ) ;
#22483 = EDGE_LOOP ( 'NONE', ( #50900, #51266, #38025, #6195 ) ) ;
#22484 = ORIENTED_EDGE ( 'NONE', *, *, #13739, .F. ) ;
#22485 = DIRECTION ( 'NONE',  ( 0.000000000000000000, -1.000000000000000000, 0.000000000000000000 ) ) ;
#22486 = CARTESIAN_POINT ( 'NONE',  ( 6.722129540286000626, -77.31653998579800202, -6.773005240843000152 ) ) ;
#22487 = VERTEX_POINT ( 'NONE', #5773 ) ;
#22488 = CARTESIAN_POINT ( 'NONE',  ( 8.926771828799410002, -79.52861684990361368, 3.353330014368605561 ) ) ;
#22489 = VERTEX_POINT ( 'NONE', #33508 ) ;
#22490 = CARTESIAN_POINT ( 'NONE',  ( 7.943805570349000256, -24.43402324524999969, 9.641149735076000482 ) ) ;
#22491 = CIRCLE ( 'NONE', #33820, 4.799999999999999822 ) ;
#22492 = B_SPLINE_CURVE_WITH_KNOTS ( 'NONE', 3,
 ( #56864, #53009, #48307, #49163, #34407, #3141 ),
 .UNSPECIFIED., .F., .F.,
 ( 4, 1, 1, 4 ),
 ( 0.000000000000000000, 0.3333333333333000081, 0.6666666666667000474, 1.000000000000000000 ),
 .UNSPECIFIED. ) ;
#22493 = CARTESIAN_POINT ( 'NONE',  ( -8.082524092276882399, -79.54166666666665719, -4.658475568430820779 ) ) ;
#22494 = CARTESIAN_POINT ( 'NONE',  ( 0.9057247795391590861, -82.41316108956780795, 0.9056628583376803432 ) ) ;
#22495 = CARTESIAN_POINT ( 'NONE',  ( -9.250000000000000000, -78.09999999999999432, 0.000000000000000000 ) ) ;
#22496 = CARTESIAN_POINT ( 'NONE',  ( -0.2721098858049000313, -79.07524782868000557, 11.21356619464000026 ) ) ;
#22497 = CARTESIAN_POINT ( 'NONE',  ( 3.938458446976999205, -79.21000000000000796, -8.369650235310999165 ) ) ;
#22498 = ORIENTED_EDGE ( 'NONE', *, *, #44185, .F. ) ;
#22499 = VERTEX_POINT ( 'NONE', #50956 ) ;
#22500 = EDGE_CURVE ( 'NONE', #3819, #21753, #37356, .T. ) ;
#22501 = CARTESIAN_POINT ( 'NONE',  ( 6.073699447519306460, -77.41819971103011255, 6.993117814290229717 ) ) ;
#22502 = CARTESIAN_POINT ( 'NONE',  ( -0.5413127449341000874, -77.99094517446199859, -11.02683867434999954 ) ) ;
#22503 = B_SPLINE_CURVE_WITH_KNOTS ( 'NONE', 3,
 ( #32481, #45811, #660, #15071, #14487, #23355 ),
 .UNSPECIFIED., .F., .F.,
 ( 4, 1, 1, 4 ),
 ( 0.000000000000000000, 0.3333333333333000081, 0.6666666666667000474, 1.000000000000000000 ),
 .UNSPECIFIED. ) ;
#22504 = DIRECTION ( 'NONE',  ( 0.000000000000000000, 1.000000000000000000, 0.000000000000000000 ) ) ;
#22505 = CARTESIAN_POINT ( 'NONE',  ( 9.662203867310999783, -79.14785501805998535, 0.9012207007054000574 ) ) ;
#22506 = CARTESIAN_POINT ( 'NONE',  ( -12.80820168571000117, -75.83158071878000328, -0.01956446631054999802 ) ) ;
#22507 = AXIS2_PLACEMENT_3D ( 'NONE', #33390, #51427, #10983 ) ;
#22508 = CARTESIAN_POINT ( 'NONE',  ( -6.729900695599003946, -79.46213953550058307, -6.704927793111417955 ) ) ;
#22509 = CARTESIAN_POINT ( 'NONE',  ( 12.80088938724999892, -59.56256651724000051, 1.980532758767000301 ) ) ;
#22510 = CARTESIAN_POINT ( 'NONE',  ( -3.692575783495599673, -79.39408385515501720, -8.790537166344741138 ) ) ;
#22511 = CARTESIAN_POINT ( 'NONE',  ( 12.68702648026999924, -18.24922088193000036, -1.889939500033999797 ) ) ;
#22512 = CARTESIAN_POINT ( 'NONE',  ( -11.61705142569443794, -76.68723828451983593, 1.824568759944894536 ) ) ;
#22513 = EDGE_CURVE ( 'NONE', #50534, #54581, #19808, .T. ) ;
#22514 = CARTESIAN_POINT ( 'NONE',  ( 3.170431021627999613, -82.37817607281098731, 1.682935794284000197 ) ) ;
#22515 = EDGE_LOOP ( 'NONE', ( #42480, #25307, #20249, #8832, #53564 ) ) ;
#22516 = CARTESIAN_POINT ( 'NONE',  ( -3.843694318990999559, -79.27341986734299439, 11.82438401172999853 ) ) ;
#22517 = CARTESIAN_POINT ( 'NONE',  ( 1.582175077527999907, -76.41246662722099359, -11.50424973215999991 ) ) ;
#22518 = CARTESIAN_POINT ( 'NONE',  ( -6.074904069602191647, -78.02296353543388818, 8.868935607531122756 ) ) ;
#22519 = EDGE_CURVE ( 'NONE', #24789, #12731, #56280, .T. ) ;
#22520 = CARTESIAN_POINT ( 'NONE',  ( -4.743879332790999825, -78.72649471530600351, -11.00053059214000051 ) ) ;
#22521 = CARTESIAN_POINT ( 'NONE',  ( -10.18948933931999967, -18.78467389927000042, 7.645397892297999931 ) ) ;
#22523 = CARTESIAN_POINT ( 'NONE',  ( 0.000000000000000000, -23.15000000000000213, 11.89999999977000122 ) ) ;
#22522 = CARTESIAN_POINT ( 'NONE',  ( 10.52982398497215577, -78.27927571967974529, -2.879177815852805633 ) ) ;
#22524 = CARTESIAN_POINT ( 'NONE',  ( 3.654181830570000233, -86.09999999999999432, -1.626946572303000105 ) ) ;
#22525 = CARTESIAN_POINT ( 'NONE',  ( -8.263041386619001116, -80.49726512904899778, 7.695848569717000487 ) ) ;
#22526 = CARTESIAN_POINT ( 'NONE',  ( 1.243547092045970581, -78.43541666666664014, -9.500000000000000000 ) ) ;
#22527 = CARTESIAN_POINT ( 'NONE',  ( 6.393694643109999909, -77.56474813712100058, -9.131005934809000024 ) ) ;
#22528 = CARTESIAN_POINT ( 'NONE',  ( -3.165411199172029288, -1.979166666666666297, 0.8506806241676482250 ) ) ;
#22529 = CARTESIAN_POINT ( 'NONE',  ( 7.370453364210000302, -80.64212683706639950, -8.200218203919000359 ) ) ;
#22530 = ORIENTED_EDGE ( 'NONE', *, *, #3397, .F. ) ;
#22531 = DIRECTION ( 'NONE',  ( 0.9999548435846228323, 0.000000000000000000, 0.009503199022040218977 ) ) ;
#22532 = CARTESIAN_POINT ( 'NONE',  ( 0.005928781627640000024, -53.59886949703999903, 12.66336824414000084 ) ) ;
#22533 = CARTESIAN_POINT ( 'NONE',  ( -1.666698456695999919, -59.99181739808000202, -12.50018138922999889 ) ) ;
#22534 = CARTESIAN_POINT ( 'NONE',  ( 3.504303451278000026, -2.516831454374000021, -1.857678891402000154 ) ) ;
#22535 = CIRCLE ( 'NONE', #14984, 0.5000000000000006661 ) ;
#22536 = CARTESIAN_POINT ( 'NONE',  ( -0.8253947190445000137, -77.31745615340899747, -11.18645762290999990 ) ) ;
#22537 = DIRECTION ( 'NONE',  ( 0.000000000000000000, -0.7071067811866525998, -0.7071067811864425456 ) ) ;
#22538 = CARTESIAN_POINT ( 'NONE',  ( -2.598917237794085455, -1.552083333333333037, -1.997276839918474600 ) ) ;
#22539 = CARTESIAN_POINT ( 'NONE',  ( -4.000000000000000000, -5.200000000000000178, 0.5999999999999999778 ) ) ;
#22540 = CARTESIAN_POINT ( 'NONE',  ( -0.9212224518285999642, -61.61954101805999784, 12.54670315985999984 ) ) ;
#22541 = CARTESIAN_POINT ( 'NONE',  ( 12.83836748062999966, -18.79372227161000097, 2.062147040910000229 ) ) ;
#22542 = CARTESIAN_POINT ( 'NONE',  ( -3.364651624423000253, -84.90774735065198797, -2.471582332770999813 ) ) ;
#22544 = ADVANCED_FACE ( 'NONE', ( #46542 ), #50640, .F. ) ;
#22543 = AXIS2_PLACEMENT_3D ( 'NONE', #3282, #34263, #7987 ) ;
#22545 = CARTESIAN_POINT ( 'NONE',  ( -3.630949683904999947, -76.04999999999999716, 11.17491406647000041 ) ) ;
#22546 = CARTESIAN_POINT ( 'NONE',  ( -8.908963061728000454, -79.23128271215000495, -8.963338373884001342 ) ) ;
#22547 = CARTESIAN_POINT ( 'NONE',  ( -9.465408641230000697, -77.16458445751899831, 5.887328751257999926 ) ) ;
#22548 = CARTESIAN_POINT ( 'NONE',  ( -0.7048934085577001074, -80.86062486154999362, -1.509431780672999990 ) ) ;
#22549 = CARTESIAN_POINT ( 'NONE',  ( 0.3813430617698000402, -79.10306886790999670, -1.382988530009999995 ) ) ;
#22550 = CARTESIAN_POINT ( 'NONE',  ( -1.501534314757656308, -61.35152951622679041, 12.70455943744299354 ) ) ;
#22551 = CARTESIAN_POINT ( 'NONE',  ( -0.5530976515504120172, -82.84513323647280458, -1.407674718852016227 ) ) ;
#22552 = DIRECTION ( 'NONE',  ( -1.000000000000000000, 0.000000000000000000, 0.000000000000000000 ) ) ;
#22553 = CARTESIAN_POINT ( 'NONE',  ( 0.000000000000000000, -33.10361340872000113, 0.000000000000000000 ) ) ;
#22554 = CARTESIAN_POINT ( 'NONE',  ( 1.407171709420440342, -77.13541666666665719, -10.74999999999999822 ) ) ;
#22555 = CARTESIAN_POINT ( 'NONE',  ( 6.766496333857535461, -79.52643867575977765, -8.946291764058088347 ) ) ;
#22556 = VECTOR ( 'NONE', #55470, 1000.000000000000000 ) ;
#22557 = EDGE_CURVE ( 'NONE', #19958, #48994, #6358, .T. ) ;
#22558 = DIRECTION ( 'NONE',  ( -1.000000000000000000, 0.000000000000000000, 0.000000000000000000 ) ) ;
#22559 = CARTESIAN_POINT ( 'NONE',  ( -1.439896632895332207, -79.48541666666665151, 10.99999999999999822 ) ) ;
#22560 = CARTESIAN_POINT ( 'NONE',  ( 6.724228645090999379, -79.56766689940799608, -8.890407735272999545 ) ) ;
#22561 = CARTESIAN_POINT ( 'NONE',  ( 8.838834764832000701, -23.25000000000000000, -8.838834764832000701 ) ) ;
#22562 = EDGE_LOOP ( 'NONE', ( #45241, #25671, #10676, #20884 ) ) ;
#22563 = VERTEX_POINT ( 'NONE', #37652 ) ;
#22564 = CARTESIAN_POINT ( 'NONE',  ( -0.9343553003753000130, -80.61948045011800446, -1.194030576736000215 ) ) ;
#22565 = ORIENTED_EDGE ( 'NONE', *, *, #9953, .T. ) ;
#22566 = CARTESIAN_POINT ( 'NONE',  ( -1.750000000000000000, -60.04999999966999980, -12.00000000000000000 ) ) ;
#22567 = ORIENTED_EDGE ( 'NONE', *, *, #7090, .F. ) ;
#22568 = DIRECTION ( 'NONE',  ( 0.000000000000000000, -1.000000000000000000, 0.000000000000000000 ) ) ;
#22569 = CARTESIAN_POINT ( 'NONE',  ( -9.254388464354001087, -79.80752053325198858, 5.469807505829999528 ) ) ;
#22570 = DIRECTION ( 'NONE',  ( 0.000000000000000000, -1.000000000000000000, 0.000000000000000000 ) ) ;
#22571 = CARTESIAN_POINT ( 'NONE',  ( 1.666727925315000025, -23.19174481776000007, -12.50018462903999961 ) ) ;
#22572 = CARTESIAN_POINT ( 'NONE',  ( 3.423420673917999757, -82.66232476339300206, 0.3453276880145999539 ) ) ;
#22573 = CARTESIAN_POINT ( 'NONE',  ( -9.292587090298047414, -79.38272904684014009, 1.999716160172516632 ) ) ;
#22574 = CARTESIAN_POINT ( 'NONE',  ( -9.050627908548998235, -77.39852255496806777, -6.322205650057998838 ) ) ;
#22575 = CARTESIAN_POINT ( 'NONE',  ( 10.24094026722000095, -79.20834499803000028, -6.917727457792000045 ) ) ;
#22576 = ORIENTED_EDGE ( 'NONE', *, *, #45487, .T. ) ;
#22577 = PRODUCT_DEFINITION_FORMATION_WITH_SPECIFIED_SOURCE ( 'ANY', '', #38457, .NOT_KNOWN. ) ;
#22578 = ORIENTED_EDGE ( 'NONE', *, *, #30223, .F. ) ;
#22579 = CARTESIAN_POINT ( 'NONE',  ( 14.00000000000000000, -0.2000000000000005107, 0.000000000000000000 ) ) ;
#22580 = CARTESIAN_POINT ( 'NONE',  ( -0.6211595220380999871, -80.84927638728399302, -1.084739991049000096 ) ) ;
#22581 = CARTESIAN_POINT ( 'NONE',  ( -7.456816947376000648, -78.65428412062898644, 6.210200510404999541 ) ) ;
#22582 = AXIS2_PLACEMENT_3D ( 'NONE', #12787, #22229, #44679 ) ;
#22583 = CARTESIAN_POINT ( 'NONE',  ( -3.808769407549206232, -86.09999999999979536, -2.658222959242663386 ) ) ;
#22584 = CARTESIAN_POINT ( 'NONE',  ( 3.243587544365338360, -85.82689775056601889, 1.505994140326985198 ) ) ;
#22585 = CARTESIAN_POINT ( 'NONE',  ( 12.45567317068999991, -78.14634877619000974, -3.566394712320999805 ) ) ;
#22586 = CARTESIAN_POINT ( 'NONE',  ( 5.621201030502000151, -78.17027720837999993, 11.49883638144000031 ) ) ;
#22587 = CARTESIAN_POINT ( 'NONE',  ( 7.362589990311000143, -76.14342849098198940, -7.926760118590000737 ) ) ;
#22588 = CARTESIAN_POINT ( 'NONE',  ( -2.935661446561999899, -76.94999999999998863, -9.035036904803998681 ) ) ;
#22589 = CARTESIAN_POINT ( 'NONE',  ( 1.940427222861999867, -79.89656500032499764, 3.645991759044000080 ) ) ;
#22591 = AXIS2_PLACEMENT_3D ( 'NONE', #54069, #13605, #49052 ) ;
#22590 = CARTESIAN_POINT ( 'NONE',  ( -8.418594644163000851, -80.89173212753800613, -7.485750452785000064 ) ) ;
#22592 = CYLINDRICAL_SURFACE ( 'NONE', #45009, 0.5000000000000006661 ) ;
#22593 = LINE ( 'NONE', #202, #42797 ) ;
#22594 = DIRECTION ( 'NONE',  ( 0.9999548435846228323, 0.000000000000000000, 0.009503199022040118363 ) ) ;
#22595 = TOROIDAL_SURFACE ( 'NONE', #38608, 1.250000000000000000, 0.5000000000000000000 ) ;
#22597 = CARTESIAN_POINT ( 'NONE',  ( -1.256362333281000110, -77.75166772233730228, 0.2270125678640999844 ) ) ;
#22596 = CARTESIAN_POINT ( 'NONE',  ( -1.250000000000000000, -82.49999999999998579, 0.000000000000000000 ) ) ;
#22598 = DIRECTION ( 'NONE',  ( 1.000000000000000000, 0.000000000000000000, 0.000000000000000000 ) ) ;
#22599 = CARTESIAN_POINT ( 'NONE',  ( -4.454457568640999732, -80.80903225079606500, 10.34731867136000005 ) ) ;
#22600 = CARTESIAN_POINT ( 'NONE',  ( -3.796701970596999764, -2.846418933659000228, 0.2667143827384000354 ) ) ;
#22601 = CARTESIAN_POINT ( 'NONE',  ( 1.041570653413430803, -80.54886380914602739, 0.7342313532027737732 ) ) ;
#22602 = VERTEX_POINT ( 'NONE', #6064 ) ;
#22603 = PLANE ( 'NONE',  #11256 ) ;
#22604 = CARTESIAN_POINT ( 'NONE',  ( -14.00000000000000000, -72.89999999999999147, 0.000000000000000000 ) ) ;
#22605 = CARTESIAN_POINT ( 'NONE',  ( -1.250000000000000000, -18.75000000000000000, -12.50000000000000000 ) ) ;
#22606 = CARTESIAN_POINT ( 'NONE',  ( 2.062502994258999856, -58.55648180022999583, 12.92181194095999963 ) ) ;
#22607 = CARTESIAN_POINT ( 'NONE',  ( -9.287618194362000423, -77.57908599310999875, -9.114789584104999065 ) ) ;
#22608 = EDGE_CURVE ( 'NONE', #29770, #24848, #6413, .T. ) ;
#22609 = FACE_OUTER_BOUND ( 'NONE', #42687, .T. ) ;
#22610 = CARTESIAN_POINT ( 'NONE',  ( 11.25874264225000054, -76.71236898706999341, -4.774966140054999642 ) ) ;
#22611 = B_SPLINE_CURVE_WITH_KNOTS ( 'NONE', 3,
 ( #49934, #27170, #9478, #1220, #23628, #32466, #49343, #935, #41640, #31889 ),
 .UNSPECIFIED., .F., .F.,
 ( 4, 2, 2, 2, 4 ),
 ( 0.000000000000000000, 0.2500000000000000555, 0.5000000000000001110, 0.7500000000000002220, 1.000000000000000000 ),
 .UNSPECIFIED. ) ;
#22612 = ORIENTED_EDGE ( 'NONE', *, *, #46449, .T. ) ;
#22613 = CARTESIAN_POINT ( 'NONE',  ( -12.50000000000000000, -63.73717104351998586, 0.000000000000000000 ) ) ;
#22614 = CARTESIAN_POINT ( 'NONE',  ( 9.102137319295220408, -53.82814024817236742, -8.583672456402702267 ) ) ;
#22615 = CARTESIAN_POINT ( 'NONE',  ( -0.5811420367779999152, -81.33038571333599975, -1.174774391002999963 ) ) ;
#22616 = CARTESIAN_POINT ( 'NONE',  ( -1.532229594827145380, -17.87701036866945259, 12.51228690880938110 ) ) ;
#22617 = CARTESIAN_POINT ( 'NONE',  ( 2.813750093493999849, -78.10580916391599260, -9.096877851405000825 ) ) ;
#22619 = CARTESIAN_POINT ( 'NONE',  ( -3.249661007175000282, -0.7327531080796000351, 2.357191814219000037 ) ) ;
#22618 = CARTESIAN_POINT ( 'NONE',  ( 1.276195428221999828, -84.06168188654598339, 3.928083336394000202 ) ) ;
#22620 = CARTESIAN_POINT ( 'NONE',  ( -1.799502287691000069, -60.10716680829000325, -12.60413670423000099 ) ) ;
#22621 = B_SPLINE_CURVE_WITH_KNOTS ( 'NONE', 3,
 ( #53787, #26899, #18064, #36057, #27185, #45225, #46110, #23934, #32196, #1522, #28943, #41952, #32484, #28650, #46986, #19515, #37510, #33372 ),
 .UNSPECIFIED., .F., .F.,
 ( 4, 2, 2, 2, 2, 2, 2, 2, 4 ),
 ( 0.000000000000000000, 0.1249999999999999722, 0.2499999999999999445, 0.3749999999999998890, 0.4999999999999998890, 0.6249999999999998890, 0.7499999999999997780, 0.8749999999999998890, 1.000000000000000000 ),
 .UNSPECIFIED. ) ;
#22622 = CARTESIAN_POINT ( 'NONE',  ( -1.137653363949000074, -79.48983917928698872, 1.002340751266999952 ) ) ;
#22623 = ORIENTED_EDGE ( 'NONE', *, *, #8089, .F. ) ;
#22624 = CARTESIAN_POINT ( 'NONE',  ( 0.2747012913232428910, -77.22714148007511881, -10.74666282699171838 ) ) ;
#22625 = DIRECTION ( 'NONE',  ( 0.000000000000000000, -1.000000000000000000, 0.000000000000000000 ) ) ;
#22626 = ORIENTED_EDGE ( 'NONE', *, *, #5557, .T. ) ;
#22628 = EDGE_CURVE ( 'NONE', #35471, #11586, #51570, .T. ) ;
#22627 = ORIENTED_EDGE ( 'NONE', *, *, #36437, .F. ) ;
#22629 = B_SPLINE_CURVE_WITH_KNOTS ( 'NONE', 3,
 ( #21507, #35061, #16510, #38933, #25930, #57235, #39222, #52809, #3790, #43957, #56951, #8505, #12648, #25357, #48676, #22077, #52522, #39796 ),
 .UNSPECIFIED., .F., .F.,
 ( 4, 2, 2, 2, 2, 2, 2, 2, 4 ),
 ( 0.000000000000000000, 0.1249999999999998890, 0.2499999999999998335, 0.3749999999999997780, 0.4999999999999997780, 0.6249999999999997780, 0.7499999999999997780, 0.8749999999999998890, 1.000000000000000000 ),
 .UNSPECIFIED. ) ;
#22630 = DIRECTION ( 'NONE',  ( -1.000000000000000000, 0.000000000000000000, 0.000000000000000000 ) ) ;
#22631 = DIRECTION ( 'NONE',  ( 1.000000000000000000, 0.000000000000000000, 0.000000000000000000 ) ) ;
#22632 = CARTESIAN_POINT ( 'NONE',  ( -10.07076617545328467, -80.47065289228903850, 3.889019895268755356 ) ) ;
#22633 = VERTEX_POINT ( 'NONE', #52117 ) ;
#22634 = CARTESIAN_POINT ( 'NONE',  ( 12.04731061283000138, -77.94272812832399211, 0.2409951698105000095 ) ) ;
#22635 = ORIENTED_EDGE ( 'NONE', *, *, #27697, .F. ) ;
#22636 = B_SPLINE_SURFACE_WITH_KNOTS ( 'NONE', 3, 3, ( 
 ( #3824, #30672, #48708, #7964, #25962, #48995, #8254, #26254, #3259, #25676, #4115, #43985, #21250, #22115, #39252, #31249, #3538, #4413, #53130, #44268, #21540, #49291, #39830, #56980, #39546, #57268, #57842, #40124, #8842, #35692, #57550, #16832, #16542, #34522, #17112 ),
 ( #35096, #52555, #12680, #30093, #10313, #18295, #19167, #36868, #41017, #10022, #50471, #23583, #36290, #31847, #27424, #14718, #892, #9724, #40429, #41598, #28000, #609, #27713, #28292, #46048, #27125, #5573, #1177, #5290, #50767, #18589, #37162, #45165, #31548, #20 ),
 ( #55176, #32715, #13851, #54880, #4715, #22713, #45757, #46343, #40727, #22416, #17999, #45459, #35990, #23297, #49889, #54312, #13556, #41306, #318, #54015, #49595, #9434, #9140, #5002, #23006, #36580, #54602, #14430, #14139, #32138, #50179, #18875, #32425, #34169, #52206 ),
 ( #20051, #6748, #42773, #33602, #51641, #15017, #7039, #56345, #51925, #24173, #11483, #37452, #11196, #51345, #33885, #55469, #10607, #20330, #55770, #20616, #2051, #43061, #47219, #29454, #15316, #46634, #42189, #41890, #38617, #33011, #38039, #25039, #28880, #2619, #6164 ) ),
 .UNSPECIFIED., .F., .F., .F.,
 ( 4, 4 ),
 ( 4, 1, 1, 1, 1, 1, 1, 1, 1, 1, 1, 1, 1, 1, 1, 1, 1, 1, 1, 1, 1, 1, 1, 1, 1, 1, 1, 1, 1, 1, 1, 1, 4 ),
 ( -0.4015584965371999937, 1.401558496537000043 ),
 ( -0.01447761194029999893, 0.009048507462687000596, 0.03257462686566999638, 0.05610074626866000391, 0.07962686567163999862, 0.1031529850746000093, 0.1266791044776000019, 0.1502052238806000084, 0.1737313432835999871, 0.1972574626865999936, 0.2207835820896000001, 0.2443097014925000032, 0.2678358208955000097, 0.2913619402984999884, 0.3148880597015000227, 0.3384141791045000014, 0.3619402985074999801, 0.3854664179103999833, 0.4089925373133999620, 0.4325186567163999962, 0.4560447761193999749, 0.4795708955224000092, 0.5030970149253999324, 0.5266231343284000221, 0.5501492537312999698, 0.5736753731343000595, 0.5972014925372999272, 0.6207276119402999059, 0.6442537313433001067, 0.6677798507462999744, 0.6913059701493000642, 0.7148320895521999008, 0.7383582089551999905 ),
 .UNSPECIFIED. ) ;
#22637 = ORIENTED_EDGE ( 'NONE', *, *, #9082, .F. ) ;
#22638 = CIRCLE ( 'NONE', #57479, 10.40000000000000036 ) ;
#22639 = CARTESIAN_POINT ( 'NONE',  ( -4.000000000000000000, -75.00000000000001421, -0.5999999999999999778 ) ) ;
#22640 = EDGE_CURVE ( 'NONE', #19148, #18069, #7233, .T. ) ;
#22641 = CARTESIAN_POINT ( 'NONE',  ( -9.541585721800542430, -76.45157166904904500, -7.319559354884466629 ) ) ;
#22642 = CARTESIAN_POINT ( 'NONE',  ( 8.985706068735000329, -79.96796090277857161, -3.828549499589000149 ) ) ;
#22643 = EDGE_CURVE ( 'NONE', #54661, #11972, #2863, .T. ) ;
#22644 = ORIENTED_EDGE ( 'NONE', *, *, #27495, .T. ) ;
#22645 = ORIENTED_EDGE ( 'NONE', *, *, #9988, .F. ) ;
#22646 = CARTESIAN_POINT ( 'NONE',  ( 9.008013791555782745, -79.32919974289639242, -2.421050323904322177 ) ) ;
#22647 = CARTESIAN_POINT ( 'NONE',  ( 3.999999999999816147, -78.72610001270986402, -1.484001723589534194E-15 ) ) ;
#22648 = CARTESIAN_POINT ( 'NONE',  ( -4.000000000000000000, -5.000000000000000000, 0.5999999999999999778 ) ) ;
#22649 = CARTESIAN_POINT ( 'NONE',  ( -7.642147947518999729, -22.78485473281999774, -10.55910102242999926 ) ) ;
#22650 = CARTESIAN_POINT ( 'NONE',  ( 0.9999999970599000587, -81.20000000293998710, -6.999999982650000341 ) ) ;
#22651 = CARTESIAN_POINT ( 'NONE',  ( 11.74999999999999289, -78.56041666666666856, 1.538071403320028452 ) ) ;
#22652 = CARTESIAN_POINT ( 'NONE',  ( 6.060555231919183328, -77.31796419498604678, -10.11800260501370730 ) ) ;
#22653 = CARTESIAN_POINT ( 'NONE',  ( 0.002314721400742156526, -78.72516494628735018, -9.249912767016533977 ) ) ;
#22654 = CARTESIAN_POINT ( 'NONE',  ( 0.000000000000000000, -81.99999999999998579, 0.000000000000000000 ) ) ;
#22655 = CONICAL_SURFACE ( 'NONE', #64, 0.6999999997695000031, 0.7853981633972997312 ) ;
#22656 = CARTESIAN_POINT ( 'NONE',  ( -10.36222489919000012, -23.22120223852000009, 7.631889817950999522 ) ) ;
#22657 = DIRECTION ( 'NONE',  ( -0.9957542217955486219, -0.04890179608105237746, -0.07798810240279377415 ) ) ;
#22658 = CARTESIAN_POINT ( 'NONE',  ( 8.954446855713042552, -77.82933363352677247, -2.398406063174361336 ) ) ;
#22659 = CARTESIAN_POINT ( 'NONE',  ( 3.230515030065010951, -78.30642889406193774, 11.63305551197263021 ) ) ;
#22660 = CARTESIAN_POINT ( 'NONE',  ( -1.151506974306000020, -81.40430496681199202, 4.010497975643999347 ) ) ;
#22661 = CARTESIAN_POINT ( 'NONE',  ( -8.554185150784999081, -77.36226001420200760, -4.929210599936999948 ) ) ;
#22662 = CARTESIAN_POINT ( 'NONE',  ( -0.006417454803627380307, -79.62467248096164951, -1.262730415849851573 ) ) ;
#22663 = CARTESIAN_POINT ( 'NONE',  ( 7.601397897754999633, -55.54999999966999980, -9.369164850722000892 ) ) ;
#22664 = CARTESIAN_POINT ( 'NONE',  ( 0.4356486348717999446, -24.88064955810000001, 12.43591427121000237 ) ) ;
#22665 = DIRECTION ( 'NONE',  ( 0.000000000000000000, -1.000000000000000000, 0.000000000000000000 ) ) ;
#22666 = CARTESIAN_POINT ( 'NONE',  ( -1.162810066705999956, -0.7833146285216000537, 3.409566898876999819 ) ) ;
#22667 = CARTESIAN_POINT ( 'NONE',  ( -1.250000000000000000, -80.99999999999998579, 0.000000000000000000 ) ) ;
#22668 = CARTESIAN_POINT ( 'NONE',  ( 8.954706589602396960, -79.82963375756635571, -2.398204254170784200 ) ) ;
#22669 = CARTESIAN_POINT ( 'NONE',  ( 0.9951084243826858744, -81.03151564770095661, -1.137131669208984786 ) ) ;
#22670 = CARTESIAN_POINT ( 'NONE',  ( 12.55458806508999992, -60.96283916815999504, -1.575041344316999936 ) ) ;
#22671 = CARTESIAN_POINT ( 'NONE',  ( 9.250000000000000000, -78.74999999999998579, 0.000000000000000000 ) ) ;
#22672 = DIRECTION ( 'NONE',  ( 0.000000000000000000, -1.000000000000000000, 0.000000000000000000 ) ) ;
#22673 = CARTESIAN_POINT ( 'NONE',  ( 10.89987286286000057, -78.27216546898499416, -0.6067434084558999130 ) ) ;
#22674 = VECTOR ( 'NONE', #13614, 1000.000000000000000 ) ;
#22675 = CARTESIAN_POINT ( 'NONE',  ( -10.11841891201000010, -77.39430565866300071, 6.752786780719000070 ) ) ;
#22676 = CARTESIAN_POINT ( 'NONE',  ( -4.043136777828877371, -78.19531677776082290, -10.31450538517581883 ) ) ;
#22678 = CARTESIAN_POINT ( 'NONE',  ( -0.1877060973040000080, -78.41174741493239253, -1.405284953735000064 ) ) ;
#22677 = DIRECTION ( 'NONE',  ( -1.000000000000000000, 0.000000000000000000, 0.000000000000000000 ) ) ;
#22679 = CARTESIAN_POINT ( 'NONE',  ( 1.503815466746999840, -81.98234125147999407, 0.5029271919957000181 ) ) ;
#22680 = EDGE_LOOP ( 'NONE', ( #45231, #2463, #1666, #19667, #12987 ) ) ;
#22681 = CARTESIAN_POINT ( 'NONE',  ( -3.315816780652000251, -86.19041401731898588, 0.9364754677271999173 ) ) ;
#22682 = CARTESIAN_POINT ( 'NONE',  ( 3.695666939335999768, -80.22553196422599342, -10.41991477582000059 ) ) ;
#22683 = CARTESIAN_POINT ( 'NONE',  ( -1.980532734072999901, -59.56232686814000488, -12.80090744966000038 ) ) ;
#22684 = CARTESIAN_POINT ( 'NONE',  ( 1.199500263597271799, -81.69791666666667140, -0.9218200799623701425 ) ) ;
#22685 = CARTESIAN_POINT ( 'NONE',  ( -12.85144117167999944, -57.04527983067000463, -1.980464439859999981 ) ) ;
#22686 = CARTESIAN_POINT ( 'NONE',  ( 4.202230864774000096, -78.48968660667100039, -8.786407198941001084 ) ) ;
#22687 = CARTESIAN_POINT ( 'NONE',  ( -8.971242061857001460, -77.31783216571999162, -8.906291659541000882 ) ) ;
#22688 = CARTESIAN_POINT ( 'NONE',  ( 9.188870790291838730, -78.07333333333335190, 2.784684813981618490 ) ) ;
#22689 = CARTESIAN_POINT ( 'NONE',  ( 12.61112459819999998, -23.21565178569999688, -1.798929298655999931 ) ) ;
#22690 = CARTESIAN_POINT ( 'NONE',  ( -7.648026766715999791, -55.54999999381000464, -10.12290050087000104 ) ) ;
#22691 = ORIENTED_EDGE ( 'NONE', *, *, #49273, .T. ) ;
#22692 = CARTESIAN_POINT ( 'NONE',  ( 1.500000000000000222, -80.73359037631325918, -0.3093141193355201102 ) ) ;
#22693 = LINE ( 'NONE', #28567, #54279 ) ;
#22694 = CARTESIAN_POINT ( 'NONE',  ( 10.88867600136477520, -75.91842355713455959, -4.512338881074533958 ) ) ;
#22695 = EDGE_CURVE ( 'NONE', #31318, #17717, #26666, .T. ) ;
#22696 = CARTESIAN_POINT ( 'NONE',  ( 2.264809212410999647E-14, -92.79999999999999716, 0.000000000000000000 ) ) ;
#22697 = CARTESIAN_POINT ( 'NONE',  ( -12.58338334673999981, -57.05199022587000002, -1.667961445601999992 ) ) ;
#22698 = CARTESIAN_POINT ( 'NONE',  ( 0.000000000000000000, -81.10000000285099020, 7.000000000000000000 ) ) ;
#22699 = VERTEX_POINT ( 'NONE', #52976 ) ;
#22700 = AXIS2_PLACEMENT_3D ( 'NONE', #55300, #51180, #32840 ) ;
#22701 = CARTESIAN_POINT ( 'NONE',  ( -1.799490225533999732, -22.77152778045000048, 12.64500484462999985 ) ) ;
#22702 = EDGE_LOOP ( 'NONE', ( #43508, #16456, #18654 ) ) ;
#22703 = ORIENTED_EDGE ( 'NONE', *, *, #22944, .F. ) ;
#22704 = CARTESIAN_POINT ( 'NONE',  ( -9.641218323587999350, -54.36606991882000273, -7.943737929401001985 ) ) ;
#22705 = PRESENTATION_STYLE_ASSIGNMENT (( #8834 ) ) ;
#22706 = CARTESIAN_POINT ( 'NONE',  ( -7.479908383216000267, -79.38573615547299767, -6.281056869080000382 ) ) ;
#22707 = ADVANCED_FACE ( 'NONE', ( #42968 ), #15733, .F. ) ;
#22708 = VERTEX_POINT ( 'NONE', #34372 ) ;
#22709 = CARTESIAN_POINT ( 'NONE',  ( 4.281740904750999555, -76.77686128452499759, -11.46096623826999839 ) ) ;
#22710 = CARTESIAN_POINT ( 'NONE',  ( -9.586068793935504928, -78.63753982021442823, -4.864924515320017129 ) ) ;
#22711 = CARTESIAN_POINT ( 'NONE',  ( 1.595957623597000108, -77.99986730064999563, -0.4120752205041999794 ) ) ;
#22712 = ORIENTED_EDGE ( 'NONE', *, *, #55001, .T. ) ;
#22713 = CARTESIAN_POINT ( 'NONE',  ( 8.503129636637000388, -77.78324805011499166, -4.225430575863000193 ) ) ;
#22714 = AXIS2_PLACEMENT_3D ( 'NONE', #44492, #40055, #31182 ) ;
#22715 = CARTESIAN_POINT ( 'NONE',  ( 0.8949709245464939622, -80.28907454115488918, -0.8721969588273668084 ) ) ;
#22716 = CARTESIAN_POINT ( 'NONE',  ( 7.344138154013000630, -78.16668243576999942, -10.86413439232000044 ) ) ;
#22717 = CARTESIAN_POINT ( 'NONE',  ( -3.244487197725999916, -76.85164885045787742, -10.73738397614000029 ) ) ;
#22718 = CARTESIAN_POINT ( 'NONE',  ( 4.177667811529521380, -86.39318692614398287, 0.4795288509365496221 ) ) ;
#22719 = CARTESIAN_POINT ( 'NONE',  ( -4.814859605045999302, -78.66631515532277774, 8.425427962446999430 ) ) ;
#22720 = CARTESIAN_POINT ( 'NONE',  ( 5.435707952731398507, -79.92548822285989729, 7.484002565572681398 ) ) ;
#22721 = CARTESIAN_POINT ( 'NONE',  ( 3.404852354755926847, -79.58645832216895144, 2.196520115241515470 ) ) ;
#22722 = ORIENTED_EDGE ( 'NONE', *, *, #21413, .F. ) ;
#22723 = PLANE ( 'NONE',  #38218 ) ;
#22724 = CARTESIAN_POINT ( 'NONE',  ( 2.868090520736068516, -77.25025914830622753, -8.794003640997004823 ) ) ;
#22725 = CARTESIAN_POINT ( 'NONE',  ( 1.602460118848999970, -80.14825829503000421, -0.1983317763271000012 ) ) ;
#22726 = EDGE_CURVE ( 'NONE', #52059, #25178, #18956, .T. ) ;
#22727 = CARTESIAN_POINT ( 'NONE',  ( 1.001315002657000131, -61.48522411647999775, -12.50000000000000000 ) ) ;
#22728 = CARTESIAN_POINT ( 'NONE',  ( -0.7737575051148579686, -3.456640438237565061, -3.432738176510635952 ) ) ;
#22729 = CYLINDRICAL_SURFACE ( 'NONE', #14358, 10.50000000000000000 ) ;
#22730 = CARTESIAN_POINT ( 'NONE',  ( 3.090997446795999970, -77.34692757071799463, -11.88544462247999967 ) ) ;
#22731 = CARTESIAN_POINT ( 'NONE',  ( 0.000000000000000000, -76.89999999999999147, -9.549999999999952749 ) ) ;
#22732 = CARTESIAN_POINT ( 'NONE',  ( -7.226567707739000923, -77.32088998579800432, 6.526040278862000221 ) ) ;
#22733 = CARTESIAN_POINT ( 'NONE',  ( -10.79065230704753198, -77.08694916350313520, -5.396898631840323368 ) ) ;
#22734 = CARTESIAN_POINT ( 'NONE',  ( -9.748677221152634687, -76.51023458671352273, -8.641220746763186966 ) ) ;
#22735 = AXIS2_PLACEMENT_3D ( 'NONE', #50096, #40936, #58055 ) ;
#22736 = VERTEX_POINT ( 'NONE', #21953 ) ;
#22737 = CARTESIAN_POINT ( 'NONE',  ( -0.4275916205537000359, -81.79006927205000466, 1.526944760756999919 ) ) ;
#22738 = CARTESIAN_POINT ( 'NONE',  ( -0.6532870389514158216, -78.68357565247356433, -1.115868458321769952 ) ) ;
#22739 = DIRECTION ( 'NONE',  ( 0.000000000000000000, 0.000000000000000000, 1.000000000000000000 ) ) ;
#22740 = CARTESIAN_POINT ( 'NONE',  ( -1.250000000000001332, -78.98958333333331439, 0.1636246173744632659 ) ) ;
#22741 = CARTESIAN_POINT ( 'NONE',  ( 7.639893274927809230, -23.38715751204583171, 10.11462445490727546 ) ) ;
#22742 = EDGE_CURVE ( 'NONE', #28360, #13397, #40247, .T. ) ;
#22743 = DIRECTION ( 'NONE',  ( -0.7071067811865474617, -0.7071067811865474617, 9.038574250522602634E-10 ) ) ;
#22744 = CARTESIAN_POINT ( 'NONE',  ( -9.601739433208001273, -79.02244415034599001, -1.533141744029000053 ) ) ;
#22745 = CARTESIAN_POINT ( 'NONE',  ( 9.078688998878000405, -79.04716346014799910, 3.126726393672000004 ) ) ;
#22746 = CARTESIAN_POINT ( 'NONE',  ( 0.003566689646507039367, -76.07464878890591820, 11.74978033122256704 ) ) ;
#22747 = CARTESIAN_POINT ( 'NONE',  ( -0.4035379437255999791, -79.64864834222998979, -10.90928609572000063 ) ) ;
#22748 = DIRECTION ( 'NONE',  ( 0.000000000000000000, 1.000000000000000000, 0.000000000000000000 ) ) ;
#22749 = ORIENTED_EDGE ( 'NONE', *, *, #23349, .T. ) ;
#22750 = LINE ( 'NONE', #36903, #49280 ) ;
#22751 = CARTESIAN_POINT ( 'NONE',  ( 3.407095545933005010, -78.62148120184446043, -1.253608761936364502E-15 ) ) ;
#22752 = CARTESIAN_POINT ( 'NONE',  ( -10.75000000000000355, -77.48958333333332860, 1.407171709420384609 ) ) ;
#22753 = AXIS2_PLACEMENT_3D ( 'NONE', #46408, #4779, #9794 ) ;
#22754 = CARTESIAN_POINT ( 'NONE',  ( -0.5193979750644999172, -79.05138421710698537, -10.96331347381999954 ) ) ;
#22755 = CARTESIAN_POINT ( 'NONE',  ( -1.342463812738999916E-14, -80.75000000002938805, 0.000000000000000000 ) ) ;
#22756 = CARTESIAN_POINT ( 'NONE',  ( -12.00000000000000000, -77.89999999999999147, -2.795183092923000262E-14 ) ) ;
#22757 = CARTESIAN_POINT ( 'NONE',  ( -1.750000000001000089, -55.55000001292999912, -12.56594318049000059 ) ) ;
#22758 = CARTESIAN_POINT ( 'NONE',  ( 0.000000000000000000, -76.79999999999999716, -3.999999999999249045 ) ) ;
#22759 = VERTEX_POINT ( 'NONE', #53554 ) ;
#22760 = VECTOR ( 'NONE', #26021, 1000.000000000000000 ) ;
#22761 = CARTESIAN_POINT ( 'NONE',  ( -11.25198206936999945, -79.77995714425598806, -0.4763024974861999605 ) ) ;
#22762 = CARTESIAN_POINT ( 'NONE',  ( -0.5999999998848000171, -23.14999999478999726, -11.79999999988000070 ) ) ;
#22763 = CARTESIAN_POINT ( 'NONE',  ( 3.851650068366999857, -78.43735716284258785, -4.716910927661330529E-16 ) ) ;
#22764 = EDGE_CURVE ( 'NONE', #35854, #55147, #35227, .T. ) ;
#22765 = CARTESIAN_POINT ( 'NONE',  ( -0.9386777138244112306, -81.54303105412684261, 0.8252884126292686640 ) ) ;
#22766 = CARTESIAN_POINT ( 'NONE',  ( 0.9241086513771999966, -78.61146369488598395, 11.11924560648999893 ) ) ;
#22767 = ADVANCED_FACE ( 'NONE', ( #13388 ), #30792, .T. ) ;
#22768 = CARTESIAN_POINT ( 'NONE',  ( 7.229432123684064848, -76.31666666666667709, 8.035240866938130111 ) ) ;
#22769 = CARTESIAN_POINT ( 'NONE',  ( 1.412381594861192191, -81.62866237199072827, 0.5432125840743284861 ) ) ;
#22770 = CARTESIAN_POINT ( 'NONE',  ( 7.396918292183153554, -79.80208333333332860, 5.684557159767984480 ) ) ;
#22771 = CARTESIAN_POINT ( 'NONE',  ( -3.023821996898441000, -79.59699371105349996, 10.64354645710085201 ) ) ;
#22772 = PRESENTATION_STYLE_ASSIGNMENT (( #49949 ) ) ;
#22773 = CARTESIAN_POINT ( 'NONE',  ( 8.343860018000999190, -55.64999999967000122, 8.343860018000999190 ) ) ;
#22774 = EDGE_LOOP ( 'NONE', ( #40653, #50824, #25536, #12820, #9787 ) ) ;
#22775 = EDGE_CURVE ( 'NONE', #12955, #41153, #673, .T. ) ;
#22776 = ORIENTED_EDGE ( 'NONE', *, *, #36838, .T. ) ;
#22777 = STYLED_ITEM ( 'NONE', ( #55604 ), #42678 ) ;
#22778 = CARTESIAN_POINT ( 'NONE',  ( -7.601397897754999633, -23.24999999758999536, 10.07627163191000008 ) ) ;
#22779 = CARTESIAN_POINT ( 'NONE',  ( 12.50000000000000000, -13.07071424677999971, 0.000000000000000000 ) ) ;
#22780 = ORIENTED_EDGE ( 'NONE', *, *, #36033, .T. ) ;
#22781 = CARTESIAN_POINT ( 'NONE',  ( -5.279550234765999939, -76.33587572314411318, -9.859017853534000508 ) ) ;
#22782 = ORIENTED_EDGE ( 'NONE', *, *, #31173, .F. ) ;
#22783 = CARTESIAN_POINT ( 'NONE',  ( 2.843708761399523777, -82.59270834996989663, 1.941616614676821229 ) ) ;
#22784 = CARTESIAN_POINT ( 'NONE',  ( 8.061453700986000115, -77.45092985212998826, 7.530916186516999566 ) ) ;
#22785 = CARTESIAN_POINT ( 'NONE',  ( 9.009247259181924150, -79.72916666666665719, -2.421167930323326001 ) ) ;
#22786 = CARTESIAN_POINT ( 'NONE',  ( 4.581254438705999910, -78.79353998579799168, -8.535416510302999527 ) ) ;
#22787 = CARTESIAN_POINT ( 'NONE',  ( -5.757354885052930804, -78.17157179074094131, -7.240009484917052873 ) ) ;
#22788 = CARTESIAN_POINT ( 'NONE',  ( 4.653115705712000505, -78.92514563794199489, -10.20620521156999949 ) ) ;
#22789 = DIRECTION ( 'NONE',  ( 0.000000000000000000, 3.439130521500999441E-11, -1.000000000000000000 ) ) ;
#22790 = ORIENTED_EDGE ( 'NONE', *, *, #3245, .F. ) ;
#22791 = CARTESIAN_POINT ( 'NONE',  ( 9.369164850722000892, -55.54999999966999980, 7.601397897754999633 ) ) ;
#22792 = ORIENTED_EDGE ( 'NONE', *, *, #39537, .F. ) ;
#22793 = CARTESIAN_POINT ( 'NONE',  ( 1.801927416992543218, -77.45946252748643701, 9.073133184625993053 ) ) ;
#22794 = CARTESIAN_POINT ( 'NONE',  ( -1.996894868142000012, -77.37992772649998585, 10.85801781015000067 ) ) ;
#22795 = CARTESIAN_POINT ( 'NONE',  ( 1.460959015002472494, -77.77083333333335702, 0.3926218265389233020 ) ) ;
#22796 = DIRECTION ( 'NONE',  ( 0.000000000000000000, 0.7071067811866525998, -0.7071067811864425456 ) ) ;
#22797 = VECTOR ( 'NONE', #27111, 1000.000000000000000 ) ;
#22798 = CARTESIAN_POINT ( 'NONE',  ( 8.553489385229999797, -79.17627884718898201, 4.133741566275999979 ) ) ;
#22799 = CARTESIAN_POINT ( 'NONE',  ( 10.62738844531999938, -76.71202665592998926, -6.424126605269999679 ) ) ;
#22800 = CARTESIAN_POINT ( 'NONE',  ( -7.985521294471968012, -79.44573719447619453, -5.195944220544125081 ) ) ;
#22801 = CARTESIAN_POINT ( 'NONE',  ( 1.136899222205000060, -79.08384707092999122, 1.164526648744999893 ) ) ;
#22802 = CARTESIAN_POINT ( 'NONE',  ( 0.000000000000000000, -78.00000000000000000, -7.200000000000000178 ) ) ;
#22803 = CARTESIAN_POINT ( 'NONE',  ( 0.1286847231337999997, -79.30325033209098251, 10.93943584368999922 ) ) ;
#22804 = CARTESIAN_POINT ( 'NONE',  ( 0.000000000000000000, -60.04999999966999980, 12.00000000000000000 ) ) ;
#22805 = CARTESIAN_POINT ( 'NONE',  ( -11.52318292100913233, -76.68414653309548612, 2.296907436951973747 ) ) ;
#22806 = CARTESIAN_POINT ( 'NONE',  ( -3.513994194679999961, -85.82921411580198878, 0.9922410806546999584 ) ) ;
#22807 = ORIENTED_EDGE ( 'NONE', *, *, #5195, .F. ) ;
#22808 = CARTESIAN_POINT ( 'NONE',  ( -0.5565216587110000113, -78.88749453345599250, 12.18770865518000157 ) ) ;
#22809 = CARTESIAN_POINT ( 'NONE',  ( -5.797379302154999969, -76.05869307850399252, 9.786931085294000354 ) ) ;
#22810 = CARTESIAN_POINT ( 'NONE',  ( -4.117775072621233434, -78.00630082584859792, 9.930058322751628808 ) ) ;
#22811 = CARTESIAN_POINT ( 'NONE',  ( -1.835125225091999823, -78.02113251428799856, 11.83842809849000055 ) ) ;
#22812 = CYLINDRICAL_SURFACE ( 'NONE', #54200, 11.75000000000000000 ) ;
#22813 = EDGE_CURVE ( 'NONE', #10320, #34146, #18603, .T. ) ;
#22814 = CARTESIAN_POINT ( 'NONE',  ( 0.000000000000000000, -81.99999999999998579, 0.000000000000000000 ) ) ;
#22815 = DIRECTION ( 'NONE',  ( 0.000000000000000000, 1.000000000000000000, 0.000000000000000000 ) ) ;
#22816 = CARTESIAN_POINT ( 'NONE',  ( 6.297347977225174809, -80.92545155199817941, 8.712196151594245208 ) ) ;
#22817 = CARTESIAN_POINT ( 'NONE',  ( 10.38645071868999992, -59.57819125629999490, -7.655542440085000067 ) ) ;
#22818 = CARTESIAN_POINT ( 'NONE',  ( -7.596835002782709623, -78.35208333333333997, -5.838193839761696147 ) ) ;
#22819 = CARTESIAN_POINT ( 'NONE',  ( 6.290530912463999869, -78.21842036916400787, 9.202381290206000486 ) ) ;
#22820 = CARTESIAN_POINT ( 'NONE',  ( 1.570796326794857478, -78.16458333333332575, 12.00000000000000533 ) ) ;
#22821 = CARTESIAN_POINT ( 'NONE',  ( -8.998761386569000820, -80.50788840704829852, -6.370985394032000926 ) ) ;
#22822 = ORIENTED_EDGE ( 'NONE', *, *, #22132, .F. ) ;
#22823 = CARTESIAN_POINT ( 'NONE',  ( 0.005523896503961000029, -53.73036543741000060, 12.55021156877000088 ) ) ;
#22824 = CARTESIAN_POINT ( 'NONE',  ( 0.000000000000000000, -76.75499999999999545, 0.000000000000000000 ) ) ;
#22825 = CARTESIAN_POINT ( 'NONE',  ( -10.09635298636609058, -23.52373519997163953, 7.644087781972075391 ) ) ;
#22826 = CARTESIAN_POINT ( 'NONE',  ( -5.859445663532000914, -77.61705592642898921, 9.564779511708000115 ) ) ;
#22827 = CARTESIAN_POINT ( 'NONE',  ( -6.760013919724056741, -79.77291666666666003, -8.796335266379987416 ) ) ;
#22828 = CARTESIAN_POINT ( 'NONE',  ( -9.500000000000000000, -77.29999999999999716, 0.000000000000000000 ) ) ;
#22829 = CARTESIAN_POINT ( 'NONE',  ( 3.761670435195240358, -82.53489581458633495, 1.396303704899410691 ) ) ;
#22830 = CARTESIAN_POINT ( 'NONE',  ( -10.69999999999999929, -76.39999999999999147, 0.000000000000000000 ) ) ;
#22831 = DIRECTION ( 'NONE',  ( 0.000000000000000000, 1.000000000000000000, 0.000000000000000000 ) ) ;
#22832 = CARTESIAN_POINT ( 'NONE',  ( 4.038168894520000052, -83.87669503318799968, -1.050359118944999892 ) ) ;
#22833 = CARTESIAN_POINT ( 'NONE',  ( -8.782705134682748493, -76.05000000000001137, 7.901937436400075399 ) ) ;
#22834 = CARTESIAN_POINT ( 'NONE',  ( 9.963464501270999918, -55.11723479348000154, -7.659241807016999637 ) ) ;
#22835 = CARTESIAN_POINT ( 'NONE',  ( -11.26188033092999952, -77.77703838196799779, -0.06337168221170999538 ) ) ;
#22836 = ADVANCED_FACE ( 'NONE', ( #44398 ), #17729, .F. ) ;
#22837 = CARTESIAN_POINT ( 'NONE',  ( -0.5298108134926000634, -80.61193089235000286, 1.579417458585999912 ) ) ;
#22838 = CARTESIAN_POINT ( 'NONE',  ( 1.543707792073999885, -78.64998119068999927, 0.1290987484668000007 ) ) ;
#22839 = CARTESIAN_POINT ( 'NONE',  ( -8.324924863653999196, -77.34795187468598954, 4.923709561474999497 ) ) ;
#22840 = CARTESIAN_POINT ( 'NONE',  ( 9.250000000000000000, -78.24999999999998579, -1.152201742116999973E-14 ) ) ;
#22841 = CIRCLE ( 'NONE', #46419, 0.5000000000000004441 ) ;
#22842 = CARTESIAN_POINT ( 'NONE',  ( -12.59651352883999920, -60.19056208351000237, 1.801710201210000140 ) ) ;
#22843 = LINE ( 'NONE', #44996, #21701 ) ;
#22844 = DIRECTION ( 'NONE',  ( -1.000000000000000000, 0.000000000000000000, 0.000000000000000000 ) ) ;
#22845 = CARTESIAN_POINT ( 'NONE',  ( 0.3993207018968132904, -77.99983260076393776, 1.209697183087648620 ) ) ;
#22846 = CARTESIAN_POINT ( 'NONE',  ( 1.060064467237852970, -81.80564032585678547, -0.6624441280364113949 ) ) ;
#22847 = B_SPLINE_CURVE_WITH_KNOTS ( 'NONE', 3,
 ( #16596, #26013, #56464, #7732 ),
 .UNSPECIFIED., .F., .F.,
 ( 4, 4 ),
 ( 0.000000000000000000, 1.000000000000000000 ),
 .UNSPECIFIED. ) ;
#22848 = CIRCLE ( 'NONE', #55854, 13.86363636363999952 ) ;
#22849 = CARTESIAN_POINT ( 'NONE',  ( -1.001315002657000131, -61.48522411647999775, 12.50000000000000000 ) ) ;
#22850 = CARTESIAN_POINT ( 'NONE',  ( 8.500810681529999968, -80.08515741644239938, -7.210465973013999275 ) ) ;
#22851 = CARTESIAN_POINT ( 'NONE',  ( -0.4635254915624000271, -77.75000000000000000, 1.426584774443000025 ) ) ;
#22852 = EDGE_LOOP ( 'NONE', ( #26973, #48913, #16256, #43083 ) ) ;
#22853 = EDGE_CURVE ( 'NONE', #31523, #55944, #55303, .T. ) ;
#22854 = VERTEX_POINT ( 'NONE', #42020 ) ;
#22855 = CARTESIAN_POINT ( 'NONE',  ( 1.593618269839000012, -81.75481172353600812, 0.2599901540301000069 ) ) ;
#22856 = EDGE_CURVE ( 'NONE', #28471, #35775, #45027, .T. ) ;
#22857 = VERTEX_POINT ( 'NONE', #28127 ) ;
#22858 = ORIENTED_EDGE ( 'NONE', *, *, #56979, .F. ) ;
#22859 = CARTESIAN_POINT ( 'NONE',  ( 0.000000000000000000, -0.2000000000000000111, -3.600000000000000089 ) ) ;
#22860 = AXIS2_PLACEMENT_3D ( 'NONE', #22026, #29720, #7303 ) ;
#22861 = DIRECTION ( 'NONE',  ( 0.9999548435846228323, 0.000000000000000000, 0.009503199022040218977 ) ) ;
#22862 = CARTESIAN_POINT ( 'NONE',  ( 3.142447459108117513, -81.05104165469458621, 1.410275201556511870 ) ) ;
#22863 = CIRCLE ( 'NONE', #21008, 9.760776772971999193 ) ;
#22864 = CARTESIAN_POINT ( 'NONE',  ( 1.056237665594999875, -25.04866013698000060, -12.77256098197999989 ) ) ;
#22865 = CARTESIAN_POINT ( 'NONE',  ( -3.666049313226999562, -82.05721315976299479, -0.8194224013866000522 ) ) ;
#22866 = CARTESIAN_POINT ( 'NONE',  ( 7.528714304400998536, -78.03471672827505756, -8.074838600060001426 ) ) ;
#22867 = CARTESIAN_POINT ( 'NONE',  ( 11.86573868791000130, -78.48725095961999898, -1.065667360763999927 ) ) ;
#22868 = VERTEX_POINT ( 'NONE', #1022 ) ;
#22869 = ORIENTED_EDGE ( 'NONE', *, *, #27165, .T. ) ;
#22870 = CARTESIAN_POINT ( 'NONE',  ( -1.232226823824148054, -17.47709088732338856, -12.50408896749709342 ) ) ;
#22871 = CARTESIAN_POINT ( 'NONE',  ( -0.9565643533716999825, -80.16053826575100061, 0.9292797142584000580 ) ) ;
#22872 = CARTESIAN_POINT ( 'NONE',  ( 9.512131559252001267, -77.94368839240499369, -1.920953556448999899 ) ) ;
#22873 = EDGE_CURVE ( 'NONE', #50534, #5620, #1888, .T. ) ;
#22874 = CARTESIAN_POINT ( 'NONE',  ( -3.727357686973370221, -86.31452044229999387, -2.601403949838035246 ) ) ;
#22875 = CARTESIAN_POINT ( 'NONE',  ( -10.24996238026999862, -21.75171076523999858, 7.705119999407000542 ) ) ;
#22876 = CARTESIAN_POINT ( 'NONE',  ( -10.46686097783000058, -76.78266118432999576, 7.365735401690999495 ) ) ;
#22877 = CARTESIAN_POINT ( 'NONE',  ( 1.195983586496999873, -79.34407194668000329, -0.8522763136304999376 ) ) ;
#22878 = CARTESIAN_POINT ( 'NONE',  ( 10.80179710294999929, -76.28640138136300664, 1.338497018408000061 ) ) ;
#22879 = CARTESIAN_POINT ( 'NONE',  ( 4.000000000000000000, -75.00000000000001421, 0.5999999999999999778 ) ) ;
#22880 = CARTESIAN_POINT ( 'NONE',  ( -1.508573806804000217, -79.04323530191599900, -3.892781328016000408 ) ) ;
#22882 = AXIS2_PLACEMENT_3D ( 'NONE', #51003, #37395, #15847 ) ;
#22881 = CARTESIAN_POINT ( 'NONE',  ( -0.3187246912203000049, -80.71114601151622026, 11.26088853021000169 ) ) ;
#22883 = CARTESIAN_POINT ( 'NONE',  ( -10.18589226633000067, -60.08917723397000543, 7.641012305241000391 ) ) ;
#22884 = CARTESIAN_POINT ( 'NONE',  ( -8.970693127363905006, -78.24378014202663678, 7.659364560157510660 ) ) ;
#22885 = CARTESIAN_POINT ( 'NONE',  ( 3.263030560321000362, -82.37257046129099081, -1.391707485291000079 ) ) ;
#22886 = CARTESIAN_POINT ( 'NONE',  ( 0.6284244718204999858, -78.38593289096679939, -1.176290284212999859 ) ) ;
#22887 = FACE_BOUND ( 'NONE', #37183, .T. ) ;
#22888 = CARTESIAN_POINT ( 'NONE',  ( 10.78853149093999875, -80.56065758149809142, -3.242959171380999983 ) ) ;
#22889 = CARTESIAN_POINT ( 'NONE',  ( -2.707053224964000027, -2.789967474678999526, 2.675433656965999774 ) ) ;
#22890 = CARTESIAN_POINT ( 'NONE',  ( -1.704234056905189032, -77.20000000000001705, -10.88120482596699468 ) ) ;
#22891 = EDGE_CURVE ( 'NONE', #29025, #4628, #24241, .T. ) ;
#22892 = ORIENTED_EDGE ( 'NONE', *, *, #41163, .F. ) ;
#22893 = CARTESIAN_POINT ( 'NONE',  ( -0.5705388283852488307, -23.34010097529044003, 10.98520465578149441 ) ) ;
#22894 = DIRECTION ( 'NONE',  ( -0.7071067811865475727, 0.000000000000000000, 0.7071067811865475727 ) ) ;
#22895 = CARTESIAN_POINT ( 'NONE',  ( -9.611650271896834852, -79.24166666666666003, -5.539808784079895965 ) ) ;
#22896 = CARTESIAN_POINT ( 'NONE',  ( -11.00000000000000000, -78.69999999999998863, 0.000000000000000000 ) ) ;
#22897 = CARTESIAN_POINT ( 'NONE',  ( 2.062597265787999845, -59.58461666436000570, 12.87024489159000140 ) ) ;
#22898 = CARTESIAN_POINT ( 'NONE',  ( 11.82764905900999963, -77.30156278830001781, 5.426413045081000419 ) ) ;
#22899 = CARTESIAN_POINT ( 'NONE',  ( -6.290935915195801975, -79.52477021992575601, 8.717027692168942465 ) ) ;
#22900 = CIRCLE ( 'NONE', #12529, 12.50000000000000000 ) ;
#22901 = CARTESIAN_POINT ( 'NONE',  ( -9.629019889039001967, -79.50708667140099806, -0.02420058354726000241 ) ) ;
#22902 = CARTESIAN_POINT ( 'NONE',  ( 9.546815224142999767, -17.31472046677999899, 8.130854305520999858 ) ) ;
#22903 = ORIENTED_EDGE ( 'NONE', *, *, #35705, .F. ) ;
#22904 = CIRCLE ( 'NONE', #19159, 12.25000000000000000 ) ;
#22905 = FACE_OUTER_BOUND ( 'NONE', #10373, .T. ) ;
#22906 = DIRECTION ( 'NONE',  ( 0.000000000000000000, 0.000000000000000000, -1.000000000000000000 ) ) ;
#22907 = CARTESIAN_POINT ( 'NONE',  ( 0.4476906417931999504, -81.89468275219000759, -1.231825476718000134 ) ) ;
#22908 = CARTESIAN_POINT ( 'NONE',  ( -1.749722766159037324, -18.52411007112459274, 12.54673760678534755 ) ) ;
#22909 = CARTESIAN_POINT ( 'NONE',  ( -8.883074525067000238, -78.99397594943899037, 3.114832498031999908 ) ) ;
#22911 = CARTESIAN_POINT ( 'NONE',  ( 4.010845454633999552, -1.563237677197000020, -0.2065758488482999922 ) ) ;
#22910 = CARTESIAN_POINT ( 'NONE',  ( 0.2029945029552999991, -85.62493728501499390, 4.125195677802000027 ) ) ;
#22912 = CARTESIAN_POINT ( 'NONE',  ( -1.799490225533999732, -56.02847221959000024, -12.64500484464000074 ) ) ;
#22913 = FACE_OUTER_BOUND ( 'NONE', #48289, .T. ) ;
#22914 = ORIENTED_EDGE ( 'NONE', *, *, #49486, .F. ) ;
#22915 = CARTESIAN_POINT ( 'NONE',  ( -3.256966265956249273, -77.20063234487528803, -10.24510830600284628 ) ) ;
#22916 = CARTESIAN_POINT ( 'NONE',  ( -12.50000000000000000, -24.68359816828999698, -1.003641515615000035 ) ) ;
#22917 = CARTESIAN_POINT ( 'NONE',  ( -3.992904449609000483, -78.77851881763731967, -1.675407828963362202E-14 ) ) ;
#22918 = ORIENTED_EDGE ( 'NONE', *, *, #38310, .T. ) ;
#22919 = ORIENTED_EDGE ( 'NONE', *, *, #51521, .T. ) ;
#22920 = CARTESIAN_POINT ( 'NONE',  ( -12.02912753549999891, -79.70112007896199202, 0.08506824670321999626 ) ) ;
#22921 = FACE_OUTER_BOUND ( 'NONE', #14438, .T. ) ;
#22922 = CARTESIAN_POINT ( 'NONE',  ( 5.642595794959916589, -80.33125413066214549, 9.203581900605376731 ) ) ;
#22923 = ORIENTED_EDGE ( 'NONE', *, *, #47931, .F. ) ;
#22924 = CARTESIAN_POINT ( 'NONE',  ( 3.947980971697000019, -78.53957306764699808, 11.38460442531999917 ) ) ;
#22925 = CIRCLE ( 'NONE', #24819, 0.6000000000000008660 ) ;
#22926 = ORIENTED_EDGE ( 'NONE', *, *, #5485, .T. ) ;
#22927 = ORIENTED_EDGE ( 'NONE', *, *, #1079, .T. ) ;
#22928 = CARTESIAN_POINT ( 'NONE',  ( -2.437508518915010303, -2.658928065967017584, -2.157570479308826172 ) ) ;
#22929 = AXIS2_PLACEMENT_3D ( 'NONE', #16497, #7629, #40971 ) ;
#22930 = CARTESIAN_POINT ( 'NONE',  ( -1.571007341338103158, -76.51400069817373151, -12.00174526218152593 ) ) ;
#22931 = LINE ( 'NONE', #32638, #8181 ) ;
#22932 = B_SPLINE_SURFACE_WITH_KNOTS ( 'NONE', 3, 3, ( 
 ( #39359, #11642, #24917, #12206 ),
 ( #16061, #57366, #6909, #29900 ),
 ( #24629, #3066, #7489, #38198 ),
 ( #12489, #11922, #15767, #29619 ) ),
 .UNSPECIFIED., .F., .F., .F.,
 ( 4, 4 ),
 ( 4, 4 ),
 ( 0.7425508590987000002, 1.053716877278999986 ),
 ( -0.0006517983049530999724, 0.01399779397395000020 ),
 .UNSPECIFIED. ) ;
#22933 = ORIENTED_EDGE ( 'NONE', *, *, #49017, .T. ) ;
#22934 = CARTESIAN_POINT ( 'NONE',  ( -7.958763982144999360, -54.32301960774000094, -9.723170657514000226 ) ) ;
#22935 = ORIENTED_EDGE ( 'NONE', *, *, #32881, .T. ) ;
#22936 = CARTESIAN_POINT ( 'NONE',  ( 1.062151845517925741, -80.35325191499507014, -0.7033190988423592138 ) ) ;
#22937 = CARTESIAN_POINT ( 'NONE',  ( -0.03769889196559914751, -78.69999999999997442, -3.999822345247594502 ) ) ;
#22938 = AXIS2_PLACEMENT_3D ( 'NONE', #16879, #30143, #48753 ) ;
#22939 = CARTESIAN_POINT ( 'NONE',  ( 10.00844281756000065, -55.43109810584000030, 7.647097920671999560 ) ) ;
#22940 = EDGE_CURVE ( 'NONE', #51133, #4628, #23862, .T. ) ;
#22941 = CARTESIAN_POINT ( 'NONE',  ( -7.705142895619999877, -20.24916621771999914, -10.24998526317999925 ) ) ;
#22942 = CARTESIAN_POINT ( 'NONE',  ( -8.179414028884684384, -24.74093020613540617, 9.502908389705549297 ) ) ;
#22943 = VECTOR ( 'NONE', #58116, 1000.000000000000000 ) ;
#22944 = EDGE_CURVE ( 'NONE', #8584, #47685, #15770, .T. ) ;
#22945 = CARTESIAN_POINT ( 'NONE',  ( -1.750000000001000089, -55.54999998977000075, 12.56594317853999954 ) ) ;
#22946 = CARTESIAN_POINT ( 'NONE',  ( -11.06076315228000340, -78.11862656061613563, 4.601693484369000053 ) ) ;
#22947 = CARTESIAN_POINT ( 'NONE',  ( -1.239656168602880193, -78.71434633308196283, -9.167881758628666944 ) ) ;
#22948 = CARTESIAN_POINT ( 'NONE',  ( 1.980464483675000054, -21.75560170741999855, -12.85140862641999959 ) ) ;
#22949 = CARTESIAN_POINT ( 'NONE',  ( -0.1963495408493606265, -80.01458333333334849, -1.500000000000000222 ) ) ;
#22950 = CYLINDRICAL_SURFACE ( 'NONE', #3179, 9.599999999999999645 ) ;
#22951 = CARTESIAN_POINT ( 'NONE',  ( 0.000000000000000000, -76.19999999999998863, 0.000000000000000000 ) ) ;
#22952 = DIRECTION ( 'NONE',  ( 0.000000000000000000, 1.000000000000000000, 0.000000000000000000 ) ) ;
#22953 = CARTESIAN_POINT ( 'NONE',  ( -3.959059990207000723, -79.88453455456799190, 0.1783950617379000125 ) ) ;
#22954 = CARTESIAN_POINT ( 'NONE',  ( 1.250000000000000000, -79.75000000000000000, 0.000000000000000000 ) ) ;
#22955 = DIRECTION ( 'NONE',  ( 0.000000000000000000, -1.000000000000000000, 0.000000000000000000 ) ) ;
#22956 = CARTESIAN_POINT ( 'NONE',  ( 0.8445585116436000739, -24.71040443242999984, 12.43380736237000050 ) ) ;
#22957 = CARTESIAN_POINT ( 'NONE',  ( 0.7980979214679511102, -81.57372931353624779, 1.057891434376452500 ) ) ;
#22958 = CARTESIAN_POINT ( 'NONE',  ( 3.425937024882473377E-06, -77.82827182887865547, -1.422119424801547627 ) ) ;
#22959 = EDGE_CURVE ( 'NONE', #42525, #45004, #33140, .T. ) ;
#22960 = CARTESIAN_POINT ( 'NONE',  ( 1.997783339681999948, -1.048587262671999865, -3.414494216060000475 ) ) ;
#22961 = CARTESIAN_POINT ( 'NONE',  ( -10.75000000000000000, -78.10000000000000853, 0.000000000000000000 ) ) ;
#22962 = CARTESIAN_POINT ( 'NONE',  ( 10.21380041493999968, -56.02847221959000024, 7.668936932630000314 ) ) ;
#22963 = CARTESIAN_POINT ( 'NONE',  ( -1.886823409076000102, -23.76319684362000118, -12.68610076205999881 ) ) ;
#22964 = CARTESIAN_POINT ( 'NONE',  ( -0.1240015960471890777, -78.48315057415604201, 1.244361994668307769 ) ) ;
#22965 = DIRECTION ( 'NONE',  ( 0.000000000000000000, -1.000000000000000000, 0.000000000000000000 ) ) ;
#22966 = CARTESIAN_POINT ( 'NONE',  ( 0.000000000000000000, -0.6500000000000000222, -3.599999999999761613 ) ) ;
#22967 = CARTESIAN_POINT ( 'NONE',  ( -0.7681833999686432657, -80.57291666666668561, -0.9995835529977258327 ) ) ;
#22968 = CARTESIAN_POINT ( 'NONE',  ( -9.781286103897478768, -77.48590718889759899, -4.665239663755555100 ) ) ;
#22969 = DIRECTION ( 'NONE',  ( 0.000000000000000000, 1.000000000000000000, 0.000000000000000000 ) ) ;
#22971 = CARTESIAN_POINT ( 'NONE',  ( -1.411465571349000081, -79.30477463579200048, -0.1328074485833999896 ) ) ;
#22970 = DIRECTION ( 'NONE',  ( 0.000000000000000000, 1.000000000000000000, 0.000000000000000000 ) ) ;
#22972 = CARTESIAN_POINT ( 'NONE',  ( -0.4275916205537000359, -81.60338596081999185, 1.526944760756999919 ) ) ;
#22973 = ORIENTED_EDGE ( 'NONE', *, *, #20588, .T. ) ;
#22974 = CARTESIAN_POINT ( 'NONE',  ( 2.055825304754000271, -82.99146544543100390, 3.144024286863999595 ) ) ;
#22975 = VECTOR ( 'NONE', #48119, 1000.000000000000114 ) ;
#22976 = ADVANCED_FACE ( 'NONE', ( #23714 ), #22371, .T. ) ;
#22977 = CARTESIAN_POINT ( 'NONE',  ( 2.308634773277999930, -80.71514956827684273, -10.81215905564999957 ) ) ;
#22978 = CARTESIAN_POINT ( 'NONE',  ( -1.980532758766000212, -56.03743349309000621, -12.80088938803999810 ) ) ;
#22979 = CARTESIAN_POINT ( 'NONE',  ( 0.3254755831213840822, -85.09791667550392447, -3.428796880094302946 ) ) ;
#22980 = CARTESIAN_POINT ( 'NONE',  ( 12.77562786365999870, -53.53761952105000432, -0.5426593252874000184 ) ) ;
#22981 = CARTESIAN_POINT ( 'NONE',  ( -7.229693382246000333, -78.88762021447698203, -6.526195624661000672 ) ) ;
#22982 = CARTESIAN_POINT ( 'NONE',  ( -3.383423064118999957, -0.8512077160052000657, -2.181280105692999793 ) ) ;
#22983 = CARTESIAN_POINT ( 'NONE',  ( 8.485281374238999419, -60.04999999966999980, 8.485281374238999419 ) ) ;
#22984 = CARTESIAN_POINT ( 'NONE',  ( -8.179414027356866512, -61.54093020445927209, 9.502908391262463894 ) ) ;
#22985 = CARTESIAN_POINT ( 'NONE',  ( -4.639000034858584698, -77.00000000000001421, 8.062223707945781470 ) ) ;
#22986 = ORIENTED_EDGE ( 'NONE', *, *, #40043, .F. ) ;
#22987 = DIRECTION ( 'NONE',  ( 0.000000000000000000, -1.000000000000000000, 0.000000000000000000 ) ) ;
#22988 = CARTESIAN_POINT ( 'NONE',  ( 0.000000000000000000, -74.64999999999999147, 0.000000000000000000 ) ) ;
#22989 = CARTESIAN_POINT ( 'NONE',  ( 12.00000000000000000, -23.25000000000000000, 0.000000000000000000 ) ) ;
#22990 = CARTESIAN_POINT ( 'NONE',  ( -0.1120320062231000002, -77.75264599861779402, -1.328911429676000067 ) ) ;
#22991 = CARTESIAN_POINT ( 'NONE',  ( -12.60552511012999943, -60.08917723397000543, -1.799501877793999949 ) ) ;
#22992 = DIRECTION ( 'NONE',  ( 0.000000000000000000, 0.000000000000000000, -1.000000000000000000 ) ) ;
#22993 = ORIENTED_EDGE ( 'NONE', *, *, #54655, .F. ) ;
#22994 = CARTESIAN_POINT ( 'NONE',  ( 10.68751571525999999, -77.76749638891799066, 3.388774203076999836 ) ) ;
#22995 = CARTESIAN_POINT ( 'NONE',  ( 10.07627163191000008, -55.55000000278000272, 7.601397897754999633 ) ) ;
#22996 = ORIENTED_EDGE ( 'NONE', *, *, #38488, .T. ) ;
#22997 = VERTEX_POINT ( 'NONE', #23424 ) ;
#22998 = LINE ( 'NONE', #13841, #32988 ) ;
#22999 = CARTESIAN_POINT ( 'NONE',  ( -8.396223008680999911, -80.05298179846350592, -4.990405176070999538 ) ) ;
#23000 = AXIS2_PLACEMENT_3D ( 'NONE', #830, #36223, #40660 ) ;
#23001 = VERTEX_POINT ( 'NONE', #1302 ) ;
#23002 = CARTESIAN_POINT ( 'NONE',  ( -10.81540289212000161, -76.16212020995099863, -5.719638876297000074 ) ) ;
#23003 = CARTESIAN_POINT ( 'NONE',  ( 0.000000000000000000, -77.50000000000000000, 0.000000000000000000 ) ) ;
#23004 = CARTESIAN_POINT ( 'NONE',  ( -0.1733946080540000045, -79.15336183579998419, 1.639152535173999947 ) ) ;
#23005 = EDGE_LOOP ( 'NONE', ( #7470, #39053, #4978, #8760 ) ) ;
#23006 = CARTESIAN_POINT ( 'NONE',  ( -1.269916711065999904, -77.18427305011499584, -9.409822520238998678 ) ) ;
#23007 = CARTESIAN_POINT ( 'NONE',  ( 0.000000000000000000, -78.00000000000000000, 0.000000000000000000 ) ) ;
#23008 = CARTESIAN_POINT ( 'NONE',  ( 1.148914256626027530, -80.31786800289191319, -0.4925239578509333360 ) ) ;
#23009 = CARTESIAN_POINT ( 'NONE',  ( 5.622921568558999716, -77.92073543972999516, 11.67242091225999978 ) ) ;
#23010 = CARTESIAN_POINT ( 'NONE',  ( -3.437187628289000152, -78.54828564256808932, 7.107975105357999081E-08 ) ) ;
#23011 = AXIS2_PLACEMENT_3D ( 'NONE', #12593, #39744, #57180 ) ;
#23012 = CARTESIAN_POINT ( 'NONE',  ( 8.991799503152567041, -79.86894767324388056, 2.169986940879844894 ) ) ;
#23013 = CARTESIAN_POINT ( 'NONE',  ( -1.107038077825813316, -79.00833331572410145, -3.857210535151066821 ) ) ;
#23014 = ORIENTED_EDGE ( 'NONE', *, *, #35413, .T. ) ;
#23015 = CARTESIAN_POINT ( 'NONE',  ( -3.591972190522999764, -77.15527870113453446, 8.980252640667000463 ) ) ;
#23016 = CARTESIAN_POINT ( 'NONE',  ( 2.968291740961590985, -77.25116615474895809, -8.760739757934345562 ) ) ;
#23017 = CARTESIAN_POINT ( 'NONE',  ( -0.9624967649451999785, -80.91976366365300066, -1.086495216026000188 ) ) ;
#23018 = CARTESIAN_POINT ( 'NONE',  ( -0.5814085523173397885, -2.237425844885325699, 3.471270272878386631 ) ) ;
#23019 = CARTESIAN_POINT ( 'NONE',  ( 8.260136572142000588, -61.74034376533999335, -9.643347111204001010 ) ) ;
#23020 = CARTESIAN_POINT ( 'NONE',  ( -11.38660623898999980, -79.04761274831000151, -4.554589311945999697 ) ) ;
#23021 = CARTESIAN_POINT ( 'NONE',  ( -3.699256142337000064, -77.10103114088899190, 11.71059914860999918 ) ) ;
#23022 = CARTESIAN_POINT ( 'NONE',  ( -3.453171399369999950, -1.763032031398999999, -0.5706200895263999762 ) ) ;
#23023 = EDGE_CURVE ( 'NONE', #44068, #13297, #720, .T. ) ;
#23024 = CARTESIAN_POINT ( 'NONE',  ( -1.220391020831000040, -77.26433998579800289, 9.660389656331998864 ) ) ;
#23025 = CARTESIAN_POINT ( 'NONE',  ( 5.911099458924215178, -77.21592629394673679, -10.46277219946754400 ) ) ;
#23026 = FACE_OUTER_BOUND ( 'NONE', #57989, .T. ) ;
#23027 = EDGE_LOOP ( 'NONE', ( #13175, #50491, #8032, #12852 ) ) ;
#23028 = CARTESIAN_POINT ( 'NONE',  ( 1.413069887183999951, -82.10586534759998756, -0.7194652256120001033 ) ) ;
#23029 = CARTESIAN_POINT ( 'NONE',  ( -0.3271710452716786732, -78.70441584275798164, -1.250829328336668045 ) ) ;
#23030 = CARTESIAN_POINT ( 'NONE',  ( -0.6295237254636286695, -79.41666666666665719, 1.092232985442819881 ) ) ;
#23031 = CARTESIAN_POINT ( 'NONE',  ( -8.885616033064000163, -77.93981403858299473, 8.035041515002001589 ) ) ;
#23032 = CARTESIAN_POINT ( 'NONE',  ( 2.943243612629382611, -76.94999999999997442, -9.063334067170245589 ) ) ;
#23033 = CARTESIAN_POINT ( 'NONE',  ( 2.241689414777999989, -77.86897245443199722, 11.83936654731000004 ) ) ;
#23034 = CARTESIAN_POINT ( 'NONE',  ( -0.8481231068849000021, -78.89179415034600140, 9.686304223355000076 ) ) ;
#23035 = CARTESIAN_POINT ( 'NONE',  ( 5.436864099232999514, -78.94294275334198119, -8.080855302300999909 ) ) ;
#23036 = CARTESIAN_POINT ( 'NONE',  ( 2.317456097674912563, -76.05899144437520931, 11.51905596437094914 ) ) ;
#23037 = CARTESIAN_POINT ( 'NONE',  ( -10.11939726227999969, -80.05719348725739337, -4.095505467953000078 ) ) ;
#23038 = CARTESIAN_POINT ( 'NONE',  ( -0.4994022981160649577, -85.88547957940600952, 4.016310797290806534 ) ) ;
#23039 = ORIENTED_EDGE ( 'NONE', *, *, #10974, .F. ) ;
#23040 = CARTESIAN_POINT ( 'NONE',  ( 7.639893379697014097, -18.61284423925059173, -10.11462454831195323 ) ) ;
#23041 = EDGE_CURVE ( 'NONE', #39698, #24542, #36995, .T. ) ;
#23042 = CARTESIAN_POINT ( 'NONE',  ( -0.03561181053916687156, -78.40681307243319509, -3.778384671869483125 ) ) ;
#23043 = CARTESIAN_POINT ( 'NONE',  ( -1.407171709420465211, -77.38541666666665719, 10.74999999999999467 ) ) ;
#23044 = CARTESIAN_POINT ( 'NONE',  ( 7.318097147681000614, -79.67353422943199348, -8.179820946710000484 ) ) ;
#23045 = DIRECTION ( 'NONE',  ( 0.000000000000000000, 0.000000000000000000, -1.000000000000000000 ) ) ;
#23046 = DIRECTION ( 'NONE',  ( -3.552713678800000476E-14, -1.000000000000000000, -5.625129991434000464E-14 ) ) ;
#23047 = DIRECTION ( 'NONE',  ( 0.000000000000000000, 0.000000000000000000, 1.000000000000000000 ) ) ;
#23048 = CARTESIAN_POINT ( 'NONE',  ( 7.619712398446999657, -18.59595871862000038, -10.35409979026999849 ) ) ;
#23049 = ORIENTED_EDGE ( 'NONE', *, *, #54218, .T. ) ;
#23050 = CARTESIAN_POINT ( 'NONE',  ( -5.416162833245999231, -79.86166617326099981, -9.874165520190000933 ) ) ;
#23051 = CARTESIAN_POINT ( 'NONE',  ( 11.75000000000000000, -76.95000000000000284, 0.000000000000000000 ) ) ;
#23052 = CARTESIAN_POINT ( 'NONE',  ( 9.750701472721992502, -79.75205468146413068, -6.704702372767138208 ) ) ;
#23053 = CARTESIAN_POINT ( 'NONE',  ( -0.03284966253593384761, -78.48547957940618858, 3.485344415041724098 ) ) ;
#23055 = CARTESIAN_POINT ( 'NONE',  ( 11.50401822733106627, -76.43342449743093425, -2.391363945934446011 ) ) ;
#23054 = AXIS2_PLACEMENT_3D ( 'NONE', #4848, #49129, #8981 ) ;
#23056 = CARTESIAN_POINT ( 'NONE',  ( 10.04848221952999943, -78.59106237267099004, 4.594115663639000147 ) ) ;
#23057 = DIRECTION ( 'NONE',  ( 1.000000000000000000, 0.000000000000000000, 0.000000000000000000 ) ) ;
#23058 = CARTESIAN_POINT ( 'NONE',  ( -9.019406119850758685, -17.00707871055384146, -8.666949039027842971 ) ) ;
#23059 = EDGE_CURVE ( 'NONE', #54879, #36311, #50891, .T. ) ;
#23060 = B_SPLINE_CURVE_WITH_KNOTS ( 'NONE', 3,
 ( #40111, #40413, #58124, #17387, #57830, #8829, #30659, #13544, #4100, #44847, #31535, #48412, #8239, #7949, #4401, #8, #35373, #48695, #22401, #17987, #53398, #22100, #25952, #17686 ),
 .UNSPECIFIED., .F., .F.,
 ( 4, 2, 2, 2, 2, 2, 2, 2, 2, 2, 2, 4 ),
 ( 0.000000000000000000, 0.1250000000000000278, 0.2500000000000000555, 0.3750000000000001110, 0.4375000000000001110, 0.5000000000000001110, 0.6250000000000001110, 0.6875000000000000000, 0.7499999999999998890, 0.8750000000000000000, 0.9375000000000000000, 1.000000000000000000 ),
 .UNSPECIFIED. ) ;
#23061 = CARTESIAN_POINT ( 'NONE',  ( -12.56594317819999951, -55.54999998572999687, -1.750000000000000000 ) ) ;
#23062 = CARTESIAN_POINT ( 'NONE',  ( -10.96690505107538449, -78.45330275085734684, -0.4413756512486020078 ) ) ;
#23063 = CARTESIAN_POINT ( 'NONE',  ( -12.54977961484000026, -25.04832888628999754, -0.03757501521676000211 ) ) ;
#23064 = ORIENTED_EDGE ( 'NONE', *, *, #11689, .T. ) ;
#23065 = ORIENTED_EDGE ( 'NONE', *, *, #5195, .T. ) ;
#23066 = CARTESIAN_POINT ( 'NONE',  ( 10.05419478484149209, -78.82130372894751247, -3.806463643893830184 ) ) ;
#23067 = CARTESIAN_POINT ( 'NONE',  ( -0.5999999999999999778, -5.000000000000000000, 0.5999999999999999778 ) ) ;
#23068 = VERTEX_POINT ( 'NONE', #46768 ) ;
#23069 = DIRECTION ( 'NONE',  ( 0.000000000000000000, -1.000000000000000000, 0.000000000000000000 ) ) ;
#23070 = CARTESIAN_POINT ( 'NONE',  ( 10.31444895689000063, -24.30075145017000082, 7.758883253342000685 ) ) ;
#23071 = CARTESIAN_POINT ( 'NONE',  ( 0.2611009988844999463, -78.26802014218399961, -11.02876811737000118 ) ) ;
#23072 = CARTESIAN_POINT ( 'NONE',  ( 10.00831380746999955, -60.17230364551999600, 7.646786653150000390 ) ) ;
#23073 = CARTESIAN_POINT ( 'NONE',  ( 10.14802651313347681, -76.25255601911207748, -6.771239379213880305 ) ) ;
#23074 = CARTESIAN_POINT ( 'NONE',  ( -7.167702442858890244, -77.47594342440135051, 9.599168351470673599 ) ) ;
#23075 = CARTESIAN_POINT ( 'NONE',  ( 11.21485848424000054, -80.08238791129060985, -0.2123177049684000228 ) ) ;
#23076 = CARTESIAN_POINT ( 'NONE',  ( 9.313025180101760725, -81.00000000000001421, 5.731444158754912088 ) ) ;
#23077 = AXIS2_PLACEMENT_3D ( 'NONE', #4235, #53835, #17818 ) ;
#23078 = EDGE_LOOP ( 'NONE', ( #26628, #46484, #19844, #26458 ) ) ;
#23079 = CARTESIAN_POINT ( 'NONE',  ( 2.853743189567553630E-14, -82.09999999999999432, -10.25000000000000000 ) ) ;
#23080 = EDGE_LOOP ( 'NONE', ( #51042, #41900, #24526 ) ) ;
#23081 = CARTESIAN_POINT ( 'NONE',  ( 2.134072831818245142, -77.45658836226374433, 9.000378734383811974 ) ) ;
#23082 = CARTESIAN_POINT ( 'NONE',  ( 10.94195044575999987, -77.60922867047798945, -1.468969119710000104 ) ) ;
#23083 = AXIS2_PLACEMENT_3D ( 'NONE', #31282, #35724, #22150 ) ;
#23084 = CARTESIAN_POINT ( 'NONE',  ( -1.370379768245999841E-14, -74.59999999999999432, 0.000000000000000000 ) ) ;
#23085 = CARTESIAN_POINT ( 'NONE',  ( 6.983565664416999219, -78.57937843548099011, -6.737990796766999857 ) ) ;
#23086 = CARTESIAN_POINT ( 'NONE',  ( 5.964045881227000301, -75.66430287301000135, 10.18467341643999902 ) ) ;
#23087 = CARTESIAN_POINT ( 'NONE',  ( -1.980584515752000119, -60.06485146591000301, 12.76303204605000197 ) ) ;
#23088 = CARTESIAN_POINT ( 'NONE',  ( -0.6580604922749000441, -79.36225491982999358, -1.488334326434000099 ) ) ;
#23089 = CARTESIAN_POINT ( 'NONE',  ( 3.324665820279027351, -79.45421531254355330, -8.934852078635632466 ) ) ;
#23090 = CARTESIAN_POINT ( 'NONE',  ( -2.919153588227000107, -78.82568030843599161, 10.54354582977000021 ) ) ;
#23091 = EDGE_CURVE ( 'NONE', #12208, #28137, #16136, .T. ) ;
#23092 = VECTOR ( 'NONE', #47094, 1000.000000000000000 ) ;
#23093 = CARTESIAN_POINT ( 'NONE',  ( -9.205846894750999709, -25.00798911347999720, -8.541134278086001785 ) ) ;
#23094 = B_SPLINE_CURVE_WITH_KNOTS ( 'NONE', 3,
 ( #37158, #6161, #36576, #23872, #888, #13846, #55173, #14714, #10603, #5863, #41887, #41303, #54877, #28587, #54599, #15014, #36287, #51054, #1464, #19455, #50175, #31844, #18871, #46631 ),
 .UNSPECIFIED., .F., .F.,
 ( 4, 2, 2, 2, 2, 2, 2, 2, 2, 2, 2, 4 ),
 ( 0.000000000000000000, 0.1250000000000006661, 0.2500000000000013323, 0.3750000000000019984, 0.4375000000000026645, 0.5000000000000033307, 0.6250000000000039968, 0.7500000000000046629, 0.8125000000000049960, 0.8437500000000042188, 0.8750000000000035527, 1.000000000000000000 ),
 .UNSPECIFIED. ) ;
#23095 = CARTESIAN_POINT ( 'NONE',  ( -8.178338515874317594, -60.10416868444268346, 7.356278612544878470 ) ) ;
#23096 = CARTESIAN_POINT ( 'NONE',  ( -1.649271994007999842, -85.62879675702399140, 3.375121960417999833 ) ) ;
#23097 = VERTEX_POINT ( 'NONE', #44327 ) ;
#23098 = EDGE_CURVE ( 'NONE', #51331, #22110, #36051, .T. ) ;
#23099 = CARTESIAN_POINT ( 'NONE',  ( 11.77091756615000051, -79.16735377751798808, -3.626500858022000173 ) ) ;
#23100 = CARTESIAN_POINT ( 'NONE',  ( -5.736890744663000419, -75.99096601409100060, 9.684816437834999903 ) ) ;
#23101 = CARTESIAN_POINT ( 'NONE',  ( 5.302235052053965170, -77.93411949478270628, 9.360072782316642304 ) ) ;
#23102 = CARTESIAN_POINT ( 'NONE',  ( 8.272973658470998970, -78.31955498394898996, -8.664523719228998999 ) ) ;
#23103 = CARTESIAN_POINT ( 'NONE',  ( -10.01676221091000052, -18.79058563473000021, 7.658899961851000526 ) ) ;
#23105 = DIRECTION ( 'NONE',  ( 0.000000000000000000, 1.000000000000000000, 0.000000000000000000 ) ) ;
#23104 = CARTESIAN_POINT ( 'NONE',  ( 10.44944364268402026, -78.22927179638983830, -2.857199357458220401 ) ) ;
#23106 = CARTESIAN_POINT ( 'NONE',  ( -1.199999999999999956, -80.99999999999998579, 7.000000000000000000 ) ) ;
#23107 = CARTESIAN_POINT ( 'NONE',  ( 6.281390822460244827, -80.92560318168439437, 8.723718198624005993 ) ) ;
#23108 = CARTESIAN_POINT ( 'NONE',  ( 4.000000000000000000, -5.000000000000000000, 0.5999999999999999778 ) ) ;
#23109 = CARTESIAN_POINT ( 'NONE',  ( -6.525630976922989213, -85.80681307243297340, -5.366883173815897301 ) ) ;
#23110 = CARTESIAN_POINT ( 'NONE',  ( -6.618456890295999706, -76.96554859108100288, -8.969427176287000592 ) ) ;
#23111 = CYLINDRICAL_SURFACE ( 'NONE', #46050, 0.5000000000000006661 ) ;
#23112 = CARTESIAN_POINT ( 'NONE',  ( 2.021665076779000092, -81.09853749912809917, -10.83880671474999957 ) ) ;
#23113 = ORIENTED_EDGE ( 'NONE', *, *, #37892, .F. ) ;
#23114 = CARTESIAN_POINT ( 'NONE',  ( 2.411445140827727318, -77.00404005906661098, 8.942079950171093472 ) ) ;
#23115 = EDGE_CURVE ( 'NONE', #36426, #57837, #16703, .T. ) ;
#23116 = CARTESIAN_POINT ( 'NONE',  ( -0.9955135976122998498, -2.700810831311999838, 3.839279387930000009 ) ) ;
#23117 = CARTESIAN_POINT ( 'NONE',  ( 2.976864594307000011, -77.34469249641099964, -10.81463766284999828 ) ) ;
#23118 = DIRECTION ( 'NONE',  ( 1.000000000000000000, 0.000000000000000000, 0.000000000000000000 ) ) ;
#23119 = CARTESIAN_POINT ( 'NONE',  ( 7.660431276880000695, -23.19179487662999861, -10.01749742441000102 ) ) ;
#23120 = CARTESIAN_POINT ( 'NONE',  ( 2.428549115787052237, -82.66979164937175995, 3.194813371584084294 ) ) ;
#23121 = CARTESIAN_POINT ( 'NONE',  ( 4.846722427696010804, -79.75000000000000000, -7.911989270330391122 ) ) ;
#23122 = CARTESIAN_POINT ( 'NONE',  ( 12.79895942954000176, -18.19538174383999873, 2.015930660725000045 ) ) ;
#23123 = B_SPLINE_SURFACE_WITH_KNOTS ( 'NONE', 3, 3, ( 
 ( #52933, #12482, #18088, #54397, #13934, #36081, #691, #54100, #31341, #35477, #27210, #45249, #35185, #8634, #4798, #39919, #49679, #22799, #40808 ),
 ( #30761, #31929, #21911, #49974, #45545, #400, #13344, #8340, #40217, #44355, #5090, #53217, #9517, #13642, #36371, #31637, #27504, #48794, #31047 ),
 ( #23086, #57934, #41099, #9225, #22506, #110, #18378, #12765, #4505, #40517, #3909, #26337, #17490, #53508, #13048, #26919, #49082, #49383, #26620 ),
 ( #44656, #4209, #22206, #58228, #17792, #35779, #53808, #8931, #44950, #42562, #975, #54964, #54680, #51432, #18959, #51140, #1261, #15099, #15401 ) ),
 .UNSPECIFIED., .F., .F., .F.,
 ( 4, 4 ),
 ( 4, 1, 1, 1, 1, 1, 1, 1, 1, 1, 1, 1, 1, 1, 1, 1, 4 ),
 ( -0.3708084972812999980, 1.370808497280999960 ),
 ( 0.4876602516776999963, 0.5203093532865000759, 0.5529584548952999334, 0.5856075565039999820, 0.6182566581127999505, 0.6509057597216000302, 0.6835548613303999987, 0.7162039629391000473, 0.7488530645478999048, 0.7815021661566999844, 0.8141512677654999530, 0.8468003693742000015, 0.8794494709829999701, 0.9120985725918000497, 0.9447476742004999872, 0.9773967758092999558, 1.010045877418000115 ),
 .UNSPECIFIED. ) ;
#23124 = PLANE ( 'NONE',  #8824 ) ;
#23125 = CARTESIAN_POINT ( 'NONE',  ( -0.9218200799623775810, -80.42708333333334281, 1.199500263597266247 ) ) ;
#23126 = B_SPLINE_CURVE_WITH_KNOTS ( 'NONE', 3,
 ( #6995, #24999, #47176, #6412, #12009, #6707 ),
 .UNSPECIFIED., .F., .F.,
 ( 4, 2, 4 ),
 ( 0.000000000000000000, 0.5000000000000000000, 1.000000000000000000 ),
 .UNSPECIFIED. ) ;
#23127 = CARTESIAN_POINT ( 'NONE',  ( 8.950130560535999535, -53.59887407320999841, -8.958576480190000524 ) ) ;
#23128 = CARTESIAN_POINT ( 'NONE',  ( 9.707899084501001141, -77.06889346392100038, 5.708822989341999943 ) ) ;
#23129 = CARTESIAN_POINT ( 'NONE',  ( -1.570423240223999928, -80.79746564644000273, -0.5559045111934000083 ) ) ;
#23130 = CARTESIAN_POINT ( 'NONE',  ( -0.5681478814570000146, -78.60956985887999338, -1.191589642135999938 ) ) ;
#23131 = AXIS2_PLACEMENT_3D ( 'NONE', #45396, #32363, #40952 ) ;
#23132 = CARTESIAN_POINT ( 'NONE',  ( -9.467475792354999697, -77.37406124165399035, 1.978357023055999919 ) ) ;
#23133 = CARTESIAN_POINT ( 'NONE',  ( -1.320760026772257456, -83.20951332364732878, 0.7341362115397076504 ) ) ;
#23134 = B_SPLINE_CURVE_WITH_KNOTS ( 'NONE', 3,
 ( #5404, #14546, #32538, #13671 ),
 .UNSPECIFIED., .F., .F.,
 ( 4, 4 ),
 ( 0.000000000000000000, 1.000000000000000000 ),
 .UNSPECIFIED. ) ;
#23135 = CARTESIAN_POINT ( 'NONE',  ( -12.77649794763000024, -62.10831393445000259, -0.06464137375187999079 ) ) ;
#23136 = CARTESIAN_POINT ( 'NONE',  ( -4.985523414424999800, -78.43747757365058249, -9.777963635945001286 ) ) ;
#23137 = DIRECTION ( 'NONE',  ( -1.000000000000000000, 0.000000000000000000, 0.000000000000000000 ) ) ;
#23138 = VERTEX_POINT ( 'NONE', #3597 ) ;
#23139 = CARTESIAN_POINT ( 'NONE',  ( 1.249949556334875034, -81.84594067282965568, -0.07348289510804084657 ) ) ;
#23140 = DIRECTION ( 'NONE',  ( 1.000000000000000000, 0.000000000000000000, 0.000000000000000000 ) ) ;
#23141 = CARTESIAN_POINT ( 'NONE',  ( -11.24501830132000002, -78.81903125994999471, 0.6192963436278000611 ) ) ;
#23142 = CARTESIAN_POINT ( 'NONE',  ( 7.401770473313850296, -55.34844303569387591, 8.137215171344873710 ) ) ;
#23143 = EDGE_LOOP ( 'NONE', ( #49285, #43207, #28140, #50078 ) ) ;
#23144 = ORIENTED_EDGE ( 'NONE', *, *, #7027, .T. ) ;
#23145 = CARTESIAN_POINT ( 'NONE',  ( -1.427657462233000052, -81.95326221706000069, 0.7543074114907001304 ) ) ;
#23146 = CARTESIAN_POINT ( 'NONE',  ( -0.9224894341409000109, -78.71213903957999491, -1.081399571158999873 ) ) ;
#23147 = ORIENTED_EDGE ( 'NONE', *, *, #55384, .T. ) ;
#23149 = EDGE_CURVE ( 'NONE', #27335, #41402, #39607, .T. ) ;
#23148 = ORIENTED_EDGE ( 'NONE', *, *, #49164, .T. ) ;
#23150 = DIRECTION ( 'NONE',  ( 1.000000000000000000, 0.000000000000000000, 0.000000000000000000 ) ) ;
#23151 = CARTESIAN_POINT ( 'NONE',  ( 2.839805762151334179, -1.291666666666666075, 1.636761686205429056 ) ) ;
#23152 = CARTESIAN_POINT ( 'NONE',  ( -0.9876844338732081452, -79.89479165920646153, 3.298423224253481223 ) ) ;
#23153 = CARTESIAN_POINT ( 'NONE',  ( -7.374560639698971798, -76.37291666663053036, -9.596002108778163731 ) ) ;
#23154 = CARTESIAN_POINT ( 'NONE',  ( -3.812492577196000099, -78.97078559807879117, 0.5515665665854999622 ) ) ;
#23155 = CARTESIAN_POINT ( 'NONE',  ( 12.00000000000000000, -18.84999999997999964, -0.7999999999999001243 ) ) ;
#23156 = CARTESIAN_POINT ( 'NONE',  ( -10.44428606408999904, -78.37314678282000102, -6.033606583391000200 ) ) ;
#23157 = ORIENTED_EDGE ( 'NONE', *, *, #3749, .F. ) ;
#23158 = EDGE_LOOP ( 'NONE', ( #40241, #757, #30818, #51208 ) ) ;
#23159 = DIRECTION ( 'NONE',  ( 0.000000000000000000, -1.000000000000000000, 9.177843670233999678E-14 ) ) ;
#23160 = DIRECTION ( 'NONE',  ( -1.000000000000000000, 0.000000000000000000, 0.000000000000000000 ) ) ;
#23161 = CARTESIAN_POINT ( 'NONE',  ( 0.6454797251309331019, -17.11193487860316154, 12.50471521368260497 ) ) ;
#23162 = CARTESIAN_POINT ( 'NONE',  ( 5.927986824875999261, -77.88684073414698616, -7.683077610609999830 ) ) ;
#23163 = DIRECTION ( 'NONE',  ( 0.000000000000000000, 0.000000000000000000, -1.000000000000000000 ) ) ;
#23164 = CARTESIAN_POINT ( 'NONE',  ( -10.18491068059999805, -23.30716934606000024, 7.640030139755999983 ) ) ;
#23165 = CARTESIAN_POINT ( 'NONE',  ( -12.75936573546999853, -77.33770759395000027, -1.003864233875000123 ) ) ;
#23166 = B_SPLINE_SURFACE_WITH_KNOTS ( 'NONE', 3, 3, ( 
 ( #12499, #52949, #34344, #52380, #11366, #15778, #20785, #52093, #16075, #47682, #6631, #34055, #3077, #11651, #11934, #20219, #47964, #47099, #47387 ),
 ( #29628, #24639, #7499, #25497, #42651, #52662, #12216, #2785, #38786, #2218, #38208, #56805, #33770, #29912, #51809, #21072, #29341, #30204, #6919 ),
 ( #20503, #43814, #38499, #39077, #56517, #57085, #3359, #18398, #31064, #8356, #57657, #18106, #13066, #26354, #40828, #22525, #9245, #35496, #48813 ),
 ( #36101, #39935, #12781, #420, #8652, #54118, #4226, #31654, #49698, #13659, #130, #26936, #44373, #40535, #45269, #30497, #3925, #26638, #54416 ) ),
 .UNSPECIFIED., .F., .F., .F.,
 ( 4, 4 ),
 ( 4, 1, 1, 1, 1, 1, 1, 1, 1, 1, 1, 1, 1, 1, 1, 1, 4 ),
 ( -0.1387574078320999993, 1.138757407831999968 ),
 ( -0.006275936313672000021, 0.01412085670576000013, 0.03451764972519000274, 0.05491444274463000430, 0.07531123576405999998, 0.09570802878349000953, 0.1161048218028999934, 0.1365016148224000025, 0.1568984078418000083, 0.1772952008611999863, 0.1976919938806999955, 0.2180887869001000012, 0.2384855799195000070, 0.2588823729390000161, 0.2792791659584000219, 0.2996759589778000277, 0.3200727519973000090 ),
 .UNSPECIFIED. ) ;
#23167 = CARTESIAN_POINT ( 'NONE',  ( 0.6650966107743999656, -80.48093781866000995, 1.309234371339000225 ) ) ;
#23168 = STYLED_ITEM ( 'NONE', ( #43229 ), #36141 ) ;
#23169 = DIRECTION ( 'NONE',  ( 1.000000000000000000, 0.000000000000000000, 0.000000000000000000 ) ) ;
#23170 = DIRECTION ( 'NONE',  ( 0.7071067811865475727, 0.000000000000000000, -0.7071067811865475727 ) ) ;
#23172 = EDGE_CURVE ( 'NONE', #1755, #56911, #37240, .T. ) ;
#23171 = B_SPLINE_CURVE_WITH_KNOTS ( 'NONE', 3,
 ( #737, #31685, #23139, #18136, #54447, #41146, #44405, #5140, #57983, #31094, #36133, #45000, #4556, #13098, #54149, #49433, #8983, #22846, #39970, #35830, #17540, #12813, #9275, #26968, #27263, #35531, #50022, #44704, #450, #36420, #18431, #53559, #27552, #18718, #36713, #30811, #48843, #4258, #22255, #40269, #50896, #10746, #41730, #6003, #46475, #10440, #6298, #37585, #28133, #24310, #42614, #15151, #55603, #29022, #42324, #11039, #19008, #37292, #9861, #37000, #1893, #24600, #19885, #46184, #42027, #47060, #55308, #14854, #1309, #32849, #1595, #2178, #37878, #1026, #55899, #15453, #33145, #14563, #19585, #20179, #24008, #14270, #51190, #28721, #27843, #33444, #46774, #32557, #51481, #23719, #6590, #28427, #32268, #54726, #50313, #45888, #5421, #23430 ),
 .UNSPECIFIED., .F., .F.,
 ( 4, 2, 2, 2, 1, 1, 2, 2, 2, 1, 1, 1, 2, 2, 2, 2, 2, 2, 2, 2, 1, 1, 1, 2, 2, 2, 2, 2, 1, 1, 1, 2, 2, 2, 2, 2, 1, 1, 1, 2, 2, 2, 2, 2, 1, 1, 1, 2, 2, 2, 2, 2, 1, 1, 1, 2, 2, 2, 4 ),
 ( 0.000000000000000000, 0.06250000000005537237, 0.09375000000008305856, 0.1093750000000968947, 0.1171875000001040279, 0.1210937500001075945, 0.1230468750001091766, 0.1250000000001107725, 0.1562500000001333378, 0.1718750000001446621, 0.1796875000001502964, 0.1835937500001527667, 0.1855468750001543765, 0.1875000000001559586, 0.2187500000001829925, 0.2343750000001968703, 0.2500000000002107203, 0.3125000000002646772, 0.3437500000002917111, 0.3593750000003052003, 0.3671875000003119727, 0.3710937500003154699, 0.3730468750003171352, 0.3740234375003181899, 0.3750000000003193001, 0.4375000000002924883, 0.4687500000002794431, 0.4843750000002731704, 0.4921875000002697842, 0.4960937500002681744, 0.4980468750002673417, 0.4990234375002667311, 0.5000000000002661205, 0.5625000000002297051, 0.5937500000002110534, 0.6093750000002020606, 0.6171875000001972866, 0.6210937500001948441, 0.6230468750001939560, 0.6240234375001935119, 0.6250000000001929568, 0.6875000000001660894, 0.7187500000001526557, 0.7343750000001459943, 0.7421875000001429967, 0.7460937500001416645, 0.7480468750001411093, 0.7490234375001408873, 0.7500000000001406653, 0.8125000000000772715, 0.8437500000000451861, 0.8593750000000291989, 0.8671875000000212053, 0.8710937500000168754, 0.8730468750000147660, 0.8740234375000135447, 0.8750000000000122125, 0.9375000000000061062, 1.000000000000000000 ),
 .UNSPECIFIED. ) ;
#23173 = CARTESIAN_POINT ( 'NONE',  ( 3.275350148889000224, -80.77793935167099448, -2.584986284871999551 ) ) ;
#23174 = CARTESIAN_POINT ( 'NONE',  ( -9.578166812159000898, -80.22198985418920358, 5.930253639820000089 ) ) ;
#23175 = CARTESIAN_POINT ( 'NONE',  ( 6.644622036202999737, -78.25581001420199811, -7.049129409659999901 ) ) ;
#23176 = CARTESIAN_POINT ( 'NONE',  ( 2.905579743612289878, -2.888279987876714916, 1.454858905742103747 ) ) ;
#23177 = CARTESIAN_POINT ( 'NONE',  ( 11.58335411283808902, -76.19322916655099220, -3.113814941787591994 ) ) ;
#23178 = B_SPLINE_CURVE_WITH_KNOTS ( 'NONE', 3,
 ( #51082, #28030, #41918, #6186, #41623, #1202, #54628, #19775, #24198, #49915, #54339, #19194, #55200, #37186, #18901, #23327, #54905, #42215, #27447, #1490, #36893, #13878, #14743, #27737 ),
 .UNSPECIFIED., .F., .F.,
 ( 4, 2, 2, 2, 2, 2, 2, 2, 2, 2, 2, 4 ),
 ( 0.000000000000000000, 0.1250000000000006939, 0.2500000000000013878, 0.3750000000000016653, 0.4375000000000018319, 0.5000000000000018874, 0.6250000000000022204, 0.7500000000000025535, 0.8125000000000027756, 0.8437500000000022204, 0.8750000000000017764, 1.000000000000000000 ),
 .UNSPECIFIED. ) ;
#23179 = AXIS2_PLACEMENT_3D ( 'NONE', #39368, #49990, #41409 ) ;
#23180 = CARTESIAN_POINT ( 'NONE',  ( -0.9151233253627000241, -78.33048166178321026, -0.9701162038759999495 ) ) ;
#23181 = DIRECTION ( 'NONE',  ( 0.000000000000000000, 1.000000000000000000, 0.000000000000000000 ) ) ;
#23182 = CARTESIAN_POINT ( 'NONE',  ( 6.391066299911739357, -79.99999999999998579, -7.100169416382021481 ) ) ;
#23183 = CARTESIAN_POINT ( 'NONE',  ( 3.542727183245000244, -3.072224769576999748, -1.391102635753999950 ) ) ;
#23184 = CARTESIAN_POINT ( 'NONE',  ( -1.092232985442822102, -79.04166666666662877, -0.6295237254636245616 ) ) ;
#23185 = ORIENTED_EDGE ( 'NONE', *, *, #13106, .T. ) ;
#23186 = CARTESIAN_POINT ( 'NONE',  ( 0.4515105396429240914, -23.54721902467404959, 10.99076531923714661 ) ) ;
#23187 = DIRECTION ( 'NONE',  ( -1.000000000000000000, 0.000000000000000000, 0.000000000000000000 ) ) ;
#23188 = CARTESIAN_POINT ( 'NONE',  ( -5.539808784079909287, -79.11666666666667425, 9.611650271896829523 ) ) ;
#23189 = EDGE_CURVE ( 'NONE', #10285, #24723, #40779, .T. ) ;
#23190 = CARTESIAN_POINT ( 'NONE',  ( 7.919239162352998740, -79.52960703100998785, -5.689950727604999869 ) ) ;
#23191 = CARTESIAN_POINT ( 'NONE',  ( -3.201433918554999813, -77.91211383888000341, 12.61309089657999927 ) ) ;
#23192 = CARTESIAN_POINT ( 'NONE',  ( -7.605077663679784550, -79.53769900547050042, 7.597564707201073908 ) ) ;
#23193 = DIRECTION ( 'NONE',  ( 0.000000000000000000, 1.000000000000000000, 0.000000000000000000 ) ) ;
#23194 = CARTESIAN_POINT ( 'NONE',  ( 11.16700323483553348, -78.47423932945110892, 3.653994498481349495 ) ) ;
#23195 = EDGE_LOOP ( 'NONE', ( #17928, #2602, #43232, #57338 ) ) ;
#23196 = FACE_BOUND ( 'NONE', #25881, .T. ) ;
#23197 = CARTESIAN_POINT ( 'NONE',  ( 10.99516458417999942, -77.41144710480799063, -2.492447527329999968 ) ) ;
#23198 = CARTESIAN_POINT ( 'NONE',  ( 1.137028337533999789, -81.99707919315601146, -0.8312398915222000140 ) ) ;
#23199 = CARTESIAN_POINT ( 'NONE',  ( 7.655555357433999397, -22.77795407709999864, -10.38646360829000059 ) ) ;
#23200 = CARTESIAN_POINT ( 'NONE',  ( -4.341134711875000107, -79.10767126595499121, -8.352589043283000336 ) ) ;
#23202 = CARTESIAN_POINT ( 'NONE',  ( -0.7824435345810000220, -1.673265174611999972, 3.939770163431000061 ) ) ;
#23201 = CARTESIAN_POINT ( 'NONE',  ( 4.129629397805000046, -82.25792565754399277, -0.06497024241327999106 ) ) ;
#23203 = CARTESIAN_POINT ( 'NONE',  ( -1.667916687244999974, -55.50150862742999891, -12.49168433577000137 ) ) ;
#23204 = CARTESIAN_POINT ( 'NONE',  ( 1.157603047269999852, -79.94787091841099880, 0.6328671228825999417 ) ) ;
#23205 = EDGE_LOOP ( 'NONE', ( #12038, #48759, #37897, #37742, #27745 ) ) ;
#23206 = CARTESIAN_POINT ( 'NONE',  ( -3.830267234649249897, -77.19605609133061819, -10.04658309097634650 ) ) ;
#23207 = DIRECTION ( 'NONE',  ( -1.000000000000000000, 0.000000000000000000, 0.000000000000000000 ) ) ;
#23208 = VERTEX_POINT ( 'NONE', #17762 ) ;
#23209 = ORIENTED_EDGE ( 'NONE', *, *, #19142, .F. ) ;
#23210 = CARTESIAN_POINT ( 'NONE',  ( 10.68099162494999987, -79.63817051509798262, 2.367326398803000220 ) ) ;
#23211 = CARTESIAN_POINT ( 'NONE',  ( 0.000000000000000000, -39.49523982883999906, 0.000000000000000000 ) ) ;
#23212 = FACE_OUTER_BOUND ( 'NONE', #56420, .T. ) ;
#23213 = VERTEX_POINT ( 'NONE', #12737 ) ;
#23214 = CARTESIAN_POINT ( 'NONE',  ( -10.93129665128000028, -77.72569360493399415, -5.069765792968000007 ) ) ;
#23215 = EDGE_LOOP ( 'NONE', ( #49805, #10416, #7546, #18497 ) ) ;
#23216 = AXIS2_PLACEMENT_3D ( 'NONE', #38645, #48670, #39509 ) ;
#23218 = ADVANCED_FACE ( 'NONE', ( #31310 ), #49649, .F. ) ;
#23217 = ORIENTED_EDGE ( 'NONE', *, *, #531, .F. ) ;
#23219 = CARTESIAN_POINT ( 'NONE',  ( -2.921860942912723580, -2.637121803128768871, -1.423448106538530267 ) ) ;
#23220 = AXIS2_PLACEMENT_3D ( 'NONE', #31268, #4732, #36008 ) ;
#23221 = EDGE_CURVE ( 'NONE', #13012, #2890, #11959, .T. ) ;
#23222 = B_SPLINE_SURFACE_WITH_KNOTS ( 'NONE', 3, 3, ( 
 ( #721, #45576, #18698, #23119 ),
 ( #10422, #36692, #51170, #42005 ),
 ( #10724, #14545, #28702, #46164 ),
 ( #46753, #33425, #15431, #5689 ),
 ( #18990, #1287, #46454, #5982 ),
 ( #6272, #42305, #23989, #19567 ),
 ( #24289, #27824, #32247, #11016 ),
 ( #41126, #1872, #55881, #37860 ),
 ( #5403, #50291, #45870, #41422 ),
 ( #1005, #19281, #36982, #54996 ),
 ( #10138, #28113, #47040, #38442 ),
 ( #6570, #25442, #12160, #52609 ),
 ( #29571, #6861, #56459, #20732 ),
 ( #16013, #7443, #39021, #56749 ),
 ( #57033, #34290, #33716, #24581 ),
 ( #7150, #30146, #38730, #34576 ),
 ( #43461, #48196, #42597, #16592 ) ),
 .UNSPECIFIED., .F., .F., .F.,
 ( 4, 1, 1, 1, 1, 1, 1, 1, 1, 1, 1, 1, 1, 1, 4 ),
 ( 4, 4 ),
 ( -0.01011786823680000010, 0.000000000000000000, 0.08333333333333001192, 0.1666666666667000196, 0.2500000000000000000, 0.3333333333333000081, 0.4166666666666999919, 0.5000000000000000000, 0.5833333333333000637, 0.6666666666667000474, 0.7500000000000000000, 0.8333333333333000637, 0.9166666666667000474, 1.000000000000000000, 1.010371592463000123 ),
 ( -0.3559705548529999986, 1.357613344742000017 ),
 .UNSPECIFIED. ) ;
#23223 = CARTESIAN_POINT ( 'NONE',  ( -7.320008597215652557, -76.47238134542388366, -9.541710111217275525 ) ) ;
#23224 = CARTESIAN_POINT ( 'NONE',  ( 9.231185137975039368, -79.16876909680533458, 2.269161111927250563 ) ) ;
#23225 = ORIENTED_EDGE ( 'NONE', *, *, #48378, .F. ) ;
#23226 = CARTESIAN_POINT ( 'NONE',  ( 0.8837568277754281887, -82.78815962236846815, -0.8834506328319239321 ) ) ;
#23227 = CONICAL_SURFACE ( 'NONE', #30742, 2.699999999213000379, 0.7853981633972997312 ) ;
#23228 = ORIENTED_EDGE ( 'NONE', *, *, #42573, .F. ) ;
#23229 = CARTESIAN_POINT ( 'NONE',  ( -6.606377239730330864, -80.57291666666665719, -8.596418555780440229 ) ) ;
#23230 = CARTESIAN_POINT ( 'NONE',  ( 8.445116086859872695, -78.14089606339597083, 4.780569220243218176 ) ) ;
#23231 = DIRECTION ( 'NONE',  ( 1.000000000000000000, 0.000000000000000000, 0.000000000000000000 ) ) ;
#23232 = CARTESIAN_POINT ( 'NONE',  ( -12.02332076413289208, -78.43441775370509106, 2.418180990960641541 ) ) ;
#23233 = CARTESIAN_POINT ( 'NONE',  ( -7.695020077040999773, -76.13370154875299534, 8.115451295621999961 ) ) ;
#23234 = CARTESIAN_POINT ( 'NONE',  ( 11.74999999999999289, -77.06041666666664014, 1.538071403320028452 ) ) ;
#23235 = CARTESIAN_POINT ( 'NONE',  ( 1.538071403319964281, -78.66458333333332575, 11.75000000000000711 ) ) ;
#23236 = CARTESIAN_POINT ( 'NONE',  ( -7.668936932637000048, -59.57152778012000027, -10.21380041493999968 ) ) ;
#23237 = CARTESIAN_POINT ( 'NONE',  ( 0.6886906644032062541, -78.73113614952505657, -9.226155803845061953 ) ) ;
#23238 = CARTESIAN_POINT ( 'NONE',  ( 11.31056051666590889, -76.47239290234516318, 3.271005276656067107 ) ) ;
#23239 = CARTESIAN_POINT ( 'NONE',  ( 7.601898381947000516, -77.37083501420200093, 5.548685371626999263 ) ) ;
#23240 = CARTESIAN_POINT ( 'NONE',  ( -1.327128730425999992, -79.62647662016500760, 0.1315503032697999675 ) ) ;
#23241 = CARTESIAN_POINT ( 'NONE',  ( -7.310560282016263400, -80.16762514998541178, -8.219721594426141920 ) ) ;
#23242 = CARTESIAN_POINT ( 'NONE',  ( 12.18685347097914118, -78.20858279583087835, 0.8549723098153251266 ) ) ;
#23243 = CARTESIAN_POINT ( 'NONE',  ( 4.005932268072999847, -82.24559216449299015, -0.2640443533972999801 ) ) ;
#23244 = CARTESIAN_POINT ( 'NONE',  ( 9.126301671913999769, -77.41671332859898769, -3.143863093112999607 ) ) ;
#23245 = DIRECTION ( 'NONE',  ( 0.000000000000000000, -1.000000000000000000, 2.878889714326999635E-13 ) ) ;
#23246 = CARTESIAN_POINT ( 'NONE',  ( -1.489189600238929989, -77.01250000000003126, -9.412174122262570108 ) ) ;
#23247 = CARTESIAN_POINT ( 'NONE',  ( -0.9212224518303000487, -24.81954101839000160, 12.54670315981999984 ) ) ;
#23248 = DIRECTION ( 'NONE',  ( -1.000000000000000000, 0.000000000000000000, 0.000000000000000000 ) ) ;
#23249 = CARTESIAN_POINT ( 'NONE',  ( 3.618123952455000403, -1.801525618456000011, -0.1863489967816000237 ) ) ;
#23250 = CYLINDRICAL_SURFACE ( 'NONE', #12560, 9.500000000000000000 ) ;
#23251 = DIRECTION ( 'NONE',  ( 0.000000000000000000, 0.7071067811866525998, -0.7071067811864425456 ) ) ;
#23252 = EDGE_CURVE ( 'NONE', #52412, #33741, #45516, .T. ) ;
#23253 = CARTESIAN_POINT ( 'NONE',  ( 10.42274798264000069, -58.55365779174999830, 7.691916945401000127 ) ) ;
#23254 = CARTESIAN_POINT ( 'NONE',  ( -1.666698456700999920, -23.19181739840000134, -12.50018138921000066 ) ) ;
#23255 = CARTESIAN_POINT ( 'NONE',  ( 13.94241845804000057, -69.26002936526001008, 4.312607202219999873E-05 ) ) ;
#23256 = CARTESIAN_POINT ( 'NONE',  ( -1.667474681734999908, -3.461675931787000060, 2.801048656332000064 ) ) ;
#23257 = EDGE_CURVE ( 'NONE', #25542, #891, #3470, .T. ) ;
#23258 = AXIS2_PLACEMENT_3D ( 'NONE', #4389, #49262, #45432 ) ;
#23259 = CARTESIAN_POINT ( 'NONE',  ( 10.73158301355000077, -77.16380270170699873, 5.968995448363000556 ) ) ;
#23260 = CARTESIAN_POINT ( 'NONE',  ( -11.79999999999999893, -23.15000000000999947, -0.5999999999999999778 ) ) ;
#23262 = CARTESIAN_POINT ( 'NONE',  ( -0.2007418666109000160, -78.46711910266039069, -1.502878855747000086 ) ) ;
#23261 = CARTESIAN_POINT ( 'NONE',  ( -1.310679582531389276, -79.85833333333332007, 0.7554284705563443225 ) ) ;
#23263 = CARTESIAN_POINT ( 'NONE',  ( -1.553390134080000040, -82.80356852156999992, -0.6977077157647000316 ) ) ;
#23264 = ORIENTED_EDGE ( 'NONE', *, *, #9288, .T. ) ;
#23265 = CONICAL_SURFACE ( 'NONE', #35501, 10.59999999995999964, 0.7853981633972997312 ) ;
#23266 = CARTESIAN_POINT ( 'NONE',  ( 2.606239186342999670, -83.95732450217400356, -2.468046761181999837 ) ) ;
#23267 = CARTESIAN_POINT ( 'NONE',  ( 10.70141235895999898, -79.33702760564798950, -5.264563250036999875 ) ) ;
#23268 = CARTESIAN_POINT ( 'NONE',  ( 5.141835936095000115, -80.04623191901920620, 10.04998108304999782 ) ) ;
#23269 = AXIS2_PLACEMENT_3D ( 'NONE', #55623, #32287, #19031 ) ;
#23270 = DIRECTION ( 'NONE',  ( 0.000000000000000000, -1.000000000000000000, 0.000000000000000000 ) ) ;
#23271 = CARTESIAN_POINT ( 'NONE',  ( -1.634254835633885516, -84.44270834421041627, 3.031084325246120592 ) ) ;
#23272 = DIRECTION ( 'NONE',  ( 0.000000000000000000, -1.000000000000000000, 0.000000000000000000 ) ) ;
#23273 = CYLINDRICAL_SURFACE ( 'NONE', #36807, 1.750000000000000000 ) ;
#23274 = AXIS2_PLACEMENT_3D ( 'NONE', #16387, #12525, #26096 ) ;
#23275 = CARTESIAN_POINT ( 'NONE',  ( -9.022377653937999398, -77.81737393437001060, -8.854484771337999049 ) ) ;
#23276 = CARTESIAN_POINT ( 'NONE',  ( -4.310687854694967847, -76.39525775715499378, -11.00524620388241814 ) ) ;
#23277 = CARTESIAN_POINT ( 'NONE',  ( -1.923984835444398023, -77.00000000000001421, 9.100276353209897806 ) ) ;
#23278 = ORIENTED_EDGE ( 'NONE', *, *, #25379, .F. ) ;
#23279 = CARTESIAN_POINT ( 'NONE',  ( -0.8898229089153880667, -53.77675468783602497, -12.70296869040735999 ) ) ;
#23280 = CARTESIAN_POINT ( 'NONE',  ( 9.448795662942000462, -79.52248667140099769, 1.876396759601000053 ) ) ;
#23281 = EDGE_CURVE ( 'NONE', #29379, #31775, #44994, .T. ) ;
#23282 = CARTESIAN_POINT ( 'NONE',  ( -3.630949683906000036, -75.80000000000001137, -11.17491406647000041 ) ) ;
#23283 = DIRECTION ( 'NONE',  ( 0.000000000000000000, 0.000000000000000000, 1.000000000000000000 ) ) ;
#23284 = ORIENTED_EDGE ( 'NONE', *, *, #38556, .T. ) ;
#23285 = CARTESIAN_POINT ( 'NONE',  ( 3.606090020748000224, -77.20773208238998109, -10.73262889482999860 ) ) ;
#23286 = CARTESIAN_POINT ( 'NONE',  ( -2.062673488410000200, -18.67547726287999765, 12.82904109062999964 ) ) ;
#23287 = EDGE_LOOP ( 'NONE', ( #3311, #56620, #34234, #1456 ) ) ;
#23288 = ORIENTED_EDGE ( 'NONE', *, *, #13626, .F. ) ;
#23289 = CARTESIAN_POINT ( 'NONE',  ( -1.180289549356538625, -80.57346338427628041, 0.4123096908613480549 ) ) ;
#23290 = EDGE_CURVE ( 'NONE', #57774, #13927, #41073, .T. ) ;
#23291 =( NAMED_UNIT ( * ) SI_UNIT ( $, .STERADIAN. ) SOLID_ANGLE_UNIT ( ) );
#23292 = CARTESIAN_POINT ( 'NONE',  ( 8.985706068735000329, -79.72825521588151787, -3.828549499589000149 ) ) ;
#23293 = ORIENTED_EDGE ( 'NONE', *, *, #25230, .F. ) ;
#23294 = CYLINDRICAL_SURFACE ( 'NONE', #56347, 1.750000000000000000 ) ;
#23295 = CARTESIAN_POINT ( 'NONE',  ( -1.250000000000000000, -82.99999999999998579, 0.000000000000000000 ) ) ;
#23296 = CARTESIAN_POINT ( 'NONE',  ( -1.338663453569000072, -79.24733985637000444, -0.7509245179382000313 ) ) ;
#23297 = CARTESIAN_POINT ( 'NONE',  ( -8.383077572658999443, -77.53104805011500389, 4.458862939031999595 ) ) ;
#23298 = VECTOR ( 'NONE', #26339, 1000.000000000000000 ) ;
#23299 = DIRECTION ( 'NONE',  ( -1.000000000000000000, 0.000000000000000000, 0.000000000000000000 ) ) ;
#23300 = CARTESIAN_POINT ( 'NONE',  ( 10.41144070832756618, -18.47453159777755261, -7.610433246107068506 ) ) ;
#23301 = CARTESIAN_POINT ( 'NONE',  ( -7.710118476714000302, -58.54977139529999164, 10.18499221086999995 ) ) ;
#23302 = CIRCLE ( 'NONE', #35544, 0.5000000000000004441 ) ;
#23303 = DIRECTION ( 'NONE',  ( 0.000000000000000000, 0.7071067811866525998, -0.7071067811864425456 ) ) ;
#23304 = CARTESIAN_POINT ( 'NONE',  ( 8.994180132603776912, -79.86886303493331241, 2.160082921624130403 ) ) ;
#23305 = VECTOR ( 'NONE', #6023, 1000.000000000000000 ) ;
#23306 = CARTESIAN_POINT ( 'NONE',  ( 1.149457566070329673, -79.04350818708034865, -0.9787974342808838379 ) ) ;
#23307 = CARTESIAN_POINT ( 'NONE',  ( 0.7784319255180548458, -79.77916665765043547, 3.975193877679629839 ) ) ;
#23308 = ORIENTED_EDGE ( 'NONE', *, *, #41033, .T. ) ;
#23309 = CARTESIAN_POINT ( 'NONE',  ( -4.784380313523580064, -77.71666666666668277, 8.300970689365431809 ) ) ;
#23310 = CARTESIAN_POINT ( 'NONE',  ( 9.754023262367999436, -76.18045457895999562, -7.509630405475999915 ) ) ;
#23311 = CARTESIAN_POINT ( 'NONE',  ( 1.112922243992000126, -80.04327398392099724, -1.029731144982999780 ) ) ;
#23312 = VECTOR ( 'NONE', #35158, 1000.000000000000000 ) ;
#23313 = FACE_OUTER_BOUND ( 'NONE', #17039, .T. ) ;
#23314 = CARTESIAN_POINT ( 'NONE',  ( -3.047510419343540278, -2.390893416076438349, -1.759566424157797293 ) ) ;
#23315 = CARTESIAN_POINT ( 'NONE',  ( 7.618394338655000375, -60.02713821237000502, -10.53494418060999926 ) ) ;
#23316 = CARTESIAN_POINT ( 'NONE',  ( 10.16243366810999937, -79.25472372342998995, -6.864696462387000153 ) ) ;
#23317 = CARTESIAN_POINT ( 'NONE',  ( 11.75000000000000000, -79.79999999999999716, -4.009019365174000020E-13 ) ) ;
#23318 = DIRECTION ( 'NONE',  ( 1.308348598714000038E-10, -1.000000000000000000, 3.608116327059999754E-10 ) ) ;
#23319 = CARTESIAN_POINT ( 'NONE',  ( 12.50483465194472465, -24.86452578687064019, 0.6958747604659799579 ) ) ;
#23320 = CARTESIAN_POINT ( 'NONE',  ( -8.710754228814030498, -76.98910444386174845, 8.358220830707420390 ) ) ;
#23321 = DIRECTION ( 'NONE',  ( 1.000000000000000000, 0.000000000000000000, 0.000000000000000000 ) ) ;
#23322 = B_SPLINE_CURVE_WITH_KNOTS ( 'NONE', 3,
 ( #38182, #11052, #47654, #7182, #2192, #15750 ),
 .UNSPECIFIED., .F., .F.,
 ( 4, 2, 4 ),
 ( 0.000000000000000000, 0.5000000000000000000, 1.000000000000000000 ),
 .UNSPECIFIED. ) ;
#23323 = ORIENTED_EDGE ( 'NONE', *, *, #35099, .F. ) ;
#23324 = B_SPLINE_CURVE_WITH_KNOTS ( 'NONE', 3,
 ( #28937, #34225, #15949, #47565, #47272, #25378, #46982, #6510 ),
 .UNSPECIFIED., .F., .F.,
 ( 4, 2, 2, 4 ),
 ( 0.000000000000000000, 0.4999999999999971134, 0.7499999999999985567, 1.000000000000000000 ),
 .UNSPECIFIED. ) ;
#23325 = CARTESIAN_POINT ( 'NONE',  ( 1.250322495222000008, -82.80093166112899894, 0.5125084194436000384 ) ) ;
#23326 = CARTESIAN_POINT ( 'NONE',  ( -0.4297501350614000293, -80.92073041130998945, 1.281126864269000132 ) ) ;
#23327 = CARTESIAN_POINT ( 'NONE',  ( 7.921335223404320836, -24.55094696616630401, 10.04563431748756130 ) ) ;
#23328 = CARTESIAN_POINT ( 'NONE',  ( 1.249999999999999778, -82.76041666666665719, 0.1636246173744711763 ) ) ;
#23329 = CARTESIAN_POINT ( 'NONE',  ( 6.017032375295198854, -77.00000000000000000, 7.093946000275482611 ) ) ;
#23330 = CARTESIAN_POINT ( 'NONE',  ( 3.947980971697000019, -78.35730013205999001, 11.38460442531999917 ) ) ;
#23331 = CARTESIAN_POINT ( 'NONE',  ( -8.614692902062000002, -77.17363726482008701, 3.831263898871999807 ) ) ;
#23332 = CARTESIAN_POINT ( 'NONE',  ( 0.04984446912208501806, -76.07435069114738724, 11.74969986336399153 ) ) ;
#23333 = CARTESIAN_POINT ( 'NONE',  ( 4.576365007000999796, -79.11790344678600206, -10.03785921918999868 ) ) ;
#23334 = CARTESIAN_POINT ( 'NONE',  ( -3.131568623105716043, -86.07390000031791999, 1.324114027860883613 ) ) ;
#23335 = VERTEX_POINT ( 'NONE', #19807 ) ;
#23336 = DIRECTION ( 'NONE',  ( -1.000000000000000000, 0.000000000000000000, 0.000000000000000000 ) ) ;
#23337 = CARTESIAN_POINT ( 'NONE',  ( 2.060606489177889689, -78.43735717367049176, -3.567929020052158950 ) ) ;
#23338 = CARTESIAN_POINT ( 'NONE',  ( -7.604423127187000198, -79.92636541842598774, 7.914351627518998455 ) ) ;
#23339 = LINE ( 'NONE', #54920, #6282 ) ;
#23340 = CARTESIAN_POINT ( 'NONE',  ( 6.084904940690000430, -76.03885294825599317, -10.92373034159999889 ) ) ;
#23341 = CARTESIAN_POINT ( 'NONE',  ( 0.000000000000000000, 0.000000000000000000, 12.00000000000000000 ) ) ;
#23342 = CARTESIAN_POINT ( 'NONE',  ( 10.36289663187999999, -18.79893657682999830, -7.633501051924000080 ) ) ;
#23343 = CARTESIAN_POINT ( 'NONE',  ( 13.99936781018472232, -46.09579702914000165, 0.1330447863085613691 ) ) ;
#23344 = VERTEX_POINT ( 'NONE', #9780 ) ;
#23345 = CARTESIAN_POINT ( 'NONE',  ( 3.485296502184999756, -79.05855784779899409, 10.58807389768000107 ) ) ;
#23346 = CARTESIAN_POINT ( 'NONE',  ( 12.71107039379005066, -54.54871969218108063, 1.717622521766782873 ) ) ;
#23347 = CARTESIAN_POINT ( 'NONE',  ( -5.664454919952616407, -79.46458300272750819, 10.39013350000020530 ) ) ;
#23348 = CARTESIAN_POINT ( 'NONE',  ( 2.273238635161466181, -78.48547955770030171, 3.936100089146787884 ) ) ;
#23349 = EDGE_CURVE ( 'NONE', #46033, #41082, #22503, .T. ) ;
#23350 = CARTESIAN_POINT ( 'NONE',  ( 11.28642253013168606, -76.73199622251708263, 4.309372704845956470 ) ) ;
#23351 = CARTESIAN_POINT ( 'NONE',  ( 12.52134121561634750, -60.72745484868493548, 1.618935178750384285 ) ) ;
#23352 = CIRCLE ( 'NONE', #16735, 3.600000000000000089 ) ;
#23353 = CARTESIAN_POINT ( 'NONE',  ( -9.326577543113813817, -76.99999999999998579, -0.5108809166760798215 ) ) ;
#23354 = AXIS2_PLACEMENT_3D ( 'NONE', #8359, #27233, #31657 ) ;
#23355 = CARTESIAN_POINT ( 'NONE',  ( 10.42531124905999995, -23.26485148473999942, 7.624341765453999997 ) ) ;
#23356 = CARTESIAN_POINT ( 'NONE',  ( 0.3926218265389220807, -81.14583333333335702, -1.460959015002473382 ) ) ;
#23357 = DIRECTION ( 'NONE',  ( 0.000000000000000000, 1.000000000000000000, 0.000000000000000000 ) ) ;
#23358 = CARTESIAN_POINT ( 'NONE',  ( 9.981997996688200203, -78.73422629418405450, 4.563719410465792770 ) ) ;
#23359 = ADVANCED_FACE ( 'NONE', ( #33067 ), #9489, .F. ) ;
#23360 = FACE_OUTER_BOUND ( 'NONE', #9577, .T. ) ;
#23361 = ORIENTED_EDGE ( 'NONE', *, *, #51521, .F. ) ;
#23362 = ORIENTED_EDGE ( 'NONE', *, *, #49369, .F. ) ;
#23363 = CARTESIAN_POINT ( 'NONE',  ( -9.193055583834000899, -77.84673998579799559, 3.991918584785999702 ) ) ;
#23364 = CARTESIAN_POINT ( 'NONE',  ( 9.888817398439529782, -78.81797029978375235, -4.217298846466132289 ) ) ;
#23365 = ORIENTED_EDGE ( 'NONE', *, *, #34201, .F. ) ;
#23366 = CARTESIAN_POINT ( 'NONE',  ( 8.999999998907000531, -3.999999998907000087, -1.966783332313999974E-09 ) ) ;
#23367 = CARTESIAN_POINT ( 'NONE',  ( 2.987038927812020184, -83.82604167946361429, -1.712850616285394922 ) ) ;
#23368 = EDGE_CURVE ( 'NONE', #56557, #37071, #25202, .T. ) ;
#23369 = CARTESIAN_POINT ( 'NONE',  ( 7.618386461959000044, -60.02712559312999474, 10.53495196325000016 ) ) ;
#23370 = DIRECTION ( 'NONE',  ( -0.009503199022040095811, 0.000000000000000000, 0.9999548435846228323 ) ) ;
#23371 = CARTESIAN_POINT ( 'NONE',  ( 11.53516957136256416, -78.77815056474238986, -3.234168909645118717 ) ) ;
#23372 = CARTESIAN_POINT ( 'NONE',  ( 2.039250879084999912, -79.97344253928329749, -11.02993955029000084 ) ) ;
#23373 = CARTESIAN_POINT ( 'NONE',  ( 8.136205013521058405, -81.00000000000001421, 7.261636552250462451 ) ) ;
#23374 = ADVANCED_FACE ( 'NONE', ( #23640 ), #12918, .F. ) ;
#23375 = EDGE_LOOP ( 'NONE', ( #28011, #10524, #55239, #38154, #43979 ) ) ;
#23376 = CARTESIAN_POINT ( 'NONE',  ( 7.655984445742698874, -60.50337239307589954, -10.06694410270556617 ) ) ;
#23377 = VERTEX_POINT ( 'NONE', #5923 ) ;
#23378 = CARTESIAN_POINT ( 'NONE',  ( 9.068127558788219744, -77.36599329621280674, 1.827539330042447174 ) ) ;
#23379 = CARTESIAN_POINT ( 'NONE',  ( 6.393001003723999709, -77.25600538349898727, 9.000752526674000720 ) ) ;
#23380 = CARTESIAN_POINT ( 'NONE',  ( 10.81758370320302731, -76.05000000000001137, 2.303648476915329368 ) ) ;
#23381 = CARTESIAN_POINT ( 'NONE',  ( -1.598336519864000049, -78.50327671425300480, -0.2292036100155999956 ) ) ;
#23382 = CARTESIAN_POINT ( 'NONE',  ( 10.48543666025110355, -77.60833333333330586, -6.043427764450775008 ) ) ;
#23383 = CARTESIAN_POINT ( 'NONE',  ( -3.000161766333798496, -2.032779362115749056, -1.313064309588372502 ) ) ;
#23384 = CARTESIAN_POINT ( 'NONE',  ( -1.578837173282999995, -79.25089178026999548, 0.3948290484592000271 ) ) ;
#23385 = CARTESIAN_POINT ( 'NONE',  ( 7.648026768024999811, -18.75000001589999954, -10.12290050218000026 ) ) ;
#23386 = CARTESIAN_POINT ( 'NONE',  ( 4.025753977166000475, -79.58417387541800281, -10.17256709246999868 ) ) ;
#23387 = CARTESIAN_POINT ( 'NONE',  ( 1.667917367010000040, -60.08056692637000396, -12.49306752636999995 ) ) ;
#23388 = CARTESIAN_POINT ( 'NONE',  ( 12.92181194095999963, -58.55648180022999583, -2.062502994258999856 ) ) ;
#23389 = CARTESIAN_POINT ( 'NONE',  ( -0.6763775780641000379, -84.18193230181299214, 3.525089843763999919 ) ) ;
#23390 = ORIENTED_EDGE ( 'NONE', *, *, #51415, .T. ) ;
#23391 = CARTESIAN_POINT ( 'NONE',  ( -12.12831959444000063, -78.89107492802000365, -2.737500678952999422 ) ) ;
#23392 = CARTESIAN_POINT ( 'NONE',  ( 8.153967731313999323, -76.38394096989499360, 7.760240090419999959 ) ) ;
#23393 = CARTESIAN_POINT ( 'NONE',  ( 10.45286035002862768, -77.86879287204392597, 2.509877197284648975 ) ) ;
#23394 = CARTESIAN_POINT ( 'NONE',  ( -8.148905501844000199, -78.63157684660600921, -8.781309899900000104 ) ) ;
#23395 = ADVANCED_FACE ( 'NONE', ( #10667 ), #340, .F. ) ;
#23396 = CARTESIAN_POINT ( 'NONE',  ( -1.636761686205434607, -3.416666666666666519, 2.839805762151332402 ) ) ;
#23398 = DIRECTION ( 'NONE',  ( -0.7071067811865475727, 0.000000000000000000, 0.7071067811865475727 ) ) ;
#23397 = DIRECTION ( 'NONE',  ( 0.4045602624632262945, 0.8201597332662526885, -0.4045602624632262945 ) ) ;
#23399 = AXIS2_PLACEMENT_3D ( 'NONE', #23853, #28271, #27983 ) ;
#23400 = CARTESIAN_POINT ( 'NONE',  ( 2.162570926564036267, -3.427626334641581174, -2.781109552613596492 ) ) ;
#23401 = CARTESIAN_POINT ( 'NONE',  ( 9.227078657215999513, -77.81332916973599367, -1.863387764540999969 ) ) ;
#23402 = CARTESIAN_POINT ( 'NONE',  ( -3.106054555984679055, -86.07390000031791999, 1.382904586457439189 ) ) ;
#23403 = CARTESIAN_POINT ( 'NONE',  ( 11.12204776531999961, -77.64645716612598392, 0.7447510167176000229 ) ) ;
#23404 = DIRECTION ( 'NONE',  ( 0.7071067811865475727, 0.000000000000000000, -0.7071067811865475727 ) ) ;
#23405 = CARTESIAN_POINT ( 'NONE',  ( 7.367354511904000702, -80.70863820267163646, 8.356990619368000139 ) ) ;
#23406 = ORIENTED_EDGE ( 'NONE', *, *, #372, .F. ) ;
#23407 = CARTESIAN_POINT ( 'NONE',  ( -2.712012240502000182, -77.54804903538301630, 9.099584490865000319 ) ) ;
#23408 = CARTESIAN_POINT ( 'NONE',  ( 3.503826891403000410, -2.000465391789000069, 1.486277921227999954 ) ) ;
#23409 = CARTESIAN_POINT ( 'NONE',  ( -4.647088938219000376, -78.17509865373799016, 10.20895072913000057 ) ) ;
#23410 = CARTESIAN_POINT ( 'NONE',  ( -3.548303639235999896, -79.40834838942097917, -10.38621961377000069 ) ) ;
#23411 = FACE_OUTER_BOUND ( 'NONE', #32894, .T. ) ;
#23412 = LINE ( 'NONE', #44982, #12839 ) ;
#23413 = CARTESIAN_POINT ( 'NONE',  ( 0.4261031628618374700, -1.966084445875545095, 3.248887486669486346 ) ) ;
#23414 = DIRECTION ( 'NONE',  ( 1.000000000000000000, -1.534448722697999916E-11, 4.093422659635999854E-14 ) ) ;
#23415 = CARTESIAN_POINT ( 'NONE',  ( -3.902709220513999711, -86.11509620537599119, 1.102229611723000158 ) ) ;
#23416 = CARTESIAN_POINT ( 'NONE',  ( -10.45204383630000144, -19.23743350652000217, -7.651147548127999798 ) ) ;
#23417 = CARTESIAN_POINT ( 'NONE',  ( -12.94500186834999944, -78.49632521500998905, -0.3167920335189999825 ) ) ;
#23418 = B_SPLINE_SURFACE_WITH_KNOTS ( 'NONE', 3, 3, ( 
 ( #26925, #17798, #31053, #26626 ),
 ( #44661, #35784, #53813, #13647 ),
 ( #36088, #31642, #406, #9231 ),
 ( #17203, #13940, #49389, #36376 ),
 ( #18384, #54402, #3914, #48514 ),
 ( #35482, #26055, #35191, #53223 ),
 ( #12770, #8937, #21917, #39925 ),
 ( #17495, #13054, #23093, #23674 ),
 ( #55261, #18966, #28090, #41104 ),
 ( #9815, #54970, #55555, #10397 ),
 ( #33101, #23961, #19541, #19254 ),
 ( #982, #32513, #49979, #36958 ),
 ( #14520, #14809, #5095, #32805 ),
 ( #50851, #5379, #1550, #19840 ),
 ( #28382, #6247, #37539, #46729 ),
 ( #50557, #45550, #42279, #46140 ),
 ( #37249, #696, #10110, #18678 ) ),
 .UNSPECIFIED., .F., .F., .F.,
 ( 4, 1, 1, 1, 1, 1, 1, 1, 1, 1, 1, 1, 1, 1, 4 ),
 ( 4, 4 ),
 ( -0.01011400514348999996, 0.000000000000000000, 0.08333333333333001192, 0.1666666666667000196, 0.2500000000000000000, 0.3333333333333000081, 0.4166666666666999919, 0.5000000000000000000, 0.5833333333333000637, 0.6666666666667000474, 0.7500000000000000000, 0.8333333333333000637, 0.9166666666667000474, 1.000000000000000000, 1.010365328128000062 ),
 ( -0.3559705546945000076, 1.357612395619000045 ),
 .UNSPECIFIED. ) ;
#23419 = CARTESIAN_POINT ( 'NONE',  ( 4.292950718366999929, -76.93271174891199848, -10.41175003194000048 ) ) ;
#23420 = CARTESIAN_POINT ( 'NONE',  ( 1.472546342128999930, -80.42245324701998754, -0.7790162248558000213 ) ) ;
#23421 = CARTESIAN_POINT ( 'NONE',  ( 0.3144971358097000125, -78.16411730064999119, -1.282096067459000066 ) ) ;
#23422 = CARTESIAN_POINT ( 'NONE',  ( 0.000000000000000000, -74.99999999999998579, 0.000000000000000000 ) ) ;
#23423 = CARTESIAN_POINT ( 'NONE',  ( -0.9781074130570392988, -81.68114129133320489, 1.150371876388886383 ) ) ;
#23424 = CARTESIAN_POINT ( 'NONE',  ( -12.56594317984999876, -18.75000000536999778, 1.750000000000000000 ) ) ;
#23425 = FACE_OUTER_BOUND ( 'NONE', #33453, .T. ) ;
#23426 = CARTESIAN_POINT ( 'NONE',  ( 1.163576041378186599, -79.82060005907925415, -0.4561830117966773623 ) ) ;
#23427 = AXIS2_PLACEMENT_3D ( 'NONE', #47880, #12130, #30118 ) ;
#23428 = CARTESIAN_POINT ( 'NONE',  ( 12.50679926046298540, -54.49581646307559879, -1.424414840068722210 ) ) ;
#23429 = EDGE_LOOP ( 'NONE', ( #4871, #17153 ) ) ;
#23430 = CARTESIAN_POINT ( 'NONE',  ( -1.250000000000000000, -81.59999999999999432, 0.000000000000000000 ) ) ;
#23431 = EDGE_CURVE ( 'NONE', #49808, #25686, #55383, .T. ) ;
#23432 = CARTESIAN_POINT ( 'NONE',  ( 4.703593957913000168, -79.79881202183199207, 9.978874598900000947 ) ) ;
#23433 = DIRECTION ( 'NONE',  ( 0.7592504785509028853, -0.04890181650812019248, -0.6489586451866029559 ) ) ;
#23434 = VERTEX_POINT ( 'NONE', #6043 ) ;
#23435 = EDGE_CURVE ( 'NONE', #27512, #7116, #21411, .T. ) ;
#23436 = CARTESIAN_POINT ( 'NONE',  ( 0.2448185669109000095, -81.90940865802599546, 1.496330837606000053 ) ) ;
#23437 = ORIENTED_EDGE ( 'NONE', *, *, #29733, .F. ) ;
#23438 = VERTEX_POINT ( 'NONE', #47102 ) ;
#23439 = CARTESIAN_POINT ( 'NONE',  ( 1.698401934077000019, -17.77985954096000043, 12.66748707612999958 ) ) ;
#23440 = CARTESIAN_POINT ( 'NONE',  ( 0.000000000000000000, -87.20000000000000284, 0.000000000000000000 ) ) ;
#23441 = AXIS2_PLACEMENT_3D ( 'NONE', #32505, #45542, #55253 ) ;
#23442 = CARTESIAN_POINT ( 'NONE',  ( 2.158813089671214769, -79.66354166010867743, 2.682229611206861541 ) ) ;
#23443 = CARTESIAN_POINT ( 'NONE',  ( 3.792898146759813738, -78.25866108564824231, -8.437158711453742299 ) ) ;
#23444 = DIRECTION ( 'NONE',  ( -0.7071067811865473507, 1.433669009702094715E-08, -0.7071067811865473507 ) ) ;
#23445 = ADVANCED_FACE ( 'NONE', ( #19927 ), #33772, .T. ) ;
#23446 = VERTEX_POINT ( 'NONE', #25211 ) ;
#23447 = ORIENTED_EDGE ( 'NONE', *, *, #57827, .T. ) ;
#23448 = CARTESIAN_POINT ( 'NONE',  ( 6.486170634443213956, -79.97433694125503223, 8.676707126471709941 ) ) ;
#23449 = CARTESIAN_POINT ( 'NONE',  ( 0.9995835529977233902, -81.30208333333334281, 0.7681833999686461523 ) ) ;
#23450 = DIRECTION ( 'NONE',  ( -1.000000000000000000, 0.000000000000000000, 0.000000000000000000 ) ) ;
#23451 = CARTESIAN_POINT ( 'NONE',  ( -9.669247687117000112, -77.77660068504400215, -0.8224101967608999919 ) ) ;
#23452 = CARTESIAN_POINT ( 'NONE',  ( 10.21026636382018715, -61.05606635917384040, 7.764233071724031099 ) ) ;
#23453 = CARTESIAN_POINT ( 'NONE',  ( 2.936513971769209252, -85.86020212823702025, 2.544426056595365804 ) ) ;
#23454 = CARTESIAN_POINT ( 'NONE',  ( 5.488019371950999314, -76.75873275214000557, 11.73632836356999931 ) ) ;
#23455 = CARTESIAN_POINT ( 'NONE',  ( -0.8692139286044998636, -81.28111201704999189, -1.194008811194000153 ) ) ;
#23456 = FACE_OUTER_BOUND ( 'NONE', #41441, .T. ) ;
#23457 = CARTESIAN_POINT ( 'NONE',  ( -7.142344700882925501, -76.62645210080975744, 9.337520193347636166 ) ) ;
#23458 = CARTESIAN_POINT ( 'NONE',  ( -4.072058394011000004, -81.73994274751999001, -0.9101721179166000208 ) ) ;
#23459 = CARTESIAN_POINT ( 'NONE',  ( -2.612980907336999614, -80.37247828420728979, -10.95817168551000087 ) ) ;
#23460 = CARTESIAN_POINT ( 'NONE',  ( -6.043427764450832740, -76.71666666666666856, 10.48543666025107512 ) ) ;
#23461 = CARTESIAN_POINT ( 'NONE',  ( -12.00000000000000000, -79.39999999999999147, 0.000000000000000000 ) ) ;
#23462 = ADVANCED_FACE ( 'NONE', ( #6338 ), #28014, .F. ) ;
#23463 = CARTESIAN_POINT ( 'NONE',  ( 0.7882581348285999656, -81.28405496681197917, 3.458353866083999861 ) ) ;
#23465 = CARTESIAN_POINT ( 'NONE',  ( 0.9834589317531000630, -78.98712297734201115, 0.9007689179829999615 ) ) ;
#23464 = LINE ( 'NONE', #22596, #52356 ) ;
#23466 = VECTOR ( 'NONE', #55554, 1000.000000000000000 ) ;
#23467 = CARTESIAN_POINT ( 'NONE',  ( 0.000000000000000000, -79.79999999999999716, 0.000000000000000000 ) ) ;
#23468 = CARTESIAN_POINT ( 'NONE',  ( -1.249999999999999778, -79.01041666666665719, -0.1636246173744686228 ) ) ;
#23469 = ORIENTED_EDGE ( 'NONE', *, *, #26299, .F. ) ;
#23470 = CARTESIAN_POINT ( 'NONE',  ( 1.081559480311999888, -3.500000000000000000, -3.328697807033000000 ) ) ;
#23471 = B_SPLINE_CURVE_WITH_KNOTS ( 'NONE', 3,
 ( #48266, #7801, #26085, #25801, #7223, #43828, #38514, #47975, #57672, #12229 ),
 .UNSPECIFIED., .F., .F.,
 ( 4, 2, 2, 2, 4 ),
 ( 0.000000000000000000, 0.2500000000000000000, 0.5000000000000000000, 0.7500000000000000000, 1.000000000000000000 ),
 .UNSPECIFIED. ) ;
#23472 = CARTESIAN_POINT ( 'NONE',  ( 0.1577469407304877558, -18.24957415542310457, -11.00002392222777381 ) ) ;
#23473 = CARTESIAN_POINT ( 'NONE',  ( 9.611650271896847286, -78.99166666666666003, 5.539808784079873760 ) ) ;
#23474 = CARTESIAN_POINT ( 'NONE',  ( -7.567403614301999148, -79.38349373972098988, -6.150145586324001101 ) ) ;
#23475 = CARTESIAN_POINT ( 'NONE',  ( 12.50000000000000000, -17.31640971966000109, -1.003652782652999953 ) ) ;
#23476 = CARTESIAN_POINT ( 'NONE',  ( 5.932307977941824184, -79.42851911752600813, 8.979481857698141667 ) ) ;
#23477 = EDGE_CURVE ( 'NONE', #21690, #13072, #29630, .T. ) ;
#23478 = LINE ( 'NONE', #28480, #1837 ) ;
#23479 = DIRECTION ( 'NONE',  ( 0.000000000000000000, -1.000000000000000000, 0.000000000000000000 ) ) ;
#23480 = CYLINDRICAL_SURFACE ( 'NONE', #22142, 10.75000000000000000 ) ;
#23481 = CARTESIAN_POINT ( 'NONE',  ( -4.869124390976999450, -77.26864856148100102, -10.16845940041999974 ) ) ;
#23482 = CARTESIAN_POINT ( 'NONE',  ( -4.505485344499866152, -76.29322575161846487, -10.85157014020616906 ) ) ;
#23483 = CARTESIAN_POINT ( 'NONE',  ( -1.444291512224999963, -80.93220373766600062, -0.4522057381387999953 ) ) ;
#23484 = CARTESIAN_POINT ( 'NONE',  ( 0.000000000000000000, -80.69999999999998863, 0.000000000000000000 ) ) ;
#23485 = CARTESIAN_POINT ( 'NONE',  ( -9.004250860540000900, -77.54436066386098503, -2.744961831234999927 ) ) ;
#23487 = CARTESIAN_POINT ( 'NONE',  ( -2.839805762151343949, -2.958333333333331705, 1.636761686205412181 ) ) ;
#23486 = CARTESIAN_POINT ( 'NONE',  ( -0.7782851299293001013, -84.18193230181299214, 4.056203363392000050 ) ) ;
#23488 = CARTESIAN_POINT ( 'NONE',  ( 1.861092857305999937, -79.77065194988500707, -9.371850619045000386 ) ) ;
#23489 = CARTESIAN_POINT ( 'NONE',  ( -1.250000000000000000, -82.49999999999998579, 0.000000000000000000 ) ) ;
#23490 = CARTESIAN_POINT ( 'NONE',  ( -1.312870888196999930, -79.65019517812399386, 0.1301370089704000088 ) ) ;
#23491 = CARTESIAN_POINT ( 'NONE',  ( -7.597510670570571278, -77.16254964678856254, -7.605260874623661849 ) ) ;
#23492 = CARTESIAN_POINT ( 'NONE',  ( -3.599999993293999889, -0.2000000067061999953, -5.600095662875000459E-09 ) ) ;
#23493 = CARTESIAN_POINT ( 'NONE',  ( 3.999999999999815259, -78.72610001270986402, -4.898587196589186031E-16 ) ) ;
#23494 = ORIENTED_EDGE ( 'NONE', *, *, #23943, .T. ) ;
#23495 = CARTESIAN_POINT ( 'NONE',  ( -8.734850699938000673, -79.57356426399098837, 8.271005326623001253 ) ) ;
#23496 = EDGE_CURVE ( 'NONE', #51603, #7386, #57225, .T. ) ;
#23497 = CARTESIAN_POINT ( 'NONE',  ( -1.250000000000000000, -81.99999999999998579, 0.000000000000000000 ) ) ;
#23498 = B_SPLINE_CURVE_WITH_KNOTS ( 'NONE', 3,
 ( #49544, #8791, #54555, #40379, #9090, #45116 ),
 .UNSPECIFIED., .F., .F.,
 ( 4, 2, 4 ),
 ( 0.000000000000000000, 0.5000000000000000000, 1.000000000000000000 ),
 .UNSPECIFIED. ) ;
#23499 = DIRECTION ( 'NONE',  ( 0.000000000000000000, -1.000000000000000000, 0.000000000000000000 ) ) ;
#23500 = VERTEX_POINT ( 'NONE', #1639 ) ;
#23501 = EDGE_CURVE ( 'NONE', #5875, #41593, #14033, .T. ) ;
#23502 = LINE ( 'NONE', #29092, #9876 ) ;
#23503 = ORIENTED_EDGE ( 'NONE', *, *, #55384, .F. ) ;
#23504 = VERTEX_POINT ( 'NONE', #6920 ) ;
#23505 = DIRECTION ( 'NONE',  ( 0.000000000000000000, 0.000000000000000000, -1.000000000000000000 ) ) ;
#23506 = AXIS2_PLACEMENT_3D ( 'NONE', #35257, #35856, #17564 ) ;
#23507 = ORIENTED_EDGE ( 'NONE', *, *, #17332, .T. ) ;
#23508 = DIRECTION ( 'NONE',  ( -1.893719484533980254E-11, -1.538483569415980182E-07, -0.9999999999999882316 ) ) ;
#23509 = CARTESIAN_POINT ( 'NONE',  ( 7.342331066867000544, -55.64999999967000122, -8.190859204290999784 ) ) ;
#23510 = VERTEX_POINT ( 'NONE', #29060 ) ;
#23512 = EDGE_CURVE ( 'NONE', #28878, #7381, #33185, .T. ) ;
#23511 = CARTESIAN_POINT ( 'NONE',  ( -8.060167321872524937, -54.17936585329436383, -9.621722524781038288 ) ) ;
#23513 = ORIENTED_EDGE ( 'NONE', *, *, #50912, .T. ) ;
#23514 = CARTESIAN_POINT ( 'NONE',  ( 2.813789756862274505, -80.64583333333331439, -10.47020627418438821 ) ) ;
#23515 = CARTESIAN_POINT ( 'NONE',  ( -9.479095156995775540, -77.35887667588667682, -1.070679073321031183 ) ) ;
#23516 = AXIS2_PLACEMENT_3D ( 'NONE', #13084, #49718, #21944 ) ;
#23517 = CARTESIAN_POINT ( 'NONE',  ( 3.992904449609001372, -78.77851881763731967, -1.477225460011499791E-15 ) ) ;
#23518 = DIRECTION ( 'NONE',  ( 0.7071067811865475727, 0.000000000000000000, -0.7071067811865475727 ) ) ;
#23519 = DIRECTION ( 'NONE',  ( 0.000000000000000000, 1.000000000000000000, 0.000000000000000000 ) ) ;
#23520 = CARTESIAN_POINT ( 'NONE',  ( -1.660522255173999984, -76.65296505783298642, 11.05968181062000077 ) ) ;
#23521 = CARTESIAN_POINT ( 'NONE',  ( 0.000000000000000000, 4.040000000000000036, 0.000000000000000000 ) ) ;
#23522 = CARTESIAN_POINT ( 'NONE',  ( -1.438191329984999989, -76.20862989806899179, 11.13621724565999926 ) ) ;
#23523 = CARTESIAN_POINT ( 'NONE',  ( 7.802584695901705558, -78.80492006119759196, -4.968624645346182866 ) ) ;
#23524 = CARTESIAN_POINT ( 'NONE',  ( 2.297810458696917024, -76.55893299319272671, 11.52286801981460229 ) ) ;
#23525 = CARTESIAN_POINT ( 'NONE',  ( -7.278018565911000159, -77.62531001420200027, -5.967178069611000168 ) ) ;
#23526 = CARTESIAN_POINT ( 'NONE',  ( 1.199918086393000127, -80.42027859426200109, 0.5820416783086000967 ) ) ;
#23527 = CARTESIAN_POINT ( 'NONE',  ( -7.600204320007741821, -80.16470501430156048, -7.951820076216480793 ) ) ;
#23528 = CARTESIAN_POINT ( 'NONE',  ( -8.815468636818138748, -78.01289059936662795, -8.261290690983104312 ) ) ;
#23529 = CARTESIAN_POINT ( 'NONE',  ( 2.747530502382999895, -80.96292549782599224, 3.083760634012000068 ) ) ;
#23530 = CARTESIAN_POINT ( 'NONE',  ( -12.70956139859000089, -18.59498835749000278, 1.933780970936999966 ) ) ;
#23531 = CARTESIAN_POINT ( 'NONE',  ( -1.108406828139037570, -83.06136306326980900, 0.5900032945368707260 ) ) ;
#23532 = CARTESIAN_POINT ( 'NONE',  ( 12.99510751537000353, -63.10294702886003648, 6.911973076623003642 ) ) ;
#23533 = CARTESIAN_POINT ( 'NONE',  ( -0.3180038526339120097, -81.85587783296324460, -1.286455647724569884 ) ) ;
#23534 = CARTESIAN_POINT ( 'NONE',  ( -0.1554435011324208915, -82.01041666286585041, -1.489583319316136745 ) ) ;
#23535 = CARTESIAN_POINT ( 'NONE',  ( -10.01676216528999852, -60.00941514989000325, -7.658899892539000831 ) ) ;
#23536 = DIRECTION ( 'NONE',  ( -1.000000000000000000, 0.000000000000000000, 0.000000000000000000 ) ) ;
#23537 = CARTESIAN_POINT ( 'NONE',  ( -1.388062938059625884, -79.81688670877672109, 0.5997038735736672788 ) ) ;
#23538 = CARTESIAN_POINT ( 'NONE',  ( -7.601397897754999633, -23.24999999758999536, 10.07627163191000008 ) ) ;
#23539 = FACE_OUTER_BOUND ( 'NONE', #19604, .T. ) ;
#23540 = CARTESIAN_POINT ( 'NONE',  ( 12.43652404745000162, -24.92065244538000002, 0.1284256373645999982 ) ) ;
#23541 = ADVANCED_FACE ( 'NONE', ( #51522 ), #44113, .F. ) ;
#23542 = CARTESIAN_POINT ( 'NONE',  ( -10.68003080091532375, -77.44002302599371035, 1.404162012696734463 ) ) ;
#23543 = CARTESIAN_POINT ( 'NONE',  ( 0.000000000000000000, -23.15000000000000213, -11.89999999977000122 ) ) ;
#23545 = DIRECTION ( 'NONE',  ( 8.742340186909000165E-11, -1.000000000000000000, 2.562965779940999802E-09 ) ) ;
#23544 = CARTESIAN_POINT ( 'NONE',  ( -1.500000000000000000, -80.00000000000000000, 0.000000000000000000 ) ) ;
#23546 = CARTESIAN_POINT ( 'NONE',  ( 11.45652112554999924, -75.89040228657998455, -4.228683781523999485 ) ) ;
#23547 = ORIENTED_EDGE ( 'NONE', *, *, #54345, .F. ) ;
#23548 = EDGE_CURVE ( 'NONE', #15743, #14217, #19690, .T. ) ;
#23549 = CARTESIAN_POINT ( 'NONE',  ( 3.755994528103999919, -82.75096544543198718, -0.05909446711668000368 ) ) ;
#23550 = CARTESIAN_POINT ( 'NONE',  ( 6.830552694284000026, -80.88557638310635411, -8.988084353687998629 ) ) ;
#23551 = CARTESIAN_POINT ( 'NONE',  ( 8.326085669973442904, -78.31415593885135706, -4.029697569531446533 ) ) ;
#23552 = CARTESIAN_POINT ( 'NONE',  ( 10.20679554288637014, -54.56427274253432813, 7.770327721630681417 ) ) ;
#23553 = CARTESIAN_POINT ( 'NONE',  ( 1.508420534579999917, -77.76594890025400275, 11.11497989572000122 ) ) ;
#23554 = CARTESIAN_POINT ( 'NONE',  ( -1.750000000000000000, -18.75000000240999753, 12.50000000000000000 ) ) ;
#23555 = CARTESIAN_POINT ( 'NONE',  ( -9.628933692773001596, -78.89464829700199289, -0.1919528651714999812 ) ) ;
#23556 = VECTOR ( 'NONE', #9855, 1000.000000000000000 ) ;
#23557 = CYLINDRICAL_SURFACE ( 'NONE', #5346, 11.00000000000000000 ) ;
#23558 = CARTESIAN_POINT ( 'NONE',  ( 4.810664641798661378, -79.80000000000001137, -10.79160144070993610 ) ) ;
#23559 = CARTESIAN_POINT ( 'NONE',  ( 2.295494558656228534, -76.08645833332937514, 10.78189851169432956 ) ) ;
#23560 = ORIENTED_EDGE ( 'NONE', *, *, #22079, .F. ) ;
#23561 = CYLINDRICAL_SURFACE ( 'NONE', #54165, 1.750000000000000000 ) ;
#23562 = CARTESIAN_POINT ( 'NONE',  ( 8.909545442949999838, -59.94999999967000548, 8.061017305527000687 ) ) ;
#23563 = AXIS2_PLACEMENT_3D ( 'NONE', #39039, #3322, #57050 ) ;
#23564 = CARTESIAN_POINT ( 'NONE',  ( -6.709544961267000396, -79.63031332859900147, 6.760325364400999959 ) ) ;
#23565 = CARTESIAN_POINT ( 'NONE',  ( 3.643968819545335691, -75.84956472831228780, -11.20974552281418823 ) ) ;
#23566 = ORIENTED_EDGE ( 'NONE', *, *, #36821, .T. ) ;
#23567 = CARTESIAN_POINT ( 'NONE',  ( -12.50728617048089575, -17.00024476471455870, -0.1757989196447104219 ) ) ;
#23568 = DIRECTION ( 'NONE',  ( 0.000000000000000000, 0.000000000000000000, -1.000000000000000000 ) ) ;
#23569 = VERTEX_POINT ( 'NONE', #19708 ) ;
#23570 = EDGE_CURVE ( 'NONE', #51903, #33522, #35557, .T. ) ;
#23571 = CARTESIAN_POINT ( 'NONE',  ( 11.74988006023992071, -76.93969616181793469, -1.039067677832774095 ) ) ;
#23572 = CARTESIAN_POINT ( 'NONE',  ( -6.091193159344999941, -77.07048692427588321, -8.944723388890000848 ) ) ;
#23573 = DIRECTION ( 'NONE',  ( 0.000000000000000000, -1.000000000000000000, 0.000000000000000000 ) ) ;
#23574 = ORIENTED_EDGE ( 'NONE', *, *, #38239, .T. ) ;
#23575 = CARTESIAN_POINT ( 'NONE',  ( -1.239753235927716357, -80.59053486374234865, 0.1581211216746350179 ) ) ;
#23576 = CARTESIAN_POINT ( 'NONE',  ( 5.411006671257999834, -79.21873047333799889, 8.131518144102999557 ) ) ;
#23577 = ORIENTED_EDGE ( 'NONE', *, *, #16251, .F. ) ;
#23579 = EDGE_CURVE ( 'NONE', #2832, #45010, #54202, .T. ) ;
#23578 = CARTESIAN_POINT ( 'NONE',  ( 12.49989298246999958, -55.60773379962999741, 1.666426105558999948 ) ) ;
#23580 = FACE_OUTER_BOUND ( 'NONE', #382, .T. ) ;
#23581 = CARTESIAN_POINT ( 'NONE',  ( -12.70956478397999945, -23.40497526616000101, -1.933781249744999986 ) ) ;
#23582 = EDGE_CURVE ( 'NONE', #45667, #12448, #55654, .T. ) ;
#23583 = CARTESIAN_POINT ( 'NONE',  ( -9.061228178001998756, -77.65420194988499247, -2.837532765875999896 ) ) ;
#23584 = B_SPLINE_CURVE_WITH_KNOTS ( 'NONE', 3,
 ( #23282, #41287, #49872, #32407, #45737, #5273, #23565, #40706, #36562, #36271, #31829, #871, #10291, #22694, #37430, #18857, #4981, #9704 ),
 .UNSPECIFIED., .F., .F.,
 ( 4, 2, 2, 2, 2, 2, 2, 2, 4 ),
 ( 0.000000000000000000, 0.1250000000000000000, 0.2500000000000000000, 0.3750000000000000000, 0.5000000000000000000, 0.6250000000000000000, 0.7500000000000000000, 0.8750000000000000000, 1.000000000000000000 ),
 .UNSPECIFIED. ) ;
#23585 = DIRECTION ( 'NONE',  ( 0.000000000000000000, 0.000000000000000000, -1.000000000000000000 ) ) ;
#23586 = CARTESIAN_POINT ( 'NONE',  ( -0.4122473303297303215, -80.19853687741431258, -1.179911485936611770 ) ) ;
#23587 = CARTESIAN_POINT ( 'NONE',  ( 0.8804656547936360322, -16.97196605292967320, -12.70299681151658255 ) ) ;
#23588 = CARTESIAN_POINT ( 'NONE',  ( -9.500000000000000000, -78.29999999999999716, 0.000000000000000000 ) ) ;
#23589 = CARTESIAN_POINT ( 'NONE',  ( -1.867777256262999952, -77.16087362948169925, 9.751254915078000352 ) ) ;
#23590 = CARTESIAN_POINT ( 'NONE',  ( -0.2871694602881026959, -79.23982420962433082, 1.481336007913308883 ) ) ;
#23591 = CARTESIAN_POINT ( 'NONE',  ( 3.219568491329446669, -79.29739581894648381, -2.394182203109038731 ) ) ;
#23592 = ORIENTED_EDGE ( 'NONE', *, *, #6297, .T. ) ;
#23593 = CARTESIAN_POINT ( 'NONE',  ( -1.476182556144000069, -76.40189909139999713, 12.22114576030999977 ) ) ;
#23594 = CARTESIAN_POINT ( 'NONE',  ( -10.47020627418439354, -77.52083333333331439, -2.813789756862263847 ) ) ;
#23595 = CARTESIAN_POINT ( 'NONE',  ( -2.921934676155967914, -1.896386797793808254, -1.963134887269489814 ) ) ;
#23596 = VECTOR ( 'NONE', #56324, 1000.000000000000114 ) ;
#23597 = ADVANCED_FACE ( 'NONE', ( #38799 ), #34357, .F. ) ;
#23598 = CARTESIAN_POINT ( 'NONE',  ( 7.624757096145000190, -60.60351363786999457, -10.47516529250999895 ) ) ;
#23599 = CARTESIAN_POINT ( 'NONE',  ( 6.688645397968000950, -78.84642772177998893, 10.27915892414000076 ) ) ;
#23600 = CARTESIAN_POINT ( 'NONE',  ( 1.298131932841000147, -76.43267843637200087, 12.21218573294999921 ) ) ;
#23601 = LINE ( 'NONE', #27440, #8173 ) ;
#23602 = CARTESIAN_POINT ( 'NONE',  ( 5.471330588277999674, -78.45546044413198672, 9.848526282906998830 ) ) ;
#23603 = CARTESIAN_POINT ( 'NONE',  ( 2.307541886207349346, -2.788560972538888905, -2.288008278024395548 ) ) ;
#23604 = CARTESIAN_POINT ( 'NONE',  ( 9.418236657459665651, -77.35379839889799314, 7.544531841333499855 ) ) ;
#23605 = CARTESIAN_POINT ( 'NONE',  ( -9.837774000978795286, -17.68535604387229299, 7.850041800338160236 ) ) ;
#23606 = ORIENTED_EDGE ( 'NONE', *, *, #27484, .T. ) ;
#23607 = CARTESIAN_POINT ( 'NONE',  ( -1.486838331013629722, -81.23578785145382142, 0.2672933875640012280 ) ) ;
#23608 = CARTESIAN_POINT ( 'NONE',  ( -8.262032057783999406, -77.35055961578798644, 4.886512119495000306 ) ) ;
#23609 = DIRECTION ( 'NONE',  ( 0.000000000000000000, -1.000000000000000000, 0.000000000000000000 ) ) ;
#23610 = CARTESIAN_POINT ( 'NONE',  ( -4.000000000000000000, -74.80000000000001137, 0.5999999999999999778 ) ) ;
#23611 = CARTESIAN_POINT ( 'NONE',  ( -0.2932567490044000191, -2.500169754918000198, -3.702492619799000462 ) ) ;
#23612 = ADVANCED_FACE ( 'NONE', ( #52394 ), #6329, .T. ) ;
#23613 = CARTESIAN_POINT ( 'NONE',  ( 11.27339212957999948, -77.78758450816098957, 4.255161755617000274 ) ) ;
#23614 = CARTESIAN_POINT ( 'NONE',  ( 2.845884614340000063, -77.85580916391599260, -9.200769029100998253 ) ) ;
#23615 = CARTESIAN_POINT ( 'NONE',  ( 8.510637803266750012, -76.00995353112250541, 8.100988122022512172 ) ) ;
#23616 = FACE_OUTER_BOUND ( 'NONE', #5997, .T. ) ;
#23617 = CARTESIAN_POINT ( 'NONE',  ( 3.194290819685191796, -86.10000000000017906, 2.320109443757543133 ) ) ;
#23618 = ORIENTED_EDGE ( 'NONE', *, *, #5363, .T. ) ;
#23619 = ADVANCED_FACE ( 'NONE', ( #52105 ), #37637, .F. ) ;
#23620 =( GEOMETRIC_REPRESENTATION_CONTEXT ( 3 ) GLOBAL_UNCERTAINTY_ASSIGNED_CONTEXT ( ( #46722 ) ) GLOBAL_UNIT_ASSIGNED_CONTEXT ( ( #31315, #22481, #36056 ) ) REPRESENTATION_CONTEXT ( 'NONE', 'WORKASPACE' ) );
#23621 = DIRECTION ( 'NONE',  ( 0.000000000000000000, -1.000000000000000000, 0.000000000000000000 ) ) ;
#23622 = DIRECTION ( 'NONE',  ( -0.7071067811865475727, 0.000000000000000000, -0.7071067811865475727 ) ) ;
#23623 = VECTOR ( 'NONE', #38741, 1000.000000000000000 ) ;
#23624 = CARTESIAN_POINT ( 'NONE',  ( 1.025029370886000101E-14, -0.2000000000000005107, 0.000000000000000000 ) ) ;
#23625 = CARTESIAN_POINT ( 'NONE',  ( -10.81649518602000093, -79.47688774910298548, 1.862108609190000097 ) ) ;
#23626 = CARTESIAN_POINT ( 'NONE',  ( 6.760013919724043419, -79.27708333333333712, -8.796335266379996298 ) ) ;
#23627 = CARTESIAN_POINT ( 'NONE',  ( -12.00000000000000888, -77.88958333333334849, 1.570796326794847264 ) ) ;
#23628 = CARTESIAN_POINT ( 'NONE',  ( 0.9521775314477300967, -79.29341203308139541, -0.8298931526774534495 ) ) ;
#23629 = CARTESIAN_POINT ( 'NONE',  ( 7.620012214426000519, -18.79439747922000237, -10.53562508625000049 ) ) ;
#23630 = LINE ( 'NONE', #41642, #17359 ) ;
#23631 = VERTEX_POINT ( 'NONE', #37927 ) ;
#23632 = CARTESIAN_POINT ( 'NONE',  ( 3.521285801175999985, -79.12628491221198601, 10.69740673549999954 ) ) ;
#23633 = DIRECTION ( 'NONE',  ( -1.411446131769000029E-10, -6.386278974555000074E-09, 1.000000000000000000 ) ) ;
#23634 = CARTESIAN_POINT ( 'NONE',  ( 0.07899549168242259167, -79.67539556713441584, -11.83310309920475767 ) ) ;
#23635 = CARTESIAN_POINT ( 'NONE',  ( 3.699999999670000150, -78.39678895079168797, -4.531193156441073745E-16 ) ) ;
#23636 = CARTESIAN_POINT ( 'NONE',  ( 4.230813626878798139, -77.79940820322376283, 11.25355361728754922 ) ) ;
#23637 = LINE ( 'NONE', #41363, #43079 ) ;
#23638 = VECTOR ( 'NONE', #18340, 1000.000000000000000 ) ;
#23639 = CARTESIAN_POINT ( 'NONE',  ( 12.50485692592770626, -61.66593462659085390, -0.6924071803391340652 ) ) ;
#23640 = FACE_OUTER_BOUND ( 'NONE', #4489, .T. ) ;
#23641 = CIRCLE ( 'NONE', #56646, 0.5000000000000004441 ) ;
#23642 = CARTESIAN_POINT ( 'NONE',  ( 0.3375844306956000129, -79.28888630715999852, -1.278415048790000119 ) ) ;
#23643 = CARTESIAN_POINT ( 'NONE',  ( 10.75000000000000000, -79.25000000000000000, 0.000000000000000000 ) ) ;
#23644 = CARTESIAN_POINT ( 'NONE',  ( -2.169201898071945855, -78.34093333352706168, 10.75929280804342447 ) ) ;
#23645 = DIRECTION ( 'NONE',  ( -1.000000000000000000, 0.000000000000000000, 0.000000000000000000 ) ) ;
#23646 = ORIENTED_EDGE ( 'NONE', *, *, #26394, .F. ) ;
#23647 = ORIENTED_EDGE ( 'NONE', *, *, #45300, .T. ) ;
#23648 = CARTESIAN_POINT ( 'NONE',  ( 8.642645349805999189, -78.58708998579800209, -5.074666031188000304 ) ) ;
#23649 = CARTESIAN_POINT ( 'NONE',  ( 6.826798571050595399, -78.77984587750025014, -8.303980297556394774 ) ) ;
#23650 = EDGE_CURVE ( 'NONE', #34714, #44555, #55951, .T. ) ;
#23651 = ORIENTED_EDGE ( 'NONE', *, *, #26588, .F. ) ;
#23652 = CARTESIAN_POINT ( 'NONE',  ( -7.695020077041000661, -76.18538407120952627, 8.115451295621999961 ) ) ;
#23653 = CARTESIAN_POINT ( 'NONE',  ( -1.349723918382976784, -83.47916668054376998, -3.167509171181071448 ) ) ;
#23654 = CARTESIAN_POINT ( 'NONE',  ( -9.222359558045559069, -79.38018218778096013, 2.295680754222614084 ) ) ;
#23655 = CARTESIAN_POINT ( 'NONE',  ( 7.981656248376999940, -61.51865039470999363, 10.08154475893999980 ) ) ;
#23656 = DIRECTION ( 'NONE',  ( 0.000000000000000000, 1.000000000000000000, 0.000000000000000000 ) ) ;
#23657 = CARTESIAN_POINT ( 'NONE',  ( 11.79859628133356786, -77.28603821643537231, -2.076809670760434656 ) ) ;
#23658 = CARTESIAN_POINT ( 'NONE',  ( 8.733858618705999888, -78.46212780691099908, -7.038306768505999678 ) ) ;
#23659 = ORIENTED_EDGE ( 'NONE', *, *, #36924, .T. ) ;
#23660 = CARTESIAN_POINT ( 'NONE',  ( -10.10447584118665887, -24.45118490549160484, 7.864774383118550816 ) ) ;
#23661 = AXIS2_PLACEMENT_3D ( 'NONE', #10814, #38238, #37069 ) ;
#23662 = VERTEX_POINT ( 'NONE', #11089 ) ;
#23663 = CARTESIAN_POINT ( 'NONE',  ( 8.795818401383446172, -77.37508321831271019, 2.862770402330162334 ) ) ;
#23664 = CARTESIAN_POINT ( 'NONE',  ( -9.050627908549000011, -77.53897626982698910, -6.322205650057999726 ) ) ;
#23665 = CARTESIAN_POINT ( 'NONE',  ( 0.5999999999999999778, -5.000000000000000000, 4.000000000000000000 ) ) ;
#23666 = CARTESIAN_POINT ( 'NONE',  ( -1.466115278491000096, -77.95753785706131112, 0.6765500100044000709 ) ) ;
#23667 = CARTESIAN_POINT ( 'NONE',  ( -10.48543666025109289, -77.44166666666666288, -6.043427764450796325 ) ) ;
#23668 = EDGE_CURVE ( 'NONE', #55921, #30078, #4475, .T. ) ;
#23669 = FACE_OUTER_BOUND ( 'NONE', #44901, .T. ) ;
#23670 = CARTESIAN_POINT ( 'NONE',  ( 0.1198033158700999995, -79.13952864070999738, 1.623056241665000066 ) ) ;
#23671 = DIRECTION ( 'NONE',  ( 0.000000000000000000, 0.7071067811866525998, -0.7071067811864425456 ) ) ;
#23672 = CARTESIAN_POINT ( 'NONE',  ( 6.591600424694998850, -79.75272800141398477, 8.731473042948000085 ) ) ;
#23673 = EDGE_CURVE ( 'NONE', #47577, #43330, #26083, .T. ) ;
#23674 = CARTESIAN_POINT ( 'NONE',  ( -9.101516360816999551, -24.88066799059000189, -8.485522730740999720 ) ) ;
#23675 = CARTESIAN_POINT ( 'NONE',  ( 12.53239398060000021, -56.03513569577999931, -1.667936688463999895 ) ) ;
#23676 = CARTESIAN_POINT ( 'NONE',  ( 1.109092207577000000, -84.06168188654598339, 3.413745671519000435 ) ) ;
#23677 = ORIENTED_EDGE ( 'NONE', *, *, #38488, .F. ) ;
#23678 = CARTESIAN_POINT ( 'NONE',  ( -9.831591192207000063, -78.92583355886799268, -7.611166649991000455 ) ) ;
#23679 = VECTOR ( 'NONE', #47578, 1000.000000000000114 ) ;
#23680 = CARTESIAN_POINT ( 'NONE',  ( -0.6709475781581999421, -80.98357467910000196, -1.436741477991000160 ) ) ;
#23681 = CARTESIAN_POINT ( 'NONE',  ( -0.5817747831294644012, -77.97935686554528445, 10.73539099268632846 ) ) ;
#23682 = CARTESIAN_POINT ( 'NONE',  ( -11.61454496413000115, -77.61419278293099921, 2.935712811417999557 ) ) ;
#23683 = DIRECTION ( 'NONE',  ( 0.000000000000000000, 1.000000000000000000, 0.000000000000000000 ) ) ;
#23684 = AXIS2_PLACEMENT_3D ( 'NONE', #24882, #21312, #2457 ) ;
#23685 = CARTESIAN_POINT ( 'NONE',  ( 8.190859204290999784, -59.94999999967000548, -7.342331066867000544 ) ) ;
#23686 = CARTESIAN_POINT ( 'NONE',  ( 2.077614454027474356, -3.074804716019511108, 2.843664572838004112 ) ) ;
#23687 = CARTESIAN_POINT ( 'NONE',  ( 10.44832407724852530, -80.86929795574350521, 2.527760674094279736 ) ) ;
#23688 = CARTESIAN_POINT ( 'NONE',  ( -7.831519877845000366, -78.12599129015498534, -5.222881475815000840 ) ) ;
#23689 = CARTESIAN_POINT ( 'NONE',  ( 3.308356911591977756, -85.80681307385599155, -1.472975398279049442 ) ) ;
#23690 = CARTESIAN_POINT ( 'NONE',  ( 9.509459933319000413, -77.25116639950799424, 5.592128946851999238 ) ) ;
#23691 = FACE_OUTER_BOUND ( 'NONE', #54171, .T. ) ;
#23692 = CARTESIAN_POINT ( 'NONE',  ( 7.397492105520000472, -80.20748139727048454, 8.141545085894000167 ) ) ;
#23693 = ORIENTED_EDGE ( 'NONE', *, *, #50416, .F. ) ;
#23694 = EDGE_CURVE ( 'NONE', #32275, #40010, #35511, .T. ) ;
#23695 = FACE_OUTER_BOUND ( 'NONE', #54358, .T. ) ;
#23696 = CARTESIAN_POINT ( 'NONE',  ( -8.190817883596805515, -55.56980390652987722, 7.342377162852848471 ) ) ;
#23697 = CARTESIAN_POINT ( 'NONE',  ( 4.275724345439000373, -76.85443832237800166, -10.36997068233999997 ) ) ;
#23698 = CARTESIAN_POINT ( 'NONE',  ( -9.091539081997000338, -78.76222423976999210, 6.148815634104000338 ) ) ;
#23699 = CARTESIAN_POINT ( 'NONE',  ( 6.486265764543627022, -80.27377157478035485, 8.676841151407936437 ) ) ;
#23700 = CARTESIAN_POINT ( 'NONE',  ( 0.01844432583040244572, -82.82395831769791528, 4.013020696622482397 ) ) ;
#23701 = DIRECTION ( 'NONE',  ( 0.000000000000000000, 0.7071067811865475727, 0.7071067811865475727 ) ) ;
#23702 = CARTESIAN_POINT ( 'NONE',  ( -10.04568514500204834, -54.24913840230841799, -7.921286339674650456 ) ) ;
#23703 = CARTESIAN_POINT ( 'NONE',  ( -2.666402605432000250, -84.47794503318799286, 3.209417306183000029 ) ) ;
#23704 = DIRECTION ( 'NONE',  ( 0.000000000000000000, -1.000000000000000000, 0.000000000000000000 ) ) ;
#23705 = EDGE_CURVE ( 'NONE', #41153, #9574, #16665, .T. ) ;
#23707 = EDGE_CURVE ( 'NONE', #35685, #26753, #25511, .T. ) ;
#23706 = CARTESIAN_POINT ( 'NONE',  ( 10.52682159589000044, -55.37432398227000618, -7.605688676848999741 ) ) ;
#23708 =( GEOMETRIC_REPRESENTATION_CONTEXT ( 3 ) GLOBAL_UNCERTAINTY_ASSIGNED_CONTEXT ( ( #25408 ) ) GLOBAL_UNIT_ASSIGNED_CONTEXT ( ( #48490, #52341, #6880 ) ) REPRESENTATION_CONTEXT ( 'NONE', 'WORKASPACE' ) );
#23709 = CARTESIAN_POINT ( 'NONE',  ( 0.5495723139228999576, -76.90547540590999631, -11.24864145460999865 ) ) ;
#23710 = CARTESIAN_POINT ( 'NONE',  ( -1.630114970985000022, -79.72770188080998821, -0.3434887894992000312 ) ) ;
#23711 = CARTESIAN_POINT ( 'NONE',  ( 1.313811648119000086, -79.27774869623999621, 0.1287517855103000042 ) ) ;
#23712 = CARTESIAN_POINT ( 'NONE',  ( -12.00000000000000178, -79.31041666666665435, -1.570796326794897890 ) ) ;
#23713 = CARTESIAN_POINT ( 'NONE',  ( 0.8719698933019950360, -81.92406134944869223, -1.233151496242500533 ) ) ;
#23714 = FACE_OUTER_BOUND ( 'NONE', #28623, .T. ) ;
#23715 = CARTESIAN_POINT ( 'NONE',  ( 10.36935812844000004, -78.07876026662599145, -2.835297515976000327 ) ) ;
#23716 = CARTESIAN_POINT ( 'NONE',  ( 1.156157754792947578, -79.81928919401691758, -0.4747237588690541021 ) ) ;
#23717 = CARTESIAN_POINT ( 'NONE',  ( -7.921329716846313040, -54.24906234234291702, 10.04564005580055053 ) ) ;
#23718 = VERTEX_POINT ( 'NONE', #17823 ) ;
#23719 = CARTESIAN_POINT ( 'NONE',  ( -1.149810464072230198, -81.63223063354799081, -0.4900990545918544883 ) ) ;
#23720 = CARTESIAN_POINT ( 'NONE',  ( -0.4077927620925000385, -79.58092127781698366, -11.02431129116999919 ) ) ;
#23721 = DIRECTION ( 'NONE',  ( -1.000000000000000000, 0.000000000000000000, 0.000000000000000000 ) ) ;
#23722 = EDGE_LOOP ( 'NONE', ( #42033, #6922, #58062, #12943 ) ) ;
#23723 = ORIENTED_EDGE ( 'NONE', *, *, #54792, .T. ) ;
#23724 = CARTESIAN_POINT ( 'NONE',  ( 0.7804898537227999977, -80.77407738460799180, -1.183584831557000117 ) ) ;
#23725 = AXIS2_PLACEMENT_3D ( 'NONE', #36740, #45332, #9599 ) ;
#23726 = EDGE_CURVE ( 'NONE', #24467, #47685, #26651, .T. ) ;
#23727 = ORIENTED_EDGE ( 'NONE', *, *, #40552, .T. ) ;
#23728 = ORIENTED_EDGE ( 'NONE', *, *, #7349, .T. ) ;
#23729 = VECTOR ( 'NONE', #32627, 1000.000000000000000 ) ;
#23730 = CARTESIAN_POINT ( 'NONE',  ( 0.8537148449481000156, -17.29501854091000013, 12.43377424872999981 ) ) ;
#23731 = CARTESIAN_POINT ( 'NONE',  ( -1.499999999971000086, -77.75000000002998490, -1.761798912373000190E-09 ) ) ;
#23732 = DIRECTION ( 'NONE',  ( 0.000000000000000000, 0.000000000000000000, 1.000000000000000000 ) ) ;
#23733 = CARTESIAN_POINT ( 'NONE',  ( 2.868552210033068928, -81.08958332121085277, 1.904464906000009838 ) ) ;
#23734 = CARTESIAN_POINT ( 'NONE',  ( 3.571212153075712159, -78.25658151030941667, -8.532799217283892901 ) ) ;
#23735 = CARTESIAN_POINT ( 'NONE',  ( 10.75000000000000000, -78.25000000000000000, 1.005550720961999908E-14 ) ) ;
#23736 = VERTEX_POINT ( 'NONE', #17521 ) ;
#23737 = ORIENTED_EDGE ( 'NONE', *, *, #2671, .T. ) ;
#23738 = CARTESIAN_POINT ( 'NONE',  ( -8.069289515393755607, -77.55933884297279235, 4.525049359534452087 ) ) ;
#23739 = CARTESIAN_POINT ( 'NONE',  ( 6.436424241555000592, -79.92391735373439587, 8.610165096135999008 ) ) ;
#23740 = LINE ( 'NONE', #15173, #23305 ) ;
#23741 = CARTESIAN_POINT ( 'NONE',  ( 1.318114156659812908, -61.53572477165494803, -12.70261578166418737 ) ) ;
#23742 = CARTESIAN_POINT ( 'NONE',  ( 8.898653440358000211, -78.48719641326798069, -3.871004561473999850 ) ) ;
#23743 = CYLINDRICAL_SURFACE ( 'NONE', #34111, 12.05000000000000071 ) ;
#23744 = CARTESIAN_POINT ( 'NONE',  ( -10.38645071867999903, -22.77819125662999866, 7.655542440070999710 ) ) ;
#23745 = CARTESIAN_POINT ( 'NONE',  ( 0.3704480450335023156, -77.42746413819746465, -12.03686759590604005 ) ) ;
#23746 = CARTESIAN_POINT ( 'NONE',  ( -0.5042965048037999498, -80.60741372253998804, 1.503356827960000031 ) ) ;
#23747 = CARTESIAN_POINT ( 'NONE',  ( 1.708922835747884506, -77.68932193750340787, -9.291094250111688879 ) ) ;
#23748 = CARTESIAN_POINT ( 'NONE',  ( -9.455880892872714938, -76.64914396672122621, 6.975925114676199357 ) ) ;
#23749 = B_SPLINE_CURVE_WITH_KNOTS ( 'NONE', 3,
 ( #27018, #45054, #44750, #4606, #40615, #19932, #23188, #19634, #32606, #1353, #41780, #5756, #1645, #32897, #23473, #37631, #37922, #5182 ),
 .UNSPECIFIED., .F., .F.,
 ( 4, 2, 2, 2, 2, 2, 2, 2, 4 ),
 ( 0.000000000000000000, 0.1250000000000000000, 0.2500000000000000000, 0.3750000000000000000, 0.5000000000000000000, 0.6250000000000000000, 0.7500000000000000000, 0.8750000000000000000, 1.000000000000000000 ),
 .UNSPECIFIED. ) ;
#23750 = CARTESIAN_POINT ( 'NONE',  ( -2.944205202882999917, -81.49944189855800403, 2.956641395289000052 ) ) ;
#23751 = CARTESIAN_POINT ( 'NONE',  ( -11.03620408507000050, -80.21439667292020204, -2.260839449595000161 ) ) ;
#23752 = CARTESIAN_POINT ( 'NONE',  ( -9.596002108778193929, -76.74791666666664014, 7.374560639698935383 ) ) ;
#23753 = CARTESIAN_POINT ( 'NONE',  ( -2.813846212576811556, -76.70429982244345979, -10.47057735762498609 ) ) ;
#23754 = CARTESIAN_POINT ( 'NONE',  ( -0.9788895612340001717, -81.40430496681199202, 3.409301629348000073 ) ) ;
#23756 = CARTESIAN_POINT ( 'NONE',  ( 0.2725326480772000126, -79.03673560072299153, 1.305490477442999842 ) ) ;
#23755 = DIRECTION ( 'NONE',  ( 0.000000000000000000, -1.000000000000000000, 0.000000000000000000 ) ) ;
#23757 = CARTESIAN_POINT ( 'NONE',  ( -5.685008486195640032, -79.52738042223084847, 7.397161007072386774 ) ) ;
#23758 = LINE ( 'NONE', #19627, #21258 ) ;
#23759 = CARTESIAN_POINT ( 'NONE',  ( -2.561320322697239860, -77.20000000000000284, -10.72273578054103105 ) ) ;
#23760 = ORIENTED_EDGE ( 'NONE', *, *, #41347, .T. ) ;
#23761 = CARTESIAN_POINT ( 'NONE',  ( -11.00000000000000000, -78.21041666666667425, -1.439896632895322881 ) ) ;
#23762 = ADVANCED_FACE ( 'NONE', ( #17226 ), #22284, .F. ) ;
#23763 = CARTESIAN_POINT ( 'NONE',  ( 0.5999999999999999778, -18.84999999999999787, -10.98362417419999915 ) ) ;
#23764 = CARTESIAN_POINT ( 'NONE',  ( -10.19635340580301097, -77.65732487548163476, 5.890683536056261715 ) ) ;
#23765 = CARTESIAN_POINT ( 'NONE',  ( -3.950656329793999610, -79.23738044843098294, 8.915279242129001247 ) ) ;
#23766 = VECTOR ( 'NONE', #2195, 1000.000000000000114 ) ;
#23767 = CARTESIAN_POINT ( 'NONE',  ( -10.55511172854000002, -77.89828514651000546, 7.611100925114999249 ) ) ;
#23768 = CARTESIAN_POINT ( 'NONE',  ( -0.05316490922953205633, -79.47551739595091647, 10.74981279920144672 ) ) ;
#23769 = VECTOR ( 'NONE', #40690, 1000.000000000000000 ) ;
#23770 = CARTESIAN_POINT ( 'NONE',  ( 8.307189301499999345, -79.65391332859900331, -4.458756970628000360 ) ) ;
#23771 = CARTESIAN_POINT ( 'NONE',  ( 12.76303204298000082, -60.06485150663000638, -1.980584515756000030 ) ) ;
#23772 = CARTESIAN_POINT ( 'NONE',  ( -3.929469618655000218, -77.64668109758299863, 10.45105132569000084 ) ) ;
#23773 = EDGE_CURVE ( 'NONE', #43973, #31318, #35883, .T. ) ;
#23774 = CARTESIAN_POINT ( 'NONE',  ( 0.9660827079681000296, -81.73162454270899957, 1.280557929256000094 ) ) ;
#23775 = PLANE ( 'NONE',  #44606 ) ;
#23776 = CARTESIAN_POINT ( 'NONE',  ( -8.866000417715000026, -77.49698761531298885, 2.742227037787000388 ) ) ;
#23778 = CARTESIAN_POINT ( 'NONE',  ( 2.863963203921999767, -1.163821851618000114, 2.815564610575000071 ) ) ;
#23777 = CARTESIAN_POINT ( 'NONE',  ( 3.318041721436999936, -82.26178512955299027, 1.761290859772999928 ) ) ;
#23779 = CARTESIAN_POINT ( 'NONE',  ( 2.769824414688999870, -79.27925194988499413, -8.825563591736999669 ) ) ;
#23780 = CARTESIAN_POINT ( 'NONE',  ( 0.6295237254636258939, -82.66666666666667140, -1.092232985442821658 ) ) ;
#23781 = CARTESIAN_POINT ( 'NONE',  ( 0.5703284788033999853, -79.99748354179199339, 1.189660050829999927 ) ) ;
#23782 = DIRECTION ( 'NONE',  ( 0.000000000000000000, 1.000000000000000000, 0.000000000000000000 ) ) ;
#23783 = LINE ( 'NONE', #41799, #46439 ) ;
#23784 = VECTOR ( 'NONE', #24669, 1000.000000000000000 ) ;
#23785 = CARTESIAN_POINT ( 'NONE',  ( -3.999999999999674927, -78.69999999999997442, -1.678385095468326031E-14 ) ) ;
#23786 = ORIENTED_EDGE ( 'NONE', *, *, #31817, .T. ) ;
#23787 = CARTESIAN_POINT ( 'NONE',  ( -11.15966350340000091, -79.60344789483799843, 4.490997254915999548 ) ) ;
#23788 = CARTESIAN_POINT ( 'NONE',  ( 0.000000000000000000, -75.09999999996229292, -11.54999999996000071 ) ) ;
#23789 = DIRECTION ( 'NONE',  ( 0.000000000000000000, 1.000000000000000000, 0.000000000000000000 ) ) ;
#23790 = VERTEX_POINT ( 'NONE', #21369 ) ;
#23791 = DIRECTION ( 'NONE',  ( 0.000000000000000000, 0.000000000000000000, -1.000000000000000000 ) ) ;
#23792 = ADVANCED_FACE ( 'NONE', ( #8368 ), #19473, .F. ) ;
#23793 = ORIENTED_EDGE ( 'NONE', *, *, #23929, .F. ) ;
#23794 = EDGE_LOOP ( 'NONE', ( #41775, #45173, #31109, #24314, #8643, #55094, #2699 ) ) ;
#23795 = ORIENTED_EDGE ( 'NONE', *, *, #887, .T. ) ;
#23796 = CARTESIAN_POINT ( 'NONE',  ( -3.543450156475999702, -80.17668722926399028, 0.1597837688739999762 ) ) ;
#23797 = CARTESIAN_POINT ( 'NONE',  ( 10.42531125072000009, -55.53514854654000032, 7.624341767124000135 ) ) ;
#23798 = EDGE_LOOP ( 'NONE', ( #3579, #22919, #7720, #29516, #1282, #44194, #6564, #14926 ) ) ;
#23799 = CARTESIAN_POINT ( 'NONE',  ( 1.216162773206594938, -82.83133620506080774, -0.2928064032228187008 ) ) ;
#23800 = CARTESIAN_POINT ( 'NONE',  ( 3.397703318627999458, -2.301921241517000283, -0.1580915791678000060 ) ) ;
#23801 = ORIENTED_EDGE ( 'NONE', *, *, #26512, .F. ) ;
#23802 = CARTESIAN_POINT ( 'NONE',  ( -9.250000000000000000, -79.09999999999999432, 1.813240672189999963E-14 ) ) ;
#23803 = CARTESIAN_POINT ( 'NONE',  ( 11.00000000000000000, -78.84999999999999432, 0.000000000000000000 ) ) ;
#23804 = AXIS2_PLACEMENT_3D ( 'NONE', #33614, #33896, #46941 ) ;
#23805 = CARTESIAN_POINT ( 'NONE',  ( -6.943703696083231236, -79.79999999999999716, -9.645494662058867519 ) ) ;
#23806 = LINE ( 'NONE', #19677, #19909 ) ;
#23807 = CARTESIAN_POINT ( 'NONE',  ( 2.714678808024538537, -0.9374999996105841671, 1.968551052210687491 ) ) ;
#23808 = CARTESIAN_POINT ( 'NONE',  ( 9.703485699160999900, -77.50093816103475319, 0.1143444355825999903 ) ) ;
#23809 = CARTESIAN_POINT ( 'NONE',  ( 8.154961773732001262, -76.07608039208299999, 7.653135223926000208 ) ) ;
#23810 = CARTESIAN_POINT ( 'NONE',  ( -8.583677312632392642, -24.97185920791575597, 9.102132574107123730 ) ) ;
#23811 = VECTOR ( 'NONE', #27393, 999.9999999999998863 ) ;
#23812 = CARTESIAN_POINT ( 'NONE',  ( 7.653559626114000203, -60.09848884406000025, -10.01235002625000092 ) ) ;
#23813 = CARTESIAN_POINT ( 'NONE',  ( 0.4089082674944940488, -78.72870479441709790, -9.241335590917220344 ) ) ;
#23814 = CARTESIAN_POINT ( 'NONE',  ( 5.196759135519999795, -77.39911001420199455, 7.846684831825000650 ) ) ;
#23815 = DIRECTION ( 'NONE',  ( 0.000000000000000000, 1.000000000000000000, 0.000000000000000000 ) ) ;
#23816 = DIRECTION ( 'NONE',  ( 0.000000000000000000, -1.000000000000000000, 0.000000000000000000 ) ) ;
#23817 = CARTESIAN_POINT ( 'NONE',  ( 0.8338927961504822850, -61.60053577702804262, -12.50366901606078684 ) ) ;
#23818 = CARTESIAN_POINT ( 'NONE',  ( -1.431853854392999947, -78.68203455456848872, -3.695363765894000174 ) ) ;
#23819 = CARTESIAN_POINT ( 'NONE',  ( 9.361362996599000397, -77.96271332859899417, 2.353468592436000151 ) ) ;
#23820 = AXIS2_PLACEMENT_3D ( 'NONE', #7214, #6924, #24930 ) ;
#23821 = CARTESIAN_POINT ( 'NONE',  ( -12.83838672491000032, -18.79401612030999758, 2.062170725306000207 ) ) ;
#23822 = CARTESIAN_POINT ( 'NONE',  ( -0.4796248374066554576, -83.00640320879189460, 1.154279267341133952 ) ) ;
#23823 = CARTESIAN_POINT ( 'NONE',  ( 0.5999999999999999778, -5.000000000000000000, -0.5999999999999999778 ) ) ;
#23824 = LINE ( 'NONE', #14965, #12877 ) ;
#23825 = CARTESIAN_POINT ( 'NONE',  ( 0.007687615972125512107, -79.99999999999997158, 9.299168372948120265 ) ) ;
#23826 = FACE_OUTER_BOUND ( 'NONE', #49154, .T. ) ;
#23827 = EDGE_CURVE ( 'NONE', #41145, #15626, #57670, .T. ) ;
#23828 = CARTESIAN_POINT ( 'NONE',  ( 10.18491068058999893, -55.49283065365000311, 7.640030139739999449 ) ) ;
#23830 = EDGE_CURVE ( 'NONE', #13151, #55023, #14759, .T. ) ;
#23829 = CARTESIAN_POINT ( 'NONE',  ( -2.062312494845999655, -23.22715659892999795, -12.83634740209000036 ) ) ;
#23831 = CARTESIAN_POINT ( 'NONE',  ( 3.079612352930999997, -2.255588905189000126, -1.632544367598999902 ) ) ;
#23832 = CARTESIAN_POINT ( 'NONE',  ( 0.000000000000000000, -77.50000000000000000, 0.000000000000000000 ) ) ;
#23833 = CARTESIAN_POINT ( 'NONE',  ( -10.21414511300999983, -77.32657859425000879, 6.816672119949999775 ) ) ;
#23834 = CARTESIAN_POINT ( 'NONE',  ( -9.834111732579202680, -78.13812671110433428, -5.101590220333411807 ) ) ;
#23836 = CARTESIAN_POINT ( 'NONE',  ( -1.308715794654506714, -24.74404499199616225, -12.70256747356970628 ) ) ;
#23835 = CARTESIAN_POINT ( 'NONE',  ( 1.629367637654999923, -60.48263643365999798, 12.46114270829000148 ) ) ;
#23837 = CARTESIAN_POINT ( 'NONE',  ( -10.11011427823000020, -76.30152490496999462, -6.578289829005000477 ) ) ;
#23838 = VERTEX_POINT ( 'NONE', #54130 ) ;
#23839 = CARTESIAN_POINT ( 'NONE',  ( 3.756303339431999788, -85.75721544543100094, 0.03933749637742999655 ) ) ;
#23840 = CARTESIAN_POINT ( 'NONE',  ( 1.841799093115999986, -80.57082220907369674, 11.13776847689000071 ) ) ;
#23841 = ADVANCED_FACE ( 'NONE', ( #41127 ), #722, .T. ) ;
#23842 = CARTESIAN_POINT ( 'NONE',  ( 8.766282146675060005, -78.32424052224494915, -2.952264042087271001 ) ) ;
#23843 = CARTESIAN_POINT ( 'NONE',  ( -1.500000000000000222, -81.51041666666667140, -0.1963495408493622085 ) ) ;
#23844 = CARTESIAN_POINT ( 'NONE',  ( -2.185791986076000004, -78.01107598727000436, -11.00183730042999919 ) ) ;
#23845 = CARTESIAN_POINT ( 'NONE',  ( 12.77657003520000067, -53.48789974419999993, -0.1588669551757000142 ) ) ;
#23846 = CARTESIAN_POINT ( 'NONE',  ( -1.966850719965000494, -77.43800492889899090, -9.538930191946999315 ) ) ;
#23847 = CARTESIAN_POINT ( 'NONE',  ( 1.611423453808999984, -81.65923367201999383, 0.4225784326546000447 ) ) ;
#23848 = CYLINDRICAL_SURFACE ( 'NONE', #38727, 10.75000000000000000 ) ;
#23849 = CARTESIAN_POINT ( 'NONE',  ( 5.533470947122165917, -81.00000000000000000, -9.578222253839143718 ) ) ;
#23850 = ORIENTED_EDGE ( 'NONE', *, *, #22132, .T. ) ;
#23851 = CARTESIAN_POINT ( 'NONE',  ( -1.423702045482348355, -0.7708333333332365589, 3.195623485684481846 ) ) ;
#23852 = CARTESIAN_POINT ( 'NONE',  ( 10.78853149093999875, -80.42508047494558809, -3.242959171380999983 ) ) ;
#23853 = CARTESIAN_POINT ( 'NONE',  ( 0.000000000000000000, -6.100000000000000533, 0.000000000000000000 ) ) ;
#23854 = ORIENTED_EDGE ( 'NONE', *, *, #38292, .F. ) ;
#23855 = CARTESIAN_POINT ( 'NONE',  ( 0.6284244718204999858, -78.29838485580960139, -1.176290284212999859 ) ) ;
#23856 = AXIS2_PLACEMENT_3D ( 'NONE', #57769, #39180, #7315 ) ;
#23857 = CARTESIAN_POINT ( 'NONE',  ( -1.919663510025999997, -79.79090199409699835, -11.39231233529999976 ) ) ;
#23858 = VERTEX_POINT ( 'NONE', #54997 ) ;
#23859 = CARTESIAN_POINT ( 'NONE',  ( -8.274737932560000786, -78.82433465545000217, -8.916907688993001457 ) ) ;
#23860 = CARTESIAN_POINT ( 'NONE',  ( -8.573168234377000374, -77.43733401092899271, 7.225480548498000033 ) ) ;
#23861 = DIRECTION ( 'NONE',  ( -0.7071067811865475727, 0.000000000000000000, 0.7071067811865475727 ) ) ;
#23862 = B_SPLINE_CURVE_WITH_KNOTS ( 'NONE', 3,
 ( #29016, #15145, #15446, #28716, #14559, #10436 ),
 .UNSPECIFIED., .F., .F.,
 ( 4, 1, 1, 4 ),
 ( 0.000000000000000000, 0.3333333311588953518, 0.6666666623178907347, 0.9999999934767860310 ),
 .UNSPECIFIED. ) ;
#23863 = ORIENTED_EDGE ( 'NONE', *, *, #53645, .T. ) ;
#23864 = VERTEX_POINT ( 'NONE', #36984 ) ;
#23865 = CIRCLE ( 'NONE', #31392, 8.500000000000000000 ) ;
#23866 = LINE ( 'NONE', #31839, #44286 ) ;
#23867 = VECTOR ( 'NONE', #27532, 1000.000000000000000 ) ;
#23868 = B_SPLINE_CURVE_WITH_KNOTS ( 'NONE', 3,
 ( #48101, #43363, #2922, #38350, #42795, #47817, #20639, #43087, #16214, #25634 ),
 .UNSPECIFIED., .F., .F.,
 ( 4, 2, 2, 2, 4 ),
 ( 0.000000000000000000, 0.2500000000000000000, 0.5000000000000000000, 0.7500000000000000000, 1.000000000000000000 ),
 .UNSPECIFIED. ) ;
#23869 = CARTESIAN_POINT ( 'NONE',  ( 1.841371367509999857, -80.15039977323749554, -9.592189096167999196 ) ) ;
#23870 = ORIENTED_EDGE ( 'NONE', *, *, #24591, .F. ) ;
#23871 = CARTESIAN_POINT ( 'NONE',  ( 12.79895942951000087, -54.99538174351000208, 2.015930660723999956 ) ) ;
#23872 = CARTESIAN_POINT ( 'NONE',  ( 7.764217752274555018, -24.25600304964931198, -10.21028588416213800 ) ) ;
#23873 = VERTEX_POINT ( 'NONE', #27534 ) ;
#23874 = CARTESIAN_POINT ( 'NONE',  ( -12.43359700617999941, -24.70705514168999883, -0.8500729763772000291 ) ) ;
#23875 = CARTESIAN_POINT ( 'NONE',  ( 8.251802458334349666, -24.80055625133919150, 9.431055090842324518 ) ) ;
#23876 = EDGE_CURVE ( 'NONE', #1253, #51133, #13965, .T. ) ;
#23877 = DIRECTION ( 'NONE',  ( 0.000000000000000000, -1.000000000000000000, 9.095767555747001212E-12 ) ) ;
#23878 = CARTESIAN_POINT ( 'NONE',  ( 1.197231442357009623, -77.88020833347827931, -0.6890657380265718945 ) ) ;
#23879 = DIRECTION ( 'NONE',  ( 3.675128825892999315E-09, -0.9999999999999997780, -2.168720766502999921E-08 ) ) ;
#23880 = CARTESIAN_POINT ( 'NONE',  ( 4.571463104798961119, -86.25171438276198899, 0.5247301960419221700 ) ) ;
#23881 = CARTESIAN_POINT ( 'NONE',  ( -12.70253230850552484, -17.02944272789559577, -0.9891673677432125666 ) ) ;
#23882 = CARTESIAN_POINT ( 'NONE',  ( -1.115567212185924584, -78.90965635352397101, -1.056363245188180811 ) ) ;
#23883 = CARTESIAN_POINT ( 'NONE',  ( -3.389161288344675782, -78.83489581379073741, -2.147886495578234189 ) ) ;
#23884 = ORIENTED_EDGE ( 'NONE', *, *, #48808, .F. ) ;
#23885 = CARTESIAN_POINT ( 'NONE',  ( 1.623944433304999935, -76.15286196370999505, -12.20239005717999881 ) ) ;
#23886 = CARTESIAN_POINT ( 'NONE',  ( -0.6665627444282328229, -2.459101225494768173, -3.519322218571878658 ) ) ;
#23887 = FACE_OUTER_BOUND ( 'NONE', #31837, .T. ) ;
#23888 = CARTESIAN_POINT ( 'NONE',  ( 8.438902753042999194, -78.66805746472999772, -8.898539530003999332 ) ) ;
#23889 = CARTESIAN_POINT ( 'NONE',  ( -8.987350104473000201, -77.00643677264099551, 8.369597699504998545 ) ) ;
#23890 = CARTESIAN_POINT ( 'NONE',  ( -10.14950121161999874, -59.55077027461999961, -7.674627477469999626 ) ) ;
#23891 = CARTESIAN_POINT ( 'NONE',  ( -7.160332295859999974, -76.82136498579799877, 6.396111552352999219 ) ) ;
#23892 = CARTESIAN_POINT ( 'NONE',  ( 11.93057425389842230, -78.28777072277550531, -1.853708691180695034 ) ) ;
#23893 = DIRECTION ( 'NONE',  ( -1.000000000000000000, 0.000000000000000000, 0.000000000000000000 ) ) ;
#23894 = AXIS2_PLACEMENT_3D ( 'NONE', #2917, #20916, #38919 ) ;
#23895 = VERTEX_POINT ( 'NONE', #50292 ) ;
#23897 = EDGE_CURVE ( 'NONE', #1042, #45906, #23134, .T. ) ;
#23896 = CARTESIAN_POINT ( 'NONE',  ( -12.50000000000000000, -55.55000000278000272, 1.750000000000000000 ) ) ;
#23898 = CARTESIAN_POINT ( 'NONE',  ( -9.358039826156000274, -77.40277834972398807, -1.148306349242000035 ) ) ;
#23899 = DIRECTION ( 'NONE',  ( -1.000000000000000000, 0.000000000000000000, 0.000000000000000000 ) ) ;
#23900 = CARTESIAN_POINT ( 'NONE',  ( 1.092232985442820992, -78.79166666666664298, 0.6295237254636267821 ) ) ;
#23901 = CARTESIAN_POINT ( 'NONE',  ( 3.866260457929000083, -2.040678692333000033, -0.1798930524384000085 ) ) ;
#23902 = VECTOR ( 'NONE', #50507, 1000.000000000000000 ) ;
#23903 = CARTESIAN_POINT ( 'NONE',  ( 7.889971116623999414, -77.39411321036999425, 8.954543982858998774 ) ) ;
#23904 = CARTESIAN_POINT ( 'NONE',  ( 1.867960828343000035, -78.56640489213999956, 9.447959161044998666 ) ) ;
#23906 = DIRECTION ( 'NONE',  ( 0.000000000000000000, 1.000000000000000000, 0.000000000000000000 ) ) ;
#23905 = CARTESIAN_POINT ( 'NONE',  ( -8.279988104818777117, -76.13722974528235454, 8.336922021432648933 ) ) ;
#23907 = CARTESIAN_POINT ( 'NONE',  ( 8.500174178665998781, -78.72261268016799818, -6.849988769802000554 ) ) ;
#23908 = CARTESIAN_POINT ( 'NONE',  ( 4.093343120888095932, -85.83735717367099483, 0.4698497371742681450 ) ) ;
#23909 = ORIENTED_EDGE ( 'NONE', *, *, #37415, .T. ) ;
#23910 = CARTESIAN_POINT ( 'NONE',  ( 12.70299718800749034, -25.02583482805175308, 0.8845454261173205657 ) ) ;
#23911 = CARTESIAN_POINT ( 'NONE',  ( 3.999999999993000266, -77.30000000000720206, -8.632702228606999814E-11 ) ) ;
#23912 = EDGE_CURVE ( 'NONE', #6475, #33222, #40192, .T. ) ;
#23913 = CARTESIAN_POINT ( 'NONE',  ( 5.413904038987143785, -77.33333333333332860, 9.393203674808290771 ) ) ;
#23914 = CARTESIAN_POINT ( 'NONE',  ( -8.631379868284000167, -78.43747063879398240, 6.779623747090999686 ) ) ;
#23915 = ADVANCED_FACE ( 'NONE', ( #14253 ), #142, .F. ) ;
#23916 = CARTESIAN_POINT ( 'NONE',  ( -1.135826688880000157, -81.40663953506998496, -0.9797437077257000748 ) ) ;
#23917 = CARTESIAN_POINT ( 'NONE',  ( -2.833621800687999848, -79.24439682224598869, -9.245833289607000793 ) ) ;
#23918 = CARTESIAN_POINT ( 'NONE',  ( 7.981651535810999398, -17.28135615487000010, -10.08154952397000059 ) ) ;
#23919 = CARTESIAN_POINT ( 'NONE',  ( 7.714303428875997959, -52.49705297113997204, -12.53545825868000385 ) ) ;
#23920 = EDGE_LOOP ( 'NONE', ( #2478, #6598, #38828, #6370, #13843, #6225, #12108, #24445, #29531, #14121, #36602 ) ) ;
#23921 = CARTESIAN_POINT ( 'NONE',  ( 0.9616906432771999969, -78.90839416819699181, -11.22092312000000014 ) ) ;
#23922 = CARTESIAN_POINT ( 'NONE',  ( 12.80000000000000071, -6.000000000000000000, 0.000000000000000000 ) ) ;
#23923 = CARTESIAN_POINT ( 'NONE',  ( 8.718213946067898235, -79.51041666666540664, -3.877033209321456120 ) ) ;
#23924 = CARTESIAN_POINT ( 'NONE',  ( -9.998152690805172327, -77.90614940129853494, 6.679595771618969557 ) ) ;
#23925 = CARTESIAN_POINT ( 'NONE',  ( -0.6571235693794531540, -81.51954227144281617, 1.063877270815418274 ) ) ;
#23926 = CARTESIAN_POINT ( 'NONE',  ( 5.745827208979935818, -78.68211204270377834, 9.633643064159604918 ) ) ;
#23927 = CARTESIAN_POINT ( 'NONE',  ( -9.240267274125507413, -76.99999999999998579, 1.212345689707036156 ) ) ;
#23928 = CARTESIAN_POINT ( 'NONE',  ( -2.963791440107999886, -3.194030605494999620, 2.387889716789000083 ) ) ;
#23929 = EDGE_CURVE ( 'NONE', #19894, #23873, #37372, .T. ) ;
#23930 = CARTESIAN_POINT ( 'NONE',  ( 0.8011517691903999872, -77.75748566455999367, -1.033896367111999837 ) ) ;
#23931 = CARTESIAN_POINT ( 'NONE',  ( 1.704789469149224468, -18.29653838474853345, -12.53199752960647828 ) ) ;
#23932 = CARTESIAN_POINT ( 'NONE',  ( -2.928650166838424607, -78.84659571151506441, 10.57784605029244318 ) ) ;
#23933 = AXIS2_PLACEMENT_3D ( 'NONE', #17752, #9479, #22464 ) ;
#23934 = CARTESIAN_POINT ( 'NONE',  ( 3.140974612311327796, -77.15416666666668277, 11.68767212001979594 ) ) ;
#23935 = EDGE_LOOP ( 'NONE', ( #57059, #7534, #55035, #13547, #12153 ) ) ;
#23936 = ORIENTED_EDGE ( 'NONE', *, *, #7844, .T. ) ;
#23937 = CARTESIAN_POINT ( 'NONE',  ( 5.365645860858369254, -77.72750000000002046, 7.890595865543486020 ) ) ;
#23938 = CARTESIAN_POINT ( 'NONE',  ( 6.833867832890341276, -78.77991242188969068, -8.298164777206682885 ) ) ;
#23939 = EDGE_LOOP ( 'NONE', ( #7540, #9412, #7596, #25059 ) ) ;
#23940 = CYLINDRICAL_SURFACE ( 'NONE', #56686, 10.69999999999999929 ) ;
#23941 = EDGE_CURVE ( 'NONE', #34968, #43600, #23412, .T. ) ;
#23942 = CARTESIAN_POINT ( 'NONE',  ( -1.500000000000000444, -80.38958333333332007, 0.1963495408493560745 ) ) ;
#23943 = EDGE_CURVE ( 'NONE', #43546, #18440, #32248, .T. ) ;
#23944 = CARTESIAN_POINT ( 'NONE',  ( 10.19019669288000074, -59.99643762534999780, 7.646965578510999784 ) ) ;
#23945 = CARTESIAN_POINT ( 'NONE',  ( 0.000000000000000000, -23.25000000000000000, 12.00000000000000000 ) ) ;
#23946 = CARTESIAN_POINT ( 'NONE',  ( -0.7928288024956133828, -78.66963330304734825, -11.95371966526608176 ) ) ;
#23947 = CARTESIAN_POINT ( 'NONE',  ( 5.986115112277999195, -80.16409694029599109, 9.486000076385000312 ) ) ;
#23948 = ORIENTED_EDGE ( 'NONE', *, *, #7086, .F. ) ;
#23949 = DIRECTION ( 'NONE',  ( 1.000000000000000000, 0.000000000000000000, 0.000000000000000000 ) ) ;
#23950 = VERTEX_POINT ( 'NONE', #40841 ) ;
#23951 = CARTESIAN_POINT ( 'NONE',  ( 8.775623107093144526, -77.37563063860072532, 2.924238520614950598 ) ) ;
#23952 = CARTESIAN_POINT ( 'NONE',  ( -8.799999998347999508, 1.651506137787999915E-09, -5.811488053374000191E-09 ) ) ;
#23953 = CARTESIAN_POINT ( 'NONE',  ( -1.317826160292999926, -77.51678331097843966, 0.5319603796220000458 ) ) ;
#23954 = DIRECTION ( 'NONE',  ( -0.9999999999995751176, 0.000000000000000000, -9.217549095371770968E-07 ) ) ;
#23955 = DIRECTION ( 'NONE',  ( 0.000000000000000000, -1.000000000000000000, 0.000000000000000000 ) ) ;
#23956 = CARTESIAN_POINT ( 'NONE',  ( -0.9536002873971000104, -79.19521021049000353, 1.318830682536000110 ) ) ;
#23957 = CARTESIAN_POINT ( 'NONE',  ( -9.400797763902113857, -79.31390857863736699, -1.591501164855807948 ) ) ;
#23958 = CARTESIAN_POINT ( 'NONE',  ( -0.9292580750797257982, -79.15854484711744021, -0.8358713317426036404 ) ) ;
#23959 = CARTESIAN_POINT ( 'NONE',  ( -9.475012188928999990, -79.38752739508899481, 5.469182786826999987 ) ) ;
#23960 = DIRECTION ( 'NONE',  ( 0.000000000000000000, -1.000000000000000000, 0.000000000000000000 ) ) ;
#23961 = CARTESIAN_POINT ( 'NONE',  ( -8.252521514711000705, -24.93405767894999769, -9.650901483139000092 ) ) ;
#23962 = AXIS2_PLACEMENT_3D ( 'NONE', #10836, #28812, #6388 ) ;
#23963 = CARTESIAN_POINT ( 'NONE',  ( 9.546815224142999767, -17.31472046677999899, 8.130854305520999858 ) ) ;
#23964 = CARTESIAN_POINT ( 'NONE',  ( 3.546854729627999969, -85.46506550819998438, 0.03730069855218000330 ) ) ;
#23965 = VERTEX_POINT ( 'NONE', #22539 ) ;
#23966 = CARTESIAN_POINT ( 'NONE',  ( -1.570796326794884790, -79.51458333333332007, -12.00000000000000355 ) ) ;
#23967 = CARTESIAN_POINT ( 'NONE',  ( -1.468405992501000012, -81.36252996976000418, 0.5987774653158000060 ) ) ;
#23968 = CARTESIAN_POINT ( 'NONE',  ( 10.36866725643501752, -77.87135762240245640, 2.843763427746201611 ) ) ;
#23969 = B_SPLINE_CURVE_WITH_KNOTS ( 'NONE', 3,
 ( #11547, #17114, #35100, #11257, #16544, #29238, #34238, #38970, #47580, #2966, #47285, #2397, #52558, #51992, #52845, #3261, #15963, #12111, #47860, #20966, #25105, #48147, #7677, #43132, #25678, #2690, #20683, #38682, #30096, #16259 ),
 .UNSPECIFIED., .F., .F.,
 ( 4, 2, 2, 2, 2, 2, 2, 2, 2, 2, 2, 2, 2, 2, 4 ),
 ( 0.000000000000000000, 0.1250000000000017764, 0.1875000000000011380, 0.2500000000000004996, 0.3124999999999998890, 0.3749999999999992784, 0.4999999999999981126, 0.5624999999999975575, 0.6249999999999970024, 0.6874999999999964473, 0.7499999999999958922, 0.8124999999999953371, 0.8437499999999951150, 0.8749999999999948930, 1.000000000000000000 ),
 .UNSPECIFIED. ) ;
#23970 = CARTESIAN_POINT ( 'NONE',  ( 4.899854808515000215, -78.22463711524899566, -10.93194800986000104 ) ) ;
#23971 = CARTESIAN_POINT ( 'NONE',  ( -7.646091287767998956, -18.29149945126999910, 10.13691902392999999 ) ) ;
#23972 = CONICAL_SURFACE ( 'NONE', #9825, 12.14999999923000118, 0.7853981633972997312 ) ;
#23973 = CARTESIAN_POINT ( 'NONE',  ( 6.606447392468458801, -78.92306693067979495, 8.596639545930225168 ) ) ;
#23974 = CARTESIAN_POINT ( 'NONE',  ( -3.095526911397207925, -3.210505338566441491, 1.678399268257390942 ) ) ;
#23975 = CARTESIAN_POINT ( 'NONE',  ( 10.34875727357672304, -80.87214758697167838, 2.910059915723667512 ) ) ;
#23976 = CARTESIAN_POINT ( 'NONE',  ( -9.066428667704000688, -77.55751470757499533, 2.532008238717000204 ) ) ;
#23977 = CARTESIAN_POINT ( 'NONE',  ( 10.61613183210000066, -77.68694788753698788, -2.999913216257000137 ) ) ;
#23978 = CARTESIAN_POINT ( 'NONE',  ( 3.269729146447236889, -0.8932291625415327285, -0.8778406017527962124 ) ) ;
#23979 = CARTESIAN_POINT ( 'NONE',  ( -5.138300599984000350, -81.11256919153379386, -9.625040225332000432 ) ) ;
#23980 = EDGE_LOOP ( 'NONE', ( #3118, #51327, #43759, #10068 ) ) ;
#23981 = CARTESIAN_POINT ( 'NONE',  ( -0.05395919428434999693, -80.88743994373099611, -1.332567581519000122 ) ) ;
#23982 = B_SPLINE_CURVE_WITH_KNOTS ( 'NONE', 3,
 ( #46007, #1136, #33263, #51304 ),
 .UNSPECIFIED., .F., .F.,
 ( 4, 4 ),
 ( 0.000000000000000000, 1.000000000000000000 ),
 .UNSPECIFIED. ) ;
#23983 = AXIS2_PLACEMENT_3D ( 'NONE', #17108, #18293, #35094 ) ;
#23984 = CARTESIAN_POINT ( 'NONE',  ( 1.200170490667999967, -61.23405701964999537, -12.43444080554000131 ) ) ;
#23985 = CARTESIAN_POINT ( 'NONE',  ( -5.413111254871178168, -80.51674528042237000, 9.391950811569177660 ) ) ;
#23986 = EDGE_CURVE ( 'NONE', #13118, #21333, #1006, .T. ) ;
#23987 = CARTESIAN_POINT ( 'NONE',  ( 5.151324428776999476, -77.60313545069999464, 9.964033682248000900 ) ) ;
#23988 = CARTESIAN_POINT ( 'NONE',  ( 8.318585563179999198, -78.17640301578899198, 7.159970128962999780 ) ) ;
#23989 = CARTESIAN_POINT ( 'NONE',  ( 7.961052042448998556, -24.53567435024999810, -9.783216378915000178 ) ) ;
#23990 = EDGE_CURVE ( 'NONE', #16460, #3531, #27301, .T. ) ;
#23991 = CARTESIAN_POINT ( 'NONE',  ( 3.797598824419751384, -83.86458332889966982, -1.413738007671073271 ) ) ;
#23992 = LINE ( 'NONE', #1290, #26992 ) ;
#23993 = DIRECTION ( 'NONE',  ( 0.000000000000000000, 1.000000000000000000, 0.000000000000000000 ) ) ;
#23994 = CARTESIAN_POINT ( 'NONE',  ( 2.191089288545000180, -85.67417953870899794, 3.550449196403000052 ) ) ;
#23995 = CARTESIAN_POINT ( 'NONE',  ( 1.500000000000000000, -79.75000000000000000, 0.000000000000000000 ) ) ;
#23996 = CARTESIAN_POINT ( 'NONE',  ( 7.646944981205999525, -55.60364172484999301, -10.19022195329000091 ) ) ;
#23997 = CARTESIAN_POINT ( 'NONE',  ( -9.563148796606999014, -77.23231152193199023, 5.948121522994000543 ) ) ;
#23998 = CARTESIAN_POINT ( 'NONE',  ( -0.5713041596650000331, -79.42507309447999830, -1.442599867604999808 ) ) ;
#23999 = CARTESIAN_POINT ( 'NONE',  ( -0.6358204470927000251, -78.04511904209999784, -1.286007741733000032 ) ) ;
#24000 = PLANE ( 'NONE',  #56563 ) ;
#24001 = DIRECTION ( 'NONE',  ( 0.000000000000000000, 1.000000000000000000, 0.000000000000000000 ) ) ;
#24002 = CARTESIAN_POINT ( 'NONE',  ( -0.9519843368319620414, -83.27853334735807778, 1.174365823974324652 ) ) ;
#24003 = ORIENTED_EDGE ( 'NONE', *, *, #23897, .F. ) ;
#24004 = CARTESIAN_POINT ( 'NONE',  ( -8.300970689365446020, -77.84166666666669698, -4.784380313523547201 ) ) ;
#24005 = EDGE_CURVE ( 'NONE', #27991, #13401, #3373, .T. ) ;
#24006 = CARTESIAN_POINT ( 'NONE',  ( -9.841113773926924324, -53.96371975908724750, 8.121706172282767255 ) ) ;
#24007 = ORIENTED_EDGE ( 'NONE', *, *, #3721, .T. ) ;
#24008 = CARTESIAN_POINT ( 'NONE',  ( -0.9160563294565400305, -81.66020893391389279, -0.8511632488320945988 ) ) ;
#24009 = EDGE_CURVE ( 'NONE', #46616, #20659, #12161, .T. ) ;
#24010 = PRESENTATION_STYLE_ASSIGNMENT (( #47061 ) ) ;
#24011 = CARTESIAN_POINT ( 'NONE',  ( 3.572416533754999790, -80.30722375786560008, 10.28603406935999942 ) ) ;
#24012 = AXIS2_PLACEMENT_3D ( 'NONE', #12507, #34642, #13075 ) ;
#24013 = CARTESIAN_POINT ( 'NONE',  ( -0.9995835529977249445, -80.05208333333331439, -0.7681833999686439318 ) ) ;
#24014 = ORIENTED_EDGE ( 'NONE', *, *, #35064, .T. ) ;
#24015 = CARTESIAN_POINT ( 'NONE',  ( 1.269301140243999759, -81.81594247561099564, -0.6316121951705000459 ) ) ;
#24016 = B_SPLINE_CURVE_WITH_KNOTS ( 'NONE', 3,
 ( #9006, #50330, #36440, #41459, #27286, #26991 ),
 .UNSPECIFIED., .F., .F.,
 ( 4, 2, 4 ),
 ( 0.000000000000000000, 0.5000000000000000000, 1.000000000000000000 ),
 .UNSPECIFIED. ) ;
#24017 = VECTOR ( 'NONE', #24635, 1000.000000000000000 ) ;
#24018 = EDGE_LOOP ( 'NONE', ( #13765, #51845, #50021, #30168 ) ) ;
#24019 = ORIENTED_EDGE ( 'NONE', *, *, #47097, .T. ) ;
#24020 = CARTESIAN_POINT ( 'NONE',  ( -1.382886570147999983, -17.36901780168000187, 12.65982054476000052 ) ) ;
#24021 = CARTESIAN_POINT ( 'NONE',  ( -9.546815223803999828, -54.11472046612000497, -8.130854305859001485 ) ) ;
#24022 = APPLICATION_PROTOCOL_DEFINITION ( 'draft international standard', 'automotive_design', 1998, #40183 ) ;
#24023 = CARTESIAN_POINT ( 'NONE',  ( -3.233969914661031897, -81.78333331850373611, -1.182064197856841803 ) ) ;
#24024 = EDGE_CURVE ( 'NONE', #40455, #25733, #11843, .T. ) ;
#24025 = CARTESIAN_POINT ( 'NONE',  ( -0.6670706960860000034, -78.20096001420199627, 10.00022801703000042 ) ) ;
#24026 = CONICAL_SURFACE ( 'NONE', #25904, 10.29999999923999887, 0.7853981633972997312 ) ;
#24027 = CARTESIAN_POINT ( 'NONE',  ( 6.647991942108485652, -78.28881406770516094, -6.431782383451233542 ) ) ;
#24028 = DIRECTION ( 'NONE',  ( 0.000000000000000000, -1.000000000000000000, 0.000000000000000000 ) ) ;
#24029 = EDGE_LOOP ( 'NONE', ( #27918, #5501, #9048, #30810 ) ) ;
#24030 = ORIENTED_EDGE ( 'NONE', *, *, #32214, .F. ) ;
#24031 = CARTESIAN_POINT ( 'NONE',  ( -7.514168461771876473, -77.55044855222018896, 5.394443598068082935 ) ) ;
#24032 = CARTESIAN_POINT ( 'NONE',  ( 9.500000000000000000, -77.64999999999999147, 0.000000000000000000 ) ) ;
#24033 = CARTESIAN_POINT ( 'NONE',  ( 0.1963495408493571015, -79.36458333333330017, 1.500000000000000444 ) ) ;
#24034 = CARTESIAN_POINT ( 'NONE',  ( 0.5222397222514810755, -61.96298219368188853, -12.70447686587992564 ) ) ;
#24035 = CARTESIAN_POINT ( 'NONE',  ( -8.771427373352999268, -77.80502451417299881, -4.151237309591000013 ) ) ;
#24036 = CARTESIAN_POINT ( 'NONE',  ( -1.500000000000000000, -79.50000000000000000, 0.000000000000000000 ) ) ;
#24037 = CARTESIAN_POINT ( 'NONE',  ( -1.418579035640199937, -86.00469764872917722, 3.738292511752264513 ) ) ;
#24038 = DIRECTION ( 'NONE',  ( 1.000000000000000000, 0.000000000000000000, 0.000000000000000000 ) ) ;
#24039 = CARTESIAN_POINT ( 'NONE',  ( 0.8322913257134999521, -79.47039037689999930, 1.209850638715999960 ) ) ;
#24040 = EDGE_CURVE ( 'NONE', #7896, #49658, #40174, .T. ) ;
#24041 = CARTESIAN_POINT ( 'NONE',  ( 8.565463562696219668, -77.26519693750341844, -3.984681137958045571 ) ) ;
#24042 = CARTESIAN_POINT ( 'NONE',  ( -4.016244863222999228, -78.72256750329937347, 0.5810441187545000163 ) ) ;
#24043 = FACE_OUTER_BOUND ( 'NONE', #39113, .T. ) ;
#24044 = CARTESIAN_POINT ( 'NONE',  ( -3.218338554480999925, -78.16871001420200571, -9.136931980783000284 ) ) ;
#24045 = CARTESIAN_POINT ( 'NONE',  ( -6.606276669070258123, -76.67304179486919224, -8.596475147758464885 ) ) ;
#24046 = CARTESIAN_POINT ( 'NONE',  ( -7.624757993428000091, -18.19647951307999989, -10.47516388919000008 ) ) ;
#24048 = CARTESIAN_POINT ( 'NONE',  ( -1.150888948972000003, -79.22350888264300295, 0.6738713386821000295 ) ) ;
#24047 = PLANE ( 'NONE',  #34419 ) ;
#24049 = CARTESIAN_POINT ( 'NONE',  ( -10.50000000000000000, -7.000000000000000000, -5.990939290788000838E-12 ) ) ;
#24050 = DIRECTION ( 'NONE',  ( 1.000000000000000000, 0.000000000000000000, 0.000000000000000000 ) ) ;
#24051 = CARTESIAN_POINT ( 'NONE',  ( 0.07399134906894000441, -2.225452884884000060, 3.805339572302000040 ) ) ;
#24052 = CARTESIAN_POINT ( 'NONE',  ( 9.760313732895301797, -77.19999999999998863, -4.644364491930659256 ) ) ;
#24053 = ORIENTED_EDGE ( 'NONE', *, *, #9229, .F. ) ;
#24054 = CARTESIAN_POINT ( 'NONE',  ( -2.879226727952071574, -78.30416666666667425, -10.71369944335147473 ) ) ;
#24055 = CARTESIAN_POINT ( 'NONE',  ( -2.899238502638000092, -78.22541024847198798, -11.05877603816999866 ) ) ;
#24056 = CARTESIAN_POINT ( 'NONE',  ( 11.44555184246232749, -77.46784554053439820, 3.079248999555209032 ) ) ;
#24057 = B_SPLINE_CURVE_WITH_KNOTS ( 'NONE', 3,
 ( #545, #26767, #26472, #27650, #36803, #8776 ),
 .UNSPECIFIED., .F., .F.,
 ( 4, 1, 1, 4 ),
 ( 0.000000000000000000, 0.3333333311524483422, 0.6666666623049967155, 0.9999999934574449467 ),
 .UNSPECIFIED. ) ;
#24058 = VECTOR ( 'NONE', #12274, 1000.000000000000000 ) ;
#24059 = CARTESIAN_POINT ( 'NONE',  ( 6.097124503614000268, -79.21358821443999432, 7.470160346181000222 ) ) ;
#24060 = CARTESIAN_POINT ( 'NONE',  ( 0.000000000000000000, -15.89905023022000030, 0.000000000000000000 ) ) ;
#24061 = LINE ( 'NONE', #19639, #31345 ) ;
#24062 = AXIS2_PLACEMENT_3D ( 'NONE', #25353, #53092, #12644 ) ;
#24063 = DIRECTION ( 'NONE',  ( 1.000000000000000000, 0.000000000000000000, 0.000000000000000000 ) ) ;
#24064 = VECTOR ( 'NONE', #30200, 1000.000000000000114 ) ;
#24065 = DIRECTION ( 'NONE',  ( 0.000000000000000000, -1.000000000000000000, 0.000000000000000000 ) ) ;
#24066 = CARTESIAN_POINT ( 'NONE',  ( 1.004082900143999924, -77.81128302612299308, -11.22932683135000076 ) ) ;
#24067 = CARTESIAN_POINT ( 'NONE',  ( -2.495479390352245197, -76.30759454100098083, -11.48357277819591893 ) ) ;
#24068 = CARTESIAN_POINT ( 'NONE',  ( 0.4053230381024000017, -81.20600532260299076, 1.450728874481000075 ) ) ;
#24069 = CARTESIAN_POINT ( 'NONE',  ( 0.000000000000000000, -75.10000000019110189, 0.000000000000000000 ) ) ;
#24070 = CARTESIAN_POINT ( 'NONE',  ( 0.8359750594766999221, -78.65288999989098784, -9.376158072868999938 ) ) ;
#24072 = CARTESIAN_POINT ( 'NONE',  ( -0.8506806241676722058, -2.895833333333333481, 3.165411199172022627 ) ) ;
#24071 = CARTESIAN_POINT ( 'NONE',  ( -0.7467939645478000044, -84.06554135855498089, 3.892080259883999638 ) ) ;
#24073 = CARTESIAN_POINT ( 'NONE',  ( 5.645287065787000458, -79.39464805011499493, 7.708789581145000014 ) ) ;
#24074 = DIRECTION ( 'NONE',  ( 0.000000000000000000, 0.000000000000000000, -1.000000000000000000 ) ) ;
#24075 = DIRECTION ( 'NONE',  ( 0.000000000000000000, -1.000000000000000000, 0.000000000000000000 ) ) ;
#24076 = CARTESIAN_POINT ( 'NONE',  ( -6.938593657451757046, -77.16921983703690557, -8.210840360290770690 ) ) ;
#24077 = CARTESIAN_POINT ( 'NONE',  ( 7.596835002782696300, -77.20208333333333428, 5.838193839761711246 ) ) ;
#24078 = EDGE_CURVE ( 'NONE', #2543, #36429, #24190, .T. ) ;
#24079 = ORIENTED_EDGE ( 'NONE', *, *, #58074, .F. ) ;
#24080 = CARTESIAN_POINT ( 'NONE',  ( 6.536979956083999177, -79.37240013963898377, -10.09826910480999906 ) ) ;
#24081 = CARTESIAN_POINT ( 'NONE',  ( 0.000000000000000000, -76.75499999999999545, 0.000000000000000000 ) ) ;
#24082 = DIRECTION ( 'NONE',  ( 0.000000000000000000, 1.000000000000000000, 0.000000000000000000 ) ) ;
#24083 = ORIENTED_EDGE ( 'NONE', *, *, #15421, .F. ) ;
#24084 = CARTESIAN_POINT ( 'NONE',  ( -3.073538647258000189, -78.22768216442000266, -11.53207971834999945 ) ) ;
#24085 = B_SPLINE_CURVE_WITH_KNOTS ( 'NONE', 3,
 ( #32415, #18580, #32705, #50754, #40714, #9710, #5278, #36278, #55162, #50461, #5855, #46622, #14707, #6151, #41877, #49878, #1455, #9422, #19447, #54301, #18285, #13838, #45446, #31835 ),
 .UNSPECIFIED., .F., .F.,
 ( 4, 2, 2, 2, 2, 2, 2, 2, 2, 2, 2, 4 ),
 ( 0.000000000000000000, 0.1249999999999982236, 0.2499999999999964473, 0.3749999999999946709, 0.4374999999999943934, 0.4999999999999941158, 0.6249999999999946709, 0.7499999999999953371, 0.8124999999999942268, 0.8437499999999936717, 0.8749999999999931166, 1.000000000000000000 ),
 .UNSPECIFIED. ) ;
#24086 = ORIENTED_EDGE ( 'NONE', *, *, #31333, .F. ) ;
#24087 = ORIENTED_EDGE ( 'NONE', *, *, #40552, .F. ) ;
#24088 = EDGE_LOOP ( 'NONE', ( #52631, #55184, #30544, #22918 ) ) ;
#24089 = EDGE_CURVE ( 'NONE', #1101, #50911, #25221, .T. ) ;
#24090 = B_SPLINE_CURVE_WITH_KNOTS ( 'NONE', 3,
 ( #38370, #15942, #6795, #24802, #46686, #52250, #29504, #20660, #20376, #29214, #56392, #51688, #7368, #24510, #37495, #42237, #25368, #2943, #55516, #15063, #10658, #51106, #2095, #28636, #33931, #51969, #6206, #24220, #1802, #42526, #56105, #19799, #55813, #11526, #15366 ),
 .UNSPECIFIED., .F., .F.,
 ( 4, 1, 1, 1, 1, 1, 1, 1, 1, 1, 1, 1, 1, 1, 1, 1, 1, 1, 1, 1, 1, 1, 1, 1, 1, 1, 1, 1, 1, 1, 1, 1, 4 ),
 ( 0.000000000000000000, 0.01250039628656018226, 0.04500037037602738765, 0.07750034446551849754, 0.1100003185549878609, 0.1425002926444572382, 0.1750002667339483342, 0.2075002408234176976, 0.2400002149128653839, 0.2725001890023130424, 0.3050001630917607010, 0.3375001371814254636, 0.3700001112708732331, 0.4025000853603208917, 0.4350000594497685502, 0.4675000335392162087, 0.5000000076286638118, 0.5324999817181115258, 0.5649999558075591288, 0.5974999298972240025, 0.6299999039866716055, 0.6624998780761193196, 0.6949998521655670336, 0.7274998262550146366, 0.7599998003444622396, 0.7924997744339099537, 0.8249997485235747163, 0.8574997226130225414, 0.8899996967024700334, 0.9224996707919177474, 0.9549996448813654615, 0.9874996189708130645, 1.000000000000000000 ),
 .UNSPECIFIED. ) ;
#24091 = CARTESIAN_POINT ( 'NONE',  ( 0.7883160775726999470, -81.25894104959499487, 3.458341744451999933 ) ) ;
#24092 = CARTESIAN_POINT ( 'NONE',  ( 12.00000000000000000, -78.04999999999999716, 0.000000000000000000 ) ) ;
#24093 = AXIS2_PLACEMENT_3D ( 'NONE', #53975, #39215, #30343 ) ;
#24094 = ORIENTED_EDGE ( 'NONE', *, *, #58151, .F. ) ;
#24095 = CARTESIAN_POINT ( 'NONE',  ( 1.155800523840101679, -82.81894139901449137, -0.4759988703850971392 ) ) ;
#24096 = CARTESIAN_POINT ( 'NONE',  ( -3.233444005277000155, -2.053647766280000120, 0.09179859873625999256 ) ) ;
#24097 = EDGE_LOOP ( 'NONE', ( #29888, #43819, #19584, #32633, #26119 ) ) ;
#24098 = CARTESIAN_POINT ( 'NONE',  ( 2.398213954452620644, -79.24598686563928140, -8.954150635807138769 ) ) ;
#24099 = CARTESIAN_POINT ( 'NONE',  ( -1.165699973591947547, -78.19533224334435317, 0.9553630080629633703 ) ) ;
#24100 = CARTESIAN_POINT ( 'NONE',  ( -1.670138242175404297, -79.80000000000002558, -11.69453362392147433 ) ) ;
#24101 = CARTESIAN_POINT ( 'NONE',  ( -1.500000000000000000, -81.00000000000000000, 0.000000000000000000 ) ) ;
#24102 = CARTESIAN_POINT ( 'NONE',  ( 12.16339525242990049, -79.21041714176394066, 1.568450607538854236 ) ) ;
#24103 = CARTESIAN_POINT ( 'NONE',  ( 3.066118473086494767, -78.59774452897278252, -10.39032512872745251 ) ) ;
#24105 = ADVANCED_FACE ( 'NONE', ( #49932 ), #56233, .T. ) ;
#24104 = CARTESIAN_POINT ( 'NONE',  ( 11.06808393496999976, -76.45976679461099934, 1.603559079323000125 ) ) ;
#24106 = CARTESIAN_POINT ( 'NONE',  ( 2.217579703669401603, -76.45950790555878029, 10.54848845899178578 ) ) ;
#24107 = CARTESIAN_POINT ( 'NONE',  ( 0.9995835529977264988, -81.19791666666664298, -0.7681833999686417114 ) ) ;
#24108 = EDGE_CURVE ( 'NONE', #45676, #52926, #43955, .T. ) ;
#24109 = CARTESIAN_POINT ( 'NONE',  ( -7.613962745625999062, -60.10639784916000394, -10.53101990622000095 ) ) ;
#24110 = CARTESIAN_POINT ( 'NONE',  ( -7.168972154839425848, -78.65447478827950079, -5.845467487007924845 ) ) ;
#24111 = CARTESIAN_POINT ( 'NONE',  ( 7.912034776018140647, -76.51566614544198330, 8.694818093870058107 ) ) ;
#24112 = CARTESIAN_POINT ( 'NONE',  ( -9.408840690779999960, -77.56876001420199884, 0.2246891580983999825 ) ) ;
#24113 = DIRECTION ( 'NONE',  ( -1.000000000000000000, 0.000000000000000000, 0.000000000000000000 ) ) ;
#24114 = CARTESIAN_POINT ( 'NONE',  ( -3.035031770661409833, -3.072304190615608999, 1.160088070061187304 ) ) ;
#24115 = CARTESIAN_POINT ( 'NONE',  ( 3.643490196435000161, -82.12920122123499311, -0.2401545879082000179 ) ) ;
#24116 = CARTESIAN_POINT ( 'NONE',  ( 8.057735164907999348, -77.48951332859898855, 5.314711785903000418 ) ) ;
#24117 = CARTESIAN_POINT ( 'NONE',  ( -9.993906532420947286, -78.07006040395985735, 3.960656951342677257 ) ) ;
#24118 = CARTESIAN_POINT ( 'NONE',  ( -0.2410965598014278566, -82.99083135149682278, 1.228665170874773338 ) ) ;
#24119 = DIRECTION ( 'NONE',  ( 0.000000000000000000, -1.000000000000000000, 0.000000000000000000 ) ) ;
#24120 = CARTESIAN_POINT ( 'NONE',  ( -1.092232985442824100, -80.45833333333330017, 0.6295237254636200097 ) ) ;
#24121 = CARTESIAN_POINT ( 'NONE',  ( 3.140974612311326908, -79.25416666666664867, 11.68767212001979772 ) ) ;
#24122 = CARTESIAN_POINT ( 'NONE',  ( -10.52682159652000138, -60.22567232035000018, -7.605689092069000345 ) ) ;
#24123 = CARTESIAN_POINT ( 'NONE',  ( 1.375482337540088640, -3.499999999999999112, 3.058649307113923577 ) ) ;
#24124 = CARTESIAN_POINT ( 'NONE',  ( 0.08638142328466999476, -81.00418100790099629, 1.330832257483999914 ) ) ;
#24125 = DIRECTION ( 'NONE',  ( 0.000000000000000000, 1.000000000000000000, 0.000000000000000000 ) ) ;
#24126 = CARTESIAN_POINT ( 'NONE',  ( -7.530775182571000315, -78.12444805011499227, -6.150709233331999037 ) ) ;
#24127 = CARTESIAN_POINT ( 'NONE',  ( -8.611000705966242563, -25.17488119224633536, -9.355851007297125932 ) ) ;
#24128 = EDGE_CURVE ( 'NONE', #26499, #13623, #23339, .T. ) ;
#24129 = CARTESIAN_POINT ( 'NONE',  ( -10.12290050126000196, -60.04999999958999979, -7.648026767103999646 ) ) ;
#24130 = CARTESIAN_POINT ( 'NONE',  ( 10.61050599188999932, -78.32876026662599145, -2.901234667509999809 ) ) ;
#24131 = CARTESIAN_POINT ( 'NONE',  ( -10.90760146693999921, -78.85886288864057292, -1.219937219691999974 ) ) ;
#24132 = CARTESIAN_POINT ( 'NONE',  ( 12.07501500767000024, -76.43047190101000865, 1.824161567967000019 ) ) ;
#24133 = ORIENTED_EDGE ( 'NONE', *, *, #2639, .T. ) ;
#24134 = CARTESIAN_POINT ( 'NONE',  ( 2.891798309966000069, -84.43446544543100174, 2.709886222448000037 ) ) ;
#24135 = STYLED_ITEM ( 'NONE', ( #20863 ), #36811 ) ;
#24136 = CARTESIAN_POINT ( 'NONE',  ( 3.275195660744999682, -81.06043981312450342, 10.80351508457999898 ) ) ;
#24137 = CARTESIAN_POINT ( 'NONE',  ( 7.542821534244515291, -78.30104360775493433, -5.354097004516040315 ) ) ;
#24138 = CARTESIAN_POINT ( 'NONE',  ( 10.27342224347061084, -54.73842478141837375, 7.712153330296829701 ) ) ;
#24139 = DIRECTION ( 'NONE',  ( 0.000000000000000000, 1.000000000000000000, 0.000000000000000000 ) ) ;
#24140 = CARTESIAN_POINT ( 'NONE',  ( 1.000000000000000000, -75.20000000000000284, 7.200000000000000178 ) ) ;
#24141 = CARTESIAN_POINT ( 'NONE',  ( -8.954089450906998593, -78.92307212613098955, -3.546476007522999740 ) ) ;
#24142 = CARTESIAN_POINT ( 'NONE',  ( 0.8286895765316001361, -81.72239288712999894, 1.445177540541999983 ) ) ;
#24143 = CARTESIAN_POINT ( 'NONE',  ( 3.399999999999999911, -78.69999999999998863, 0.000000000000000000 ) ) ;
#24144 = CARTESIAN_POINT ( 'NONE',  ( 10.51823340019644526, -81.00000000000001421, -3.220802781544626292 ) ) ;
#24145 = ORIENTED_EDGE ( 'NONE', *, *, #29545, .T. ) ;
#24146 = CIRCLE ( 'NONE', #51515, 0.6000000000000008660 ) ;
#24147 = DIRECTION ( 'NONE',  ( -1.000000000000000000, 0.000000000000000000, 0.000000000000000000 ) ) ;
#24148 = CARTESIAN_POINT ( 'NONE',  ( -10.42531124903999995, -55.53514851492000304, 7.624341765436000173 ) ) ;
#24149 = FACE_OUTER_BOUND ( 'NONE', #28944, .T. ) ;
#24150 = CARTESIAN_POINT ( 'NONE',  ( 2.655560623658488328, -78.97957698290076678, -2.730538163075394209 ) ) ;
#24151 = CIRCLE ( 'NONE', #45825, 0.8000000000000000444 ) ;
#24152 = VERTEX_POINT ( 'NONE', #9476 ) ;
#24153 = CARTESIAN_POINT ( 'NONE',  ( 0.9834589317531000630, -78.94334895976399480, 0.9007689179829999615 ) ) ;
#24154 = CARTESIAN_POINT ( 'NONE',  ( 9.759566573192998362, -79.51811006564999218, -5.179648052473000419 ) ) ;
#24155 = CARTESIAN_POINT ( 'NONE',  ( -2.309473414332742891, -77.60514816509892455, -9.037436301258047422 ) ) ;
#24156 = LINE ( 'NONE', #56042, #52023 ) ;
#24157 = ORIENTED_EDGE ( 'NONE', *, *, #19611, .T. ) ;
#24158 = CARTESIAN_POINT ( 'NONE',  ( -10.42801618316999956, -78.71581739375498898, 6.264104809848999977 ) ) ;
#24159 = CARTESIAN_POINT ( 'NONE',  ( -11.15272124962999989, -77.63845490982699005, -2.513729164015999995 ) ) ;
#24160 = DIRECTION ( 'NONE',  ( 0.000000000000000000, 0.000000000000000000, -1.000000000000000000 ) ) ;
#24161 = ORIENTED_EDGE ( 'NONE', *, *, #9639, .F. ) ;
#24162 = ORIENTED_EDGE ( 'NONE', *, *, #23512, .T. ) ;
#24163 = CARTESIAN_POINT ( 'NONE',  ( -1.006352879438885184, -80.54967111464023333, 0.7434871015420349005 ) ) ;
#24164 = EDGE_CURVE ( 'NONE', #7256, #587, #45877, .T. ) ;
#24165 = CARTESIAN_POINT ( 'NONE',  ( -12.00000000000000355, -79.78958333333331154, 1.570796326794848596 ) ) ;
#24166 = CARTESIAN_POINT ( 'NONE',  ( -9.699833017908000343, -79.38109376462799105, 1.146274062705999963 ) ) ;
#24167 = EDGE_LOOP ( 'NONE', ( #28356, #54799, #15665 ) ) ;
#24168 = CARTESIAN_POINT ( 'NONE',  ( 12.54673279569000144, -53.97202488745999460, 0.9078290272348999990 ) ) ;
#24169 = DIRECTION ( 'NONE',  ( 1.000000000000000000, 0.000000000000000000, 0.000000000000000000 ) ) ;
#24170 = EDGE_CURVE ( 'NONE', #45467, #11618, #28859, .T. ) ;
#24171 = ORIENTED_EDGE ( 'NONE', *, *, #39337, .F. ) ;
#24172 = CARTESIAN_POINT ( 'NONE',  ( -12.72558241036999860, -23.20131830507999737, -1.930284820930999956 ) ) ;
#24173 = CARTESIAN_POINT ( 'NONE',  ( -4.342561293556999935, -77.59704415034600800, -8.443909622126001935 ) ) ;
#24174 = DIRECTION ( 'NONE',  ( 0.000000000000000000, 1.000000000000000000, 0.000000000000000000 ) ) ;
#24175 = CARTESIAN_POINT ( 'NONE',  ( -0.2770819934162573883, -80.20771142070574911, -1.219419118597123930 ) ) ;
#24176 = CARTESIAN_POINT ( 'NONE',  ( -1.782734487924091393, -17.87754631440509812, -12.71547286926139186 ) ) ;
#24177 = CARTESIAN_POINT ( 'NONE',  ( 9.723591721872441695, -78.80042913613843325, 0.1588614647341892172 ) ) ;
#24178 = CARTESIAN_POINT ( 'NONE',  ( -9.404328087084998344, -77.22694376941500138, -0.9147582690626000490 ) ) ;
#24179 = EDGE_CURVE ( 'NONE', #45504, #23965, #45205, .T. ) ;
#24180 = CARTESIAN_POINT ( 'NONE',  ( 1.433939993129704771, -78.57056504184866697, -0.5545599285302943438 ) ) ;
#24181 = DIRECTION ( 'NONE',  ( -1.000000000000000000, 0.000000000000000000, 0.000000000000000000 ) ) ;
#24182 = CARTESIAN_POINT ( 'NONE',  ( -9.844172144369998989, -75.93141745127000775, 7.391061701651999272 ) ) ;
#24183 = VECTOR ( 'NONE', #31822, 1000.000000000000000 ) ;
#24184 = CARTESIAN_POINT ( 'NONE',  ( 1.615685760171753360, -2.186269987821578553, 3.127213907787655511 ) ) ;
#24185 = CARTESIAN_POINT ( 'NONE',  ( 12.50000000000000000, -13.07071422275999950, 0.000000000000000000 ) ) ;
#24186 = CARTESIAN_POINT ( 'NONE',  ( -7.766269599678000013, -78.58776125908998722, -9.491266709826000181 ) ) ;
#24187 = CARTESIAN_POINT ( 'NONE',  ( 3.090997446795999970, -77.21135046416598868, -11.88544462247999967 ) ) ;
#24188 = AXIS2_PLACEMENT_3D ( 'NONE', #8730, #31733, #4897 ) ;
#24189 = CARTESIAN_POINT ( 'NONE',  ( 12.70299804978429137, -16.97411689984641470, -0.8844418155417017591 ) ) ;
#24190 = CIRCLE ( 'NONE', #44924, 9.700000000000001066 ) ;
#24191 = CARTESIAN_POINT ( 'NONE',  ( 3.004897403630924391, -2.819918783981688826, -1.236614688018551123 ) ) ;
#24192 = CARTESIAN_POINT ( 'NONE',  ( -9.993982900435000261, -78.00313153835666924, 6.676790657254138672 ) ) ;
#24193 = CARTESIAN_POINT ( 'NONE',  ( -4.019809786096000259, -79.15416738576453781, 10.47183077952999852 ) ) ;
#24194 = AXIS2_PLACEMENT_3D ( 'NONE', #31435, #13730, #26715 ) ;
#24195 = VERTEX_POINT ( 'NONE', #10063 ) ;
#24196 = CARTESIAN_POINT ( 'NONE',  ( -1.288646058034000008, -83.49568302734098779, 0.4058063692239000098 ) ) ;
#24197 = CARTESIAN_POINT ( 'NONE',  ( 5.173304380012000436, -77.06335657913808745, -8.085540331045999451 ) ) ;
#24198 = CARTESIAN_POINT ( 'NONE',  ( 9.346069275190213688, -25.16527745691412221, 8.620894635682162743 ) ) ;
#24199 = VECTOR ( 'NONE', #32933, 1000.000000000000000 ) ;
#24200 = CARTESIAN_POINT ( 'NONE',  ( 0.6295237254636211199, -78.83333333333335702, 1.092232985442824322 ) ) ;
#24201 = CARTESIAN_POINT ( 'NONE',  ( -3.824246539154000146, -2.306685987230000290, -0.5962100206719000983 ) ) ;
#24202 = CARTESIAN_POINT ( 'NONE',  ( -11.80948866808000020, -78.49294670917899452, 2.394107155543000243 ) ) ;
#24203 = CARTESIAN_POINT ( 'NONE',  ( 9.084121021304000010, -77.55017512602198337, 3.512611703280999809 ) ) ;
#24205 = CARTESIAN_POINT ( 'NONE',  ( -5.751575622429521140, -77.09192708334455801, 7.482738014362807277 ) ) ;
#24204 = CARTESIAN_POINT ( 'NONE',  ( -9.012532435264512642, -76.14435526899964657, 7.538916498839152602 ) ) ;
#24206 = CARTESIAN_POINT ( 'NONE',  ( 0.4917238316050000502, -82.23466316459999348, -1.258641686703000140 ) ) ;
#24207 = CARTESIAN_POINT ( 'NONE',  ( -3.210317642310111186, -85.88547957940599531, 1.357411296278074442 ) ) ;
#24208 = ORIENTED_EDGE ( 'NONE', *, *, #50223, .F. ) ;
#24209 = CARTESIAN_POINT ( 'NONE',  ( 12.70451647735429823, -24.55458569105848454, 1.498866843994218545 ) ) ;
#24210 = CARTESIAN_POINT ( 'NONE',  ( 11.63677945028385174, -79.08342241646654713, -2.480315150004160696 ) ) ;
#24211 = DIRECTION ( 'NONE',  ( 1.000000000000000000, 0.000000000000000000, 0.000000000000000000 ) ) ;
#24212 = CARTESIAN_POINT ( 'NONE',  ( 4.634563706678000550, -78.83076359945098943, 9.949112313689999709 ) ) ;
#24213 = CARTESIAN_POINT ( 'NONE',  ( -10.96337388901621424, -80.09393029936845210, 0.8942561643144778527 ) ) ;
#24214 = CARTESIAN_POINT ( 'NONE',  ( 5.718781654312999230, -79.25521639797898388, -7.660718028547000458 ) ) ;
#24215 = CARTESIAN_POINT ( 'NONE',  ( 10.35398565887000011, -18.59211376270000216, -7.619387877927000119 ) ) ;
#24216 = DIRECTION ( 'NONE',  ( 0.000000000000000000, 1.000000000000000000, 0.000000000000000000 ) ) ;
#24217 = B_SPLINE_CURVE_WITH_KNOTS ( 'NONE', 3,
 ( #43168, #29273, #43745, #52598, #16872, #24569 ),
 .UNSPECIFIED., .F., .F.,
 ( 4, 1, 1, 4 ),
 ( 0.000000000000000000, 0.3333333333333000081, 0.6666666666667000474, 1.000000000000000000 ),
 .UNSPECIFIED. ) ;
#24218 = EDGE_LOOP ( 'NONE', ( #47719, #15015, #13461 ) ) ;
#24219 = ADVANCED_FACE ( 'NONE', ( #32464 ), #39259, .T. ) ;
#24220 = CARTESIAN_POINT ( 'NONE',  ( 5.380879925577582767, -76.18494410599546995, 9.804299052675480297 ) ) ;
#24221 = DIRECTION ( 'NONE',  ( 3.552713678800000476E-14, 1.000000000000000000, -1.480997164338000095E-13 ) ) ;
#24222 = CARTESIAN_POINT ( 'NONE',  ( -1.500410155940665735, -81.91674653272079354, -0.3141412879893631382 ) ) ;
#24223 = CARTESIAN_POINT ( 'NONE',  ( 2.690846299717935874, -77.31017771206632005, 11.76998691515812112 ) ) ;
#24225 = CARTESIAN_POINT ( 'NONE',  ( 0.4658870802631708830, -81.44483258142587090, 1.159784591535937937 ) ) ;
#24224 = CARTESIAN_POINT ( 'NONE',  ( 0.1494146964801000010, -81.52402579967099427, 1.310816866976999950 ) ) ;
#24226 = CARTESIAN_POINT ( 'NONE',  ( 1.270896956543958733, -78.90621706637968202, 0.09642097433307661447 ) ) ;
#24227 = CARTESIAN_POINT ( 'NONE',  ( -5.329221945977861807, -76.99999999999998579, -7.828459959116974787 ) ) ;
#24228 = CARTESIAN_POINT ( 'NONE',  ( -0.6934022908089999548, -3.137579146514999806, 3.742362521638999961 ) ) ;
#24229 = CIRCLE ( 'NONE', #56306, 1.750000000000000666 ) ;
#24230 = CARTESIAN_POINT ( 'NONE',  ( -1.175921224601000015, -78.54395921125998825, 0.5727056776607999389 ) ) ;
#24231 = CARTESIAN_POINT ( 'NONE',  ( 1.405334850311761752, -17.68507052220335751, -12.50716844834626684 ) ) ;
#24232 = AXIS2_PLACEMENT_3D ( 'NONE', #56395, #15068, #33063 ) ;
#24233 = CARTESIAN_POINT ( 'NONE',  ( -9.091682561854286249, -78.90278042018009330, 6.148912672809537128 ) ) ;
#24234 = CARTESIAN_POINT ( 'NONE',  ( 0.000000000000000000, -75.00000000000001421, 0.000000000000000000 ) ) ;
#24235 = ORIENTED_EDGE ( 'NONE', *, *, #34552, .F. ) ;
#24236 = AXIS2_PLACEMENT_3D ( 'NONE', #35374, #53399, #26820 ) ;
#24237 = ORIENTED_EDGE ( 'NONE', *, *, #35004, .T. ) ;
#24238 = CARTESIAN_POINT ( 'NONE',  ( 4.448768332841000372, -78.71773998579799070, 8.980869306721999124 ) ) ;
#24239 = CARTESIAN_POINT ( 'NONE',  ( 6.955482170287579535, -78.78106476872730468, -8.196585751274280796 ) ) ;
#24240 = ADVANCED_FACE ( 'NONE', ( #45500 ), #25108, .T. ) ;
#24241 = CIRCLE ( 'NONE', #45967, 13.86363636363999952 ) ;
#24242 = VERTEX_POINT ( 'NONE', #646 ) ;
#24243 = CARTESIAN_POINT ( 'NONE',  ( 8.194873807830999723, -17.28956116771000140, 9.389185139535999980 ) ) ;
#24244 = CARTESIAN_POINT ( 'NONE',  ( -9.035542397009781013, -79.37473505568793541, 2.933552591326429315 ) ) ;
#24245 = CARTESIAN_POINT ( 'NONE',  ( 6.578523888628000194, -78.66055396357999996, 10.10992338718000028 ) ) ;
#24246 = CARTESIAN_POINT ( 'NONE',  ( 10.15323304115999825, -61.03079615981999950, 7.760925857031000241 ) ) ;
#24247 = CARTESIAN_POINT ( 'NONE',  ( 1.218445119259581544, -82.37149458593418672, 0.3277830641851678384 ) ) ;
#24248 = CARTESIAN_POINT ( 'NONE',  ( -11.92783303768075776, -77.55733137067235816, -1.116597677413008194 ) ) ;
#24249 = CARTESIAN_POINT ( 'NONE',  ( -7.408849624938999234, -79.40147933624500354, -8.421820339245000397 ) ) ;
#24250 = ADVANCED_FACE ( 'NONE', ( #36623, #18337 ), #54061, .F. ) ;
#24251 = EDGE_LOOP ( 'NONE', ( #36779, #341, #50913, #51665 ) ) ;
#24252 = CARTESIAN_POINT ( 'NONE',  ( 7.630100270854876854, -78.11902925543334675, 8.993494391708773961 ) ) ;
#24253 = ORIENTED_EDGE ( 'NONE', *, *, #24776, .T. ) ;
#24254 = CARTESIAN_POINT ( 'NONE',  ( 7.625531225268916913, -77.39806426064797051, 5.241218712637033761 ) ) ;
#24255 = CARTESIAN_POINT ( 'NONE',  ( -3.513492303797125071, -78.44955557553232950, -10.65255456408984180 ) ) ;
#24256 = UNCERTAINTY_MEASURE_WITH_UNIT (LENGTH_MEASURE( 1.000000000000000082E-05 ), #52057, 'distance_accuracy_value', 'NONE');
#24257 = DIRECTION ( 'NONE',  ( 0.000000000000000000, 1.000000000000000000, 0.000000000000000000 ) ) ;
#24258 = CARTESIAN_POINT ( 'NONE',  ( -12.80000000000000071, -6.000000000000000000, 0.000000000000000000 ) ) ;
#24259 = CARTESIAN_POINT ( 'NONE',  ( 10.48543666025110355, -78.60833333333330586, -6.043427764450775008 ) ) ;
#24260 = CARTESIAN_POINT ( 'NONE',  ( 1.328072050606999843, -78.53056612723000285, -0.9406846882429998891 ) ) ;
#24261 = CARTESIAN_POINT ( 'NONE',  ( -1.003367537693320877, -79.15123299649694388, -0.7504123186897171394 ) ) ;
#24262 = CARTESIAN_POINT ( 'NONE',  ( 3.325053339351000226, -79.14238723821299004, -10.53669369097999997 ) ) ;
#24263 = CARTESIAN_POINT ( 'NONE',  ( 12.70451681032941238, -61.97641660161944799, 0.5206746372120837352 ) ) ;
#24264 = CARTESIAN_POINT ( 'NONE',  ( 12.82904109066000053, -60.12452273675999947, -2.062673488410000200 ) ) ;
#24265 = CARTESIAN_POINT ( 'NONE',  ( -1.473390922089000021, -82.94607228207600258, 3.227022943217999984 ) ) ;
#24266 = ORIENTED_EDGE ( 'NONE', *, *, #16512, .T. ) ;
#24267 = CARTESIAN_POINT ( 'NONE',  ( 9.596002108778174389, -79.59791666666666288, -7.374560639698961140 ) ) ;
#24268 = CARTESIAN_POINT ( 'NONE',  ( -5.918356417140000048, -76.19414720733000479, 9.991160380212999570 ) ) ;
#24269 = CARTESIAN_POINT ( 'NONE',  ( 10.74991461791089264, -77.85495667263820962, 0.6503649595168488062 ) ) ;
#24270 = CARTESIAN_POINT ( 'NONE',  ( -10.61596739836999959, -78.60444753118198946, -5.551333230057999835 ) ) ;
#24271 = CARTESIAN_POINT ( 'NONE',  ( -8.220399303327999618, -17.18050618273999675, 9.523318109998999859 ) ) ;
#24272 = AXIS2_PLACEMENT_3D ( 'NONE', #14225, #54400, #979 ) ;
#24273 = CARTESIAN_POINT ( 'NONE',  ( 9.662273249694312227, -78.88660371430214013, 4.763867255732987971 ) ) ;
#24274 = CARTESIAN_POINT ( 'NONE',  ( 3.405878126756061608, -3.020524467000565760, 0.8975563214481486751 ) ) ;
#24275 = CARTESIAN_POINT ( 'NONE',  ( -3.039602602086000083, -79.28985584965398914, -9.236151215514999180 ) ) ;
#24276 = CARTESIAN_POINT ( 'NONE',  ( 6.774287055642999711, -78.26811043579999705, -6.536071403775000732 ) ) ;
#24277 = CARTESIAN_POINT ( 'NONE',  ( -3.654181830570442990, -86.09999999999999432, 1.626946572303610283 ) ) ;
#24278 = CARTESIAN_POINT ( 'NONE',  ( 8.145694891731999121, -78.14996571856799790, -7.439717004853000581 ) ) ;
#24279 = CARTESIAN_POINT ( 'NONE',  ( -7.624341766629000539, -55.53514853726999689, 10.42531125022999916 ) ) ;
#24280 = CARTESIAN_POINT ( 'NONE',  ( -10.89192327684000006, -80.52192009945389373, 0.6399950417793000002 ) ) ;
#24281 = ORIENTED_EDGE ( 'NONE', *, *, #125, .F. ) ;
#24282 = CARTESIAN_POINT ( 'NONE',  ( -0.7068627984950999199, -81.18511568401699208, 1.130893941374999878 ) ) ;
#24283 = CARTESIAN_POINT ( 'NONE',  ( -1.691611010926999947, -61.03082691197000287, -12.66722148972999840 ) ) ;
#24284 = AXIS2_PLACEMENT_3D ( 'NONE', #22773, #26597, #41077 ) ;
#24285 = CARTESIAN_POINT ( 'NONE',  ( -10.74953850517756848, -80.58960968215087917, 1.406898149230603412 ) ) ;
#24286 = CARTESIAN_POINT ( 'NONE',  ( -10.96060824219999930, -77.24906299167599855, 2.383941600041999731 ) ) ;
#24287 = CARTESIAN_POINT ( 'NONE',  ( -9.438868967565998247, -79.35216368075597870, -5.601050722391000214 ) ) ;
#24288 = AXIS2_PLACEMENT_3D ( 'NONE', #40899, #44444, #22598 ) ;
#24289 = CARTESIAN_POINT ( 'NONE',  ( 8.292771711448001071, -25.05529938523999789, -9.770424367364000773 ) ) ;
#24290 = CARTESIAN_POINT ( 'NONE',  ( 3.056131291857314469, -85.61822918110996739, 2.599642428790069015 ) ) ;
#24291 = CARTESIAN_POINT ( 'NONE',  ( -7.601397897754999633, -18.75000000240999753, -10.07627163191000008 ) ) ;
#24292 = FACE_OUTER_BOUND ( 'NONE', #8995, .T. ) ;
#24293 = ORIENTED_EDGE ( 'NONE', *, *, #2858, .F. ) ;
#24294 = EDGE_CURVE ( 'NONE', #10086, #31168, #54354, .T. ) ;
#24295 = CARTESIAN_POINT ( 'NONE',  ( -0.5890800888495719700, -80.01449628974698669, 1.102351224369839677 ) ) ;
#24296 = AXIS2_PLACEMENT_3D ( 'NONE', #15281, #2303, #5837 ) ;
#24297 = CARTESIAN_POINT ( 'NONE',  ( 0.1963495408493638184, -79.63541666666667140, -1.499999999999999778 ) ) ;
#24298 = EDGE_CURVE ( 'NONE', #47767, #21227, #28031, .T. ) ;
#24299 = CARTESIAN_POINT ( 'NONE',  ( 8.252512830309999714, -53.86594982524999864, -9.650910120403001002 ) ) ;
#24300 = CARTESIAN_POINT ( 'NONE',  ( -8.763613300111000370, -76.72389978589799853, 6.838397221053000408 ) ) ;
#24301 = CARTESIAN_POINT ( 'NONE',  ( -0.5298108134926000634, -80.73036354008999638, 1.579417458585999912 ) ) ;
#24302 = CARTESIAN_POINT ( 'NONE',  ( 1.170683199339999758, -78.65761630967999452, -0.8292048310924000631 ) ) ;
#24303 = CARTESIAN_POINT ( 'NONE',  ( -9.596002108778193929, -77.74791666666664014, 7.374560639698935383 ) ) ;
#24304 = CARTESIAN_POINT ( 'NONE',  ( -0.9345908190077275579, -82.17710307665237224, 1.232018202299275611 ) ) ;
#24305 = CARTESIAN_POINT ( 'NONE',  ( 12.76303204294000082, -18.73514849292999784, 1.980584515756000030 ) ) ;
#24306 = ORIENTED_EDGE ( 'NONE', *, *, #11738, .T. ) ;
#24307 = DIRECTION ( 'NONE',  ( 0.000000000000000000, -1.000000000000000000, 0.000000000000000000 ) ) ;
#24308 = CARTESIAN_POINT ( 'NONE',  ( 6.091423516370726666E-05, -80.97567851488123836, 1.280875928844625644 ) ) ;
#24309 = ORIENTED_EDGE ( 'NONE', *, *, #40301, .F. ) ;
#24310 = CARTESIAN_POINT ( 'NONE',  ( 0.03373185335276917413, -81.72769218985609996, -1.249292863317937652 ) ) ;
#24311 =( NAMED_UNIT ( * ) PLANE_ANGLE_UNIT ( ) SI_UNIT ( $, .RADIAN. ) );
#24312 = CARTESIAN_POINT ( 'NONE',  ( -6.285096537930999538, -78.96846735336799838, -9.206093747065001054 ) ) ;
#24313 = CARTESIAN_POINT ( 'NONE',  ( 10.75000000000000000, -80.25000000000000000, -1.651583051307000043E-14 ) ) ;
#24314 = ORIENTED_EDGE ( 'NONE', *, *, #21547, .F. ) ;
#24315 = VERTEX_POINT ( 'NONE', #36037 ) ;
#24316 = CARTESIAN_POINT ( 'NONE',  ( -0.1350024095750999853, -81.16521930730999657, -1.510204125836999811 ) ) ;
#24317 = EDGE_CURVE ( 'NONE', #56551, #41164, #35021, .T. ) ;
#24318 = VERTEX_POINT ( 'NONE', #11852 ) ;
#24319 = ORIENTED_EDGE ( 'NONE', *, *, #51038, .F. ) ;
#24320 = CARTESIAN_POINT ( 'NONE',  ( -1.460729357738999923, -17.90908756797999857, 12.44211643240000065 ) ) ;
#24321 = DIRECTION ( 'NONE',  ( 0.000000000000000000, -1.000000000000000000, 0.000000000000000000 ) ) ;
#24322 =( NAMED_UNIT ( * ) SI_UNIT ( $, .STERADIAN. ) SOLID_ANGLE_UNIT ( ) );
#24323 = B_SPLINE_SURFACE_WITH_KNOTS ( 'NONE', 3, 3, ( 
 ( #45473, #51072, #37462, #40740 ),
 ( #23315, #28016, #46063, #32152 ),
 ( #27726, #15030, #18311, #28304 ),
 ( #23598, #41610, #1191, #37176 ),
 ( #36594, #5879, #1479, #33026 ),
 ( #19469, #5015, #13868, #31862 ),
 ( #9451, #23019, #41031, #54616 ),
 ( #14154, #9738, #38914, #42202 ),
 ( #51657, #20342, #2347, #24770 ),
 ( #51939, #42493, #38630, #56932 ),
 ( #29750, #56360, #10915, #56648 ),
 ( #2062, #43075, #6467, #28895 ),
 ( #16205, #38337, #25052, #47805 ),
 ( #19764, #34182, #16492, #47524 ),
 ( #6760, #52219, #34471, #10620 ),
 ( #15911, #2633, #28601, #46648 ),
 ( #20911, #20629, #7336, #15619 ) ),
 .UNSPECIFIED., .F., .F., .F.,
 ( 4, 1, 1, 1, 1, 1, 1, 1, 1, 1, 1, 1, 1, 1, 4 ),
 ( 4, 4 ),
 ( -0.01011786823686000071, 0.000000000000000000, 0.08333333333333001192, 0.1666666666667000196, 0.2500000000000000000, 0.3333333333333000081, 0.4166666666666999919, 0.5000000000000000000, 0.5833333333333000637, 0.6666666666667000474, 0.7500000000000000000, 0.8333333333333000637, 0.9166666666667000474, 1.000000000000000000, 1.010371592463000123 ),
 ( -0.3559705548529999986, 1.357613344763000107 ),
 .UNSPECIFIED. ) ;
#24324 = CARTESIAN_POINT ( 'NONE',  ( 10.02101539056000057, -79.07196001420199138, 0.1637206938138999757 ) ) ;
#24325 = CARTESIAN_POINT ( 'NONE',  ( 7.369188213045021918, -78.29848014924698418, -5.592313299527890358 ) ) ;
#24326 = CARTESIAN_POINT ( 'NONE',  ( 8.822637088635000069, -80.00128349074179823, 6.926713255916000733 ) ) ;
#24327 = CIRCLE ( 'NONE', #45063, 8.500000000000000000 ) ;
#24328 = EDGE_CURVE ( 'NONE', #26684, #41458, #4845, .T. ) ;
#24329 = ORIENTED_EDGE ( 'NONE', *, *, #48364, .T. ) ;
#24330 = VERTEX_POINT ( 'NONE', #39279 ) ;
#24331 = CARTESIAN_POINT ( 'NONE',  ( 0.000000000000000000, -75.15999999999999659, 0.000000000000000000 ) ) ;
#24332 = DIRECTION ( 'NONE',  ( 0.7071067811865474617, 0.000000000000000000, 0.7071067811865474617 ) ) ;
#24333 = CARTESIAN_POINT ( 'NONE',  ( 1.250000000000000000, -81.24999999999998579, 0.000000000000000000 ) ) ;
#24334 = EDGE_CURVE ( 'NONE', #45569, #40274, #58102, .T. ) ;
#24335 = DIRECTION ( 'NONE',  ( -0.3090169943748909409, 0.000000000000000000, -0.9510565162951718499 ) ) ;
#24336 = CARTESIAN_POINT ( 'NONE',  ( 1.583004792652944692, -61.25209241118513859, -12.70616254415345558 ) ) ;
#24337 = CARTESIAN_POINT ( 'NONE',  ( 8.240135455977000589, -77.97556748894699297, -5.125512367919999868 ) ) ;
#24338 = VECTOR ( 'NONE', #31635, 1000.000000000000000 ) ;
#24339 = CARTESIAN_POINT ( 'NONE',  ( -1.165746613897999928E-14, -72.79999999999999716, 0.000000000000000000 ) ) ;
#24340 = CARTESIAN_POINT ( 'NONE',  ( -10.01235002622999914, -18.70151115557999688, 7.653559626094000201 ) ) ;
#24341 = DIRECTION ( 'NONE',  ( -1.000000000000000000, 0.000000000000000000, 0.000000000000000000 ) ) ;
#24342 = CARTESIAN_POINT ( 'NONE',  ( 0.7712594847575999779, -80.60757119619998434, 1.518214662813999860 ) ) ;
#24343 = CARTESIAN_POINT ( 'NONE',  ( 0.000000000000000000, 4.040000000000000036, 0.000000000000000000 ) ) ;
#24344 = CARTESIAN_POINT ( 'NONE',  ( 4.597354753046301035, -79.22265623326045159, -11.09475667319383341 ) ) ;
#24345 = CARTESIAN_POINT ( 'NONE',  ( -10.13402152808999901, -55.07694524364999467, 7.647754144006999155 ) ) ;
#24346 = CARTESIAN_POINT ( 'NONE',  ( -8.838907858698000553, -78.60421001420199616, -3.964206742940000083 ) ) ;
#24347 = CARTESIAN_POINT ( 'NONE',  ( -6.043427764450833628, -77.31666666666666288, 10.48543666025107335 ) ) ;
#24348 = CARTESIAN_POINT ( 'NONE',  ( 1.931086388578000079, -23.29778754190000001, -12.71798269385000069 ) ) ;
#24350 = CARTESIAN_POINT ( 'NONE',  ( -0.7022187824378000043, -82.19906693409399168, -1.095132696781000003 ) ) ;
#24349 = CYLINDRICAL_SURFACE ( 'NONE', #30615, 12.50000000000000000 ) ;
#24351 = ADVANCED_FACE ( 'NONE', ( #33973 ), #45088, .F. ) ;
#24352 = CARTESIAN_POINT ( 'NONE',  ( -7.397034735012056217, -79.54824835870380184, 5.685233668030444498 ) ) ;
#24353 = DIRECTION ( 'NONE',  ( 0.9957542217959282072, -0.04890179607409141094, 0.07798810240231221491 ) ) ;
#24354 = CARTESIAN_POINT ( 'NONE',  ( -7.835303970625000503, -78.25963867675800145, 8.089621514298000804 ) ) ;
#24355 = CARTESIAN_POINT ( 'NONE',  ( -3.453171399369999950, -1.763032031398999999, -0.5706200895263999762 ) ) ;
#24356 = ORIENTED_EDGE ( 'NONE', *, *, #8253, .F. ) ;
#24357 = CARTESIAN_POINT ( 'NONE',  ( -11.00000000000000000, -78.19999999999998863, 0.000000000000000000 ) ) ;
#24358 = CARTESIAN_POINT ( 'NONE',  ( -0.7705914100935935540, -77.57837515258907501, 11.74754681604737883 ) ) ;
#24359 = CARTESIAN_POINT ( 'NONE',  ( 0.7088972746458148677, -78.42728435963773848, 1.029425822873615282 ) ) ;
#24360 = CARTESIAN_POINT ( 'NONE',  ( -1.461485599008999881, -79.56969053780299816, -9.420958682499000147 ) ) ;
#24361 = CARTESIAN_POINT ( 'NONE',  ( -12.77649734579999929, -53.49171487479999598, -0.06478328530389998452 ) ) ;
#24362 = CARTESIAN_POINT ( 'NONE',  ( 9.499157866768639380, -79.10080562451891240, 0.1004279358040388037 ) ) ;
#24363 = CARTESIAN_POINT ( 'NONE',  ( -0.2916556773643344536, -79.47731085430962139, 10.74608969385784185 ) ) ;
#24364 = CIRCLE ( 'NONE', #10242, 11.00000000000000000 ) ;
#24365 = CARTESIAN_POINT ( 'NONE',  ( 8.400841032887999660, -79.59013998579800386, -4.509023106980999174 ) ) ;
#24366 = ADVANCED_FACE ( 'NONE', ( #47599 ), #18508, .F. ) ;
#24367 = CARTESIAN_POINT ( 'NONE',  ( -13.49939038839240979, -46.09579702914000165, -0.1282931867975413143 ) ) ;
#24368 = CARTESIAN_POINT ( 'NONE',  ( 9.328312098178999534, -77.44676313692498582, -6.135780202701999642 ) ) ;
#24369 = CARTESIAN_POINT ( 'NONE',  ( 0.08881464945738999639, -81.77864929594699106, 1.601641772328999958 ) ) ;
#24370 = CARTESIAN_POINT ( 'NONE',  ( -0.5312504855272001114, -78.77064514476064971, -9.708839960653000034 ) ) ;
#24371 = CARTESIAN_POINT ( 'NONE',  ( 6.774287055642999711, -78.70973765814899537, -6.536071403775000732 ) ) ;
#24373 = CARTESIAN_POINT ( 'NONE',  ( -0.1204595238885999980, -0.7297393593719998517, 3.497926457646999943 ) ) ;
#24372 = CARTESIAN_POINT ( 'NONE',  ( 3.635560235662999684, -83.58453969748799750, -0.9455538594405999975 ) ) ;
#24374 = CARTESIAN_POINT ( 'NONE',  ( 9.539544502573999551, -79.44465584965399785, 0.5400218831817999998 ) ) ;
#24375 = CARTESIAN_POINT ( 'NONE',  ( 1.092232985442823212, -82.70833333333331439, -0.6295237254636224522 ) ) ;
#24376 = CARTESIAN_POINT ( 'NONE',  ( 0.1963495408493571015, -81.36458333333332860, 1.500000000000000444 ) ) ;
#24377 = CARTESIAN_POINT ( 'NONE',  ( -7.514905133372472790, -77.16340258555835874, -7.687053346723279112 ) ) ;
#24378 = CARTESIAN_POINT ( 'NONE',  ( -1.243547092045993674, -77.28541666666666288, 9.499999999999996447 ) ) ;
#24379 = AXIS2_PLACEMENT_3D ( 'NONE', #23665, #31927, #4796 ) ;
#24380 = ORIENTED_EDGE ( 'NONE', *, *, #151, .F. ) ;
#24381 = EDGE_LOOP ( 'NONE', ( #39408, #37781 ) ) ;
#24382 = CARTESIAN_POINT ( 'NONE',  ( -11.95950202284999975, -79.12530980127799296, 1.295167635372999948 ) ) ;
#24383 = CARTESIAN_POINT ( 'NONE',  ( -12.50483465198260014, -61.66452578640176796, -0.6958747608064493884 ) ) ;
#24384 = LINE ( 'NONE', #42683, #37887 ) ;
#24385 = VERTEX_POINT ( 'NONE', #38992 ) ;
#24386 = CARTESIAN_POINT ( 'NONE',  ( 7.822091542723999424, -77.30528544001199975, -9.013910121987001034 ) ) ;
#24387 = ORIENTED_EDGE ( 'NONE', *, *, #17715, .T. ) ;
#24388 = VERTEX_POINT ( 'NONE', #15983 ) ;
#24389 = CARTESIAN_POINT ( 'NONE',  ( -2.813789756862300262, -78.89583333333334281, 10.47020627418438465 ) ) ;
#24390 = ORIENTED_EDGE ( 'NONE', *, *, #3254, .F. ) ;
#24391 = CARTESIAN_POINT ( 'NONE',  ( 2.970835140755999859, -79.57543510685839294, 1.937965009331999999 ) ) ;
#24392 = CARTESIAN_POINT ( 'NONE',  ( 6.312739868268272936, -79.21696743740758961, 7.099225441629251065 ) ) ;
#24393 = ORIENTED_EDGE ( 'NONE', *, *, #24763, .F. ) ;
#24394 = CARTESIAN_POINT ( 'NONE',  ( -0.1639670297146121059, -82.71513557757415924, -1.249649658132720331 ) ) ;
#24395 = EDGE_LOOP ( 'NONE', ( #18588, #13531, #35595, #24676, #49674, #21467, #32706, #11758, #14989, #22712, #49478, #33600 ) ) ;
#24396 = CARTESIAN_POINT ( 'NONE',  ( -0.2685658639872000042, -2.674331454374000216, -3.390759574055000058 ) ) ;
#24397 = EDGE_LOOP ( 'NONE', ( #11655, #30502, #49065, #6222 ) ) ;
#24398 = CARTESIAN_POINT ( 'NONE',  ( -8.596418555780431348, -80.55208333333331439, -6.606377239730338857 ) ) ;
#24399 = CARTESIAN_POINT ( 'NONE',  ( -1.185909154492194695, -79.19522916700250903, 0.9691166662416358379 ) ) ;
#24400 = CARTESIAN_POINT ( 'NONE',  ( -7.384493003614710283, -79.80000000000001137, -9.307078043242871246 ) ) ;
#24401 = CARTESIAN_POINT ( 'NONE',  ( -7.919595949288999570, -55.64999999965999677, 8.768124086712999699 ) ) ;
#24402 = FACE_OUTER_BOUND ( 'NONE', #9642, .T. ) ;
#24403 = CIRCLE ( 'NONE', #7460, 0.8000000000000011546 ) ;
#24404 = CARTESIAN_POINT ( 'NONE',  ( -1.565122400816999937, -78.63789132619378108, 9.577113408380000692 ) ) ;
#24405 = CARTESIAN_POINT ( 'NONE',  ( 1.546553306619000256, -76.40214563794199876, -11.07619323537999989 ) ) ;
#24406 = CARTESIAN_POINT ( 'NONE',  ( 10.82209551222215715, -76.35773650856198458, 0.9128778866761866340 ) ) ;
#24407 = LINE ( 'NONE', #10031, #3329 ) ;
#24408 = CARTESIAN_POINT ( 'NONE',  ( 5.198613046211999489, -76.66010485387299411, 9.952796194076000802 ) ) ;
#24409 = CARTESIAN_POINT ( 'NONE',  ( -6.537703431114865182, -78.66257577246084054, -6.543724569677213054 ) ) ;
#24410 = CARTESIAN_POINT ( 'NONE',  ( 6.020971146719677591, -76.53215365127321945, 10.09761672016582246 ) ) ;
#24411 = CARTESIAN_POINT ( 'NONE',  ( 0.6343572851480000496, -80.51366523522099783, 1.173101423079000005 ) ) ;
#24412 = CARTESIAN_POINT ( 'NONE',  ( -5.423101880016904630, -80.18407044839175057, -9.570620509585031854 ) ) ;
#24413 = CARTESIAN_POINT ( 'NONE',  ( -12.56594317819999951, -55.54999998572999687, -1.750000000000000000 ) ) ;
#24414 = CARTESIAN_POINT ( 'NONE',  ( 1.764731964946999909, -79.40353455456848053, 3.316185037183999818 ) ) ;
#24415 = CARTESIAN_POINT ( 'NONE',  ( 11.96908924566999843, -79.33756653719200358, 1.661418422374000059 ) ) ;
#24416 = CARTESIAN_POINT ( 'NONE',  ( -8.939668861401381506, -78.05329775042086737, 5.970159216130292101 ) ) ;
#24417 = VECTOR ( 'NONE', #29041, 1000.000000000000114 ) ;
#24418 = ADVANCED_FACE ( 'NONE', ( #16564 ), #7211, .F. ) ;
#24419 = CARTESIAN_POINT ( 'NONE',  ( 0.8703341916068573214, -82.91432341927395555, 0.8966700837326383455 ) ) ;
#24420 = CARTESIAN_POINT ( 'NONE',  ( 0.000000000000000000, -78.00000000000000000, 0.000000000000000000 ) ) ;
#24421 = CARTESIAN_POINT ( 'NONE',  ( -8.505985592041961141, -76.26002876382779050, -8.106429104623925852 ) ) ;
#24422 = CARTESIAN_POINT ( 'NONE',  ( 10.55910102244999926, -19.21514526754999963, 7.642147947538999730 ) ) ;
#24423 = DIRECTION ( 'NONE',  ( 0.000000000000000000, -1.000000000000000000, 0.000000000000000000 ) ) ;
#24424 = CARTESIAN_POINT ( 'NONE',  ( -9.250000000000000000, -79.59999999999999432, 0.000000000000000000 ) ) ;
#24425 = CARTESIAN_POINT ( 'NONE',  ( 0.000000000000000000, -81.10000000285099020, -7.000000000000000000 ) ) ;
#24426 = CARTESIAN_POINT ( 'NONE',  ( 0.000000000000000000, -87.25000000009099210, 0.000000000000000000 ) ) ;
#24427 = CARTESIAN_POINT ( 'NONE',  ( 12.66232158686000098, -25.13482640580999927, 0.5080765942054999984 ) ) ;
#24428 = CARTESIAN_POINT ( 'NONE',  ( 10.07284277676071227, -77.73062272438683351, 4.003573653696650858 ) ) ;
#24429 = CYLINDRICAL_SURFACE ( 'NONE', #55232, 1.750000000000000000 ) ;
#24430 = CARTESIAN_POINT ( 'NONE',  ( 3.176617583302000725, -79.70163351862059642, 10.50586082162000068 ) ) ;
#24431 = CARTESIAN_POINT ( 'NONE',  ( -8.677390326068000093, -76.10643013234999898, 8.592813855578000926 ) ) ;
#24432 = ORIENTED_EDGE ( 'NONE', *, *, #17808, .T. ) ;
#24433 = EDGE_CURVE ( 'NONE', #46988, #46084, #3559, .T. ) ;
#24434 = CARTESIAN_POINT ( 'NONE',  ( 0.1848134996591999923, -86.11796544543098264, 3.751952874225000123 ) ) ;
#24435 = CARTESIAN_POINT ( 'NONE',  ( -11.15592782356999990, -80.22109534903739814, -1.728406004469000168 ) ) ;
#24436 = PRODUCT_DEFINITION_FORMATION_WITH_SPECIFIED_SOURCE ( 'ANY', '', #30452, .NOT_KNOWN. ) ;
#24437 = CARTESIAN_POINT ( 'NONE',  ( 7.497431372734266297, -78.30036608647220930, -5.417634822929890959 ) ) ;
#24438 = CARTESIAN_POINT ( 'NONE',  ( 7.861037107661897672, -54.33338873118993462, 10.10708465680652957 ) ) ;
#24439 = CARTESIAN_POINT ( 'NONE',  ( 11.19180402071999936, -77.65700352824698882, 0.7494220128532999015 ) ) ;
#24440 = CARTESIAN_POINT ( 'NONE',  ( -1.799502287743000029, -18.69283065396999888, -12.60413652832999887 ) ) ;
#24441 = CARTESIAN_POINT ( 'NONE',  ( 7.433005562543999467, -77.52327641628599508, -6.293657445383999516 ) ) ;
#24442 = CARTESIAN_POINT ( 'NONE',  ( -0.6572886123566999972, -82.79609954400000049, 1.530761476772000140 ) ) ;
#24443 = CARTESIAN_POINT ( 'NONE',  ( 7.588757936995927963E-07, -80.21583927563050054, -10.98470495943546688 ) ) ;
#24444 = DIRECTION ( 'NONE',  ( 0.000000000000000000, -1.000000000000000000, 0.000000000000000000 ) ) ;
#24445 = ORIENTED_EDGE ( 'NONE', *, *, #17110, .F. ) ;
#24446 = DIRECTION ( 'NONE',  ( 1.000000000000000000, 0.000000000000000000, 0.000000000000000000 ) ) ;
#24447 = CARTESIAN_POINT ( 'NONE',  ( 2.432155020134764811, -78.96932498430172132, -2.971370035328440462 ) ) ;
#24448 = EDGE_CURVE ( 'NONE', #44346, #35538, #32941, .T. ) ;
#24449 = ORIENTED_EDGE ( 'NONE', *, *, #30681, .T. ) ;
#24450 = CARTESIAN_POINT ( 'NONE',  ( -1.309352690804000074, -78.14954698566639024, -0.2533212985548999874 ) ) ;
#24451 = CARTESIAN_POINT ( 'NONE',  ( -7.299994274544086892, -77.55341536691996396, -5.806806862848980622 ) ) ;
#24452 = CARTESIAN_POINT ( 'NONE',  ( -10.77729720431999993, -80.20851364748298806, -4.161934381267000660 ) ) ;
#24453 = EDGE_LOOP ( 'NONE', ( #30349, #34743, #651 ) ) ;
#24454 = CARTESIAN_POINT ( 'NONE',  ( 10.33787006668000075, -78.55304150121298790, 6.411783922571999916 ) ) ;
#24455 = CARTESIAN_POINT ( 'NONE',  ( 0.5827356580765999938, -77.42784033438199742, 11.30719494610999831 ) ) ;
#24456 = CARTESIAN_POINT ( 'NONE',  ( 12.50000000000000000, -60.04999999657000131, 1.750000000000000000 ) ) ;
#24457 = AXIS2_PLACEMENT_3D ( 'NONE', #52396, #51825, #30221 ) ;
#24458 = ORIENTED_EDGE ( 'NONE', *, *, #43359, .F. ) ;
#24459 = ORIENTED_EDGE ( 'NONE', *, *, #24317, .T. ) ;
#24460 = CONICAL_SURFACE ( 'NONE', #37639, 3.425000000527000044, 0.7853981633972997312 ) ;
#24461 = CARTESIAN_POINT ( 'NONE',  ( -0.6016272266181392769, -80.51522408813923448, 1.095825561504355061 ) ) ;
#24462 = CARTESIAN_POINT ( 'NONE',  ( 8.596684946446202957, -77.79795771992381503, -6.606655141920929175 ) ) ;
#24463 = CARTESIAN_POINT ( 'NONE',  ( -7.545891804452000251, -80.19526951059052067, 6.201630566990999682 ) ) ;
#24464 = ORIENTED_EDGE ( 'NONE', *, *, #5184, .F. ) ;
#24465 = CARTESIAN_POINT ( 'NONE',  ( -0.4257295889298650660, -2.486564122683458944, 3.250694461378448974 ) ) ;
#24466 = CARTESIAN_POINT ( 'NONE',  ( 10.21235917355000034, -79.79466669503099752, -3.857859667932999947 ) ) ;
#24467 = VERTEX_POINT ( 'NONE', #45183 ) ;
#24468 = CARTESIAN_POINT ( 'NONE',  ( -12.65987830573000039, -24.93692962305999927, -0.9847759095506000149 ) ) ;
#24469 = CARTESIAN_POINT ( 'NONE',  ( 3.399999999999725464, -78.69999999999998863, -1.260385025514398905E-15 ) ) ;
#24470 = CARTESIAN_POINT ( 'NONE',  ( 3.912590402935000267, -82.39999999999999147, -0.8316467632710000668 ) ) ;
#24471 = CARTESIAN_POINT ( 'NONE',  ( -7.648026768008000076, -55.55000001556999933, 10.12290050216000026 ) ) ;
#24472 = CARTESIAN_POINT ( 'NONE',  ( -3.992904449609000483, -78.62148118275521824, -1.315241435988999952E-08 ) ) ;
#24473 = CARTESIAN_POINT ( 'NONE',  ( 9.279687143926999227, -76.88845924204508719, 2.683876840368999872 ) ) ;
#24474 = CARTESIAN_POINT ( 'NONE',  ( -0.5583711603394299061, -78.94535017580587066, -1.433472983738463435 ) ) ;
#24475 = CARTESIAN_POINT ( 'NONE',  ( -11.00000000000000000, -79.59999999999999432, 0.000000000000000000 ) ) ;
#24476 = CARTESIAN_POINT ( 'NONE',  ( 9.569482281372000188, -76.71319550101999596, -7.743360016082000641 ) ) ;
#24477 = CARTESIAN_POINT ( 'NONE',  ( -1.210822168571097146, -77.88541666666665719, 9.249999999999992895 ) ) ;
#24478 = FACE_OUTER_BOUND ( 'NONE', #47491, .T. ) ;
#24479 = CARTESIAN_POINT ( 'NONE',  ( 9.000511195990998914, -79.25610635638000190, 8.067084866081000172 ) ) ;
#24480 = CARTESIAN_POINT ( 'NONE',  ( 8.174587033571999228, -77.25233320247099300, -8.440297792765999674 ) ) ;
#24481 = DIRECTION ( 'NONE',  ( 1.000000000000000000, 0.000000000000000000, 0.000000000000000000 ) ) ;
#24482 = CARTESIAN_POINT ( 'NONE',  ( 1.430424515561402377, -2.762473447842865415, -2.917857303619362686 ) ) ;
#24483 = CARTESIAN_POINT ( 'NONE',  ( 11.96897150190605075, -77.78965215004572542, -1.561179379743549367 ) ) ;
#24484 = CARTESIAN_POINT ( 'NONE',  ( 10.58946819037999987, -78.47325881071910203, -3.698823201301000285 ) ) ;
#24485 = ORIENTED_EDGE ( 'NONE', *, *, #29875, .T. ) ;
#24486 = CARTESIAN_POINT ( 'NONE',  ( -1.232656909444999949, -83.05356852156999992, -0.5536498640889000455 ) ) ;
#24487 = CARTESIAN_POINT ( 'NONE',  ( 7.220923959705269013, -77.97708333333335418, -9.396085398178609438 ) ) ;
#24488 = DIRECTION ( 'NONE',  ( 0.000000000000000000, 0.000000000000000000, -1.000000000000000000 ) ) ;
#24489 = TOROIDAL_SURFACE ( 'NONE', #8460, 1.250000000000000000, 0.5000000000000000000 ) ;
#24490 = DIRECTION ( 'NONE',  ( 0.000000000000000000, 0.000000000000000000, -1.000000000000000000 ) ) ;
#24491 = CARTESIAN_POINT ( 'NONE',  ( -1.257078809512000017, -2.978982885733000074, -3.494882541721000102 ) ) ;
#24492 = AXIS2_PLACEMENT_3D ( 'NONE', #17176, #87, #40193 ) ;
#24493 = CARTESIAN_POINT ( 'NONE',  ( 1.659836960048000076, -78.80503006069899641, 11.81542141165000004 ) ) ;
#24494 = CARTESIAN_POINT ( 'NONE',  ( 4.763371395742999503, -77.43647980950599674, -8.495292134120999705 ) ) ;
#24496 = CARTESIAN_POINT ( 'NONE',  ( 10.14948852600000073, -22.75100835510000152, -7.674614791843000106 ) ) ;
#24495 = CARTESIAN_POINT ( 'NONE',  ( -10.95378741321288274, -76.17043301730200255, 4.259322154369808544 ) ) ;
#24497 = CARTESIAN_POINT ( 'NONE',  ( -10.46946769381999864, -79.04944879618999209, -3.092832390908999862 ) ) ;
#24498 = CARTESIAN_POINT ( 'NONE',  ( -7.624341766647000362, -18.73514853758999976, 10.42531125024999916 ) ) ;
#24499 = EDGE_LOOP ( 'NONE', ( #55234, #38467 ) ) ;
#24500 = ADVANCED_FACE ( 'NONE', ( #12699 ), #4138, .F. ) ;
#24501 = CARTESIAN_POINT ( 'NONE',  ( -0.2201363562291999698, -79.46327907014000402, -1.483758735329000045 ) ) ;
#24502 = DIRECTION ( 'NONE',  ( 0.000000000000000000, 1.000000000000000000, 0.000000000000000000 ) ) ;
#24503 = CARTESIAN_POINT ( 'NONE',  ( -12.50000000000000000, -18.75000000000000000, 0.000000000000000000 ) ) ;
#24504 = PLANE ( 'NONE',  #53412 ) ;
#24505 = CARTESIAN_POINT ( 'NONE',  ( 9.417408019640999939, -79.81543127184799857, -1.644225498658999918 ) ) ;
#24506 = CARTESIAN_POINT ( 'NONE',  ( 2.900236547156423761, -3.308449514079526033, -1.699047120294984392 ) ) ;
#24507 = CARTESIAN_POINT ( 'NONE',  ( -1.210822168571057400, -79.11458333333335702, -9.250000000000001776 ) ) ;
#24508 = ORIENTED_EDGE ( 'NONE', *, *, #2518, .F. ) ;
#24509 = CARTESIAN_POINT ( 'NONE',  ( 10.94267788024999888, -79.50759371423698951, -2.663036869319000299 ) ) ;
#24510 = CARTESIAN_POINT ( 'NONE',  ( 7.778309126724593625, -76.53609129384345522, -8.035922781116632052 ) ) ;
#24511 = CARTESIAN_POINT ( 'NONE',  ( 0.4924606920183405290, -79.42146225091693168, 11.76080498934809704 ) ) ;
#24512 = CARTESIAN_POINT ( 'NONE',  ( -3.474811874272821566, -78.54828564506389910, 1.963390425425277641 ) ) ;
#24513 = CARTESIAN_POINT ( 'NONE',  ( 6.378305113030960705, -77.28349241254731794, 10.18992046857810330 ) ) ;
#24515 = CARTESIAN_POINT ( 'NONE',  ( -0.4788088652293910341, -81.50646803775929072, 1.154537243539281555 ) ) ;
#24514 = CARTESIAN_POINT ( 'NONE',  ( -0.9554212428760000542, -82.21860252700599858, -0.9097111415877999763 ) ) ;
#24516 = EDGE_CURVE ( 'NONE', #38602, #4702, #9160, .T. ) ;
#24517 = AXIS2_PLACEMENT_3D ( 'NONE', #40966, #36235, #36527 ) ;
#24518 = CARTESIAN_POINT ( 'NONE',  ( 0.7733564461248794153, -78.82670965711476185, -1.012296451130571873 ) ) ;
#24519 = CARTESIAN_POINT ( 'NONE',  ( -1.250000000000000000, -82.09999999999999432, 0.000000000000000000 ) ) ;
#24520 = DIRECTION ( 'NONE',  ( 0.7071067811865475727, 0.000000000000000000, 0.7071067811865475727 ) ) ;
#24521 = CARTESIAN_POINT ( 'NONE',  ( -1.301447353884999991, -78.07207508323999434, 0.1304503950232999976 ) ) ;
#24522 = CARTESIAN_POINT ( 'NONE',  ( 9.913660282387342093, -76.25821898709155278, 4.411731727441804196 ) ) ;
#24523 = CARTESIAN_POINT ( 'NONE',  ( 1.407199643270103717, -78.46460707205700658, 10.68074055511154086 ) ) ;
#24524 = FACE_OUTER_BOUND ( 'NONE', #13027, .T. ) ;
#24525 = ORIENTED_EDGE ( 'NONE', *, *, #51735, .F. ) ;
#24526 = ORIENTED_EDGE ( 'NONE', *, *, #34883, .T. ) ;
#24527 = CARTESIAN_POINT ( 'NONE',  ( 9.633138876124000660, -78.15158998579799743, 2.765897569310999948 ) ) ;
#24528 = CARTESIAN_POINT ( 'NONE',  ( 1.277940389835883872, -78.73453218978592361, -10.67965253657788516 ) ) ;
#24529 = VERTEX_POINT ( 'NONE', #40742 ) ;
#24530 = EDGE_CURVE ( 'NONE', #37512, #233, #26998, .T. ) ;
#24531 = CARTESIAN_POINT ( 'NONE',  ( 9.213130513696000889, -16.99475660687000200, 8.533779407534000327 ) ) ;
#24532 = B_SPLINE_CURVE_WITH_KNOTS ( 'NONE', 3,
 ( #5028, #50495, #15043, #32450 ),
 .UNSPECIFIED., .F., .F.,
 ( 4, 4 ),
 ( 0.000000000000000000, 1.000000000000000000 ),
 .UNSPECIFIED. ) ;
#24533 = AXIS2_PLACEMENT_3D ( 'NONE', #27275, #17854, #23150 ) ;
#24534 = CARTESIAN_POINT ( 'NONE',  ( -9.034130664364234065, -79.37469812230315824, 2.937899820749584112 ) ) ;
#24535 = CARTESIAN_POINT ( 'NONE',  ( -11.19913774713999999, -78.86173899011001254, -4.479602790820000457 ) ) ;
#24536 = CARTESIAN_POINT ( 'NONE',  ( 13.95956770449999951, -33.08075762116000362, 5.182382778583999788E-05 ) ) ;
#24537 = DIRECTION ( 'NONE',  ( 0.07798810297945017733, -0.04890180924492008863, -0.9957542211039027702 ) ) ;
#24538 = CARTESIAN_POINT ( 'NONE',  ( -3.138103972814393572, -86.17851879815597727, 1.326877354892202376 ) ) ;
#24539 = CARTESIAN_POINT ( 'NONE',  ( 3.632329907060999563, -80.25004305557349937, 10.45854222826000068 ) ) ;
#24540 = ORIENTED_EDGE ( 'NONE', *, *, #47407, .T. ) ;
#24541 = CARTESIAN_POINT ( 'NONE',  ( 7.639893379675799068, -55.41284423887101696, -10.11462454828658686 ) ) ;
#24542 = VERTEX_POINT ( 'NONE', #22731 ) ;
#24543 = CARTESIAN_POINT ( 'NONE',  ( 9.134591787879230651, -77.36274324294630844, 1.455986419346108507 ) ) ;
#24544 = CARTESIAN_POINT ( 'NONE',  ( -7.062685404271999978, -77.92069277381098402, 8.485436034813998774 ) ) ;
#24545 = CARTESIAN_POINT ( 'NONE',  ( -10.96076062099048976, -77.33286551245832641, 2.383974742557829707 ) ) ;
#24546 = EDGE_CURVE ( 'NONE', #48410, #51331, #39850, .T. ) ;
#24547 = DIRECTION ( 'NONE',  ( 0.7071067811864980568, 0.7071067811865969777, -6.547095300151979771E-10 ) ) ;
#24548 = CARTESIAN_POINT ( 'NONE',  ( -9.723199429427999974, -17.52306056076000118, 7.958735708429999889 ) ) ;
#24549 = CARTESIAN_POINT ( 'NONE',  ( 0.8819056695273819191, -81.68554651168997793, -0.9213067782626794822 ) ) ;
#24550 = CARTESIAN_POINT ( 'NONE',  ( -0.7213013439201000354, -77.97728518351999583, -1.458901041394999876 ) ) ;
#24551 = CARTESIAN_POINT ( 'NONE',  ( -1.151522233741549606, -79.13191606329839090, -0.4866886816611077915 ) ) ;
#24552 = CARTESIAN_POINT ( 'NONE',  ( 8.374122929021998729, -78.29961660823299496, 7.207772231549999908 ) ) ;
#24553 = CARTESIAN_POINT ( 'NONE',  ( 7.710095619827000313, -58.55064714318000085, 10.18496935397999970 ) ) ;
#24554 = CARTESIAN_POINT ( 'NONE',  ( -12.76303204298000082, -60.06485150663000638, 1.980584515756000030 ) ) ;
#24555 = CARTESIAN_POINT ( 'NONE',  ( 7.601397897754999633, -55.54999999966999980, 9.369164850722000892 ) ) ;
#24556 = CARTESIAN_POINT ( 'NONE',  ( 3.122280780499000485, -85.27576277546900485, -1.678193656463999872 ) ) ;
#24557 = EDGE_LOOP ( 'NONE', ( #48568, #28079, #51055, #46402 ) ) ;
#24558 = CARTESIAN_POINT ( 'NONE',  ( 7.685088506145000942, -78.69410935321799627, 9.438228493448001188 ) ) ;
#24559 = CARTESIAN_POINT ( 'NONE',  ( 0.2675321060165000153, -79.46759604279999678, -1.681415376183999832 ) ) ;
#24560 = CARTESIAN_POINT ( 'NONE',  ( -7.601397897754999633, -55.54999999966999980, -9.369164850722000892 ) ) ;
#24561 = CARTESIAN_POINT ( 'NONE',  ( 7.851705946354000432, -77.31577031326999361, -9.048036745432998629 ) ) ;
#24562 = FACE_OUTER_BOUND ( 'NONE', #43612, .T. ) ;
#24563 = CARTESIAN_POINT ( 'NONE',  ( 0.1450192808573305958, -78.11592896146416365, 1.266846556839069216 ) ) ;
#24564 = CARTESIAN_POINT ( 'NONE',  ( 3.281580320494910996, -3.029571175170358011, 1.280763927392095436 ) ) ;
#24565 = CARTESIAN_POINT ( 'NONE',  ( 8.384816012895999648, -78.89790584965399489, -4.923277454554000343 ) ) ;
#24566 = CARTESIAN_POINT ( 'NONE',  ( -4.391285525405000278, -78.72991978438899707, -8.449082048777999177 ) ) ;
#24567 = CARTESIAN_POINT ( 'NONE',  ( -0.03502584505609534354, -81.22258658432861012, -1.254136478721574299 ) ) ;
#24568 = CARTESIAN_POINT ( 'NONE',  ( 6.963658808075999573, -78.70794695701400201, -8.131364605499999954 ) ) ;
#24569 = CARTESIAN_POINT ( 'NONE',  ( -7.648026766735999793, -23.25000000582000226, 10.12290050089000104 ) ) ;
#24570 = CARTESIAN_POINT ( 'NONE',  ( 5.346968534282000363, -80.36083398343220097, 9.510689753416999181 ) ) ;
#24571 = CARTESIAN_POINT ( 'NONE',  ( -1.034480412912579972, -81.10062156208175566, 0.7433832837861729104 ) ) ;
#24572 = ORIENTED_EDGE ( 'NONE', *, *, #45707, .T. ) ;
#24573 = CARTESIAN_POINT ( 'NONE',  ( -0.1187445621502999926, -81.38356617754199362, -1.328335755224000048 ) ) ;
#24574 = ADVANCED_FACE ( 'NONE', ( #54034 ), #42108, .F. ) ;
#24575 = CARTESIAN_POINT ( 'NONE',  ( 0.000000000000000000, 4.040000000000000036, 0.000000000000000000 ) ) ;
#24576 = CARTESIAN_POINT ( 'NONE',  ( 0.006333666751048999850, -62.13262644267000212, -12.77652491961000081 ) ) ;
#24577 = FACE_OUTER_BOUND ( 'NONE', #6085, .T. ) ;
#24578 = EDGE_CURVE ( 'NONE', #9748, #2879, #3845, .T. ) ;
#24579 = CARTESIAN_POINT ( 'NONE',  ( 8.282307197233999219, -77.95720790972299596, -7.564489280985000619 ) ) ;
#24580 = CARTESIAN_POINT ( 'NONE',  ( 10.28103400416999946, -78.20861358712699030, 3.842432268884000024 ) ) ;
#24581 = CARTESIAN_POINT ( 'NONE',  ( 10.00844230537000001, -23.36891112553000127, -7.647097279392999880 ) ) ;
#24582 = CARTESIAN_POINT ( 'NONE',  ( -3.140358198060591466, -83.36354165683960105, -2.558558009700006686 ) ) ;
#24583 = CARTESIAN_POINT ( 'NONE',  ( -6.446612550560000265, -76.65709426284900019, -10.30178301210999869 ) ) ;
#24584 = CARTESIAN_POINT ( 'NONE',  ( 6.199008894429987926, -78.52998459842886803, 9.981703030362384155 ) ) ;
#24585 = CARTESIAN_POINT ( 'NONE',  ( -1.121108069640562199, -81.13836208406755190, -0.5751273790267441566 ) ) ;
#24586 = ORIENTED_EDGE ( 'NONE', *, *, #12384, .T. ) ;
#24587 = AXIS2_PLACEMENT_3D ( 'NONE', #24812, #20670, #42825 ) ;
#24588 = DIRECTION ( 'NONE',  ( 0.000000000000000000, 0.000000000000000000, -1.000000000000000000 ) ) ;
#24589 = CARTESIAN_POINT ( 'NONE',  ( -11.00000000000000711, -78.18958333333333144, 1.439896632895276696 ) ) ;
#24590 = CARTESIAN_POINT ( 'NONE',  ( 7.620012214408999895, -55.59439747889000216, -10.53562508622999871 ) ) ;
#24591 = EDGE_CURVE ( 'NONE', #25733, #29374, #56185, .T. ) ;
#24592 = CARTESIAN_POINT ( 'NONE',  ( 9.887211716164999942, -78.96897326909299863, 5.401109038458000278 ) ) ;
#24593 = CARTESIAN_POINT ( 'NONE',  ( -3.126089899156312857, -79.19010414275966525, -11.62900749261814326 ) ) ;
#24594 = LINE ( 'NONE', #10434, #23556 ) ;
#24595 = CARTESIAN_POINT ( 'NONE',  ( -0.4798816485349043925, -81.65077628406871213, 1.434309721071634236 ) ) ;
#24596 = CARTESIAN_POINT ( 'NONE',  ( 1.502590276041740447, -82.58012170747866776, -0.3796259133681765263 ) ) ;
#24597 = CARTESIAN_POINT ( 'NONE',  ( -1.058270554699162869, -79.64529829993477961, -0.6656290506933998374 ) ) ;
#24598 = CARTESIAN_POINT ( 'NONE',  ( 1.218586970313583207, -80.87149228721223437, 0.3277392589856675809 ) ) ;
#24599 = ORIENTED_EDGE ( 'NONE', *, *, #37170, .F. ) ;
#24600 = CARTESIAN_POINT ( 'NONE',  ( -0.4278239563775090293, -81.69741778646303487, -1.174506411635975134 ) ) ;
#24601 = CARTESIAN_POINT ( 'NONE',  ( -11.00000000000000711, -79.58958333333332291, 1.439896632895279138 ) ) ;
#24602 = DIRECTION ( 'NONE',  ( 0.000000000000000000, -1.000000000000000000, 0.000000000000000000 ) ) ;
#24603 = ORIENTED_EDGE ( 'NONE', *, *, #656, .F. ) ;
#24604 = ORIENTED_EDGE ( 'NONE', *, *, #40012, .F. ) ;
#24605 = AXIS2_PLACEMENT_3D ( 'NONE', #29580, #47637, #15730 ) ;
#24606 = CARTESIAN_POINT ( 'NONE',  ( 0.09820828907688000653, -80.91715619040499519, 1.513042435352000004 ) ) ;
#24607 = ORIENTED_EDGE ( 'NONE', *, *, #42437, .F. ) ;
#24608 = VERTEX_POINT ( 'NONE', #17419 ) ;
#24609 = CARTESIAN_POINT ( 'NONE',  ( 1.484804496640999893, -17.28130846616999605, 12.77261165608999960 ) ) ;
#24610 = CARTESIAN_POINT ( 'NONE',  ( -4.559293336502967087, -80.44036368348199062, -9.818763842569914857 ) ) ;
#24611 =( LENGTH_UNIT ( ) NAMED_UNIT ( * ) SI_UNIT ( .MILLI., .METRE. ) );
#24612 = CARTESIAN_POINT ( 'NONE',  ( -13.63885489310999510, -56.01421830980998351, -7.254376133916000668 ) ) ;
#24613 = B_SPLINE_CURVE_WITH_KNOTS ( 'NONE', 3,
 ( #11786, #47241, #39504, #52513, #29759, #33908, #52797, #25921, #33627, #47538, #43944, #56371, #6772, #51949, #7063, #38641, #7347, #25347 ),
 .UNSPECIFIED., .F., .F.,
 ( 4, 2, 2, 2, 2, 2, 2, 2, 4 ),
 ( 0.000000000000000000, 0.1250000000000000000, 0.2500000000000000000, 0.3750000000000000000, 0.5000000000000000000, 0.6250000000000000000, 0.7500000000000000000, 0.8750000000000000000, 1.000000000000000000 ),
 .UNSPECIFIED. ) ;
#24614 = CARTESIAN_POINT ( 'NONE',  ( 5.320338141332999982, -79.36539666193300491, -7.841092173349999861 ) ) ;
#24615 = CARTESIAN_POINT ( 'NONE',  ( -1.525577938756555785, -78.21193052228882436, -9.123864793022928410 ) ) ;
#24616 = CARTESIAN_POINT ( 'NONE',  ( 4.782478426736999744, -79.53826565971098717, 10.14623135401999932 ) ) ;
#24617 = ORIENTED_EDGE ( 'NONE', *, *, #9778, .T. ) ;
#24618 = ORIENTED_EDGE ( 'NONE', *, *, #43881, .F. ) ;
#24619 = CARTESIAN_POINT ( 'NONE',  ( -8.891768023477260030, -77.57778467934028299, 2.551063254158453475 ) ) ;
#24620 = AXIS2_PLACEMENT_3D ( 'NONE', #44861, #12395, #30385 ) ;
#24621 = CARTESIAN_POINT ( 'NONE',  ( -1.500000000000000000, -79.00000000000000000, 0.000000000000000000 ) ) ;
#24622 = EDGE_CURVE ( 'NONE', #1594, #39914, #12564, .T. ) ;
#24623 = CARTESIAN_POINT ( 'NONE',  ( -12.49837680052000088, -60.00957148770000060, -1.667051419334000029 ) ) ;
#24624 = CARTESIAN_POINT ( 'NONE',  ( 9.583411031200000707, -78.03241514720498628, 1.526087275887999972 ) ) ;
#24625 = CARTESIAN_POINT ( 'NONE',  ( 7.730443418333229566, -60.92191635792816129, 10.25197760567252558 ) ) ;
#24626 = DIRECTION ( 'NONE',  ( 0.000000000000000000, -0.5547001962253867990, -0.8320502943377385829 ) ) ;
#24627 = CARTESIAN_POINT ( 'NONE',  ( 0.000000000000000000, -0.5000000000000000000, 0.000000000000000000 ) ) ;
#24628 = CARTESIAN_POINT ( 'NONE',  ( -0.4036326496859999891, -80.10214000165998982, 1.533452771621000021 ) ) ;
#24629 = CARTESIAN_POINT ( 'NONE',  ( -0.6947089123876000194, -82.22113100666500429, -1.054176937042999862 ) ) ;
#24630 = CARTESIAN_POINT ( 'NONE',  ( -9.630374193854642328, -76.65109570096610980, 6.732137028299512771 ) ) ;
#24631 = CARTESIAN_POINT ( 'NONE',  ( -3.559519890270999909, -80.05017131030399469, 2.176321128746000255 ) ) ;
#24632 = CARTESIAN_POINT ( 'NONE',  ( -10.52682159589000044, -55.37432398227000618, 7.605688676848999741 ) ) ;
#24633 = CARTESIAN_POINT ( 'NONE',  ( 4.634092916811999530, -78.67108667140098532, -8.633860817301998836 ) ) ;
#24634 = CARTESIAN_POINT ( 'NONE',  ( 9.393545413109377407, -76.80849324769383202, -5.414107032282895915 ) ) ;
#24635 = DIRECTION ( 'NONE',  ( 0.000000000000000000, -1.000000000000000000, -9.403026372076000847E-14 ) ) ;
#24637 = DIRECTION ( 'NONE',  ( 1.000000000000000000, 0.000000000000000000, 0.000000000000000000 ) ) ;
#24636 = CARTESIAN_POINT ( 'NONE',  ( -11.00000000000000000, -18.25000000000000000, 0.000000000000000000 ) ) ;
#24638 = CARTESIAN_POINT ( 'NONE',  ( -12.00000000000000888, -78.38958333333333428, 1.570796326794847264 ) ) ;
#24639 = CARTESIAN_POINT ( 'NONE',  ( -9.474082757681998146, -79.95148679530498725, 5.468759164920000693 ) ) ;
#24640 = CARTESIAN_POINT ( 'NONE',  ( 0.2665495375979000103, -78.45029307777100769, -11.25891151133000001 ) ) ;
#24641 = CARTESIAN_POINT ( 'NONE',  ( -3.099241092295174305, -1.710269946423099929, 1.691961027787603378 ) ) ;
#24642 = ORIENTED_EDGE ( 'NONE', *, *, #17350, .F. ) ;
#24643 = CARTESIAN_POINT ( 'NONE',  ( -1.894625102906858594, -3.499999999999999556, -2.799120236218770597 ) ) ;
#24644 = DIRECTION ( 'NONE',  ( 1.000000000000000000, 0.000000000000000000, 0.000000000000000000 ) ) ;
#24645 = CARTESIAN_POINT ( 'NONE',  ( 0.6540410530999497540, -78.43152095752569153, 1.066316062253257702 ) ) ;
#24646 =( GEOMETRIC_REPRESENTATION_CONTEXT ( 3 ) GLOBAL_UNCERTAINTY_ASSIGNED_CONTEXT ( ( #52006 ) ) GLOBAL_UNIT_ASSIGNED_CONTEXT ( ( #38750, #25751, #16329 ) ) REPRESENTATION_CONTEXT ( 'NONE', 'WORKASPACE' ) );
#24648 = EDGE_CURVE ( 'NONE', #5425, #9344, #13812, .T. ) ;
#24647 = B_SPLINE_CURVE_WITH_KNOTS ( 'NONE', 3,
 ( #35626, #53655, #13195, #19398, #41245, #45695, #15254, #32951, #36808, #32656, #19688, #834, #42129, #1407, #5515, #32081, #10247, #18816 ),
 .UNSPECIFIED., .F., .F.,
 ( 4, 2, 2, 2, 2, 2, 2, 2, 4 ),
 ( 0.000000000000000000, 0.06250000000000079103, 0.1250000000000015821, 0.2500000000000031086, 0.5000000000000023315, 0.7500000000000016653, 0.8125000000000025535, 0.8750000000000034417, 1.000000000000000000 ),
 .UNSPECIFIED. ) ;
#24649 = CARTESIAN_POINT ( 'NONE',  ( -6.456202977062000414, -79.89113977864099070, 7.014830417985999489 ) ) ;
#24650 = CARTESIAN_POINT ( 'NONE',  ( -3.346450045594000056, -76.84369696823999618, 12.57540552286999791 ) ) ;
#24651 = CARTESIAN_POINT ( 'NONE',  ( -0.5544288313492085063, -79.47928052470416560, 10.73600753435132482 ) ) ;
#24652 = B_SPLINE_CURVE_WITH_KNOTS ( 'NONE', 3,
 ( #40672, #27947, #263, #18245, #36234, #54257, #31791, #49833, #37982, #46583, #28535, #24989, #7275, #56294, #15262, #15557, #6985, #25277 ),
 .UNSPECIFIED., .F., .F.,
 ( 4, 2, 2, 2, 2, 2, 2, 2, 4 ),
 ( 0.000000000000000000, 0.1250000000000000555, 0.2500000000000001110, 0.3750000000000001665, 0.5000000000000002220, 0.6250000000000002220, 0.7500000000000002220, 0.8750000000000001110, 1.000000000000000000 ),
 .UNSPECIFIED. ) ;
#24653 = CARTESIAN_POINT ( 'NONE',  ( 7.737894983877000143, -79.57843998579799916, -5.744169665113000534 ) ) ;
#24654 = B_SPLINE_CURVE_WITH_KNOTS ( 'NONE', 3,
 ( #28051, #365, #27761, #45804, #23346, #18345, #1511, #5339, #18922, #32471, #31600, #50517, #9189, #27174, #36335, #54360 ),
 .UNSPECIFIED., .F., .F.,
 ( 4, 2, 2, 2, 2, 2, 2, 4 ),
 ( 0.000000000000000000, 0.2499999999999954481, 0.3749999999999962252, 0.4374999999999965583, 0.4999999999999970024, 0.6249999999999976685, 0.7499999999999985567, 1.000000000000000000 ),
 .UNSPECIFIED. ) ;
#24655 = FACE_OUTER_BOUND ( 'NONE', #10353, .T. ) ;
#24656 = CARTESIAN_POINT ( 'NONE',  ( 6.450682458815999887, -77.54595490982698891, -8.845531009145000567 ) ) ;
#24657 = ADVANCED_FACE ( 'NONE', ( #4434 ), #30738, .F. ) ;
#24658 = CARTESIAN_POINT ( 'NONE',  ( 1.367042039058000036, -82.20187207508699601, 0.8392497673348999765 ) ) ;
#24659 = CARTESIAN_POINT ( 'NONE',  ( 4.316051676898999823, -78.98839514476064494, 8.712949996777000550 ) ) ;
#24660 = CIRCLE ( 'NONE', #35976, 1.750000000000001332 ) ;
#24661 = CARTESIAN_POINT ( 'NONE',  ( -2.495045882587000108, -78.62446617076199118, -9.076670124625998426 ) ) ;
#24662 = EDGE_CURVE ( 'NONE', #7670, #54925, #5310, .T. ) ;
#24664 = DIRECTION ( 'NONE',  ( -0.7592504788685899841, -0.04890177849874939586, -0.6489586476790920599 ) ) ;
#24663 = CARTESIAN_POINT ( 'NONE',  ( -1.739964340038000046, -85.62879675702399140, 3.560717623133999865 ) ) ;
#24665 = CARTESIAN_POINT ( 'NONE',  ( 1.861092857305999937, -79.83075584965399685, -9.371850619045000386 ) ) ;
#24666 = CARTESIAN_POINT ( 'NONE',  ( -0.3271848554490991434, -82.60416666666665719, -1.217465845835395299 ) ) ;
#24667 = CARTESIAN_POINT ( 'NONE',  ( 4.168617279563824773, -80.25678616003493460, -9.908796504410707584 ) ) ;
#24668 = DIRECTION ( 'NONE',  ( 0.000000000000000000, -1.000000000000000000, 0.000000000000000000 ) ) ;
#24669 = DIRECTION ( 'NONE',  ( -1.000000000000000000, 0.000000000000000000, 0.000000000000000000 ) ) ;
#24670 = AXIS2_PLACEMENT_3D ( 'NONE', #55106, #1396, #19391 ) ;
#24671 = CARTESIAN_POINT ( 'NONE',  ( -10.65106809510000119, -79.09542617043000234, 5.591232889670999739 ) ) ;
#24672 = FACE_OUTER_BOUND ( 'NONE', #10384, .T. ) ;
#24673 = DIRECTION ( 'NONE',  ( 0.000000000000000000, 1.000000000000000000, 0.000000000000000000 ) ) ;
#24674 = ORIENTED_EDGE ( 'NONE', *, *, #19378, .F. ) ;
#24675 = CARTESIAN_POINT ( 'NONE',  ( -10.23070583620000207, -78.58036326492899093, 6.145580569783000158 ) ) ;
#24676 = ORIENTED_EDGE ( 'NONE', *, *, #8769, .F. ) ;
#24677 = VERTEX_POINT ( 'NONE', #51075 ) ;
#24678 = ADVANCED_FACE ( 'NONE', ( #42207 ), #55192, .T. ) ;
#24679 = ORIENTED_EDGE ( 'NONE', *, *, #29166, .F. ) ;
#24680 = CARTESIAN_POINT ( 'NONE',  ( 3.537682960765999862, -79.44891918789778629, 0.2633619146721000170 ) ) ;
#24681 = CARTESIAN_POINT ( 'NONE',  ( 6.963965595795851726, -79.20918829156502738, 6.469944903610358011 ) ) ;
#24682 = ORIENTED_EDGE ( 'NONE', *, *, #56544, .T. ) ;
#24683 = CARTESIAN_POINT ( 'NONE',  ( -10.42531125072000009, -55.53514854654000032, -7.624341767124000135 ) ) ;
#24684 = ORIENTED_EDGE ( 'NONE', *, *, #7574, .T. ) ;
#24685 = COLOUR_RGB ( '', 0.66274510, 0.83137255, 0.94901961) ;
#24686 = CARTESIAN_POINT ( 'NONE',  ( -10.07979664880000037, -76.97175206120299151, 3.736335038366999761 ) ) ;
#24687 = ORIENTED_EDGE ( 'NONE', *, *, #53630, .F. ) ;
#24688 = CARTESIAN_POINT ( 'NONE',  ( -1.162279827862261916, -79.57043678867249525, 0.4597564725974967459 ) ) ;
#24689 = CARTESIAN_POINT ( 'NONE',  ( 1.162102752763446878, -78.94315431229624380, -1.000785636504023524 ) ) ;
#24690 = CARTESIAN_POINT ( 'NONE',  ( 10.62400023845289532, -79.79999999999999716, 5.163243916854518112 ) ) ;
#24691 = EDGE_CURVE ( 'NONE', #23377, #35060, #49166, .T. ) ;
#24692 = CARTESIAN_POINT ( 'NONE',  ( -1.777724524818122598, -78.83678780677392695, 12.13456374090698553 ) ) ;
#24693 = CARTESIAN_POINT ( 'NONE',  ( 9.259046916275000427, -78.52419600967778024, 2.905298533503999803 ) ) ;
#24694 = CARTESIAN_POINT ( 'NONE',  ( -10.99972769911000015, -76.31944253928298849, 2.019869862886000345 ) ) ;
#24695 = DIRECTION ( 'NONE',  ( -1.000000000000000000, 0.000000000000000000, 0.000000000000000000 ) ) ;
#24696 = EDGE_CURVE ( 'NONE', #3531, #36712, #57625, .T. ) ;
#24697 = CARTESIAN_POINT ( 'NONE',  ( -5.539808784079931492, -78.61666666666667425, 9.611650271896815312 ) ) ;
#24698 = CARTESIAN_POINT ( 'NONE',  ( -7.942520732695999008, -76.51965762081900380, -7.609088033453000222 ) ) ;
#24699 = CARTESIAN_POINT ( 'NONE',  ( -7.448626198570991619, -78.65061730849956234, -5.485182927975110090 ) ) ;
#24700 = CARTESIAN_POINT ( 'NONE',  ( 2.303363178838841119, -76.55889284051112043, 11.52175839890178288 ) ) ;
#24701 = AXIS2_PLACEMENT_3D ( 'NONE', #50553, #41394, #45840 ) ;
#24702 = CARTESIAN_POINT ( 'NONE',  ( -10.88354252222900520, -80.11174396849405355, -1.596899905050069401 ) ) ;
#24703 = FACE_OUTER_BOUND ( 'NONE', #12607, .T. ) ;
#24704 = CARTESIAN_POINT ( 'NONE',  ( -2.815196241353000506, -81.56803455456798702, -2.487173068765999862 ) ) ;
#24705 = CARTESIAN_POINT ( 'NONE',  ( -11.78732249294000134, -79.09425612125899363, -2.660533726555999845 ) ) ;
#24706 = VECTOR ( 'NONE', #47494, 1000.000000000000000 ) ;
#24707 = CARTESIAN_POINT ( 'NONE',  ( -8.337895600304513266, -78.04578102920540061, 6.785427785908417775 ) ) ;
#24708 = CARTESIAN_POINT ( 'NONE',  ( 0.8599086838611078587, -82.91523954447930578, 0.9066764497312405080 ) ) ;
#24709 = CARTESIAN_POINT ( 'NONE',  ( -12.00000000000000000, -55.54999999966999980, -1.750000000000000000 ) ) ;
#24710 = B_SPLINE_CURVE_WITH_KNOTS ( 'NONE', 3,
 ( #5368, #36945, #54956, #14509 ),
 .UNSPECIFIED., .F., .F.,
 ( 4, 4 ),
 ( 0.000000000000000000, 1.000000000000000000 ),
 .UNSPECIFIED. ) ;
#24711 = CARTESIAN_POINT ( 'NONE',  ( -3.999999999999815259, -78.72610001270986402, -1.678385095468384722E-14 ) ) ;
#24712 = CARTESIAN_POINT ( 'NONE',  ( 0.9995835529977233902, -80.30208333333334281, 0.7681833999686461523 ) ) ;
#24713 = DIRECTION ( 'NONE',  ( 0.000000000000000000, 0.000000000000000000, -1.000000000000000000 ) ) ;
#24714 = DIRECTION ( 'NONE',  ( 1.000000000000000000, 0.000000000000000000, 1.147010004337999914E-14 ) ) ;
#24715 = CARTESIAN_POINT ( 'NONE',  ( 9.500000000000001776, -78.16041666666667709, 1.243547092045981239 ) ) ;
#24716 = CARTESIAN_POINT ( 'NONE',  ( 0.6224761083686999319, -81.79798298199800399, -1.179448874982999884 ) ) ;
#24717 = FACE_OUTER_BOUND ( 'NONE', #39691, .T. ) ;
#24718 = CARTESIAN_POINT ( 'NONE',  ( 12.77301895549999955, -25.05186686373999905, 1.052127376137000025 ) ) ;
#24719 = CARTESIAN_POINT ( 'NONE',  ( 7.782819286693597682, -77.76121216632311928, 7.448878563881510040 ) ) ;
#24720 =( NAMED_UNIT ( * ) SI_UNIT ( $, .STERADIAN. ) SOLID_ANGLE_UNIT ( ) );
#24721 = CARTESIAN_POINT ( 'NONE',  ( -1.930860503526836469, -23.77417505915145668, -12.72930866331899225 ) ) ;
#24722 = DIRECTION ( 'NONE',  ( 0.000000000000000000, 1.000000000000000000, 0.000000000000000000 ) ) ;
#24723 = VERTEX_POINT ( 'NONE', #32155 ) ;
#24724 = CARTESIAN_POINT ( 'NONE',  ( -3.181627547869000150, -83.35221544543098560, 2.362885332182999676 ) ) ;
#24725 = CARTESIAN_POINT ( 'NONE',  ( -10.40000000000000036, 0.000000000000000000, 0.000000000000000000 ) ) ;
#24726 = CARTESIAN_POINT ( 'NONE',  ( 9.191416345675177624, -78.34109437452993063, -1.039168553220889635 ) ) ;
#24727 = DIRECTION ( 'NONE',  ( -1.000000000000000000, 0.000000000000000000, 0.000000000000000000 ) ) ;
#24728 = CARTESIAN_POINT ( 'NONE',  ( -10.05535668103000191, -78.36514844629400045, 4.970705447719999448 ) ) ;
#24729 = CARTESIAN_POINT ( 'NONE',  ( 12.83838672487999943, -55.59401611997999737, -2.062170725306000207 ) ) ;
#24730 = CARTESIAN_POINT ( 'NONE',  ( -8.803456334546002182, -77.86436236583298864, -4.166395597179999299 ) ) ;
#24731 = DIRECTION ( 'NONE',  ( 1.000000000000000000, 0.000000000000000000, 0.000000000000000000 ) ) ;
#24732 = CARTESIAN_POINT ( 'NONE',  ( -12.00000000000000000, -18.84999999999999787, 0.000000000000000000 ) ) ;
#24733 = CARTESIAN_POINT ( 'NONE',  ( -0.2056945464814999847, -80.37710733580000522, 1.601533168507999871 ) ) ;
#24734 = ORIENTED_EDGE ( 'NONE', *, *, #18313, .T. ) ;
#24735 = CARTESIAN_POINT ( 'NONE',  ( -7.601397897754999633, -18.75000000310999937, 10.07627163191000008 ) ) ;
#24736 = CARTESIAN_POINT ( 'NONE',  ( 2.984579200595963488, -79.00013989958746663, -2.163174824610843316 ) ) ;
#24737 = ORIENTED_EDGE ( 'NONE', *, *, #52565, .T. ) ;
#24738 = CARTESIAN_POINT ( 'NONE',  ( 0.6849175148897999055, -77.84603263957740182, -1.144319635748999975 ) ) ;
#24739 = CARTESIAN_POINT ( 'NONE',  ( 12.87022657274000004, -59.58485473249000108, 2.062597299672999540 ) ) ;
#24740 = CARTESIAN_POINT ( 'NONE',  ( 0.7676926012113186593, -80.77788394861798338, -0.9996391181222294975 ) ) ;
#24741 = ORIENTED_EDGE ( 'NONE', *, *, #28233, .T. ) ;
#24742 = CARTESIAN_POINT ( 'NONE',  ( 9.289757862025998847, -78.06471382358499511, 7.853848066408001038 ) ) ;
#24743 = CARTESIAN_POINT ( 'NONE',  ( 0.3834289305765000155, -77.68463329503899217, -11.31570682219000012 ) ) ;
#24744 = AXIS2_PLACEMENT_3D ( 'NONE', #46136, #36665, #41682 ) ;
#24745 = VERTEX_POINT ( 'NONE', #13871 ) ;
#24746 = ORIENTED_EDGE ( 'NONE', *, *, #25046, .T. ) ;
#24747 = EDGE_CURVE ( 'NONE', #51603, #28435, #15035, .T. ) ;
#24748 = CARTESIAN_POINT ( 'NONE',  ( -0.008218136894757548452, -80.47612516791997450, 1.249622453350030638 ) ) ;
#24749 = EDGE_CURVE ( 'NONE', #39417, #38447, #42794, .T. ) ;
#24750 = VECTOR ( 'NONE', #56140, 1000.000000000000000 ) ;
#24751 = CARTESIAN_POINT ( 'NONE',  ( 10.48543666025108401, -79.59166666666666856, 6.043427764450814976 ) ) ;
#24752 = CARTESIAN_POINT ( 'NONE',  ( -5.726462542197000793, -80.32516014362252577, -7.912542777261000637 ) ) ;
#24753 = ORIENTED_EDGE ( 'NONE', *, *, #6783, .F. ) ;
#24754 = CARTESIAN_POINT ( 'NONE',  ( -8.065049863481000614, -78.51455857394600457, 7.357332172019000360 ) ) ;
#24755 = ORIENTED_EDGE ( 'NONE', *, *, #20942, .T. ) ;
#24756 = CARTESIAN_POINT ( 'NONE',  ( 3.463448050014508173, -80.75108394742497353, -10.20029982960495651 ) ) ;
#24757 = CARTESIAN_POINT ( 'NONE',  ( 9.102117850491421081, -24.97186524165807242, 8.583692176894766490 ) ) ;
#24758 = AXIS2_PLACEMENT_3D ( 'NONE', #37655, #14630, #50675 ) ;
#24759 = CARTESIAN_POINT ( 'NONE',  ( 9.073547343531414455, -16.77191135192954619, -8.894853367293087842 ) ) ;
#24760 = CARTESIAN_POINT ( 'NONE',  ( -1.310679582531389276, -81.35833333333332007, 0.7554284705563443225 ) ) ;
#24761 = B_SPLINE_CURVE_WITH_KNOTS ( 'NONE', 3,
 ( #5272, #40705, #18572, #26811 ),
 .UNSPECIFIED., .F., .F.,
 ( 4, 4 ),
 ( 0.7500000006367434358, 1.000000000000000000 ),
 .UNSPECIFIED. ) ;
#24762 = CARTESIAN_POINT ( 'NONE',  ( -7.531956854635054377, -78.10362913613842295, -6.151674355925288218 ) ) ;
#24763 = EDGE_CURVE ( 'NONE', #33222, #46115, #5588, .T. ) ;
#24764 = VECTOR ( 'NONE', #48383, 999.9999999999998863 ) ;
#24765 = CARTESIAN_POINT ( 'NONE',  ( -9.078045636453000000, -77.18772503547859287, 3.793810669397000179 ) ) ;
#24766 = CARTESIAN_POINT ( 'NONE',  ( 11.79999999999999893, -23.15000000000999947, 0.5999999999999999778 ) ) ;
#24767 = CARTESIAN_POINT ( 'NONE',  ( 5.539808784079905735, -79.76666666666666572, -9.611650271896829523 ) ) ;
#24768 = CARTESIAN_POINT ( 'NONE',  ( -7.948089776770999926, -24.44033979720000360, 9.636757666087000018 ) ) ;
#24769 = FACE_OUTER_BOUND ( 'NONE', #44206, .T. ) ;
#24770 = CARTESIAN_POINT ( 'NONE',  ( 8.798028344890999719, -61.73813495650999528, -8.790623041469000754 ) ) ;
#24771 = CARTESIAN_POINT ( 'NONE',  ( -12.02296678431999943, -78.43220577152999340, 2.418109797047000242 ) ) ;
#24772 = CARTESIAN_POINT ( 'NONE',  ( -12.17466003208999936, -76.55562665128699962, 1.612538369963999907 ) ) ;
#24773 = DIRECTION ( 'NONE',  ( 0.000000000000000000, 1.000000000000000000, 0.000000000000000000 ) ) ;
#24774 = CARTESIAN_POINT ( 'NONE',  ( -11.64898813392143317, -77.57617276172848619, -3.925102516053998070 ) ) ;
#24775 = CARTESIAN_POINT ( 'NONE',  ( -10.48543666025109111, -77.84166666666665435, -6.043427764450793660 ) ) ;
#24776 = EDGE_CURVE ( 'NONE', #10831, #54597, #23601, .T. ) ;
#24777 = ORIENTED_EDGE ( 'NONE', *, *, #7953, .F. ) ;
#24778 = CARTESIAN_POINT ( 'NONE',  ( 0.9533626797078339488, -80.07179590631209010, 1.220572805882581990 ) ) ;
#24779 = CARTESIAN_POINT ( 'NONE',  ( -0.8436256567094999603, -76.94726210441848480, -9.670559092448998584 ) ) ;
#24780 = CARTESIAN_POINT ( 'NONE',  ( 1.798944584243999945, -23.21533228280000216, 12.61116915999999932 ) ) ;
#24781 = CARTESIAN_POINT ( 'NONE',  ( -14.00000000000000000, -6.100000000000000533, 0.000000000000000000 ) ) ;
#24782 = CARTESIAN_POINT ( 'NONE',  ( -3.669758066562000209, -2.393766836959000166, -0.5721248644209000478 ) ) ;
#24783 = CARTESIAN_POINT ( 'NONE',  ( 10.85897810694999954, -78.15392649052799356, -5.483167429328999809 ) ) ;
#24784 = CARTESIAN_POINT ( 'NONE',  ( -9.480927541711999140, -78.28919468337598175, -2.229732866345000009 ) ) ;
#24786 = DIRECTION ( 'NONE',  ( 0.000000000000000000, 1.000000000000000000, 0.000000000000000000 ) ) ;
#24785 = CARTESIAN_POINT ( 'NONE',  ( -8.887117850294183441, -76.14310715044948097, 7.686514976405625532 ) ) ;
#24787 = CARTESIAN_POINT ( 'NONE',  ( -0.6329778402533998705, -81.66623022861000436, -1.193863583722999833 ) ) ;
#24788 = DIRECTION ( 'NONE',  ( 0.7071067811865475727, 0.000000000000000000, -0.7071067811865475727 ) ) ;
#24789 = VERTEX_POINT ( 'NONE', #45773 ) ;
#24790 = CARTESIAN_POINT ( 'NONE',  ( 8.815588752397863104, -76.73947780777287164, -8.371812616114789662 ) ) ;
#24791 = AXIS2_PLACEMENT_3D ( 'NONE', #15038, #51944, #3212 ) ;
#24792 = DIRECTION ( 'NONE',  ( -1.000000000000000000, 0.000000000000000000, 0.000000000000000000 ) ) ;
#24793 = CARTESIAN_POINT ( 'NONE',  ( -8.909545442949999838, -57.79999999967000690, -7.919595949288999570 ) ) ;
#24794 = CARTESIAN_POINT ( 'NONE',  ( 2.269106295766999856E-14, -92.79999999999999716, -12.09999999998845865 ) ) ;
#24795 = LINE ( 'NONE', #33924, #29862 ) ;
#24796 = CARTESIAN_POINT ( 'NONE',  ( -2.967406986365000332, -79.47930234752600143, 9.087659770315999808 ) ) ;
#24797 = CARTESIAN_POINT ( 'NONE',  ( -1.570796326794884790, -78.01458333333333428, -12.00000000000000355 ) ) ;
#24798 = CARTESIAN_POINT ( 'NONE',  ( -12.70255494770078109, -54.05391159001328560, -1.306413223709476323 ) ) ;
#24799 = ORIENTED_EDGE ( 'NONE', *, *, #57608, .F. ) ;
#24801 = AXIS2_PLACEMENT_3D ( 'NONE', #11941, #51815, #47393 ) ;
#24800 = CARTESIAN_POINT ( 'NONE',  ( -4.169330562119000660, -79.37141199922800183, -10.46186633551000078 ) ) ;
#24802 = CARTESIAN_POINT ( 'NONE',  ( -7.860640992941333671, -76.78691071373445709, 7.955411750889882505 ) ) ;
#24803 = CARTESIAN_POINT ( 'NONE',  ( 12.50000000000000000, -23.24999999688999708, 1.750000000000000000 ) ) ;
#24804 = CARTESIAN_POINT ( 'NONE',  ( 0.5999999999999999778, -5.200000000000000178, 4.000000000000000000 ) ) ;
#24805 = AXIS2_PLACEMENT_3D ( 'NONE', #290, #14115, #54853 ) ;
#24806 = CARTESIAN_POINT ( 'NONE',  ( 0.4350654701194750507, -81.44699977334819607, 1.171762940142557552 ) ) ;
#24807 = B_SPLINE_CURVE_WITH_KNOTS ( 'NONE', 3,
 ( #5525, #51300, #23534, #843 ),
 .UNSPECIFIED., .F., .F.,
 ( 4, 4 ),
 ( 0.000000000000000000, 0.1666666058611807055 ),
 .UNSPECIFIED. ) ;
#24808 = CARTESIAN_POINT ( 'NONE',  ( -0.3252833033496160819, -78.25425631041045449, -1.232823141656065102 ) ) ;
#24809 = CARTESIAN_POINT ( 'NONE',  ( -0.7678540140355195609, -82.17356543371400335, -0.9996003491978228128 ) ) ;
#24810 = CARTESIAN_POINT ( 'NONE',  ( 1.667916687331000070, -55.50151115525000023, -12.49168451095999899 ) ) ;
#24811 = CARTESIAN_POINT ( 'NONE',  ( 0.8160112056498999289, -78.81700217913999040, -1.163845997288000200 ) ) ;
#24812 = CARTESIAN_POINT ( 'NONE',  ( -8.485281374238999419, 0.000000000000000000, -8.485281374238999419 ) ) ;
#24813 = DIRECTION ( 'NONE',  ( 0.7071067811865974218, 0.7071067811864975017, 8.595327382698963620E-09 ) ) ;
#24814 = CARTESIAN_POINT ( 'NONE',  ( 9.202039358297998461, -79.97952878580598224, 2.360608321670000453 ) ) ;
#24815 = ORIENTED_EDGE ( 'NONE', *, *, #23694, .F. ) ;
#24816 = ORIENTED_EDGE ( 'NONE', *, *, #56755, .T. ) ;
#24817 = CARTESIAN_POINT ( 'NONE',  ( 12.26182288558000089, -76.99428088996099007, -2.272484397021000024 ) ) ;
#24818 = CARTESIAN_POINT ( 'NONE',  ( 5.974621249351785401, -78.77206790660797253, -8.936673600286241026 ) ) ;
#24819 = AXIS2_PLACEMENT_3D ( 'NONE', #10630, #10334, #32742 ) ;
#24820 = EDGE_LOOP ( 'NONE', ( #11939, #28841, #28946, #25474 ) ) ;
#24821 = CARTESIAN_POINT ( 'NONE',  ( 7.645398650971000798, -18.78468617155999709, 10.18948982068999953 ) ) ;
#24822 = CARTESIAN_POINT ( 'NONE',  ( -7.220923959705244144, -75.87291666666665435, -9.396085398178621872 ) ) ;
#24823 = CARTESIAN_POINT ( 'NONE',  ( 5.486311112560000147, -78.09489713918000575, 11.38883617360999878 ) ) ;
#24824 = CARTESIAN_POINT ( 'NONE',  ( 1.407207864692765265, -79.73543568848991470, -10.68080165316230001 ) ) ;
#24826 = EDGE_CURVE ( 'NONE', #23344, #21820, #28307, .T. ) ;
#24825 = CARTESIAN_POINT ( 'NONE',  ( 0.000000000000000000, 4.040000000000000036, 0.000000000000000000 ) ) ;
#24827 = DIRECTION ( 'NONE',  ( -0.9957542217959268749, -0.04890179607413128876, -0.07798810240230209800 ) ) ;
#24828 = CARTESIAN_POINT ( 'NONE',  ( 10.89876807034000095, -79.56489739425599339, -2.652350870517000025 ) ) ;
#24829 = ORIENTED_EDGE ( 'NONE', *, *, #44536, .T. ) ;
#24830 = CARTESIAN_POINT ( 'NONE',  ( -0.9088587313318036154, -78.18115558532333864, 11.75905384473932713 ) ) ;
#24831 = ORIENTED_EDGE ( 'NONE', *, *, #10266, .T. ) ;
#24832 = CARTESIAN_POINT ( 'NONE',  ( 5.585446503142362573, -77.27674399426018681, -7.373492375193941406 ) ) ;
#24833 = CARTESIAN_POINT ( 'NONE',  ( 14.00000000000000000, -69.50420297070000686, 0.000000000000000000 ) ) ;
#24834 = CARTESIAN_POINT ( 'NONE',  ( 10.50000000000000000, -76.19999999999998863, 0.000000000000000000 ) ) ;
#24835 = CARTESIAN_POINT ( 'NONE',  ( -0.9512462306705773418, -78.23166483151833006, 11.17661574778309408 ) ) ;
#24836 = UNCERTAINTY_MEASURE_WITH_UNIT (LENGTH_MEASURE( 1.000000000000000082E-05 ), #24962, 'distance_accuracy_value', 'NONE');
#24837 = CARTESIAN_POINT ( 'NONE',  ( -1.500872881732000064, -78.55864840198100296, -0.2152271930174000092 ) ) ;
#24838 = AXIS2_PLACEMENT_3D ( 'NONE', #36828, #1712, #19123 ) ;
#24839 = CARTESIAN_POINT ( 'NONE',  ( 0.000000000000000000, -76.15000000005198899, 0.000000000000000000 ) ) ;
#24840 = DIRECTION ( 'NONE',  ( 0.7071067811865474617, 0.000000000000000000, 0.7071067811865474617 ) ) ;
#24841 = CARTESIAN_POINT ( 'NONE',  ( -1.560595261880000084, -77.86592204395999772, 0.4619550309703999713 ) ) ;
#24842 = CARTESIAN_POINT ( 'NONE',  ( -1.141620584689441609, -79.13348047058508428, -0.5094065323112431098 ) ) ;
#24843 = CARTESIAN_POINT ( 'NONE',  ( 10.78711022396000097, -79.76041903353200269, 2.390846439793999689 ) ) ;
#24844 = CARTESIAN_POINT ( 'NONE',  ( 7.652056849481999379, -79.47013533719341183, 9.281873293285000770 ) ) ;
#24845 = EDGE_CURVE ( 'NONE', #12605, #19229, #41436, .T. ) ;
#24846 = CARTESIAN_POINT ( 'NONE',  ( -7.674614791501999989, -59.55100836074000625, -10.14948852566000070 ) ) ;
#24847 = CARTESIAN_POINT ( 'NONE',  ( -3.308771268993000003, -83.30055803339699594, -1.278124539089000145 ) ) ;
#24848 = VERTEX_POINT ( 'NONE', #56077 ) ;
#24849 = CARTESIAN_POINT ( 'NONE',  ( -0.6962927961685000389, -82.42150394949298686, -1.554024870232999955 ) ) ;
#24850 = CARTESIAN_POINT ( 'NONE',  ( 1.554657762476000071, -81.04657642056000100, -0.6948770361563999520 ) ) ;
#24851 = CARTESIAN_POINT ( 'NONE',  ( 6.606356555483213100, -79.27722184295002705, -8.596560213042563348 ) ) ;
#24852 = CARTESIAN_POINT ( 'NONE',  ( 4.899854808515000215, -78.15684856197299268, -10.93194800986000104 ) ) ;
#24853 = CARTESIAN_POINT ( 'NONE',  ( -7.969034948596000589, -17.37623147815000024, 9.934750886910000744 ) ) ;
#24854 = CARTESIAN_POINT ( 'NONE',  ( -1.250000000000000000, -77.75000000000000000, 0.000000000000000000 ) ) ;
#24855 = FACE_OUTER_BOUND ( 'NONE', #41631, .T. ) ;
#24856 = CARTESIAN_POINT ( 'NONE',  ( 10.24002203034363490, -80.87489730094399931, 3.274717220204576229 ) ) ;
#24857 = CARTESIAN_POINT ( 'NONE',  ( -0.1509935689429000305, -78.01932405616399535, 9.520902119764999227 ) ) ;
#24858 = CARTESIAN_POINT ( 'NONE',  ( 1.886823409076999969, -55.03680315604999151, -12.68610076202999792 ) ) ;
#24859 = CARTESIAN_POINT ( 'NONE',  ( 6.327673118679000730, -77.63247520153299774, -9.036718833993001354 ) ) ;
#24860 = DIRECTION ( 'NONE',  ( 0.7071067811865474617, 0.000000000000000000, -0.7071067811865474617 ) ) ;
#24861 = CARTESIAN_POINT ( 'NONE',  ( -8.965068030445999980, -80.97833076151569287, 6.218612530207000333 ) ) ;
#24862 = CARTESIAN_POINT ( 'NONE',  ( 0.8920022376942984277, -81.46635564469825397, 0.9829159123015102084 ) ) ;
#24863 = ORIENTED_EDGE ( 'NONE', *, *, #4833, .F. ) ;
#24864 = CARTESIAN_POINT ( 'NONE',  ( 10.98754182310580063, -18.54785535412668551, -0.5242772304895085833 ) ) ;
#24865 = CARTESIAN_POINT ( 'NONE',  ( 1.389926494650000066, -61.42381336221999533, -12.65988803926999928 ) ) ;
#24866 = CARTESIAN_POINT ( 'NONE',  ( -2.813754150119270658, -80.49592687992846152, 10.47067054086312332 ) ) ;
#24867 = CARTESIAN_POINT ( 'NONE',  ( 7.199825537761999961, -77.08564493366499448, 8.601198917431998936 ) ) ;
#24868 = CARTESIAN_POINT ( 'NONE',  ( 1.684372618195999927, -78.29289065012498838, 10.84559388857000073 ) ) ;
#24869 = DIRECTION ( 'NONE',  ( 0.000000000000000000, 0.000000000000000000, -1.000000000000000000 ) ) ;
#24870 = CARTESIAN_POINT ( 'NONE',  ( -3.107766917196799206, -84.86666667301983580, -2.600398495668877263 ) ) ;
#24871 = EDGE_CURVE ( 'NONE', #50394, #5279, #25340, .T. ) ;
#24872 = CARTESIAN_POINT ( 'NONE',  ( -9.850507816072157752, -61.10508874482341213, 7.836744050180310950 ) ) ;
#24873 = PLANE ( 'NONE',  #31151 ) ;
#24874 = DIRECTION ( 'NONE',  ( 0.000000000000000000, -1.000000000000000000, 0.000000000000000000 ) ) ;
#24875 = ORIENTED_EDGE ( 'NONE', *, *, #13028, .T. ) ;
#24876 = CARTESIAN_POINT ( 'NONE',  ( -0.8402681406225442906, -80.03420601024139103, 0.9269689668249517789 ) ) ;
#24877 = CARTESIAN_POINT ( 'NONE',  ( -8.800000000000000711, 0.000000000000000000, 0.000000000000000000 ) ) ;
#24878 = CIRCLE ( 'NONE', #57851, 13.89999999999999858 ) ;
#24879 = CARTESIAN_POINT ( 'NONE',  ( -7.208482872893000604, -79.10943504075699195, 8.658331769851001170 ) ) ;
#24880 = DIRECTION ( 'NONE',  ( 1.000000000000000000, 0.000000000000000000, 0.000000000000000000 ) ) ;
#24881 = DIRECTION ( 'NONE',  ( 0.000000000000000000, -1.000000000000000000, 0.000000000000000000 ) ) ;
#24882 = CARTESIAN_POINT ( 'NONE',  ( 0.000000000000000000, -81.10000000285099020, 7.000000000000000000 ) ) ;
#24883 = CARTESIAN_POINT ( 'NONE',  ( -0.9352798328955729268, -82.27646447274652530, 1.232869141408684754 ) ) ;
#24884 = CARTESIAN_POINT ( 'NONE',  ( -0.4573940628493604055, -79.69555677089692836, -1.163073868470372974 ) ) ;
#24885 = AXIS2_PLACEMENT_3D ( 'NONE', #42429, #52157, #6695 ) ;
#24886 = CARTESIAN_POINT ( 'NONE',  ( -0.3926218265389189721, -78.00416666666666288, -1.460959015002473604 ) ) ;
#24887 = ORIENTED_EDGE ( 'NONE', *, *, #9038, .F. ) ;
#24888 = CARTESIAN_POINT ( 'NONE',  ( 1.667916687331000070, -23.29848884437999956, 12.49168451098999988 ) ) ;
#24889 = SURFACE_STYLE_FILL_AREA ( #56191 ) ;
#24890 = CARTESIAN_POINT ( 'NONE',  ( -12.83836862999999973, -23.20626272212999908, 2.062146390630000159 ) ) ;
#24891 = EDGE_LOOP ( 'NONE', ( #33678, #11405, #26033, #27270 ) ) ;
#24892 = EDGE_LOOP ( 'NONE', ( #39123, #22935, #14335, #7831 ) ) ;
#24893 = DIRECTION ( 'NONE',  ( 0.7592504785508701337, 0.04890181650104810651, 0.6489586451871740547 ) ) ;
#24894 = EDGE_LOOP ( 'NONE', ( #49139, #53096 ) ) ;
#24895 = ORIENTED_EDGE ( 'NONE', *, *, #11308, .F. ) ;
#24896 = CARTESIAN_POINT ( 'NONE',  ( 0.4065037703597895180, -80.99999999999997158, -10.96443877910777864 ) ) ;
#24897 = CARTESIAN_POINT ( 'NONE',  ( -10.82730428396000022, -77.08360301469699039, -1.394578048285000094 ) ) ;
#24898 = ITEM_DEFINED_TRANSFORMATION ( 'NONE', 'NONE', #31958,  #43526 ) ;
#24899 = DIRECTION ( 'NONE',  ( 1.000000000000000000, 0.000000000000000000, 0.000000000000000000 ) ) ;
#24901 = EDGE_CURVE ( 'NONE', #26739, #52133, #46891, .T. ) ;
#24900 = CARTESIAN_POINT ( 'NONE',  ( 9.557721383756000222, -78.48558667140099487, -2.621152531184999912 ) ) ;
#24902 = CARTESIAN_POINT ( 'NONE',  ( -5.706960677091378997, -79.42732870794154110, 7.378979574796262320 ) ) ;
#24903 = AXIS2_PLACEMENT_3D ( 'NONE', #12554, #38551, #25551 ) ;
#24904 = ORIENTED_EDGE ( 'NONE', *, *, #41779, .T. ) ;
#24906 = ADVANCED_FACE ( 'NONE', ( #29471 ), #21359, .T. ) ;
#24905 = VERTEX_POINT ( 'NONE', #38054 ) ;
#24907 = CARTESIAN_POINT ( 'NONE',  ( -9.139685035454183648, -77.58784146180079233, 1.423788756781738885 ) ) ;
#24908 = CARTESIAN_POINT ( 'NONE',  ( -12.00000000000000000, -76.89999999999999147, 0.000000000000000000 ) ) ;
#24909 = PRODUCT_DEFINITION_SHAPE ( 'NONE', 'NONE',  #39775 ) ;
#24910 = CARTESIAN_POINT ( 'NONE',  ( -12.77301895554999867, -61.85186686341000240, -1.052127376138000114 ) ) ;
#24911 = CARTESIAN_POINT ( 'NONE',  ( -9.022250383429000209, -78.86016145935799670, -3.573472734901999903 ) ) ;
#24912 = CARTESIAN_POINT ( 'NONE',  ( -9.491795480648855587, -79.40409383075655114, -0.5089449881589561686 ) ) ;
#24913 = CARTESIAN_POINT ( 'NONE',  ( -10.35747158362999976, -18.68415522710999710, 7.626500902215000544 ) ) ;
#24914 = CARTESIAN_POINT ( 'NONE',  ( 1.570796326794856590, -76.76458333333333428, 12.00000000000000711 ) ) ;
#24915 = CARTESIAN_POINT ( 'NONE',  ( 1.401632346086000069, -80.41793607721000114, -0.7415008327037999614 ) ) ;
#24916 = AXIS2_PLACEMENT_3D ( 'NONE', #15584, #28566, #27980 ) ;
#24917 = CARTESIAN_POINT ( 'NONE',  ( -0.5080623288857000208, -82.20492321929599200, -1.218433453902000085 ) ) ;
#24918 = EDGE_CURVE ( 'NONE', #16476, #18472, #9020, .T. ) ;
#24919 = CARTESIAN_POINT ( 'NONE',  ( -10.31444587876999996, -54.49924218061999426, 7.758886158083000417 ) ) ;
#24920 = CARTESIAN_POINT ( 'NONE',  ( 4.530904210857999992, -77.84363667140100063, 8.688217354640999091 ) ) ;
#24921 = CARTESIAN_POINT ( 'NONE',  ( -11.68767212001980127, -77.37916666666666288, 3.140974612311317138 ) ) ;
#24922 = CARTESIAN_POINT ( 'NONE',  ( 1.931043742978000077, -19.22204592323999961, -12.75763395699000036 ) ) ;
#24924 = CARTESIAN_POINT ( 'NONE',  ( -0.5995968343850351934, -82.21604462272937042, -1.140767552750202807 ) ) ;
#24923 = DIRECTION ( 'NONE',  ( -1.000000000000000000, 0.000000000000000000, 0.000000000000000000 ) ) ;
#24925 = CARTESIAN_POINT ( 'NONE',  ( -3.255604724290822816, -1.122525214333685240, -0.8495354805320418645 ) ) ;
#24926 = CARTESIAN_POINT ( 'NONE',  ( 4.029831046159999985, -78.47752942077299565, -10.51637221458999960 ) ) ;
#24927 = CARTESIAN_POINT ( 'NONE',  ( 12.00000000000000000, -60.04999999966999980, 0.000000000000000000 ) ) ;
#24928 = ORIENTED_EDGE ( 'NONE', *, *, #41163, .T. ) ;
#24929 = DIRECTION ( 'NONE',  ( 1.000000000000000000, 0.000000000000000000, 0.000000000000000000 ) ) ;
#24930 = DIRECTION ( 'NONE',  ( -1.000000000000000000, 0.000000000000000000, 0.000000000000000000 ) ) ;
#24931 = DIRECTION ( 'NONE',  ( 0.000000000000000000, -1.000000000000000000, 0.000000000000000000 ) ) ;
#24932 = CARTESIAN_POINT ( 'NONE',  ( -9.109442592336732147, -77.14879300455254452, -2.108685836323368257 ) ) ;
#24933 = CARTESIAN_POINT ( 'NONE',  ( 8.372594970691999094, -79.18436555618200146, 4.783109303148000535 ) ) ;
#24934 = CARTESIAN_POINT ( 'NONE',  ( -12.83677071375000089, -55.57261389723999656, 2.062839858856999609 ) ) ;
#24935 = CARTESIAN_POINT ( 'NONE',  ( 6.143730674703169470, -79.17034681202650859, 7.527261947263182762 ) ) ;
#24936 = CARTESIAN_POINT ( 'NONE',  ( 1.460729357734999789, -60.89091243169999501, 12.44211643244000065 ) ) ;
#24937 = CARTESIAN_POINT ( 'NONE',  ( -2.598917237794085455, -3.052083333333332593, -1.997276839918474600 ) ) ;
#24938 = CYLINDRICAL_SURFACE ( 'NONE', #35762, 10.75000000000000000 ) ;
#24939 = B_SPLINE_CURVE_WITH_KNOTS ( 'NONE', 3,
 ( #27465, #35149, #44616, #44320 ),
 .UNSPECIFIED., .F., .F.,
 ( 4, 4 ),
 ( 0.0008525611273306000007, 1.000000000000000000 ),
 .UNSPECIFIED. ) ;
#24940 = DIRECTION ( 'NONE',  ( 1.000000000000000000, 0.000000000000000000, 0.000000000000000000 ) ) ;
#24941 = CARTESIAN_POINT ( 'NONE',  ( -10.67331332832999991, -77.88867141381099657, -2.436207225683000299 ) ) ;
#24942 = VECTOR ( 'NONE', #14900, 1000.000000000000114 ) ;
#24943 = CARTESIAN_POINT ( 'NONE',  ( 6.327673118679000730, -77.31474813712100058, -9.036718833993001354 ) ) ;
#24944 = CARTESIAN_POINT ( 'NONE',  ( -0.9802155852345567633, -82.04731661387214103, 0.7777929719928468044 ) ) ;
#24945 = CARTESIAN_POINT ( 'NONE',  ( -0.6726658035522998791, -79.42188804861000051, -1.521367134781000052 ) ) ;
#24946 = CARTESIAN_POINT ( 'NONE',  ( 2.309272084855999996, -76.91403361972609787, -9.392260232199999948 ) ) ;
#24947 = DIRECTION ( 'NONE',  ( 0.000000000000000000, -1.000000000000000000, 0.000000000000000000 ) ) ;
#24948 = CARTESIAN_POINT ( 'NONE',  ( -1.359416874709192810E-05, -0.8285695117701413759, -3.421591653122290300 ) ) ;
#24949 = CARTESIAN_POINT ( 'NONE',  ( 1.310679582531385279, -81.29166666666668561, 0.7554284705563519831 ) ) ;
#24950 = ADVANCED_FACE ( 'NONE', ( #51362 ), #23265, .T. ) ;
#24951 = DIRECTION ( 'NONE',  ( 0.000000000000000000, -1.000000000000000000, 0.000000000000000000 ) ) ;
#24952 = CARTESIAN_POINT ( 'NONE',  ( -9.252740428349007118, -77.37916666666666288, 2.486604901413125734 ) ) ;
#24953 = CARTESIAN_POINT ( 'NONE',  ( 0.4713521909880000194, -78.93798672461099386, 12.02020425643999957 ) ) ;
#24954 = AXIS2_PLACEMENT_3D ( 'NONE', #58277, #30808, #22844 ) ;
#24955 = CARTESIAN_POINT ( 'NONE',  ( 2.486604901413132840, -78.65416666666668277, 9.252740428349005342 ) ) ;
#24956 = CARTESIAN_POINT ( 'NONE',  ( 0.000000000000000000, -2.660000000000000142, 0.000000000000000000 ) ) ;
#24957 = ORIENTED_EDGE ( 'NONE', *, *, #24005, .T. ) ;
#24958 = CARTESIAN_POINT ( 'NONE',  ( -1.980584515752000119, -23.26485146623999967, 12.76303204602000108 ) ) ;
#24959 = ORIENTED_EDGE ( 'NONE', *, *, #41832, .T. ) ;
#24960 = ORIENTED_EDGE ( 'NONE', *, *, #48454, .F. ) ;
#24961 = FACE_BOUND ( 'NONE', #24381, .T. ) ;
#24962 =( LENGTH_UNIT ( ) NAMED_UNIT ( * ) SI_UNIT ( .MILLI., .METRE. ) );
#24963 = CARTESIAN_POINT ( 'NONE',  ( 5.917523019358082337, -77.46666666666666856, -10.26699006316252394 ) ) ;
#24964 = CARTESIAN_POINT ( 'NONE',  ( 3.262642887984999795, -82.34119486992599946, -1.391544775636999853 ) ) ;
#24965 = CARTESIAN_POINT ( 'NONE',  ( 7.687192023495246218, -79.19968127005114411, 5.581541409190941216 ) ) ;
#24966 = ORIENTED_EDGE ( 'NONE', *, *, #49890, .F. ) ;
#24967 = CARTESIAN_POINT ( 'NONE',  ( 0.1572691907071377126, -82.73563599228513965, -1.240367807619981777 ) ) ;
#24968 = CARTESIAN_POINT ( 'NONE',  ( 13.90000000000005720, -72.79999999999999716, 0.000000000000000000 ) ) ;
#24970 = VERTEX_POINT ( 'NONE', #2638 ) ;
#24969 = ADVANCED_FACE ( 'NONE', ( #7056 ), #55785, .F. ) ;
#24971 = CARTESIAN_POINT ( 'NONE',  ( 6.929335342686214538, -79.74160298504301636, -6.198367606484551651 ) ) ;
#24972 = CARTESIAN_POINT ( 'NONE',  ( 1.108327923370202361, -78.43900460289381726, -1.059889875604768106 ) ) ;
#24973 = CARTESIAN_POINT ( 'NONE',  ( -0.4686848344790195964, -79.80000000000002558, -11.78742881352508753 ) ) ;
#24974 = CARTESIAN_POINT ( 'NONE',  ( -8.864498852882359614, -80.05242134712879931, 6.083669688407788101 ) ) ;
#24975 = CARTESIAN_POINT ( 'NONE',  ( -4.185964006270539883, -86.39318692614395445, -0.4007007872290511696 ) ) ;
#24976 = CARTESIAN_POINT ( 'NONE',  ( -8.075725583014000009, -76.39468836525099960, -7.736700848913999451 ) ) ;
#24977 = CARTESIAN_POINT ( 'NONE',  ( -6.579851013319285791, -79.78402246038903911, 7.149177186347576374 ) ) ;
#24978 = CARTESIAN_POINT ( 'NONE',  ( -8.325060287279862692, -77.30740476286068485, 4.923789656685126914 ) ) ;
#24979 = CIRCLE ( 'NONE', #12743, 13.86363636363999952 ) ;
#24980 = CARTESIAN_POINT ( 'NONE',  ( -1.423492296534000001, -76.27635696248199793, 11.02239954532999988 ) ) ;
#24981 = EDGE_CURVE ( 'NONE', #20866, #43667, #50632, .T. ) ;
#24982 = CARTESIAN_POINT ( 'NONE',  ( -2.851745628345378591, -78.70021968422466330, -8.800581811362720330 ) ) ;
#24983 = CARTESIAN_POINT ( 'NONE',  ( -1.120379678216000041, -79.22373702731300682, -0.7232983489183999470 ) ) ;
#24984 = AXIS2_PLACEMENT_3D ( 'NONE', #5577, #51062, #28005 ) ;
#24985 = DIRECTION ( 'NONE',  ( 0.9999999999995751176, 0.000000000000000000, 9.217554799814770620E-07 ) ) ;
#24986 = CARTESIAN_POINT ( 'NONE',  ( 0.2494208061600084736, -61.79288960742137249, -12.50614183116600842 ) ) ;
#24987 = CARTESIAN_POINT ( 'NONE',  ( 1.459331535918999778, -80.36553455456798645, -3.461461188124999921 ) ) ;
#24988 = CARTESIAN_POINT ( 'NONE',  ( 10.24033359635999929, -79.30459810362600592, 6.632096080123999648 ) ) ;
#24989 = CARTESIAN_POINT ( 'NONE',  ( 9.686447855663514517, -76.23750000000886473, 7.039619684793525067 ) ) ;
#24990 = DIRECTION ( 'NONE',  ( 1.000000000000000000, 0.000000000000000000, 0.000000000000000000 ) ) ;
#24991 = CARTESIAN_POINT ( 'NONE',  ( -13.63885489310999510, -56.01421830980998351, 7.254376133916000668 ) ) ;
#24992 = CARTESIAN_POINT ( 'NONE',  ( -3.299870502076000189, -84.66724735065199070, 1.294534069721999803 ) ) ;
#24993 = CARTESIAN_POINT ( 'NONE',  ( 1.217465845835393967, -80.27083333333332860, 0.3271848554491025851 ) ) ;
#24994 = CARTESIAN_POINT ( 'NONE',  ( 10.42272502865000128, -20.24546192895000019, 7.691893942754999713 ) ) ;
#24995 = CARTESIAN_POINT ( 'NONE',  ( -9.516272955320999927, -61.62538765589000178, -8.227498559458000571 ) ) ;
#24996 = CIRCLE ( 'NONE', #31588, 0.5000000000000004441 ) ;
#24997 = CARTESIAN_POINT ( 'NONE',  ( 1.243547092045927949, -78.26458333333332007, 9.500000000000003553 ) ) ;
#24998 = CARTESIAN_POINT ( 'NONE',  ( 0.8471236057751000414, -80.95456838452000170, 1.030027924806000028 ) ) ;
#24999 = CARTESIAN_POINT ( 'NONE',  ( 12.54238271613678890, -55.27146427614202651, 1.749799002657778324 ) ) ;
#25000 = CARTESIAN_POINT ( 'NONE',  ( 11.88928085110999966, -78.33531299227999511, 5.289737169833999886 ) ) ;
#25001 = CARTESIAN_POINT ( 'NONE',  ( -10.63212904442447559, -77.96514177923053524, -1.980916397344540281 ) ) ;
#25002 = CARTESIAN_POINT ( 'NONE',  ( 10.26636020442522934, -78.40548738728304556, -5.914272961825407293 ) ) ;
#25003 = CARTESIAN_POINT ( 'NONE',  ( -5.052420809101000088E-14, -80.84999999994218456, -13.94999999993999928 ) ) ;
#25004 = CARTESIAN_POINT ( 'NONE',  ( 1.413608202523000124, -75.94734000069999524, 12.28110795171000014 ) ) ;
#25005 = ORIENTED_EDGE ( 'NONE', *, *, #55153, .T. ) ;
#25006 = CARTESIAN_POINT ( 'NONE',  ( -0.3187246912203000049, -80.62725096977128203, 11.26088853021000169 ) ) ;
#25007 = CARTESIAN_POINT ( 'NONE',  ( 3.241578942234999872, -85.83735717367099483, -1.443243930775000239 ) ) ;
#25008 = CARTESIAN_POINT ( 'NONE',  ( 12.54901606610000009, -61.80731603467000213, 0.4733145588202999909 ) ) ;
#25009 = CARTESIAN_POINT ( 'NONE',  ( -12.34629048376999982, -79.26738212572000464, -1.838093833240000086 ) ) ;
#25010 = CARTESIAN_POINT ( 'NONE',  ( -7.601397897754999633, -55.55000000278000272, 10.07627163191000008 ) ) ;
#25011 = CARTESIAN_POINT ( 'NONE',  ( -7.068247108407000212, -79.01537169604299038, -6.380459158363000149 ) ) ;
#25012 = CARTESIAN_POINT ( 'NONE',  ( -1.374853770045000090, -81.36843355940999345, -0.7192078502473999713 ) ) ;
#25013 = CARTESIAN_POINT ( 'NONE',  ( 3.891476699446599241, -79.94576739355758832, 10.02177961226664671 ) ) ;
#25014 = CARTESIAN_POINT ( 'NONE',  ( 1.377412799619999850, -79.28562962141599257, 0.8425838727997000399 ) ) ;
#25015 = VERTEX_POINT ( 'NONE', #20345 ) ;
#25016 = EDGE_CURVE ( 'NONE', #46987, #29817, #58142, .T. ) ;
#25017 = FACE_OUTER_BOUND ( 'NONE', #58288, .T. ) ;
#25018 = CARTESIAN_POINT ( 'NONE',  ( 0.8528862836333073183, -78.91694510676077812, -3.387194058658217877 ) ) ;
#25019 = ORIENTED_EDGE ( 'NONE', *, *, #28832, .F. ) ;
#25020 = ADVANCED_FACE ( 'NONE', ( #10918, #33900 ), #6470, .F. ) ;
#25021 = CARTESIAN_POINT ( 'NONE',  ( 9.696433660856000003, -79.09672475065998754, 5.296892287724999981 ) ) ;
#25022 = LINE ( 'NONE', #51907, #19935 ) ;
#25023 = AXIS2_PLACEMENT_3D ( 'NONE', #51826, #21091, #24940 ) ;
#25024 = CARTESIAN_POINT ( 'NONE',  ( 0.9997866688655676626, -80.79871906944751458, -0.7680295045374020413 ) ) ;
#25025 = ORIENTED_EDGE ( 'NONE', *, *, #52887, .T. ) ;
#25026 = CARTESIAN_POINT ( 'NONE',  ( 12.06733228363000165, -78.49878287036499103, -1.536887159723000051 ) ) ;
#25027 = CARTESIAN_POINT ( 'NONE',  ( 5.605860879773000072, -77.45503136649999476, 9.963751779642000983 ) ) ;
#25028 = VECTOR ( 'NONE', #53512, 1000.000000000000000 ) ;
#25029 = ORIENTED_EDGE ( 'NONE', *, *, #40383, .F. ) ;
#25030 = ORIENTED_EDGE ( 'NONE', *, *, #56903, .F. ) ;
#25031 = CARTESIAN_POINT ( 'NONE',  ( -0.1782592318590009717, -80.48666753183738365, 1.238841185009283308 ) ) ;
#25032 = CARTESIAN_POINT ( 'NONE',  ( -3.380118193142000127, -86.40321104922298900, 1.504925578873999914 ) ) ;
#25033 = CARTESIAN_POINT ( 'NONE',  ( -9.699833017908000343, -79.50094660807849323, 1.146274062705999963 ) ) ;
#25034 = ORIENTED_EDGE ( 'NONE', *, *, #19630, .T. ) ;
#25035 = CARTESIAN_POINT ( 'NONE',  ( -12.74366183107908945, -23.52185227221844954, -1.980611001122017045 ) ) ;
#25036 = CARTESIAN_POINT ( 'NONE',  ( -6.155296265070999695, -78.65074028895499225, -9.015968826447998907 ) ) ;
#25037 = EDGE_LOOP ( 'NONE', ( #1817, #3459, #27496, #18361, #16018, #19828 ) ) ;
#25038 = CARTESIAN_POINT ( 'NONE',  ( -1.181111693982000110, -79.17654225787899236, -0.4092372983238000139 ) ) ;
#25039 = CARTESIAN_POINT ( 'NONE',  ( -2.205007487985999770, -76.90349415034600611, 9.235565851336001941 ) ) ;
#25040 = CARTESIAN_POINT ( 'NONE',  ( 7.660431561264000599, -55.60820826791000115, 10.01749754193999919 ) ) ;
#25041 = DIRECTION ( 'NONE',  ( 0.000000000000000000, -1.000000000000000000, 0.000000000000000000 ) ) ;
#25042 = CARTESIAN_POINT ( 'NONE',  ( 1.310679582531385501, -78.19166666666669130, 0.7554284705563518720 ) ) ;
#25043 = CARTESIAN_POINT ( 'NONE',  ( -11.75165102744716705, -77.20451201809390795, -0.7683522248362885110 ) ) ;
#25044 = CARTESIAN_POINT ( 'NONE',  ( -9.211739516216143286, -80.80159234348433017, 6.389716016208851990 ) ) ;
#25045 = CARTESIAN_POINT ( 'NONE',  ( 8.941518625654639507, -78.95754834277080647, 7.898890069118407631 ) ) ;
#25046 = EDGE_CURVE ( 'NONE', #26170, #7381, #16757, .T. ) ;
#25047 = CARTESIAN_POINT ( 'NONE',  ( -1.907247829674572071, -81.95677084859232764, -3.530101888956680423 ) ) ;
#25048 = CARTESIAN_POINT ( 'NONE',  ( -7.620037246293000166, -23.20567269824999812, 10.53559750859000133 ) ) ;
#25049 = EDGE_CURVE ( 'NONE', #47646, #58285, #21401, .T. ) ;
#25050 = CARTESIAN_POINT ( 'NONE',  ( 12.50000000000000000, -18.75000000310999937, -1.750000000000000000 ) ) ;
#25051 = CARTESIAN_POINT ( 'NONE',  ( 3.797573017451999711, -78.16306001420198868, 8.745505052098000220 ) ) ;
#25052 = CARTESIAN_POINT ( 'NONE',  ( 9.996770077891000028, -60.95065455317000414, -7.758602204140999881 ) ) ;
#25053 = CARTESIAN_POINT ( 'NONE',  ( 9.000511195990998914, -79.29077302305000785, 8.067084866081000172 ) ) ;
#25054 = CARTESIAN_POINT ( 'NONE',  ( -6.018890980713000438, -75.98186831501799077, 10.70471907396000155 ) ) ;
#25055 = CARTESIAN_POINT ( 'NONE',  ( 0.000000000000000000, 4.040000000000000036, 0.000000000000000000 ) ) ;
#25056 = CARTESIAN_POINT ( 'NONE',  ( 12.00000000000000000, -60.04999999966999980, -1.750000000000000000 ) ) ;
#25057 = CARTESIAN_POINT ( 'NONE',  ( -0.9995835529977249445, -78.55208333333330017, -0.7681833999686439318 ) ) ;
#25058 = AXIS2_PLACEMENT_3D ( 'NONE', #22988, #44840, #35970 ) ;
#25059 = ORIENTED_EDGE ( 'NONE', *, *, #8416, .F. ) ;
#25060 = CARTESIAN_POINT ( 'NONE',  ( 1.475564620878634159, -80.98274612424530972, -0.3262207497478352147 ) ) ;
#25061 = CARTESIAN_POINT ( 'NONE',  ( -8.168740699428001406, -77.41443535657099062, 4.831335699206999124 ) ) ;
#25062 = CARTESIAN_POINT ( 'NONE',  ( -0.7999999999999001243, -18.84999999997999964, -12.00000000000000000 ) ) ;
#25063 = DIRECTION ( 'NONE',  ( -1.000000000000000000, 0.000000000000000000, 0.000000000000000000 ) ) ;
#25064 = CARTESIAN_POINT ( 'NONE',  ( -0.4333679777835000024, -2.853257899543000242, 3.531240579163999804 ) ) ;
#25065 = AXIS2_PLACEMENT_3D ( 'NONE', #45561, #23105, #54115 ) ;
#25066 = CARTESIAN_POINT ( 'NONE',  ( -8.274737932560000786, -78.50660759103701025, -8.916907688993001457 ) ) ;
#25067 = CARTESIAN_POINT ( 'NONE',  ( 7.009066229391000213, -78.45973765814899537, -6.762594642477000484 ) ) ;
#25068 = EDGE_CURVE ( 'NONE', #49432, #23068, #14544, .T. ) ;
#25070 = CARTESIAN_POINT ( 'NONE',  ( -11.00000000000000000, -77.70953167777609849, -1.317564550621139752 ) ) ;
#25069 = CARTESIAN_POINT ( 'NONE',  ( -9.354514546012950404, -76.14787076493711027, 7.112430735605655308 ) ) ;
#25071 = CARTESIAN_POINT ( 'NONE',  ( 0.5343721329914999929, -82.29797985336999488, -1.367806479096000061 ) ) ;
#25072 = CARTESIAN_POINT ( 'NONE',  ( -9.961878266999939058, -79.56943413225670270, 4.040113604248548818 ) ) ;
#25073 = AXIS2_PLACEMENT_3D ( 'NONE', #31236, #30370, #26241 ) ;
#25074 = ORIENTED_EDGE ( 'NONE', *, *, #30799, .F. ) ;
#25075 = CARTESIAN_POINT ( 'NONE',  ( 5.894077591580000330, -76.71473343234410436, -10.80721126920999708 ) ) ;
#25076 = CARTESIAN_POINT ( 'NONE',  ( -9.424992723873112155, -79.26013535444967317, -1.207054387620474456 ) ) ;
#25077 = CARTESIAN_POINT ( 'NONE',  ( 6.290942473662262557, -79.73124999999996021, 10.26217848164658264 ) ) ;
#25078 = CARTESIAN_POINT ( 'NONE',  ( -8.798028344891999808, -61.73813495650999528, 8.790623041469000754 ) ) ;
#25079 = CARTESIAN_POINT ( 'NONE',  ( -10.41975891551938638, -80.07426127834554563, 3.525701440006863585 ) ) ;
#25080 = CARTESIAN_POINT ( 'NONE',  ( 8.565252427040000782, -79.29256405623699777, -4.245882144487000076 ) ) ;
#25081 = DIRECTION ( 'NONE',  ( -0.07798810297947010584, -0.04890180924492011638, 0.9957542211039013269 ) ) ;
#25082 = CARTESIAN_POINT ( 'NONE',  ( -12.72924182828835349, -55.02450359958543658, -1.930521792058781383 ) ) ;
#25083 = VERTEX_POINT ( 'NONE', #44809 ) ;
#25084 = CYLINDRICAL_SURFACE ( 'NONE', #354, 0.5000000000000006661 ) ;
#25085 = DIRECTION ( 'NONE',  ( -0.7071067811865475727, 0.000000000000000000, 0.7071067811865475727 ) ) ;
#25086 = CARTESIAN_POINT ( 'NONE',  ( 7.588757936995927963E-07, -80.21583927563050054, -10.98470495943546688 ) ) ;
#25087 = EDGE_CURVE ( 'NONE', #9344, #35383, #39498, .T. ) ;
#25088 = CARTESIAN_POINT ( 'NONE',  ( 0.7175553326157163569, -81.42660517918807273, 1.024974559415771536 ) ) ;
#25089 = CARTESIAN_POINT ( 'NONE',  ( 0.06739144895349272191, -78.77900521155609681, -1.272095446073437053 ) ) ;
#25090 = CARTESIAN_POINT ( 'NONE',  ( 0.9356112496015772662, -54.05892169590293861, -12.50329130245239639 ) ) ;
#25091 = CARTESIAN_POINT ( 'NONE',  ( 1.930989144707000005, -57.04634220890999785, -12.80900240956999880 ) ) ;
#25092 = B_SPLINE_CURVE_WITH_KNOTS ( 'NONE', 3,
 ( #7820, #3675, #43847, #21677, #42974, #56546, #57690, #2530, #34087, #11682, #52694, #57411, #21104, #2818, #47709, #25243, #20813, #39110 ),
 .UNSPECIFIED., .F., .F.,
 ( 4, 2, 2, 2, 2, 2, 2, 2, 4 ),
 ( 0.000000000000000000, 0.1249999999999999722, 0.2500000000000000000, 0.3750000000000000000, 0.5000000000000001110, 0.6250000000000001110, 0.7500000000000000000, 0.8750000000000000000, 1.000000000000000000 ),
 .UNSPECIFIED. ) ;
#25093 = CARTESIAN_POINT ( 'NONE',  ( 1.247385801071000166, -17.52277743742000027, -12.50301438876999960 ) ) ;
#25094 = B_SPLINE_SURFACE_WITH_KNOTS ( 'NONE', 3, 3, ( 
 ( #10020, #27998, #41595, #1175, #19164, #46338, #24466, #42478, #34963, #37744, #26397, #15605, #33599, #48574, #28877, #26116, #52993, #2616, #39695, #57702, #20612, #44418, #38614, #15895, #20048, #12542, #30540, #19749, #51638, #8116, #2047, #44137, #3685, #21687, #29169, #38036, #30824, #56342, #17257, #51921, #35247, #53278, #12824, #48858, #11192, #8400, #56058, #47215, #25036, #55767, #6744, #15313, #33307, #24754, #56629, #51342, #47509, #42770, #10901, #46923, #6451, #2331, #20326, #16979, #38322, #33881, #11479 ),
 ( #29451, #7036, #43057, #21972, #49450, #57997, #8998, #26982, #13409, #49146, #45016, #3970, #39983, #17553, #35545, #53573, #13111, #31105, #8696, #26687, #4272, #35846, #44718, #22268, #53875, #40284, #58295, #17857, #31407, #57605, #35151, #26015, #44041, #7449, #57898, #48761, #44322, #3591, #48475, #39601, #52900, #13013, #25734, #56756, #3024, #3878, #8598, #26584, #53472, #29863, #39315, #21022, #22171, #39027, #34584, #34296, #31012, #57039, #30726, #57324, #53184, #49050, #16598, #35441, #52615, #8019, #25448 ),
 ( #44618, #12732, #16888, #21877, #26307, #17455, #12166, #7734, #3312, #4174, #8307, #21596, #16315, #52330, #39885, #34869, #17165, #11885, #47917, #30152, #43469, #48203, #43761, #21306, #12449, #30444, #72, #9771, #45803, #49642, #22466, #50516, #18344, #5338, #13899, #41357, #939, #27760, #23345, #31599, #14187, #44911, #4468, #45505, #18921, #40479, #36916, #54926, #45210, #41066, #14480, #9482, #27173, #28050, #50224, #8893, #32470, #10069, #18637, #36629, #46095, #54648, #36042, #32184, #26887, #36334, #5621 ),
 ( #18051, #40179, #58192, #17755, #4759, #35742, #53773, #13309, #31303, #49346, #54067, #23050, #13603, #9188, #22761, #40770, #364, #54359, #31892, #49937, #27469, #5052, #652, #46972, #24509, #2094, #51391, #10947, #32763, #24800, #15650, #11236, #28928, #15364, #6499, #19798, #38369, #10656, #23632, #5912, #47261, #33930, #51968, #20375, #55218, #6205, #23921, #47557, #1510, #19499, #19214, #56391, #37494, #33647, #1801, #51687, #15941, #28635, #2378, #46685, #33358, #37792, #37207, #29502, #55812, #41645, #6794 ) ),
 .UNSPECIFIED., .F., .F., .F.,
 ( 4, 4 ),
 ( 4, 1, 1, 1, 1, 1, 1, 1, 1, 1, 1, 1, 1, 1, 1, 1, 1, 1, 1, 1, 1, 1, 1, 1, 1, 1, 1, 1, 1, 1, 1, 1, 1, 1, 1, 1, 1, 1, 1, 1, 1, 1, 1, 1, 1, 1, 1, 1, 1, 1, 1, 1, 1, 1, 1, 1, 1, 1, 1, 1, 1, 1, 1, 1, 4 ),
 ( -0.1772706441294000235, 1.177270644128999955 ),
 ( -0.02000000000000000042, -0.003749999999999999861, 0.01250000000000000069, 0.02875000000000000125, 0.04499999999999999833, 0.06124999999999999889, 0.07749999999999999944, 0.09375000000000000000, 0.1100000000000000006, 0.1262500000000000011, 0.1424999999999999878, 0.1587500000000000022, 0.1749999999999999889, 0.1912500000000000033, 0.2074999999999999900, 0.2237500000000000044, 0.2399999999999999911, 0.2562499999999999778, 0.2725000000000000200, 0.2887500000000000067, 0.3049999999999999933, 0.3212499999999999800, 0.3375000000000000222, 0.3537500000000000089, 0.3699999999999999956, 0.3862499999999999822, 0.4025000000000000244, 0.4187500000000000111, 0.4349999999999999978, 0.4512499999999999845, 0.4675000000000000266, 0.4837500000000000133, 0.5000000000000000000, 0.5162499999999999867, 0.5324999999999999734, 0.5487499999999999600, 0.5649999999999999467, 0.5812500000000000444, 0.5975000000000000311, 0.6137500000000000178, 0.6300000000000000044, 0.6462499999999999911, 0.6624999999999999778, 0.6787499999999999645, 0.6949999999999999512, 0.7112500000000000488, 0.7275000000000000355, 0.7437500000000000222, 0.7600000000000000089, 0.7762499999999999956, 0.7924999999999999822, 0.8087499999999999689, 0.8249999999999999556, 0.8412500000000000533, 0.8575000000000000400, 0.8737500000000000266, 0.8900000000000000133, 0.9062500000000000000, 0.9224999999999999867, 0.9387499999999999734, 0.9549999999999999600, 0.9712499999999999467, 0.9875000000000000444, 1.003749999999999920, 1.020000000000000018 ),
 .UNSPECIFIED. ) ;
#25095 = CARTESIAN_POINT ( 'NONE',  ( 9.233810704722001717, -79.74555105016035839, 5.933342942490105187 ) ) ;
#25096 = CYLINDRICAL_SURFACE ( 'NONE', #49789, 11.75000000000000000 ) ;
#25097 = ORIENTED_EDGE ( 'NONE', *, *, #30291, .F. ) ;
#25098 = VERTEX_POINT ( 'NONE', #12346 ) ;
#25099 = CARTESIAN_POINT ( 'NONE',  ( -0.6772390005816000258, -76.37953981538699111, -12.45222204340999994 ) ) ;
#25100 = CARTESIAN_POINT ( 'NONE',  ( -4.695314103947369588, -78.68919620935585613, -9.670285998753380241 ) ) ;
#25101 = B_SPLINE_CURVE_WITH_KNOTS ( 'NONE', 3,
 ( #765, #14590, #14296, #32290 ),
 .UNSPECIFIED., .F., .F.,
 ( 4, 4 ),
 ( 0.000000000000000000, 1.000000000000000000 ),
 .UNSPECIFIED. ) ;
#25102 = ORIENTED_EDGE ( 'NONE', *, *, #52449, .F. ) ;
#25103 = CARTESIAN_POINT ( 'NONE',  ( 9.395773752832997872, -17.29509747843999889, 8.188237371225000061 ) ) ;
#25104 = CARTESIAN_POINT ( 'NONE',  ( -11.00000000000000000, -77.69999999999998863, 0.000000000000000000 ) ) ;
#25105 = CARTESIAN_POINT ( 'NONE',  ( 1.318114156667296921, -54.06427522772043659, 12.70261578158577187 ) ) ;
#25106 = AXIS2_PLACEMENT_3D ( 'NONE', #7859, #3154, #43888 ) ;
#25107 = CARTESIAN_POINT ( 'NONE',  ( -9.134707332315000983, -77.73029308464001019, -8.964724163292999037 ) ) ;
#25108 = CONICAL_SURFACE ( 'NONE', #34526, 13.94999999997000018, 0.7853981633972997312 ) ;
#25109 = CARTESIAN_POINT ( 'NONE',  ( 9.250000000000000000, -79.74999999999998579, 1.907449677260999760E-14 ) ) ;
#25110 = DIRECTION ( 'NONE',  ( 0.000000000000000000, -1.000000000000000000, 0.000000000000000000 ) ) ;
#25111 = DIRECTION ( 'NONE',  ( 0.000000000000000000, -1.000000000000000000, 0.000000000000000000 ) ) ;
#25112 = CARTESIAN_POINT ( 'NONE',  ( 11.21665020278000036, -78.58438904619100640, 0.06973997782872000395 ) ) ;
#25113 =( GEOMETRIC_REPRESENTATION_CONTEXT ( 3 ) GLOBAL_UNCERTAINTY_ASSIGNED_CONTEXT ( ( #56717 ) ) GLOBAL_UNIT_ASSIGNED_CONTEXT ( ( #47884, #47601, #7416 ) ) REPRESENTATION_CONTEXT ( 'NONE', 'WORKASPACE' ) );
#25114 = VERTEX_POINT ( 'NONE', #17946 ) ;
#25115 = CARTESIAN_POINT ( 'NONE',  ( 7.678655902623765073, -55.00623020231258664, -10.03844298032646165 ) ) ;
#25116 = EDGE_LOOP ( 'NONE', ( #9282, #17323, #47064, #27572 ) ) ;
#25117 = CARTESIAN_POINT ( 'NONE',  ( 4.202209046443865503, -77.26254981315187820, -8.240357924581044102 ) ) ;
#25118 = CARTESIAN_POINT ( 'NONE',  ( -0.9462876233756999378, -80.18059372536998808, 0.9192961133846000443 ) ) ;
#25119 = CARTESIAN_POINT ( 'NONE',  ( 0.000000000000000000, -4.000000000000000000, 0.000000000000000000 ) ) ;
#25120 = CARTESIAN_POINT ( 'NONE',  ( 8.196767141791585942, -77.65970162848033453, 7.657324427439206715 ) ) ;
#25121 = CARTESIAN_POINT ( 'NONE',  ( -1.308462286196999891, -79.00516201241099168, 0.7661340681064999769 ) ) ;
#25122 = CARTESIAN_POINT ( 'NONE',  ( 0.000000000000000000, -75.15999999999999659, 0.000000000000000000 ) ) ;
#25123 = CARTESIAN_POINT ( 'NONE',  ( 10.74999999999999645, -80.76041666666665719, 1.407171709420451666 ) ) ;
#25124 = CARTESIAN_POINT ( 'NONE',  ( 1.136899222205000060, -79.20227971866999894, 1.164526648744999893 ) ) ;
#25125 = DIRECTION ( 'NONE',  ( -0.9999476293090542312, 0.000000000000000000, -0.01023418971888952027 ) ) ;
#25126 = CARTESIAN_POINT ( 'NONE',  ( 10.04848221952999943, -78.77718663188798587, 4.594115663639000147 ) ) ;
#25127 = CARTESIAN_POINT ( 'NONE',  ( -12.02912753549999891, -79.64943712227855599, 0.08506824670321999626 ) ) ;
#25128 = CARTESIAN_POINT ( 'NONE',  ( -7.674627477108999507, -56.04922971914000129, -10.14950121126000049 ) ) ;
#25129 = CARTESIAN_POINT ( 'NONE',  ( -2.266776927424000387, -84.50306218606498021, 2.728239737002000176 ) ) ;
#25130 = ORIENTED_EDGE ( 'NONE', *, *, #47250, .T. ) ;
#25131 = CARTESIAN_POINT ( 'NONE',  ( -8.157105063561195024, -77.20000000000001705, 7.261158152830655688 ) ) ;
#25132 = CARTESIAN_POINT ( 'NONE',  ( -1.321122997307999869, -79.84670880711999530, 0.8769429413327000100 ) ) ;
#25133 = CYLINDRICAL_SURFACE ( 'NONE', #330, 11.00000000000000000 ) ;
#25134 = CARTESIAN_POINT ( 'NONE',  ( 8.770451247185000909, -78.80795213214298656, 8.160602927202999624 ) ) ;
#25135 = CARTESIAN_POINT ( 'NONE',  ( -5.747123378374999980, -78.61567021304000491, 10.24856442990000005 ) ) ;
#25136 = CARTESIAN_POINT ( 'NONE',  ( 0.8344599933502094835, -78.06822408831668270, 0.9640149690932605653 ) ) ;
#25137 = CARTESIAN_POINT ( 'NONE',  ( 0.000000000000000000, -60.04999999966999980, -12.50000000000000000 ) ) ;
#25138 = CARTESIAN_POINT ( 'NONE',  ( -3.339615680726000235, -78.53295194988498906, 9.131854552393999569 ) ) ;
#25139 = CARTESIAN_POINT ( 'NONE',  ( 5.816771686847000744, -77.82035725226099032, -7.538935161885000014 ) ) ;
#25141 = EDGE_CURVE ( 'NONE', #24195, #51047, #29866, .T. ) ;
#25140 = CARTESIAN_POINT ( 'NONE',  ( 1.187590719512276793, -81.32127699930184406, -0.4706845472736139180 ) ) ;
#25142 = CARTESIAN_POINT ( 'NONE',  ( 9.605397716210999803, -77.23718443491598862, -5.187648860687999353 ) ) ;
#25143 = LINE ( 'NONE', #33991, #30907 ) ;
#25144 = CARTESIAN_POINT ( 'NONE',  ( -11.00000000000000000, -78.09999999999999432, 2.733298954964999989E-14 ) ) ;
#25145 = CARTESIAN_POINT ( 'NONE',  ( 1.226743013016005523, -80.87800081614069825, -0.3449182370377862905 ) ) ;
#25146 = ORIENTED_EDGE ( 'NONE', *, *, #9512, .F. ) ;
#25147 = CARTESIAN_POINT ( 'NONE',  ( 0.000000000000000000, -75.00000000000000000, 7.200000000000000178 ) ) ;
#25148 = CARTESIAN_POINT ( 'NONE',  ( 1.295048492659000017, -61.32893519093000378, -12.54716442239999985 ) ) ;
#25149 = DIRECTION ( 'NONE',  ( 0.000000000000000000, -1.000000000000000000, 0.000000000000000000 ) ) ;
#25150 = CARTESIAN_POINT ( 'NONE',  ( 10.79417609527999922, -77.49419007869299492, -3.050225076229999832 ) ) ;
#25151 = CARTESIAN_POINT ( 'NONE',  ( 9.694840914897000062, -79.58102073242298502, -5.145296513660000848 ) ) ;
#25152 = CARTESIAN_POINT ( 'NONE',  ( -1.306018640041678225, -79.39152295432234041, -0.7583383393078939605 ) ) ;
#25153 = CARTESIAN_POINT ( 'NONE',  ( -1.922652541418499839, -84.44270833512283048, 3.565982039631133471 ) ) ;
#25154 = CARTESIAN_POINT ( 'NONE',  ( 9.236131044632999831, -76.77029247776400211, -7.898064948592000256 ) ) ;
#25155 = FACE_OUTER_BOUND ( 'NONE', #20550, .T. ) ;
#25156 = CARTESIAN_POINT ( 'NONE',  ( -8.894916816534069071, -62.02809132899626121, 9.073484344827472015 ) ) ;
#25157 = ORIENTED_EDGE ( 'NONE', *, *, #37091, .F. ) ;
#25158 = CIRCLE ( 'NONE', #38333, 0.8000000000000011546 ) ;
#25159 = DIRECTION ( 'NONE',  ( -0.4045602622699926987, 0.8201597334568855313, 0.4045602622699926987 ) ) ;
#25160 = CARTESIAN_POINT ( 'NONE',  ( -1.378523866479640203, -75.79999999999999716, -11.70433083598206458 ) ) ;
#25161 = AXIS2_PLACEMENT_3D ( 'NONE', #14447, #46066, #50194 ) ;
#25162 = EDGE_CURVE ( 'NONE', #31399, #53636, #53418, .T. ) ;
#25163 = VECTOR ( 'NONE', #50141, 1000.000000000000000 ) ;
#25164 = CARTESIAN_POINT ( 'NONE',  ( 5.418544735220999442, -78.07770896256499782, 9.753510481391998610 ) ) ;
#25165 = CARTESIAN_POINT ( 'NONE',  ( 9.369164850722000892, -55.54999999966999980, 7.601397897754999633 ) ) ;
#25166 = CARTESIAN_POINT ( 'NONE',  ( -9.396085398178650294, -77.74791666666668277, 7.220923959705211281 ) ) ;
#25167 = CARTESIAN_POINT ( 'NONE',  ( -1.115142639999363361, -79.05850612728720250, 0.6526272847765023366 ) ) ;
#25168 = CIRCLE ( 'NONE', #19522, 1.000000000000000000 ) ;
#25169 = CARTESIAN_POINT ( 'NONE',  ( 0.5739046245057122242, -83.00524183610107798, -1.400512781010780916 ) ) ;
#25170 = CARTESIAN_POINT ( 'NONE',  ( -17.50000000000000000, -26.93717104351999936, -4.519587204488000183E-10 ) ) ;
#25171 = ORIENTED_EDGE ( 'NONE', *, *, #5001, .F. ) ;
#25172 = CARTESIAN_POINT ( 'NONE',  ( 2.062673488410000200, -23.32452273707999879, 12.82904109062999964 ) ) ;
#25173 = CARTESIAN_POINT ( 'NONE',  ( 0.000000000000000000, -0.2000000000000000111, 0.000000000000000000 ) ) ;
#25174 = ORIENTED_EDGE ( 'NONE', *, *, #53262, .F. ) ;
#25175 = VERTEX_POINT ( 'NONE', #57793 ) ;
#25176 = CARTESIAN_POINT ( 'NONE',  ( -12.65989785476000051, -53.85665906507999523, -0.9744897697748000631 ) ) ;
#25177 = ORIENTED_EDGE ( 'NONE', *, *, #41614, .T. ) ;
#25178 = VERTEX_POINT ( 'NONE', #43937 ) ;
#25179 = CARTESIAN_POINT ( 'NONE',  ( -5.773354541636604331, -81.00000000000004263, -9.267588486114398449 ) ) ;
#25180 = CARTESIAN_POINT ( 'NONE',  ( 6.261651594248000663, -77.24702107270799445, -8.942431733175999042 ) ) ;
#25181 = CONTEXT_DEPENDENT_SHAPE_REPRESENTATION ( #7779, #28155 ) ;
#25182 = CARTESIAN_POINT ( 'NONE',  ( 1.000000000000000000, -78.00000000000000000, -7.200000000000000178 ) ) ;
#25183 = CARTESIAN_POINT ( 'NONE',  ( 2.052412689622999942, -78.39848667140098826, -9.695776403646000574 ) ) ;
#25184 = CARTESIAN_POINT ( 'NONE',  ( -3.057959794837752820, -78.19827986707727518, -8.730403520994359567 ) ) ;
#25185 = CARTESIAN_POINT ( 'NONE',  ( -9.250000000000003553, -79.48961838684877534, 1.206747585507256249 ) ) ;
#25186 = B_SPLINE_CURVE_WITH_KNOTS ( 'NONE', 3,
 ( #17028, #11743, #43038, #38595, #30007, #47770, #16745, #20877, #34726, #38880, #56900, #16457, #48061, #44469, #17608, #9049, #31458, #50090, #48910, #26740, #4020, #54219, #14051, #53327, #53624, #13462, #9634, #22025, #27622, #36200, #45073, #22624, #230, #13753, #27035, #4624, #8451, #516, #49798, #45367, #40636, #4321, #44771, #58346, #9345, #49500, #40033, #32046, #18209, #30875, #31754, #45663, #58048, #4916, #22322, #35298, #27333, #22915, #5205, #40929, #18493, #17909, #23206, #35596, #36485, #57754, #54514, #17311, #12873, #13162, #26446, #31159, #40337, #49197, #8750, #35898, #53930, #37064, #50380, #50674, #29083, #19652, #28493, #801, #1960, #10808, #1369, #46544, #47128, #28788, #45955, #46834, #6361, #24076, #11103, #19365, #55964, #5486, #9927, #18784, #24377, #42389, #19953, #32621, #15218, #23491, #41504, #6068, #37942, #1089, #15515 ),
 .UNSPECIFIED., .F., .F.,
 ( 4, 2, 2, 2, 2, 2, 2, 2, 1, 1, 2, 2, 2, 2, 2, 2, 2, 2, 1, 1, 2, 2, 2, 2, 2, 2, 2, 1, 1, 1, 2, 2, 2, 2, 2, 2, 2, 1, 2, 2, 1, 1, 2, 2, 2, 2, 2, 2, 1, 2, 2, 2, 2, 1, 1, 1, 2, 1, 1, 1, 2, 2, 2, 4 ),
 ( 0.000000000000000000, 0.06250000000000904832, 0.1250000000000180966, 0.1562500000000226208, 0.1875000000000271450, 0.2187500000000316691, 0.2343750000000339173, 0.2421875000000350830, 0.2460937500000356937, 0.2480468750000359990, 0.2490234375000361655, 0.2500000000000363043, 0.2812500000000405231, 0.3125000000000447975, 0.3750000000000532352, 0.4375000000000616729, 0.4687500000000658917, 0.4843750000000680567, 0.4921875000000691669, 0.4960937500000696665, 0.4980468750000699441, 0.5000000000000701661, 0.5312500000000739409, 0.5625000000000774936, 0.5703125000000784928, 0.5712890625000786038, 0.5715332031250786038, 0.5717773437500787148, 0.5722656250000787148, 0.5742187500000786038, 0.5781250000000783817, 0.5937500000000774936, 0.6015625000000770495, 0.6054687500000769385, 0.6093750000000767164, 0.6250000000000760503, 0.6406250000000753841, 0.6425781250000753841, 0.6428222656250752731, 0.6430664062500752731, 0.6435546875000751621, 0.6445312500000749401, 0.6484375000000746070, 0.6562500000000736078, 0.6875000000000695000, 0.6953125000000685008, 0.6962890625000683897, 0.6972656250000682787, 0.6992187500000681677, 0.7031250000000677236, 0.7187500000000659472, 0.7226562500000655032, 0.7236328125000653921, 0.7246093750000651701, 0.7265625000000648370, 0.7343750000000638378, 0.7421875000000626166, 0.7460937500000620615, 0.7480468750000617284, 0.7490234375000617284, 0.7495117187500616174, 0.7500000000000616174, 0.8750000000000308642, 1.000000000000000000 ),
 .UNSPECIFIED. ) ;
#25187 = ORIENTED_EDGE ( 'NONE', *, *, #10059, .F. ) ;
#25188 = ORIENTED_EDGE ( 'NONE', *, *, #54032, .F. ) ;
#25189 = CARTESIAN_POINT ( 'NONE',  ( -5.446556518281947312, -77.52513256096960959, 7.476429722233334019 ) ) ;
#25190 = CARTESIAN_POINT ( 'NONE',  ( -12.70253258974437571, -24.97063167674132345, 0.9890392130068401677 ) ) ;
#25191 = EDGE_CURVE ( 'NONE', #1897, #11731, #8489, .T. ) ;
#25192 = AXIS2_PLACEMENT_3D ( 'NONE', #51869, #29690, #24985 ) ;
#25193 = LINE ( 'NONE', #7481, #55003 ) ;
#25194 = CARTESIAN_POINT ( 'NONE',  ( 1.882180247600000245, -78.68961848458398833, 9.519879562373999349 ) ) ;
#25195 = CARTESIAN_POINT ( 'NONE',  ( 4.606177061618105917, -86.17851881763701272, 0.5287147981155758680 ) ) ;
#25196 = CARTESIAN_POINT ( 'NONE',  ( 4.000000000000000000, -5.000000000000000000, -0.5999999999999999778 ) ) ;
#25197 = CARTESIAN_POINT ( 'NONE',  ( -10.47020627418439354, -76.52083333333334281, -2.813789756862263847 ) ) ;
#25198 = CARTESIAN_POINT ( 'NONE',  ( -11.11771682179999843, -80.29711170481299121, 1.751409206030000165 ) ) ;
#25199 = CARTESIAN_POINT ( 'NONE',  ( 1.585573224116000102, -81.04968570196999167, 0.6211121348122999875 ) ) ;
#25200 = CARTESIAN_POINT ( 'NONE',  ( -1.250000000000000000, -60.04999999966999980, 12.00000000000000000 ) ) ;
#25201 = CIRCLE ( 'NONE', #16699, 5.100000000000000533 ) ;
#25202 = CIRCLE ( 'NONE', #49757, 14.00000000000000000 ) ;
#25203 = CARTESIAN_POINT ( 'NONE',  ( -1.416867025158235149, -79.77826750275583834, -0.5258000735673173942 ) ) ;
#25204 = CARTESIAN_POINT ( 'NONE',  ( -0.6521978219530000231, -77.88718667140099683, 9.777264943591001511 ) ) ;
#25205 = CARTESIAN_POINT ( 'NONE',  ( 1.034214221880000141E-14, 0.2999999999999999334, 0.000000000000000000 ) ) ;
#25206 = CARTESIAN_POINT ( 'NONE',  ( 3.343750000583999960, -0.9062499994161000716, -3.925818329445000231E-08 ) ) ;
#25208 = CARTESIAN_POINT ( 'NONE',  ( 1.666698456700999920, -18.80818260160000222, -12.50018138921000066 ) ) ;
#25207 = DIRECTION ( 'NONE',  ( 0.000000000000000000, -1.000000000000000000, 0.000000000000000000 ) ) ;
#25209 = CARTESIAN_POINT ( 'NONE',  ( 2.486604901413172364, -78.94583333333333997, -9.252740428348998236 ) ) ;
#25210 = FACE_OUTER_BOUND ( 'NONE', #3888, .T. ) ;
#25211 = CARTESIAN_POINT ( 'NONE',  ( 1.250000000000000000, -18.75000000000000000, 12.00000000000000000 ) ) ;
#25212 = CYLINDRICAL_SURFACE ( 'NONE', #9062, 1.750000000000000000 ) ;
#25213 = ORIENTED_EDGE ( 'NONE', *, *, #20420, .T. ) ;
#25214 = DIRECTION ( 'NONE',  ( 0.000000000000000000, 1.000000000000000000, 0.000000000000000000 ) ) ;
#25215 = CARTESIAN_POINT ( 'NONE',  ( -12.89999999994999769, -2.999999999951000085, -1.886268936261000296E-09 ) ) ;
#25216 = CARTESIAN_POINT ( 'NONE',  ( -12.50386483992572195, -24.78505343634594382, 0.8574420492267335048 ) ) ;
#25217 = CARTESIAN_POINT ( 'NONE',  ( -9.309367086190000862, -77.13855160546319212, -0.1968645694141999969 ) ) ;
#25218 = CARTESIAN_POINT ( 'NONE',  ( -1.985556276454000235, -2.710628508794999725, -3.057679240689000100 ) ) ;
#25219 = CARTESIAN_POINT ( 'NONE',  ( 1.484562552624000054, -81.98291553004999344, -0.7558657512595999828 ) ) ;
#25220 = CARTESIAN_POINT ( 'NONE',  ( -1.861817488877999915, -80.00259998740499157, -9.461084334642999139 ) ) ;
#25222 = CARTESIAN_POINT ( 'NONE',  ( -12.82229880955999946, -55.37735182805000278, 2.065917129154000165 ) ) ;
#25221 = B_SPLINE_CURVE_WITH_KNOTS ( 'NONE', 3,
 ( #39309, #30440, #48470, #57599, #35146, #53178, #17749, #41060, #4753, #13893 ),
 .UNSPECIFIED., .F., .F.,
 ( 4, 2, 2, 2, 4 ),
 ( 0.000000000000000000, 0.2500000000000000000, 0.5000000000000000000, 0.7500000000000000000, 1.000000000000000000 ),
 .UNSPECIFIED. ) ;
#25223 = CARTESIAN_POINT ( 'NONE',  ( -3.936406751843953167, -79.25801478680048717, 8.883122821548814940 ) ) ;
#25224 = CARTESIAN_POINT ( 'NONE',  ( 1.500000000000000888, -80.23958333333334281, -0.1963495408493590444 ) ) ;
#25225 = DIRECTION ( 'NONE',  ( -0.7071067811865475727, 0.000000000000000000, 0.7071067811865475727 ) ) ;
#25226 = DIRECTION ( 'NONE',  ( -2.273759822993975071E-11, -5.531791025963690614E-21, 1.000000000000000000 ) ) ;
#25227 = EDGE_CURVE ( 'NONE', #51104, #46629, #1189, .T. ) ;
#25228 = CARTESIAN_POINT ( 'NONE',  ( 2.301294264262669476, -78.54828561723800817, 3.984678255335871278 ) ) ;
#25229 = CARTESIAN_POINT ( 'NONE',  ( 10.06241996419999829, -78.08858937446798620, -4.313003509706000216 ) ) ;
#25230 = EDGE_CURVE ( 'NONE', #26696, #1538, #36818, .T. ) ;
#25231 = CARTESIAN_POINT ( 'NONE',  ( 9.936789827135878994, -76.40459641371209898, -6.277323833409170106 ) ) ;
#25232 = CARTESIAN_POINT ( 'NONE',  ( 2.837175473061999575, -78.06338377657900196, 10.77984396480000129 ) ) ;
#25233 = CARTESIAN_POINT ( 'NONE',  ( -0.8918818467572275921, -82.03888351926970302, 0.8753769929997189392 ) ) ;
#25234 = CARTESIAN_POINT ( 'NONE',  ( -0.9554492926093999250, -78.75370921126000212, 1.361857491384999896 ) ) ;
#25235 = CARTESIAN_POINT ( 'NONE',  ( 9.208615812369000508, -76.98427752889628550, 2.957800710608999850 ) ) ;
#25236 = CARTESIAN_POINT ( 'NONE',  ( -1.460959015002474937, -78.97916666666664298, 0.3926218265389144757 ) ) ;
#25237 = CARTESIAN_POINT ( 'NONE',  ( 9.599999999916001059, -87.30000000008399752, -6.531555804621000072E-10 ) ) ;
#25238 = DIRECTION ( 'NONE',  ( 1.000000000000000000, 0.000000000000000000, 0.000000000000000000 ) ) ;
#25239 = VECTOR ( 'NONE', #37083, 1000.000000000000000 ) ;
#25240 = CARTESIAN_POINT ( 'NONE',  ( 7.711227883964345331, -79.91167364451388266, 7.535872567873190597 ) ) ;
#25241 = CARTESIAN_POINT ( 'NONE',  ( -1.780908991550280041, -79.96222016378874287, -11.07474478829885989 ) ) ;
#25242 = CARTESIAN_POINT ( 'NONE',  ( 11.92746894621999942, -79.32647392562900279, 1.562891678063999867 ) ) ;
#25243 = CARTESIAN_POINT ( 'NONE',  ( 1.217465845835393967, -81.77083333333330017, 0.3271848554491025851 ) ) ;
#25244 = EDGE_CURVE ( 'NONE', #13888, #47937, #1926, .T. ) ;
#25245 = CARTESIAN_POINT ( 'NONE',  ( 6.793663275700000170, -79.49993983499498995, -8.982210410292001512 ) ) ;
#25246 = CIRCLE ( 'NONE', #47852, 12.90000000000000036 ) ;
#25247 = ORIENTED_EDGE ( 'NONE', *, *, #7725, .T. ) ;
#25248 = CARTESIAN_POINT ( 'NONE',  ( 0.9935076047277175970, -24.96816187751455018, 12.70250268217055201 ) ) ;
#25249 = EDGE_LOOP ( 'NONE', ( #57078, #13618, #39941 ) ) ;
#25250 = ORIENTED_EDGE ( 'NONE', *, *, #12994, .F. ) ;
#25251 = CARTESIAN_POINT ( 'NONE',  ( -2.839805762151343949, -1.458333333333332815, 1.636761686205411737 ) ) ;
#25252 = CIRCLE ( 'NONE', #52557, 11.44999999999999929 ) ;
#25253 = VERTEX_POINT ( 'NONE', #45705 ) ;
#25254 = CARTESIAN_POINT ( 'NONE',  ( -3.541111988782999820, -80.24573954672798948, 0.1596783345572000135 ) ) ;
#25255 = CARTESIAN_POINT ( 'NONE',  ( 6.607089402419984658, -79.21351212151715515, 6.827904746749715592 ) ) ;
#25256 = VERTEX_POINT ( 'NONE', #5243 ) ;
#25257 = LINE ( 'NONE', #51851, #3527 ) ;
#25258 = CARTESIAN_POINT ( 'NONE',  ( 1.210822168571075386, -79.63541666666664298, -9.249999999999996447 ) ) ;
#25259 = ORIENTED_EDGE ( 'NONE', *, *, #5199, .F. ) ;
#25260 = CARTESIAN_POINT ( 'NONE',  ( -1.750000000001000089, -60.05000000958000328, -12.56594317859000043 ) ) ;
#25261 = CARTESIAN_POINT ( 'NONE',  ( -0.8109968711390208584, -78.17012475787373660, 1.272002705921249754 ) ) ;
#25262 = CARTESIAN_POINT ( 'NONE',  ( -0.006799328100487733902, -79.79999999999998295, 11.99550372483783889 ) ) ;
#25263 = EDGE_CURVE ( 'NONE', #47780, #11901, #27950, .T. ) ;
#25264 = CARTESIAN_POINT ( 'NONE',  ( -5.180360735014728490, -80.01521789024674547, 9.419592454460451236 ) ) ;
#25265 = DIRECTION ( 'NONE',  ( -0.7071067811865474617, 0.000000000000000000, -0.7071067811865474617 ) ) ;
#25266 = CARTESIAN_POINT ( 'NONE',  ( 0.4496812306607233523, -86.40321104920798234, -4.272713054705454816 ) ) ;
#25267 = CARTESIAN_POINT ( 'NONE',  ( 5.177752511601999785, -76.67058972713098797, 9.912858493839999952 ) ) ;
#25268 = CARTESIAN_POINT ( 'NONE',  ( 6.442726462082567274, -79.66713182735726662, 7.272994535396923865 ) ) ;
#25269 = CARTESIAN_POINT ( 'NONE',  ( -1.282582078921783664, -81.30480715895743060, 0.8019254487526868980 ) ) ;
#25270 = CARTESIAN_POINT ( 'NONE',  ( 7.945797842061000260, -76.70274997629699953, 7.770709007203000063 ) ) ;
#25271 = CARTESIAN_POINT ( 'NONE',  ( -8.283973254211803194, -78.63679031283243148, -4.116528973202782105 ) ) ;
#25272 = CARTESIAN_POINT ( 'NONE',  ( -0.6211595220380999871, -80.76172835212699397, -1.084739991049000096 ) ) ;
#25273 = DIRECTION ( 'NONE',  ( 0.7071067811865475727, 0.000000000000000000, 0.7071067811865475727 ) ) ;
#25274 = CARTESIAN_POINT ( 'NONE',  ( -0.01376364114532320840, -2.975804675509202912, 3.249696318060919076 ) ) ;
#25275 = CARTESIAN_POINT ( 'NONE',  ( -1.036694699304999912, -81.08703455456799247, 3.610626844383000300 ) ) ;
#25276 = EDGE_CURVE ( 'NONE', #8320, #12955, #10081, .T. ) ;
#25277 = CARTESIAN_POINT ( 'NONE',  ( 11.90625000002000000, -76.20625000001498961, 3.701036097655999965E-09 ) ) ;
#25278 = CARTESIAN_POINT ( 'NONE',  ( -13.97864847978000036, -33.03331574007000881, -0.0001086647257827000004 ) ) ;
#25279 = CARTESIAN_POINT ( 'NONE',  ( -12.99510751537000353, -52.49705297113997204, 6.911973076623003642 ) ) ;
#25280 = CARTESIAN_POINT ( 'NONE',  ( 0.2485007264108999858, -85.14824735065198524, -3.535988008354999934 ) ) ;
#25281 = CARTESIAN_POINT ( 'NONE',  ( -9.337502430872199000, -76.25149124130676626, -7.139128148582318367 ) ) ;
#25282 = CARTESIAN_POINT ( 'NONE',  ( 10.01332844637000008, -18.71943307332999851, 7.654537085030999499 ) ) ;
#25283 = CARTESIAN_POINT ( 'NONE',  ( -7.660411271065999728, -59.99173735459000056, -10.01752031416000044 ) ) ;
#25284 = LINE ( 'NONE', #43017, #53377 ) ;
#25285 = CARTESIAN_POINT ( 'NONE',  ( 10.35747158364999976, -60.11584477251999203, 7.626500902235000545 ) ) ;
#25286 = CARTESIAN_POINT ( 'NONE',  ( -1.066991882994506424, -79.06378521489916977, -1.111185832896742998 ) ) ;
#25287 = CARTESIAN_POINT ( 'NONE',  ( 9.175280770439000477, -76.70951328470999897, -8.221808909867000636 ) ) ;
#25288 = CARTESIAN_POINT ( 'NONE',  ( 9.931052045582879018, -24.12278631287863462, 7.764003813945582699 ) ) ;
#25289 = CIRCLE ( 'NONE', #44135, 9.250000000000000000 ) ;
#25290 = DIRECTION ( 'NONE',  ( -1.000000000000000000, 0.000000000000000000, 0.000000000000000000 ) ) ;
#25291 = CARTESIAN_POINT ( 'NONE',  ( -9.104818479629999572, -76.61049510581999300, 8.138539985441999747 ) ) ;
#25292 = ORIENTED_EDGE ( 'NONE', *, *, #42418, .F. ) ;
#25293 = EDGE_CURVE ( 'NONE', #16042, #37958, #23824, .T. ) ;
#25294 = DIRECTION ( 'NONE',  ( 1.000000000000000000, 0.000000000000000000, 0.000000000000000000 ) ) ;
#25295 = B_SPLINE_CURVE_WITH_KNOTS ( 'NONE', 3,
 ( #15802, #6062, #42385, #23487, #10506, #10211, #37650, #24072, #51542, #42672, #1956, #19949, #2240, #15511, #28190, #1085, #11387, #55664 ),
 .UNSPECIFIED., .F., .F.,
 ( 4, 2, 2, 2, 2, 2, 2, 2, 4 ),
 ( 0.000000000000000000, 0.1250000000000001665, 0.2500000000000002776, 0.3750000000000002776, 0.5000000000000002220, 0.6250000000000001110, 0.7500000000000001110, 0.8750000000000000000, 1.000000000000000000 ),
 .UNSPECIFIED. ) ;
#25296 = EDGE_CURVE ( 'NONE', #7601, #52710, #16694, .T. ) ;
#25297 = CARTESIAN_POINT ( 'NONE',  ( -10.98364301412004984, -18.76988149294739472, -0.5996551156055939247 ) ) ;
#25298 = CARTESIAN_POINT ( 'NONE',  ( 7.601397897754999633, -23.24999999758999536, -10.07627163191000008 ) ) ;
#25299 = CARTESIAN_POINT ( 'NONE',  ( -1.931087888240000217, -18.68415268018999953, -12.71658872085999903 ) ) ;
#25300 = CARTESIAN_POINT ( 'NONE',  ( 5.315453493860999856, -79.12906701255899122, -7.900401732693999257 ) ) ;
#25301 = CARTESIAN_POINT ( 'NONE',  ( 0.2050548769952000028, -85.83208224847899714, 4.167066004140999702 ) ) ;
#25302 = CARTESIAN_POINT ( 'NONE',  ( 5.221956912926488670, -79.93484039700992128, 9.402318417155663965 ) ) ;
#25303 = CARTESIAN_POINT ( 'NONE',  ( -0.6623784515263000383, -79.58330536170299752, -1.472572141918999877 ) ) ;
#25304 = ORIENTED_EDGE ( 'NONE', *, *, #41429, .T. ) ;
#25305 = LINE ( 'NONE', #43906, #8734 ) ;
#25306 = CARTESIAN_POINT ( 'NONE',  ( 2.627793897904080023, -78.98480243775595966, -2.477488290611707278 ) ) ;
#25307 = ORIENTED_EDGE ( 'NONE', *, *, #56554, .T. ) ;
#25308 = CARTESIAN_POINT ( 'NONE',  ( 10.90877671396000004, -78.62684575912199136, 0.8284967960653000230 ) ) ;
#25309 = CARTESIAN_POINT ( 'NONE',  ( -10.48774103545000003, -57.04527981721000174, 7.686941364801000098 ) ) ;
#25310 = EDGE_CURVE ( 'NONE', #14217, #48338, #51895, .T. ) ;
#25311 = CARTESIAN_POINT ( 'NONE',  ( -1.901143138367999974, -79.85477773487998832, -11.28240252173999991 ) ) ;
#25312 = ORIENTED_EDGE ( 'NONE', *, *, #20652, .F. ) ;
#25313 = CARTESIAN_POINT ( 'NONE',  ( 10.58601714202000110, -77.46786888426198914, -5.993221192758000804 ) ) ;
#25314 = EDGE_LOOP ( 'NONE', ( #51998, #26296, #26035, #27340, #46704 ) ) ;
#25315 = ORIENTED_EDGE ( 'NONE', *, *, #37529, .F. ) ;
#25316 = CIRCLE ( 'NONE', #58320, 0.5000000000000004441 ) ;
#25317 = B_SPLINE_CURVE_WITH_KNOTS ( 'NONE', 3,
 ( #43716, #26842, #21261, #44570, #21551, #7975 ),
 .UNSPECIFIED., .F., .F.,
 ( 4, 2, 4 ),
 ( 0.000000000000000000, 0.5000000000000000000, 1.000000000000000000 ),
 .UNSPECIFIED. ) ;
#25318 = CARTESIAN_POINT ( 'NONE',  ( 0.2421190662860195630, -80.45992770227913127, 1.227031503692224357 ) ) ;
#25319 = CARTESIAN_POINT ( 'NONE',  ( -7.217511925163520914, -78.12578035745170268, 9.390386475653141218 ) ) ;
#25320 = CARTESIAN_POINT ( 'NONE',  ( 8.193575559979001000, -79.30611065853049979, 5.316613930189999948 ) ) ;
#25321 = ORIENTED_EDGE ( 'NONE', *, *, #13697, .T. ) ;
#25322 = EDGE_LOOP ( 'NONE', ( #22200, #1822, #23659, #49508 ) ) ;
#25323 = CARTESIAN_POINT ( 'NONE',  ( -5.413301372347584461, -80.68336512517144854, -9.391811118427879634 ) ) ;
#25324 = CARTESIAN_POINT ( 'NONE',  ( -3.661088936265289195, -78.99318692614359350, -2.068643027229794651 ) ) ;
#25325 = CARTESIAN_POINT ( 'NONE',  ( 7.646966891740999195, -55.60358255701000019, 10.19019756604999927 ) ) ;
#25326 = AXIS2_PLACEMENT_3D ( 'NONE', #10389, #49677, #41097 ) ;
#25327 = CARTESIAN_POINT ( 'NONE',  ( 7.770365054039128694, -17.76417299472041122, -10.20675369723943859 ) ) ;
#25328 = CYLINDRICAL_SURFACE ( 'NONE', #36441, 1.750000000000001332 ) ;
#25329 = DIRECTION ( 'NONE',  ( 1.776356839400000238E-14, -1.000000000000000000, 6.231126725709000317E-14 ) ) ;
#25330 = CARTESIAN_POINT ( 'NONE',  ( -5.279679587742245772, -80.93583077350247379, -9.889870672231383608 ) ) ;
#25331 = CARTESIAN_POINT ( 'NONE',  ( -4.743879332790999825, -78.74260081536296241, -11.00053059214000051 ) ) ;
#25332 = CARTESIAN_POINT ( 'NONE',  ( 3.912590402935000267, -82.39999999999999147, -0.8316467632710000668 ) ) ;
#25333 = CARTESIAN_POINT ( 'NONE',  ( -7.974014308125999762, -24.63100890329999970, 9.929675091742998561 ) ) ;
#25334 = CARTESIAN_POINT ( 'NONE',  ( -4.014024930567999583, -78.67863830014491100, 0.5804966311653999567 ) ) ;
#25335 = EDGE_CURVE ( 'NONE', #41874, #22190, #11720, .T. ) ;
#25336 = CARTESIAN_POINT ( 'NONE',  ( 1.210822168571035418, -77.86458333333332860, 9.250000000000007105 ) ) ;
#25337 = DIRECTION ( 'NONE',  ( 0.7071067811865475727, 0.000000000000000000, -0.7071067811865475727 ) ) ;
#25338 = CARTESIAN_POINT ( 'NONE',  ( 11.03890801094999929, -78.66213151614000765, -5.342433469444999972 ) ) ;
#25339 = CARTESIAN_POINT ( 'NONE',  ( -1.750000000001000089, -60.04999998641999781, 12.56594318054000148 ) ) ;
#25340 = LINE ( 'NONE', #34185, #49703 ) ;
#25341 = CARTESIAN_POINT ( 'NONE',  ( 0.000000000000000000, -78.69999999999998863, 0.000000000000000000 ) ) ;
#25342 = FACE_OUTER_BOUND ( 'NONE', #39557, .T. ) ;
#25343 = CARTESIAN_POINT ( 'NONE',  ( 0.2749350294349880430, -79.88960586272550302, -1.486957691345828225 ) ) ;
#25344 = VECTOR ( 'NONE', #23444, 1000.000000000000227 ) ;
#25345 = CARTESIAN_POINT ( 'NONE',  ( 3.106054555984999688, -86.09999999999999432, -1.382904586457999851 ) ) ;
#25346 = CARTESIAN_POINT ( 'NONE',  ( 5.137083998358000336, -77.21100733245999947, -10.56753840748999984 ) ) ;
#25347 = CARTESIAN_POINT ( 'NONE',  ( -1.500000000000000000, -78.50000000000000000, 0.000000000000000000 ) ) ;
#25348 = CARTESIAN_POINT ( 'NONE',  ( -3.408418700480000396, -3.491675407298000078, -1.019786534199000005 ) ) ;
#25349 = CARTESIAN_POINT ( 'NONE',  ( -1.863462560416999869, -77.82837470544299663, 12.02123279331999939 ) ) ;
#25350 = CARTESIAN_POINT ( 'NONE',  ( 2.878019135186999922, -77.91968490469898256, -9.304660206797001010 ) ) ;
#25351 = CIRCLE ( 'NONE', #58360, 4.100000000000000533 ) ;
#25353 = CARTESIAN_POINT ( 'NONE',  ( 0.000000000000000000, -77.19999999999998863, 0.000000000000000000 ) ) ;
#25352 = CARTESIAN_POINT ( 'NONE',  ( -11.66824396372028971, -76.18874584464074928, 1.566409294560152654 ) ) ;
#25354 = CARTESIAN_POINT ( 'NONE',  ( 1.349879140156000190, -82.36113906847999999, -0.5781647238538999423 ) ) ;
#25355 = CARTESIAN_POINT ( 'NONE',  ( 2.273403379124000026E-14, -92.33215535459000023, 0.000000000000000000 ) ) ;
#25356 = EDGE_LOOP ( 'NONE', ( #1790, #49516, #37590, #36628, #32160, #43201, #43851, #24485, #3823, #40864 ) ) ;
#25357 = CARTESIAN_POINT ( 'NONE',  ( 1.384588047529715649, -78.76581540243206803, 11.96733435986141991 ) ) ;
#25358 = CARTESIAN_POINT ( 'NONE',  ( -9.480782379477998845, -79.31267994938899335, -7.608539354584999082 ) ) ;
#25359 = CARTESIAN_POINT ( 'NONE',  ( -6.339110262596877376, -79.18297630452198632, 7.102346778884022882 ) ) ;
#25360 = EDGE_CURVE ( 'NONE', #54154, #10368, #39210, .T. ) ;
#25361 = CARTESIAN_POINT ( 'NONE',  ( 2.580008266957357410, -80.00000000000000000, -9.145130960450376989 ) ) ;
#25362 = CARTESIAN_POINT ( 'NONE',  ( -8.958641849998000950, -62.00112647771999974, 8.950065109854000056 ) ) ;
#25363 = DIRECTION ( 'NONE',  ( 1.000000000000000000, 0.000000000000000000, 0.000000000000000000 ) ) ;
#25364 = CARTESIAN_POINT ( 'NONE',  ( -0.09919819565124000926, -79.89501551942399260, -9.890690074140000121 ) ) ;
#25365 = CARTESIAN_POINT ( 'NONE',  ( -7.374560639698973574, -77.97291666666664867, -9.596002108778167283 ) ) ;
#25366 = CARTESIAN_POINT ( 'NONE',  ( -2.421167930323333106, -79.10416666666664298, -9.009247259181917045 ) ) ;
#25367 = ORIENTED_EDGE ( 'NONE', *, *, #31084, .F. ) ;
#25368 = CARTESIAN_POINT ( 'NONE',  ( -1.963243971998659854, -76.46084546787545833, -11.01016897788577786 ) ) ;
#25369 = VECTOR ( 'NONE', #18737, 1000.000000000000000 ) ;
#25370 = CARTESIAN_POINT ( 'NONE',  ( 11.77866768790018703, -79.29209999548564269, -1.141178231376368091 ) ) ;
#25371 = CARTESIAN_POINT ( 'NONE',  ( -1.906106740367999874, -79.86568667140099365, -9.233453574281998755 ) ) ;
#25372 = CARTESIAN_POINT ( 'NONE',  ( -10.24996238029999951, -57.04828923575999511, -7.705119999435999567 ) ) ;
#25373 = CARTESIAN_POINT ( 'NONE',  ( -1.497546582071999977, -80.85273907906999113, 0.7298035716741000378 ) ) ;
#25374 = EDGE_CURVE ( 'NONE', #20090, #46623, #7549, .T. ) ;
#25375 = ORIENTED_EDGE ( 'NONE', *, *, #14208, .T. ) ;
#25376 = CARTESIAN_POINT ( 'NONE',  ( 12.70556836347999941, -16.77227722772000007, -1.774194455291999869E-09 ) ) ;
#25377 = CARTESIAN_POINT ( 'NONE',  ( 0.1638729951965073595, -82.23606986915045525, -1.249733270349860481 ) ) ;
#25378 = CARTESIAN_POINT ( 'NONE',  ( -7.644093100845077871, -23.52380578988463711, -10.09634101412614804 ) ) ;
#25379 = EDGE_CURVE ( 'NONE', #29440, #11048, #23637, .T. ) ;
#25380 = CARTESIAN_POINT ( 'NONE',  ( -9.393375537833518862, -78.55837579994272346, 5.413840788339419063 ) ) ;
#25381 = CARTESIAN_POINT ( 'NONE',  ( -7.479908383216000267, -79.26513030413099159, -6.281056869080000382 ) ) ;
#25382 = ORIENTED_EDGE ( 'NONE', *, *, #32927, .F. ) ;
#25383 = ORIENTED_EDGE ( 'NONE', *, *, #51117, .F. ) ;
#25384 = CARTESIAN_POINT ( 'NONE',  ( 7.323687853406999793, -76.65218057132500462, 10.23897242151999976 ) ) ;
#25385 = CARTESIAN_POINT ( 'NONE',  ( 2.100545712175502455, -78.74077999467331779, -10.54269051299135995 ) ) ;
#25386 = AXIS2_PLACEMENT_3D ( 'NONE', #29032, #11051, #42626 ) ;
#25387 = VERTEX_POINT ( 'NONE', #31605 ) ;
#25388 = CARTESIAN_POINT ( 'NONE',  ( 9.778561352719998823, -16.95143577368999743, 8.284566532398999428 ) ) ;
#25389 = DIRECTION ( 'NONE',  ( 1.000000000000000000, 0.000000000000000000, 0.000000000000000000 ) ) ;
#25391 = EDGE_CURVE ( 'NONE', #53569, #18786, #17612, .T. ) ;
#25390 = CIRCLE ( 'NONE', #40487, 9.599999999999999645 ) ;
#25392 = CARTESIAN_POINT ( 'NONE',  ( -0.6929804918870210440, -82.20905653057849349, -1.080747793140661717 ) ) ;
#25393 = CARTESIAN_POINT ( 'NONE',  ( 7.079708506942000490, -78.42792498495001041, -10.47296538612000028 ) ) ;
#25394 = CARTESIAN_POINT ( 'NONE',  ( 13.99609303101000002, -32.95862266598000190, 3.303296644036000229E-05 ) ) ;
#25395 = CARTESIAN_POINT ( 'NONE',  ( 12.50000000000000000, -63.73717104351998586, 0.000000000000000000 ) ) ;
#25396 = LINE ( 'NONE', #20118, #41731 ) ;
#25397 = CARTESIAN_POINT ( 'NONE',  ( 10.49311453041000064, -80.12294012156499434, -3.963918880051000126 ) ) ;
#25398 = CARTESIAN_POINT ( 'NONE',  ( 4.912554240050883259, -79.93092688505531385, 7.839266877745309614 ) ) ;
#25399 = ORIENTED_EDGE ( 'NONE', *, *, #46369, .F. ) ;
#25400 = B_SPLINE_CURVE_WITH_KNOTS ( 'NONE', 3,
 ( #9556, #27248, #45288, #4835 ),
 .UNSPECIFIED., .F., .F.,
 ( 4, 4 ),
 ( 0.000000000000000000, 1.000000000000000000 ),
 .UNSPECIFIED. ) ;
#25401 = CARTESIAN_POINT ( 'NONE',  ( -9.254388464354001087, -79.90752053325199711, 5.469807505829999528 ) ) ;
#25402 = EDGE_LOOP ( 'NONE', ( #42266, #33722, #16758, #48174 ) ) ;
#25403 = CARTESIAN_POINT ( 'NONE',  ( 1.728979404161999911, -78.48355279846498433, 11.13281482770999986 ) ) ;
#25404 = CARTESIAN_POINT ( 'NONE',  ( 8.871203788894485243, -77.32666406881654098, -2.694563217664684096 ) ) ;
#25405 = CARTESIAN_POINT ( 'NONE',  ( 0.9683804214594998738, -79.93253060846500091, -0.8959938446301999315 ) ) ;
#25406 = DIRECTION ( 'NONE',  ( 0.6489586469534662783, -0.04890178980865751007, -0.7592504787603602256 ) ) ;
#25407 = CARTESIAN_POINT ( 'NONE',  ( 9.669078507277122370, -77.14221111144533438, 5.685994177280137230 ) ) ;
#25408 = UNCERTAINTY_MEASURE_WITH_UNIT (LENGTH_MEASURE( 1.000000000000000082E-05 ), #48490, 'distance_accuracy_value', 'NONE');
#25410 = EDGE_CURVE ( 'NONE', #13850, #30955, #41320, .T. ) ;
#25409 = CARTESIAN_POINT ( 'NONE',  ( -1.403409243600000300, -78.61402008970900113, -0.2012507760191999950 ) ) ;
#25411 = CARTESIAN_POINT ( 'NONE',  ( -7.648026768036999989, -60.04999998387000204, -10.12290050219000115 ) ) ;
#25412 = AXIS2_PLACEMENT_3D ( 'NONE', #49144, #13994, #22861 ) ;
#25413 = FACE_OUTER_BOUND ( 'NONE', #13755, .T. ) ;
#25414 = CARTESIAN_POINT ( 'NONE',  ( 0.4102083068199999794, -78.47488455744999669, -1.574926093281000083 ) ) ;
#25415 = CARTESIAN_POINT ( 'NONE',  ( -12.53241208775999915, -19.23537109840999904, -1.667936697358999965 ) ) ;
#25416 = CARTESIAN_POINT ( 'NONE',  ( -1.166171049469810983, -79.12942819682623963, -0.4499060407731832467 ) ) ;
#25417 = EDGE_CURVE ( 'NONE', #38307, #56848, #33362, .T. ) ;
#25418 = CARTESIAN_POINT ( 'NONE',  ( -7.558619072263999428, -79.05811017521499195, -8.058856703501000140 ) ) ;
#25419 = CARTESIAN_POINT ( 'NONE',  ( 0.000000000000000000, -18.75000000000000000, 12.00000000000000000 ) ) ;
#25420 = CARTESIAN_POINT ( 'NONE',  ( 3.799999999999999822, -77.50000000000000000, 0.000000000000000000 ) ) ;
#25421 = CARTESIAN_POINT ( 'NONE',  ( -2.902481905820999852, -86.07258307901300043, 2.039564730455999619 ) ) ;
#25422 = ORIENTED_EDGE ( 'NONE', *, *, #44602, .F. ) ;
#25423 = CARTESIAN_POINT ( 'NONE',  ( 1.606311393998999915, -83.05309610059499903, -0.5653197666394998988 ) ) ;
#25424 = CARTESIAN_POINT ( 'NONE',  ( 0.3526082373300999939, -80.03618645244999641, -1.545983222067000007 ) ) ;
#25425 = DIRECTION ( 'NONE',  ( -1.000000000000000000, 0.000000000000000000, 0.000000000000000000 ) ) ;
#25426 = CARTESIAN_POINT ( 'NONE',  ( 9.789819849890999848, -78.69943487044800179, -6.904744247936999813 ) ) ;
#25427 = CARTESIAN_POINT ( 'NONE',  ( -12.70228859453985670, -17.17803615247013838, 1.213484947683437509 ) ) ;
#25428 = CARTESIAN_POINT ( 'NONE',  ( -0.4492251327744000156, -81.60790313063000667, 1.604198796042999753 ) ) ;
#25429 = CARTESIAN_POINT ( 'NONE',  ( 1.312589504071557833, -2.405348311454605259, -3.269350533498157407 ) ) ;
#25430 = CARTESIAN_POINT ( 'NONE',  ( -9.631455446501000495, -78.20110584965399880, -1.333735528292999906 ) ) ;
#25431 = CARTESIAN_POINT ( 'NONE',  ( -7.068247108407000212, -78.70149595525998620, -6.380459158363000149 ) ) ;
#25432 = CARTESIAN_POINT ( 'NONE',  ( 0.4638405057549351840, -81.25547559012920829, -1.160654197406111976 ) ) ;
#25433 = CARTESIAN_POINT ( 'NONE',  ( 0.5327216036087999429, -77.15547540590999631, -10.90374125898999935 ) ) ;
#25434 = CARTESIAN_POINT ( 'NONE',  ( 11.58635484046792641, -75.96315356379447792, 1.957992045167118667 ) ) ;
#25435 = CARTESIAN_POINT ( 'NONE',  ( -0.1360927073799415854, -80.76669044317051771, -1.267130688116418824 ) ) ;
#25436 = ORIENTED_EDGE ( 'NONE', *, *, #1215, .T. ) ;
#25437 = CARTESIAN_POINT ( 'NONE',  ( 1.210822168571035418, -78.86458333333334281, 9.250000000000007105 ) ) ;
#25438 = CARTESIAN_POINT ( 'NONE',  ( 10.48155006022000002, -79.62010969142899341, 6.381341495520000073 ) ) ;
#25439 = CARTESIAN_POINT ( 'NONE',  ( 3.914500761937000028, -78.48547955770028750, -1.429791614965258972E-15 ) ) ;
#25440 = CARTESIAN_POINT ( 'NONE',  ( 1.579899301681999990, -82.10529106903000240, 0.5283722218587000308 ) ) ;
#25441 = CARTESIAN_POINT ( 'NONE',  ( 6.718030245586000149, -79.04726600010199888, -8.679405866825000260 ) ) ;
#25442 = CARTESIAN_POINT ( 'NONE',  ( 9.934814764470999648, -24.62368287829000124, -7.968971842743999723 ) ) ;
#25443 = CARTESIAN_POINT ( 'NONE',  ( -9.416284655759811884, -80.42395833333223720, 5.426231776061239742 ) ) ;
#25444 = DIRECTION ( 'NONE',  ( 0.000000000000000000, -1.000000000000000000, 1.258252761242000063E-14 ) ) ;
#25445 = CARTESIAN_POINT ( 'NONE',  ( 0.1682664256278402770, -78.57055743907643830, 11.74683409834875825 ) ) ;
#25446 = DIRECTION ( 'NONE',  ( -3.675131323893999047E-09, -0.9999999999999997780, 2.168720883760999791E-08 ) ) ;
#25447 = ORIENTED_EDGE ( 'NONE', *, *, #16747, .T. ) ;
#25448 = CARTESIAN_POINT ( 'NONE',  ( -1.448527388915000103, -78.25544952233700258, -10.72114852740000046 ) ) ;
#25449 = CARTESIAN_POINT ( 'NONE',  ( -8.838834764832000701, -55.54999999966999980, -8.838834764832000701 ) ) ;
#25450 = LINE ( 'NONE', #38156, #45230 ) ;
#25451 = B_SPLINE_CURVE_WITH_KNOTS ( 'NONE', 3,
 ( #12440, #3581, #53459, #35142, #48190, #17746, #26297, #34571, #3867, #49338, #3302, #49039, #26005, #39015, #21867, #39875, #53763, #13002 ),
 .UNSPECIFIED., .F., .F.,
 ( 4, 2, 2, 2, 2, 2, 2, 2, 4 ),
 ( 0.000000000000000000, 0.1249999999999999722, 0.2499999999999999445, 0.3749999999999998890, 0.4999999999999998890, 0.6249999999999998890, 0.7499999999999997780, 0.8749999999999998890, 1.000000000000000000 ),
 .UNSPECIFIED. ) ;
#25452 = CARTESIAN_POINT ( 'NONE',  ( -7.805809014822999714, -79.61509741874499468, 8.123945268076997905 ) ) ;
#25453 = CARTESIAN_POINT ( 'NONE',  ( -12.71798269388000158, -60.09778754156999980, -1.931086388578000079 ) ) ;
#25454 = CARTESIAN_POINT ( 'NONE',  ( 10.98362417419999915, -18.84999999999999787, -0.5999999999999999778 ) ) ;
#25455 = CARTESIAN_POINT ( 'NONE',  ( 0.1633825985461731523, -78.96481209864140283, 1.249810919385931030 ) ) ;
#25456 = CIRCLE ( 'NONE', #57476, 1.200000000000000622 ) ;
#25457 = CARTESIAN_POINT ( 'NONE',  ( -1.227822524791635894, -82.29670828839515195, 0.9447229247095449978 ) ) ;
#25458 = CARTESIAN_POINT ( 'NONE',  ( -1.137583167366030601, -79.63440963302888065, -0.5175359492836348885 ) ) ;
#25459 = CIRCLE ( 'NONE', #11319, 13.86363636363999952 ) ;
#25460 = DIRECTION ( 'NONE',  ( 0.000000000000000000, 1.000000000000000000, 0.000000000000000000 ) ) ;
#25461 = FACE_OUTER_BOUND ( 'NONE', #23205, .T. ) ;
#25462 = ORIENTED_EDGE ( 'NONE', *, *, #47396, .F. ) ;
#25463 = VERTEX_POINT ( 'NONE', #47841 ) ;
#25464 = CARTESIAN_POINT ( 'NONE',  ( -12.54705919854999863, -54.26307476595999901, -1.287183453418999868 ) ) ;
#25465 = ORIENTED_EDGE ( 'NONE', *, *, #26429, .F. ) ;
#25466 = VERTEX_POINT ( 'NONE', #7372 ) ;
#25467 = CARTESIAN_POINT ( 'NONE',  ( -8.044069603293324988, -81.00000000000001421, -7.290586178141345464 ) ) ;
#25468 = CARTESIAN_POINT ( 'NONE',  ( -10.26277353288999983, -77.60109353173099578, -3.721672393288999903 ) ) ;
#25469 = ITEM_DEFINED_TRANSFORMATION ( 'NONE', 'NONE', #1821,  #43526 ) ;
#25470 = EDGE_CURVE ( 'NONE', #56311, #2750, #39318, .T. ) ;
#25471 = CARTESIAN_POINT ( 'NONE',  ( -3.255457669676000254, -78.29116332859899785, -9.242313942619999168 ) ) ;
#25472 = EDGE_CURVE ( 'NONE', #2048, #22633, #51110, .T. ) ;
#25473 = CARTESIAN_POINT ( 'NONE',  ( 10.49311453041000064, -79.91957446173628909, -3.963918880051000126 ) ) ;
#25474 = ORIENTED_EDGE ( 'NONE', *, *, #35530, .F. ) ;
#25475 = AXIS2_PLACEMENT_3D ( 'NONE', #8112, #18145, #44414 ) ;
#25476 = ORIENTED_EDGE ( 'NONE', *, *, #19611, .F. ) ;
#25477 = CARTESIAN_POINT ( 'NONE',  ( -5.786494162132466812, -77.52886857143271016, 7.216877617947186963 ) ) ;
#25478 = DIRECTION ( 'NONE',  ( 0.000000000000000000, -1.000000000000000000, 0.000000000000000000 ) ) ;
#25479 = CARTESIAN_POINT ( 'NONE',  ( 11.00000000000000000, -78.34999999999999432, 0.000000000000000000 ) ) ;
#25480 = CARTESIAN_POINT ( 'NONE',  ( -8.073459667400001649, -78.37695636416498246, -5.384232384047000330 ) ) ;
#25481 = FACE_OUTER_BOUND ( 'NONE', #12460, .T. ) ;
#25482 = FACE_OUTER_BOUND ( 'NONE', #51499, .T. ) ;
#25483 = CARTESIAN_POINT ( 'NONE',  ( 1.750000000001000089, -19.24899163674999869, 12.60354432393000046 ) ) ;
#25484 = CARTESIAN_POINT ( 'NONE',  ( -9.459258931978000717, -79.76813694385799636, 5.442530770145999952 ) ) ;
#25485 = EDGE_CURVE ( 'NONE', #31243, #36858, #48690, .T. ) ;
#25486 = CARTESIAN_POINT ( 'NONE',  ( -0.8477325451633000997, -79.28107020522999449, -1.148851298854000058 ) ) ;
#25487 = PLANE ( 'NONE',  #7294 ) ;
#25488 = CARTESIAN_POINT ( 'NONE',  ( -8.950130560535999535, -53.59887407320999841, 8.958576480190000524 ) ) ;
#25489 = CARTESIAN_POINT ( 'NONE',  ( 6.721258625739999992, -78.19203667140099867, -7.130431436203999773 ) ) ;
#25490 = CARTESIAN_POINT ( 'NONE',  ( -8.885616033064000163, -78.14317969841199840, 8.035041515002001589 ) ) ;
#25491 = CARTESIAN_POINT ( 'NONE',  ( -7.986982684666001475, -17.27364722735000058, -10.07612755993999976 ) ) ;
#25492 = CIRCLE ( 'NONE', #2882, 13.94827586206999825 ) ;
#25494 = DIRECTION ( 'NONE',  ( -0.6489586447325241814, -0.04890182339223182045, -0.7592504784956282116 ) ) ;
#25493 = CARTESIAN_POINT ( 'NONE',  ( 9.250000000000000000, -78.34999999999999432, 0.000000000000000000 ) ) ;
#25495 = AXIS2_PLACEMENT_3D ( 'NONE', #37427, #49867, #9411 ) ;
#25496 = CARTESIAN_POINT ( 'NONE',  ( 7.596835002782722057, -78.99791666666668277, -5.838193839761678383 ) ) ;
#25497 = CARTESIAN_POINT ( 'NONE',  ( -10.92178492054000039, -80.01025540420299365, -2.397173661657999943 ) ) ;
#25498 = CARTESIAN_POINT ( 'NONE',  ( 0.000000000000000000, -75.67500000000001137, 0.000000000000000000 ) ) ;
#25499 = ADVANCED_FACE ( 'NONE', ( #35076 ), #50301, .F. ) ;
#25500 = CARTESIAN_POINT ( 'NONE',  ( -11.26188033092999952, -77.82385718872900782, -0.06337168221170999538 ) ) ;
#25501 = CARTESIAN_POINT ( 'NONE',  ( 1.766902510613357569, -3.500000000000000444, 2.864370435608821985 ) ) ;
#25502 = CARTESIAN_POINT ( 'NONE',  ( -3.505293455996059127, -1.741927197408730921, 0.3622374202452205427 ) ) ;
#25503 = ORIENTED_EDGE ( 'NONE', *, *, #20905, .F. ) ;
#25504 = CARTESIAN_POINT ( 'NONE',  ( 10.75000000000000000, -80.25000000000000000, -1.651583051307000043E-14 ) ) ;
#25505 = EDGE_CURVE ( 'NONE', #26598, #50685, #42059, .T. ) ;
#25506 = DIRECTION ( 'NONE',  ( 0.000000000000000000, 1.000000000000000000, 0.000000000000000000 ) ) ;
#25507 = CARTESIAN_POINT ( 'NONE',  ( -12.60552511010000032, -18.71082276572999703, 1.799501877793999949 ) ) ;
#25508 = CARTESIAN_POINT ( 'NONE',  ( 3.250357114718000151, -1.764977233352999830, -1.258728819614999939 ) ) ;
#25509 = CARTESIAN_POINT ( 'NONE',  ( -0.4755896768997000534, -79.33590927173898422, 9.521775672420998760 ) ) ;
#25510 = CARTESIAN_POINT ( 'NONE',  ( -12.83838672487999943, -55.59401611997999737, 2.062170725306000207 ) ) ;
#25511 = LINE ( 'NONE', #40250, #31766 ) ;
#25512 = CARTESIAN_POINT ( 'NONE',  ( 2.061613410425999771, -60.00570014443000133, 12.83797036857999885 ) ) ;
#25513 = CARTESIAN_POINT ( 'NONE',  ( 0.000000000000000000, -79.50000000000000000, -9.499999999999953815 ) ) ;
#25514 = DIRECTION ( 'NONE',  ( -1.000000000000000000, 0.000000000000000000, 0.000000000000000000 ) ) ;
#25515 = CARTESIAN_POINT ( 'NONE',  ( -0.03763178688082682161, -78.62148118236265759, 3.992727112178280358 ) ) ;
#25516 = CARTESIAN_POINT ( 'NONE',  ( -10.05598257587000077, -77.40315636649998510, -4.328040802368000151 ) ) ;
#25517 = AXIS2_PLACEMENT_3D ( 'NONE', #27685, #54854, #36555 ) ;
#25518 = CARTESIAN_POINT ( 'NONE',  ( 9.746895442825083578, -76.40235638873841140, -6.561501312551729193 ) ) ;
#25519 = CARTESIAN_POINT ( 'NONE',  ( 10.90309719880000117, -76.87896664909099798, -1.680537371260999890 ) ) ;
#25520 = CARTESIAN_POINT ( 'NONE',  ( 1.225067527671359402, -81.86605588079059714, 0.2479480639099045647 ) ) ;
#25521 = CARTESIAN_POINT ( 'NONE',  ( -2.880544446985999762, -76.81021508244178619, -9.112186890989001142 ) ) ;
#25522 = CARTESIAN_POINT ( 'NONE',  ( -2.421167930323349982, -78.39583333333332860, 9.009247259181918821 ) ) ;
#25523 = CARTESIAN_POINT ( 'NONE',  ( 10.99999999999999645, -77.36041666666666572, 1.439896632895345974 ) ) ;
#25524 = CARTESIAN_POINT ( 'NONE',  ( -3.514441315269281940, -80.19895905850948736, -10.16027557698152428 ) ) ;
#25525 = EDGE_CURVE ( 'NONE', #49361, #19498, #17357, .T. ) ;
#25526 = DIRECTION ( 'NONE',  ( 0.000000000000000000, 1.000000000000000000, 0.000000000000000000 ) ) ;
#25527 = CARTESIAN_POINT ( 'NONE',  ( -10.71617508045257594, -79.82603844877975519, 3.314392947253207211 ) ) ;
#25528 = ORIENTED_EDGE ( 'NONE', *, *, #10383, .T. ) ;
#25529 = CARTESIAN_POINT ( 'NONE',  ( 0.4713521909880000194, -78.87019817133499089, 12.02020425643999957 ) ) ;
#25530 = CARTESIAN_POINT ( 'NONE',  ( 1.243547092045928615, -78.66458333333332575, 9.500000000000003553 ) ) ;
#25531 = CARTESIAN_POINT ( 'NONE',  ( 7.840078887343000069, -79.00968566096200618, -8.084993976410000727 ) ) ;
#25532 = FACE_OUTER_BOUND ( 'NONE', #47366, .T. ) ;
#25533 = ORIENTED_EDGE ( 'NONE', *, *, #42360, .T. ) ;
#25534 = AXIS2_PLACEMENT_3D ( 'NONE', #47631, #23479, #38733 ) ;
#25535 = ORIENTED_EDGE ( 'NONE', *, *, #18038, .F. ) ;
#25536 = ORIENTED_EDGE ( 'NONE', *, *, #40760, .T. ) ;
#25537 = AXIS2_PLACEMENT_3D ( 'NONE', #25725, #3013, #21009 ) ;
#25538 = FACE_OUTER_BOUND ( 'NONE', #58237, .T. ) ;
#25539 = ORIENTED_EDGE ( 'NONE', *, *, #6, .T. ) ;
#25540 = CARTESIAN_POINT ( 'NONE',  ( -3.024236528099000232, -80.12548912224700359, 1.849044269261000073 ) ) ;
#25541 = CARTESIAN_POINT ( 'NONE',  ( 1.832813866948703074, -79.25953808981230964, 9.323933791568595808 ) ) ;
#25542 = VERTEX_POINT ( 'NONE', #49873 ) ;
#25543 = CARTESIAN_POINT ( 'NONE',  ( 0.8653617893380854964, -82.78648746760886468, -0.9018584769693096526 ) ) ;
#25544 = ORIENTED_EDGE ( 'NONE', *, *, #57256, .F. ) ;
#25545 = CARTESIAN_POINT ( 'NONE',  ( 7.398464061248616552, -55.34839576620328927, -8.140250184779796783 ) ) ;
#25546 = ORIENTED_EDGE ( 'NONE', *, *, #53953, .F. ) ;
#25547 = CARTESIAN_POINT ( 'NONE',  ( -0.6256548411826953204, -79.51725861580031562, 1.084699083566985189 ) ) ;
#25548 = DIRECTION ( 'NONE',  ( 0.7071067811864970576, 3.544461080512985563E-08, -0.7071067811865970887 ) ) ;
#25549 = DIRECTION ( 'NONE',  ( 0.000000000000000000, 0.000000000000000000, 1.000000000000000000 ) ) ;
#25550 = CARTESIAN_POINT ( 'NONE',  ( -10.18724605009749773, -80.07418096558578213, 3.432876765056549484 ) ) ;
#25551 = DIRECTION ( 'NONE',  ( -1.000000000000000000, 0.000000000000000000, 0.000000000000000000 ) ) ;
#25552 = CARTESIAN_POINT ( 'NONE',  ( -3.378711645942461317, -86.36264282632897960, -2.358076299421792754 ) ) ;
#25553 = CARTESIAN_POINT ( 'NONE',  ( -5.007180289739999068, -76.81362410637399307, 10.00009952528999868 ) ) ;
#25554 = CARTESIAN_POINT ( 'NONE',  ( -3.299302781710000243, -77.40086001149001049, 12.69174137596000129 ) ) ;
#25555 = EDGE_CURVE ( 'NONE', #22104, #12731, #54863, .T. ) ;
#25556 = CARTESIAN_POINT ( 'NONE',  ( -2.935661446561999899, -79.50000000000000000, -9.035036904803998681 ) ) ;
#25557 = CARTESIAN_POINT ( 'NONE',  ( -10.67862928275000023, -76.94605063463400541, 1.734397297249000047 ) ) ;
#25558 = CARTESIAN_POINT ( 'NONE',  ( -9.230872287500126561, -78.60521422558908000, -0.6021493626502718577 ) ) ;
#25559 = CIRCLE ( 'NONE', #148, 0.5000000000000004441 ) ;
#25560 = CARTESIAN_POINT ( 'NONE',  ( -0.2976639488673999967, -79.61479940856000326, 1.299989344602000108 ) ) ;
#25561 = CARTESIAN_POINT ( 'NONE',  ( 7.601397897754999633, -55.55000000209000177, 10.07627163191000008 ) ) ;
#25562 = CARTESIAN_POINT ( 'NONE',  ( 2.471377992193831474, -2.907507802367013561, 2.123914601439464533 ) ) ;
#25563 = CARTESIAN_POINT ( 'NONE',  ( 2.111856289087000071, -79.23980496681159025, -2.849846186231000278 ) ) ;
#25564 = CARTESIAN_POINT ( 'NONE',  ( -2.281880833369933193, -77.99216318363434652, 10.50503500748997254 ) ) ;
#25565 = CARTESIAN_POINT ( 'NONE',  ( 1.151824538291304378, -82.88178188827541248, 0.4855375567635726308 ) ) ;
#25566 = CARTESIAN_POINT ( 'NONE',  ( 3.088413591160000138, -85.56019503318798058, 1.744494700727000192 ) ) ;
#25567 = CARTESIAN_POINT ( 'NONE',  ( -2.963791440107999886, -3.263363938828000244, 2.387889716789000083 ) ) ;
#25568 = CARTESIAN_POINT ( 'NONE',  ( 10.53003236233000095, -23.32452273707999879, 7.612971540276999960 ) ) ;
#25569 = CARTESIAN_POINT ( 'NONE',  ( -8.870414881026999154, -61.86963060230000622, -8.878264461126001095 ) ) ;
#25570 = EDGE_CURVE ( 'NONE', #37791, #5068, #44147, .T. ) ;
#25571 = DIRECTION ( 'NONE',  ( 0.7071067811865474617, 0.000000000000000000, 0.7071067811865474617 ) ) ;
#25572 = CARTESIAN_POINT ( 'NONE',  ( 1.221474390223999951, -81.39524338914699797, -0.5353283698298000326 ) ) ;
#25573 = CARTESIAN_POINT ( 'NONE',  ( -0.9218200799623714747, -80.47291666666669130, -1.199500263597270466 ) ) ;
#25574 = CARTESIAN_POINT ( 'NONE',  ( -3.346450045594000056, -76.94769696823999539, 12.57540552286999791 ) ) ;
#25575 = VECTOR ( 'NONE', #14703, 1000.000000000000114 ) ;
#25576 = CARTESIAN_POINT ( 'NONE',  ( -10.44304457033000055, -78.28465421611399222, 3.377400876517000050 ) ) ;
#25577 = CARTESIAN_POINT ( 'NONE',  ( -9.497876546326999403, -77.35168256874098347, -0.2008509664869000122 ) ) ;
#25578 = CARTESIAN_POINT ( 'NONE',  ( 10.53066010801000019, -75.87533071877999191, 6.475268442873999497 ) ) ;
#25579 = ORIENTED_EDGE ( 'NONE', *, *, #58126, .T. ) ;
#25580 = CARTESIAN_POINT ( 'NONE',  ( -5.059370734576000395, -80.83793477179669651, -10.06538451635999998 ) ) ;
#25581 = B_SPLINE_CURVE_WITH_KNOTS ( 'NONE', 3,
 ( #30021, #48076, #3189, #57195, #52200, #20609 ),
 .UNSPECIFIED., .F., .F.,
 ( 4, 2, 4 ),
 ( 0.000000000000000000, 0.5000000000000000000, 1.000000000000000000 ),
 .UNSPECIFIED. ) ;
#25582 = FACE_OUTER_BOUND ( 'NONE', #31145, .T. ) ;
#25583 = CARTESIAN_POINT ( 'NONE',  ( 0.3526813275444999896, -81.09526194714700864, 1.262314098292000031 ) ) ;
#25584 = CARTESIAN_POINT ( 'NONE',  ( -9.018516758304000902, -79.14420186241999033, -9.073560724760000085 ) ) ;
#25585 = CARTESIAN_POINT ( 'NONE',  ( -1.931087888049999979, -23.31584477285000290, -12.71658889741999943 ) ) ;
#25586 = CARTESIAN_POINT ( 'NONE',  ( 9.085337660295000006, -78.73113340475299538, 2.850792140868000146 ) ) ;
#25587 = CARTESIAN_POINT ( 'NONE',  ( -1.733974900253999918, -82.87075447013299367, 3.797754351674999640 ) ) ;
#25588 = DIRECTION ( 'NONE',  ( 0.000000000000000000, 1.000000000000000000, 0.000000000000000000 ) ) ;
#25589 = CARTESIAN_POINT ( 'NONE',  ( -0.7520647764090000464, -80.57555782932399779, -1.313341758254999991 ) ) ;
#25590 = EDGE_CURVE ( 'NONE', #36999, #35854, #40240, .T. ) ;
#25591 = VERTEX_POINT ( 'NONE', #18858 ) ;
#25592 = CARTESIAN_POINT ( 'NONE',  ( 5.099999999822000696, -75.20000000017779485, -7.534001399281000208E-10 ) ) ;
#25593 = CARTESIAN_POINT ( 'NONE',  ( -7.367791399714448630, -79.04847752305433062, 5.626431170726755582 ) ) ;
#25594 = CARTESIAN_POINT ( 'NONE',  ( -3.399999999999718359, -78.72609999968184979, 6.799999999999395861 ) ) ;
#25595 = ORIENTED_EDGE ( 'NONE', *, *, #47283, .F. ) ;
#25596 = CARTESIAN_POINT ( 'NONE',  ( -7.655192530954000318, -79.74284890031098882, 7.967190206674000130 ) ) ;
#25597 = CARTESIAN_POINT ( 'NONE',  ( -7.892048199455462765, -55.05053022673563845, -7.664266801485842606 ) ) ;
#25598 = CARTESIAN_POINT ( 'NONE',  ( -11.19194202533000038, -80.29450396371099430, 1.763102137848999940 ) ) ;
#25599 = ORIENTED_EDGE ( 'NONE', *, *, #21420, .F. ) ;
#25600 = CIRCLE ( 'NONE', #198, 9.199999999999999289 ) ;
#25601 = ORIENTED_EDGE ( 'NONE', *, *, #20439, .T. ) ;
#25602 = EDGE_LOOP ( 'NONE', ( #26843, #44057, #2468, #13774 ) ) ;
#25603 = CARTESIAN_POINT ( 'NONE',  ( 0.7926223457823362573, -80.42074650411231573, 0.9670736177117366106 ) ) ;
#25604 = CARTESIAN_POINT ( 'NONE',  ( 5.919062813527654399, -78.03099449878986604, 10.27295981138281356 ) ) ;
#25605 = CARTESIAN_POINT ( 'NONE',  ( 9.630577183392999174, -79.39349084372300069, 1.628483183780000010 ) ) ;
#25606 = EDGE_LOOP ( 'NONE', ( #1373, #47349, #41878 ) ) ;
#25607 = CARTESIAN_POINT ( 'NONE',  ( 12.43646312217999927, -53.87951485525000095, 0.1257251053154000153 ) ) ;
#25608 = ORIENTED_EDGE ( 'NONE', *, *, #19623, .T. ) ;
#25609 = CIRCLE ( 'NONE', #53911, 5.299999999999999822 ) ;
#25610 = CARTESIAN_POINT ( 'NONE',  ( 0.8763811889879414840, -79.33555707640819321, -0.9249508082997421887 ) ) ;
#25611 = CARTESIAN_POINT ( 'NONE',  ( -2.127490919130949454, -78.96264282632948550, -3.528455608958080525 ) ) ;
#25612 = AXIS2_PLACEMENT_3D ( 'NONE', #1669, #5784, #6951 ) ;
#25613 = CARTESIAN_POINT ( 'NONE',  ( 7.762982794220000038, -54.63910040255000666, 9.991998894170999179 ) ) ;
#25614 = PLANE ( 'NONE',  #26081 ) ;
#25615 = CARTESIAN_POINT ( 'NONE',  ( 13.99999999961999819, -72.70000000038000110, -1.691901775850999968E-09 ) ) ;
#25616 = CARTESIAN_POINT ( 'NONE',  ( 11.59999999999999964, -87.70000000000000284, 0.000000000000000000 ) ) ;
#25617 = EDGE_CURVE ( 'NONE', #10344, #24467, #3454, .T. ) ;
#25618 = CARTESIAN_POINT ( 'NONE',  ( -10.77837019794128182, -80.37202936742626491, -3.084047917684326290 ) ) ;
#25619 = CARTESIAN_POINT ( 'NONE',  ( -8.148905501844001975, -78.71547149993911319, -8.781309899900000104 ) ) ;
#25620 = DIRECTION ( 'NONE',  ( -3.788638658030000158E-11, 1.000000000000000000, 0.000000000000000000 ) ) ;
#25621 = ADVANCED_FACE ( 'NONE', ( #301 ), #36121, .F. ) ;
#25622 = CARTESIAN_POINT ( 'NONE',  ( -12.22985280536000019, -76.45708432191999293, -1.402219185755000153 ) ) ;
#25623 = CARTESIAN_POINT ( 'NONE',  ( -2.067110633960000055, -79.96757046129098967, 3.624030731625000001 ) ) ;
#25624 = CARTESIAN_POINT ( 'NONE',  ( 7.624341766629000539, -55.53514853726999689, -10.42531125022999916 ) ) ;
#25625 = CARTESIAN_POINT ( 'NONE',  ( -0.7681833999686477066, -83.42708333333331439, 0.9995835529977223910 ) ) ;
#25626 = CARTESIAN_POINT ( 'NONE',  ( 6.688645397968000950, -78.81176105510999719, 10.27915892414000076 ) ) ;
#25627 = CARTESIAN_POINT ( 'NONE',  ( -1.984586691443999795, -75.95454648948098964, 11.75553522549000007 ) ) ;
#25628 = CARTESIAN_POINT ( 'NONE',  ( -4.784380313523575623, -78.81666666666669130, 8.300970689365433586 ) ) ;
#25629 = LINE ( 'NONE', #52508, #53098 ) ;
#25630 = EDGE_CURVE ( 'NONE', #19148, #3745, #14777, .T. ) ;
#25631 = CARTESIAN_POINT ( 'NONE',  ( 1.179653558262802049, -81.05359780786231738, 0.9428567377702261609 ) ) ;
#25632 = CARTESIAN_POINT ( 'NONE',  ( 12.72394223973000038, -60.02159774832999517, -1.930881086224999876 ) ) ;
#25633 = CARTESIAN_POINT ( 'NONE',  ( 0.000000000000000000, -32.88214388149999934, 0.000000000000000000 ) ) ;
#25634 = CARTESIAN_POINT ( 'NONE',  ( 12.00000000000000000, -78.64999999999999147, 0.000000000000000000 ) ) ;
#25635 = CARTESIAN_POINT ( 'NONE',  ( -3.342386390799999774, -1.861752247163000140, 0.8450881718492999628 ) ) ;
#25636 = CARTESIAN_POINT ( 'NONE',  ( -7.209427067528999977, -77.43490340765200131, 9.655047023863000177 ) ) ;
#25637 = CARTESIAN_POINT ( 'NONE',  ( 12.56594317823000040, -18.74999998606000062, 1.750000000000000000 ) ) ;
#25639 = CARTESIAN_POINT ( 'NONE',  ( -1.100846539600000007, -79.28247803031800345, -0.6190985795237999856 ) ) ;
#25638 = CARTESIAN_POINT ( 'NONE',  ( -10.40284373066038803, -75.80000000000003979, 5.607632974479940025 ) ) ;
#25640 = CARTESIAN_POINT ( 'NONE',  ( 1.424157265477999923, -82.99288869324199425, 0.6972603243668999973 ) ) ;
#25641 = CARTESIAN_POINT ( 'NONE',  ( -10.57143388931192263, -79.58561314518549068, 1.950965474043120151 ) ) ;
#25642 = ORIENTED_EDGE ( 'NONE', *, *, #5762, .F. ) ;
#25643 = CARTESIAN_POINT ( 'NONE',  ( -1.250000000000000000, -81.99999999999998579, 0.000000000000000000 ) ) ;
#25644 = CARTESIAN_POINT ( 'NONE',  ( 1.328997109577999991, -79.39258084193100728, -12.08341310737000107 ) ) ;
#25645 = CARTESIAN_POINT ( 'NONE',  ( -9.478081404219775408, -79.25540238611779387, -0.6444716196238855499 ) ) ;
#25646 = CARTESIAN_POINT ( 'NONE',  ( 11.88845611680340220, -79.66250000000000853, 1.884907306722996445 ) ) ;
#25647 = CARTESIAN_POINT ( 'NONE',  ( -7.986976573832000881, -61.52634345601000376, 10.07613380459999952 ) ) ;
#25648 = CARTESIAN_POINT ( 'NONE',  ( -3.150225605703000475, -1.751833096891999952, -1.400642508557000010 ) ) ;
#25649 = CARTESIAN_POINT ( 'NONE',  ( -4.178495327992000519, -80.18134756606798419, 8.699161539798998533 ) ) ;
#25650 = DIRECTION ( 'NONE',  ( 0.000000000000000000, 0.000000000000000000, 1.000000000000000000 ) ) ;
#25651 = CARTESIAN_POINT ( 'NONE',  ( -12.70228549156885123, -53.97187149226591174, -1.205357499401769950 ) ) ;
#25652 = ORIENTED_EDGE ( 'NONE', *, *, #12045, .F. ) ;
#25653 = DIRECTION ( 'NONE',  ( 0.000000000000000000, 0.000000000000000000, -1.000000000000000000 ) ) ;
#25654 = CARTESIAN_POINT ( 'NONE',  ( 7.065231863527838385, -79.37355030446100557, 9.414959857278416777 ) ) ;
#25655 = CARTESIAN_POINT ( 'NONE',  ( -3.947687142456000053, -79.66548667140099838, 8.787283549286000195 ) ) ;
#25656 = CARTESIAN_POINT ( 'NONE',  ( 1.250000000000000000, -80.74999999999998579, 0.000000000000000000 ) ) ;
#25657 = CARTESIAN_POINT ( 'NONE',  ( 3.992904449609000483, -78.62148118236265759, 0.000000000000000000 ) ) ;
#25658 = CARTESIAN_POINT ( 'NONE',  ( 1.551146335801999898, -81.10931883074999860, 0.6076261867840000441 ) ) ;
#25659 = VECTOR ( 'NONE', #58404, 1000.000000000000000 ) ;
#25660 = ORIENTED_EDGE ( 'NONE', *, *, #37001, .T. ) ;
#25661 = CARTESIAN_POINT ( 'NONE',  ( 10.07627163191000008, -60.04999999657000131, -7.601397897754999633 ) ) ;
#25662 = CARTESIAN_POINT ( 'NONE',  ( -1.980584515752000119, -55.53514853344000102, -12.76303204600000107 ) ) ;
#25663 = CARTESIAN_POINT ( 'NONE',  ( 2.062502994258999856, -57.04351820043999766, -12.92181194098999875 ) ) ;
#25664 = B_SPLINE_CURVE_WITH_KNOTS ( 'NONE', 3,
 ( #29390, #24971, #42992, #2833, #38547, #20830, #56852, #34395, #13926, #31921, #36073, #45536, #36362, #54389, #36653, #44943, #45240, #4499, #22497 ),
 .UNSPECIFIED., .F., .F.,
 ( 4, 1, 1, 1, 1, 1, 1, 1, 1, 1, 1, 1, 1, 1, 1, 1, 4 ),
 ( 0.000000000000000000, 0.04500041105014277593, 0.1100003581458013774, 0.1750003052412117677, 0.2400002523368703622, 0.3050001994322810162, 0.3700001465279396107, 0.4350000936233500148, 0.5000000407190086094, 0.5649999878144189580, 0.6299999349100775525, 0.6949998820054882342, 0.7599998291011468288, 0.8249997761965572884, 0.8899997232919678591, 0.9549996703876262316, 1.000000000000000000 ),
 .UNSPECIFIED. ) ;
#25665 = EDGE_CURVE ( 'NONE', #30464, #16033, #15285, .T. ) ;
#25666 = AXIS2_PLACEMENT_3D ( 'NONE', #8828, #13242, #21811 ) ;
#25667 = CARTESIAN_POINT ( 'NONE',  ( -12.75761570867999950, -56.02180874340999850, 1.931043762602999925 ) ) ;
#25668 = CARTESIAN_POINT ( 'NONE',  ( 10.47049206515227660, -78.37083834417222761, 2.813954660210043812 ) ) ;
#25669 = AXIS2_PLACEMENT_3D ( 'NONE', #29927, #7514, #39092 ) ;
#25670 = LINE ( 'NONE', #15953, #39404 ) ;
#25671 = ORIENTED_EDGE ( 'NONE', *, *, #8778, .T. ) ;
#25672 = ORIENTED_EDGE ( 'NONE', *, *, #54184, .T. ) ;
#25673 = CARTESIAN_POINT ( 'NONE',  ( -11.56560577205999962, -76.78936719843599690, -4.664037835044000602 ) ) ;
#25674 = CARTESIAN_POINT ( 'NONE',  ( 4.240041242285670364, -78.75727277875573407, -9.878621513098671869 ) ) ;
#25675 = EDGE_LOOP ( 'NONE', ( #875, #50109, #1981, #58286 ) ) ;
#25676 = CARTESIAN_POINT ( 'NONE',  ( -4.342561293556999935, -77.77735584965398630, -8.443909622126001935 ) ) ;
#25677 = CARTESIAN_POINT ( 'NONE',  ( 2.879226727952050258, -77.55416666666666003, 10.71369944335148361 ) ) ;
#25678 = CARTESIAN_POINT ( 'NONE',  ( 1.722320550003394679, -54.56336311145909690, 12.71171904433208866 ) ) ;
#25679 = CARTESIAN_POINT ( 'NONE',  ( 12.49589899905999957, -77.31018438914000512, -3.422742383397000321 ) ) ;
#25680 = PRODUCT_DEFINITION_CONTEXT ( 'detailed design', #52268, 'design' ) ;
#25681 = CARTESIAN_POINT ( 'NONE',  ( -8.838834764832000701, -18.75000000000000000, 8.838834764832000701 ) ) ;
#25682 = DIRECTION ( 'NONE',  ( -0.7071067811865475727, 0.000000000000000000, -0.7071067811865475727 ) ) ;
#25683 = CARTESIAN_POINT ( 'NONE',  ( 1.500000000000000000, -79.75000000000000000, 0.000000000000000000 ) ) ;
#25684 = CARTESIAN_POINT ( 'NONE',  ( -1.472820794058999905, -78.51599588445799327, -10.90095403661999995 ) ) ;
#25685 = CARTESIAN_POINT ( 'NONE',  ( -0.7292915032463275216, -79.98137597068046034, 9.221144000337346824 ) ) ;
#25686 = VERTEX_POINT ( 'NONE', #16072 ) ;
#25687 = CARTESIAN_POINT ( 'NONE',  ( 0.7246619768400597295, -80.32015672653835736, 11.08451829927562926 ) ) ;
#25688 = ORIENTED_EDGE ( 'NONE', *, *, #35064, .F. ) ;
#25689 = EDGE_CURVE ( 'NONE', #47356, #29025, #3982, .T. ) ;
#25690 = CARTESIAN_POINT ( 'NONE',  ( 5.455175217613329686, -77.27533145166849238, -7.470068744196724175 ) ) ;
#25691 = CARTESIAN_POINT ( 'NONE',  ( -0.2488193260981999833, -80.18635278971700586, 1.395760840247999957 ) ) ;
#25692 = DIRECTION ( 'NONE',  ( -1.000000000000000000, 0.000000000000000000, 0.000000000000000000 ) ) ;
#25693 = VECTOR ( 'NONE', #26202, 1000.000000000000114 ) ;
#25694 = CARTESIAN_POINT ( 'NONE',  ( 0.6485435286463999693, -78.70748627212400095, -1.370523042014000215 ) ) ;
#25695 = CARTESIAN_POINT ( 'NONE',  ( 12.00000000000000000, -18.75000000000000000, -1.250000000000000000 ) ) ;
#25696 = CARTESIAN_POINT ( 'NONE',  ( 0.6727641735938050260, -81.66943313961250794, -1.083490727392691033 ) ) ;
#25697 = CARTESIAN_POINT ( 'NONE',  ( 1.000000000000000000, -81.99999999999998579, -7.000000000000000000 ) ) ;
#25698 = CARTESIAN_POINT ( 'NONE',  ( 0.000000000000000000, -76.00000000000000000, 0.000000000000000000 ) ) ;
#25699 = CARTESIAN_POINT ( 'NONE',  ( -1.168412079197438169, -79.12903572094943172, -0.4440620687051278770 ) ) ;
#25700 = CARTESIAN_POINT ( 'NONE',  ( -5.850594862776000049, -78.47586176634699484, 9.500638896661000032 ) ) ;
#25701 = CARTESIAN_POINT ( 'NONE',  ( 10.53003223722999948, -23.32452529362999982, -7.612971414713999962 ) ) ;
#25702 = CARTESIAN_POINT ( 'NONE',  ( -12.85144117164000122, -58.55472016995999951, 1.980464439859999981 ) ) ;
#25703 = DIRECTION ( 'NONE',  ( -1.000000000000000000, 0.000000000000000000, 0.000000000000000000 ) ) ;
#25704 = CIRCLE ( 'NONE', #302, 1.750000000000001332 ) ;
#25705 = FACE_OUTER_BOUND ( 'NONE', #21919, .T. ) ;
#25706 = ADVANCED_FACE ( 'NONE', ( #52378 ), #5500, .F. ) ;
#25707 = ORIENTED_EDGE ( 'NONE', *, *, #42922, .F. ) ;
#25708 = CARTESIAN_POINT ( 'NONE',  ( 1.463006681111000074, -81.53727493794998793, -0.8714086385761999898 ) ) ;
#25709 = CARTESIAN_POINT ( 'NONE',  ( 0.7181780477660000273, -80.73093781866000995, 1.413724517075999998 ) ) ;
#25710 = DIRECTION ( 'NONE',  ( 1.158063445486000064E-14, 0.000000000000000000, -1.000000000000000000 ) ) ;
#25711 = ADVANCED_FACE ( 'NONE', ( #4223 ), #12497, .T. ) ;
#25712 = CARTESIAN_POINT ( 'NONE',  ( 4.374544387491000386, -77.22085244456999931, -11.15253550093999912 ) ) ;
#25713 = CARTESIAN_POINT ( 'NONE',  ( 13.99936781018472232, -32.88214388149999934, 0.1330447863085613691 ) ) ;
#25714 = CARTESIAN_POINT ( 'NONE',  ( -1.519662023741000123, -82.74476900261298340, -0.6825586799200999977 ) ) ;
#25715 = CARTESIAN_POINT ( 'NONE',  ( -6.036864304657779456, -76.31631156611008748, 10.44601093413916537 ) ) ;
#25716 = CARTESIAN_POINT ( 'NONE',  ( 7.920136950582000068, -77.92325194988499959, 4.778486233528999705 ) ) ;
#25717 = CARTESIAN_POINT ( 'NONE',  ( 7.184025905720999639, -77.27327641628599508, -6.082841960620999799 ) ) ;
#25718 = B_SPLINE_CURVE_WITH_KNOTS ( 'NONE', 3,
 ( #49733, #36714, #9570, #41147 ),
 .UNSPECIFIED., .F., .F.,
 ( 4, 4 ),
 ( 0.000000000000000000, 1.000000000000000000 ),
 .UNSPECIFIED. ) ;
#25719 = CARTESIAN_POINT ( 'NONE',  ( -10.74996386890631328, -76.59758012670684479, 0.3350321142958054277 ) ) ;
#25720 = DIRECTION ( 'NONE',  ( 0.000000000000000000, 1.000000000000000000, 0.000000000000000000 ) ) ;
#25721 = CARTESIAN_POINT ( 'NONE',  ( 10.85622085026185069, -75.98074828373636080, 4.494179903487589556 ) ) ;
#25722 = CARTESIAN_POINT ( 'NONE',  ( 0.5071878057841813225, -81.30734082616947944, -1.169795988924593022 ) ) ;
#25723 = VERTEX_POINT ( 'NONE', #16935 ) ;
#25724 = AXIS2_PLACEMENT_3D ( 'NONE', #57172, #8163, #7871 ) ;
#25725 = CARTESIAN_POINT ( 'NONE',  ( 0.000000000000000000, -76.75499999999999545, 0.000000000000000000 ) ) ;
#25726 = CARTESIAN_POINT ( 'NONE',  ( 1.995598161747699439, -2.278437428562636757, -2.597973788337413215 ) ) ;
#25727 = LINE ( 'NONE', #3869, #56870 ) ;
#25728 = CARTESIAN_POINT ( 'NONE',  ( -4.277738290159001089, -78.96298893710398659, -10.10766895494000117 ) ) ;
#25729 = CARTESIAN_POINT ( 'NONE',  ( 0.000000000000000000, -90.29999999999999716, 0.000000000000000000 ) ) ;
#25730 = CARTESIAN_POINT ( 'NONE',  ( 8.322242302276999126, -76.25751096588899713, 9.174819693653001096 ) ) ;
#25731 = CARTESIAN_POINT ( 'NONE',  ( 5.295455463754168868, -78.53769345340680275, 10.50214436971515575 ) ) ;
#25732 = CARTESIAN_POINT ( 'NONE',  ( 8.838834764832000701, -60.04999999966999980, -8.838834764832000701 ) ) ;
#25733 = VERTEX_POINT ( 'NONE', #30201 ) ;
#25734 = CARTESIAN_POINT ( 'NONE',  ( 10.95738943370000129, -78.88188541137900245, -1.279590238973999927 ) ) ;
#25735 = CARTESIAN_POINT ( 'NONE',  ( 0.4666069534000411023, -79.94482168187342097, 1.159469772846831948 ) ) ;
#25736 = CARTESIAN_POINT ( 'NONE',  ( 1.210822168571049851, -78.13541666666667140, -9.250000000000003553 ) ) ;
#25737 = CARTESIAN_POINT ( 'NONE',  ( 8.348568777154000031, -77.93724719090198505, -7.051780313135000533 ) ) ;
#25738 = FACE_OUTER_BOUND ( 'NONE', #23215, .T. ) ;
#25739 = CARTESIAN_POINT ( 'NONE',  ( 5.894914467206975317, -77.93666666666661058, 7.125729969419699827 ) ) ;
#25740 = CARTESIAN_POINT ( 'NONE',  ( 0.000000000000000000, -81.19999999999998863, 7.000000000000000000 ) ) ;
#25741 = AXIS2_PLACEMENT_3D ( 'NONE', #58168, #4443, #8870 ) ;
#25742 = CARTESIAN_POINT ( 'NONE',  ( 1.137309322218171381, -82.53963407618115866, -1.048735418599893832 ) ) ;
#25743 = PRODUCT ( 'MAS-694', 'MAS-694', '', ( #17693 ) ) ;
#25744 = CARTESIAN_POINT ( 'NONE',  ( 0.5791152278277256205, -79.76384116944609559, -1.107571749123516192 ) ) ;
#25745 = EDGE_CURVE ( 'NONE', #42100, #2183, #44090, .T. ) ;
#25746 = VERTEX_POINT ( 'NONE', #39650 ) ;
#25747 = CARTESIAN_POINT ( 'NONE',  ( 0.000000000000000000, -4.000000000000000000, -8.999999999999927169 ) ) ;
#25748 = EDGE_CURVE ( 'NONE', #25098, #22699, #36446, .T. ) ;
#25749 = CARTESIAN_POINT ( 'NONE',  ( 1.931043762602999925, -19.22180874373999870, 12.75761570870000128 ) ) ;
#25750 = CONICAL_SURFACE ( 'NONE', #56906, 9.349999999968000353, 0.7853981633972997312 ) ;
#25751 =( NAMED_UNIT ( * ) PLANE_ANGLE_UNIT ( ) SI_UNIT ( $, .RADIAN. ) );
#25752 = DIRECTION ( 'NONE',  ( 0.000000000000000000, 1.000000000000000000, 0.000000000000000000 ) ) ;
#25753 = ORIENTED_EDGE ( 'NONE', *, *, #4722, .T. ) ;
#25754 = ORIENTED_EDGE ( 'NONE', *, *, #25525, .F. ) ;
#25755 = B_SPLINE_CURVE_WITH_KNOTS ( 'NONE', 3,
 ( #7615, #25902, #21188, #25042, #20902, #43926, #47515, #48361, #48084, #52210, #20332, #56924, #7043, #39190, #43064, #38620, #3474, #12050 ),
 .UNSPECIFIED., .F., .F.,
 ( 4, 2, 2, 2, 2, 2, 2, 2, 4 ),
 ( 0.000000000000000000, 0.1249999999999999722, 0.2499999999999999445, 0.3749999999999998890, 0.4999999999999998890, 0.6249999999999998890, 0.7499999999999997780, 0.8749999999999998890, 1.000000000000000000 ),
 .UNSPECIFIED. ) ;
#25756 = CARTESIAN_POINT ( 'NONE',  ( -12.66314509266000066, -53.62135249290999894, 0.04032083120558000583 ) ) ;
#25757 = VERTEX_POINT ( 'NONE', #3075 ) ;
#25758 = CARTESIAN_POINT ( 'NONE',  ( -4.696659842484057101, -79.66604136332699682, 8.289744325010493853 ) ) ;
#25759 = ORIENTED_EDGE ( 'NONE', *, *, #12181, .T. ) ;
#25760 = CARTESIAN_POINT ( 'NONE',  ( 10.52682159650000138, -23.42567232067999683, 7.605689092050000433 ) ) ;
#25761 = AXIS2_PLACEMENT_3D ( 'NONE', #52891, #43752, #8011 ) ;
#25762 = CARTESIAN_POINT ( 'NONE',  ( 0.2583767295277000220, -78.20029307777100769, -10.91369642039000176 ) ) ;
#25763 = AXIS2_PLACEMENT_3D ( 'NONE', #18118, #25864, #39449 ) ;
#25764 = CARTESIAN_POINT ( 'NONE',  ( 6.607804308078000233, -79.44368667140099660, -6.725089593472000082 ) ) ;
#25765 = CARTESIAN_POINT ( 'NONE',  ( 0.3345645958933402553, -78.22793362420514995, -9.244204907905819724 ) ) ;
#25766 = CARTESIAN_POINT ( 'NONE',  ( 2.315902194296999728, -78.33986656763099177, -10.97517055051999968 ) ) ;
#25767 = VERTEX_POINT ( 'NONE', #25785 ) ;
#25768 = ORIENTED_EDGE ( 'NONE', *, *, #55685, .F. ) ;
#25769 = CARTESIAN_POINT ( 'NONE',  ( -7.491156050946263356, -77.55010980111761398, 5.426323088073407241 ) ) ;
#25770 = CARTESIAN_POINT ( 'NONE',  ( -9.050627908549000011, -77.41837041848599199, -6.322205650057999726 ) ) ;
#25771 = FACE_OUTER_BOUND ( 'NONE', #20815, .T. ) ;
#25772 = CARTESIAN_POINT ( 'NONE',  ( -12.70956478401000034, -60.20497526583999814, -1.933781249744999986 ) ) ;
#25773 = CARTESIAN_POINT ( 'NONE',  ( 9.583411031200000707, -78.09271807287498746, 1.526087275887999972 ) ) ;
#25774 = FACE_OUTER_BOUND ( 'NONE', #48778, .T. ) ;
#25775 = CARTESIAN_POINT ( 'NONE',  ( 13.86363636363000218, -32.36102867817999851, 1.277888278705000044E-05 ) ) ;
#25776 = CARTESIAN_POINT ( 'NONE',  ( -11.09141466634999951, -79.91658357209098540, 1.909950515085000022 ) ) ;
#25777 = CARTESIAN_POINT ( 'NONE',  ( 0.000000000000000000, -87.64999999984398471, -9.649999999844000698 ) ) ;
#25778 = DIRECTION ( 'NONE',  ( -1.000000000000000000, 0.000000000000000000, 0.000000000000000000 ) ) ;
#25779 = ORIENTED_EDGE ( 'NONE', *, *, #2515, .T. ) ;
#25780 = CARTESIAN_POINT ( 'NONE',  ( -8.220399303298000504, -53.98050618241000365, 9.523318109972001011 ) ) ;
#25781 = EDGE_CURVE ( 'NONE', #26795, #2543, #43991, .T. ) ;
#25782 = CARTESIAN_POINT ( 'NONE',  ( 0.000000000000000000, -75.20000000000000284, 7.200000000000000178 ) ) ;
#25783 = CARTESIAN_POINT ( 'NONE',  ( -7.760941378066999796, -17.76914109191999813, -10.15321372496999963 ) ) ;
#25785 = CARTESIAN_POINT ( 'NONE',  ( 12.50240681836000078, -61.48234730679999416, -1.005418944265000114 ) ) ;
#25784 = CARTESIAN_POINT ( 'NONE',  ( 7.642147947533000085, -59.58485473249000108, 10.55910102243999837 ) ) ;
#25786 = CARTESIAN_POINT ( 'NONE',  ( 8.083193604682708866, -79.39173883515665864, 4.658712740633392357 ) ) ;
#25787 = SURFACE_STYLE_FILL_AREA ( #39371 ) ;
#25788 = CARTESIAN_POINT ( 'NONE',  ( -10.86494198988000015, -78.40907477017699989, -2.491513063939999828 ) ) ;
#25789 = CARTESIAN_POINT ( 'NONE',  ( -9.191308745188409901, -79.61083708887171895, -1.210837173519272447 ) ) ;
#25790 = CARTESIAN_POINT ( 'NONE',  ( 5.504720026230000229, -80.98993105630589184, -9.574706785621000193 ) ) ;
#25791 = EDGE_LOOP ( 'NONE', ( #48295, #14324, #36430, #4632, #14562 ) ) ;
#25792 = CARTESIAN_POINT ( 'NONE',  ( 12.49999990534960226, -49.87071424677999687, 0.001538265197309672755 ) ) ;
#25793 = AXIS2_PLACEMENT_3D ( 'NONE', #7651, #33926, #47258 ) ;
#25794 = FACE_OUTER_BOUND ( 'NONE', #985, .T. ) ;
#25795 = CARTESIAN_POINT ( 'NONE',  ( -12.75761570870000128, -19.22180874373999870, 1.931043762602999925 ) ) ;
#25796 = CARTESIAN_POINT ( 'NONE',  ( -0.4933341540935000102, -3.017260803691999893, 3.612264854784000168 ) ) ;
#25797 = CARTESIAN_POINT ( 'NONE',  ( 6.028278362248999933, -79.27746395522298428, 7.385810467003000035 ) ) ;
#25798 = CARTESIAN_POINT ( 'NONE',  ( -12.77562786365999870, -53.53761952105000432, 0.5426593252874999385 ) ) ;
#25799 = CARTESIAN_POINT ( 'NONE',  ( -1.980584515756000030, -60.06485150062000145, -12.76303204342999997 ) ) ;
#25800 = CARTESIAN_POINT ( 'NONE',  ( -3.250000000000000000, -2.100000000000000089, 0.000000000000000000 ) ) ;
#25801 = CARTESIAN_POINT ( 'NONE',  ( 8.872994237323281297, -79.12000000000000455, -3.510218210012922668 ) ) ;
#25802 = VECTOR ( 'NONE', #21854, 1000.000000000000000 ) ;
#25803 = CARTESIAN_POINT ( 'NONE',  ( -3.073398260277000027, -86.35846544543099412, 2.159909763142000116 ) ) ;
#25804 = EDGE_CURVE ( 'NONE', #25686, #49594, #19513, .T. ) ;
#25805 = DIRECTION ( 'NONE',  ( 0.9859154929576978699, -0.1672442547472993701, 2.241735036661995419E-11 ) ) ;
#25806 = CARTESIAN_POINT ( 'NONE',  ( -8.579474846409000932, -77.31747724050399029, 6.800540979835000499 ) ) ;
#25807 = CARTESIAN_POINT ( 'NONE',  ( 10.85325925093383681, -76.41847643180719274, -4.501722357903592986 ) ) ;
#25808 = CARTESIAN_POINT ( 'NONE',  ( 10.83471462526000018, -76.90620299209300015, 2.076220934837999632 ) ) ;
#25809 = DIRECTION ( 'NONE',  ( -0.7071067811865475727, 0.000000000000000000, 0.7071067811865475727 ) ) ;
#25810 = CARTESIAN_POINT ( 'NONE',  ( -3.249671636765069316, -1.085071008848613960, 0.6795062066016868130 ) ) ;
#25811 = DIRECTION ( 'NONE',  ( 0.7026410690473250398, -0.1122098755728047209, 0.7026410690473250398 ) ) ;
#25812 = CARTESIAN_POINT ( 'NONE',  ( 5.684029094576000141, -79.68554415034599003, -7.680196531179999120 ) ) ;
#25813 = CARTESIAN_POINT ( 'NONE',  ( -0.7612530485432564831, -3.494945300038082348, 3.169665447793446500 ) ) ;
#25814 = CARTESIAN_POINT ( 'NONE',  ( 0.08637108029348440630, -80.22590001772620383, -10.74954481972912745 ) ) ;
#25815 = DIRECTION ( 'NONE',  ( 0.000000000000000000, -1.000000000000000000, 0.000000000000000000 ) ) ;
#25816 = CARTESIAN_POINT ( 'NONE',  ( 10.45812042142963350, -75.79999999999999716, 6.020400211397366697 ) ) ;
#25817 = EDGE_CURVE ( 'NONE', #23965, #20634, #43811, .T. ) ;
#25818 = CARTESIAN_POINT ( 'NONE',  ( 4.847151869481000297, -78.90810309376399800, 11.00961342987999991 ) ) ;
#25819 = CARTESIAN_POINT ( 'NONE',  ( 1.250000000000000000, -76.50000000000000000, 0.000000000000000000 ) ) ;
#25820 = CARTESIAN_POINT ( 'NONE',  ( -7.438698978239999704, -79.39099446298800444, -8.455750828251000328 ) ) ;
#25821 = CARTESIAN_POINT ( 'NONE',  ( -3.463637548850266867, -77.50106921249592062, 10.20060348489307600 ) ) ;
#25822 = ORIENTED_EDGE ( 'NONE', *, *, #12233, .T. ) ;
#25823 = CARTESIAN_POINT ( 'NONE',  ( 7.644093100861836021, -60.32380578946132488, 10.09634101415691809 ) ) ;
#25824 = EDGE_LOOP ( 'NONE', ( #39755, #51775, #14510, #49731, #43553, #42333 ) ) ;
#25825 = EDGE_LOOP ( 'NONE', ( #4501, #27402, #3680, #17078 ) ) ;
#25826 = CARTESIAN_POINT ( 'NONE',  ( 0.8506806241676508895, -1.354166666666666297, 3.165411199172028400 ) ) ;
#25827 = ORIENTED_EDGE ( 'NONE', *, *, #27057, .F. ) ;
#25828 = CIRCLE ( 'NONE', #55088, 5.000000000000000000 ) ;
#25829 = CARTESIAN_POINT ( 'NONE',  ( 0.4795136812456999853, -79.29531287791878924, -3.557221409453999783 ) ) ;
#25830 = CARTESIAN_POINT ( 'NONE',  ( -2.145956266024737769, -79.29304659155522472, 9.258292488271512966 ) ) ;
#25831 = ORIENTED_EDGE ( 'NONE', *, *, #45897, .F. ) ;
#25832 = CARTESIAN_POINT ( 'NONE',  ( -5.996769837547000215, -78.92093781725999690, 10.80604144232000152 ) ) ;
#25833 = VERTEX_POINT ( 'NONE', #21353 ) ;
#25834 = CARTESIAN_POINT ( 'NONE',  ( 8.090910852014799204, -55.25278097498591734, -7.452378523310748015 ) ) ;
#25835 = ORIENTED_EDGE ( 'NONE', *, *, #47673, .F. ) ;
#25836 = CARTESIAN_POINT ( 'NONE',  ( 0.7848080566249374668, -77.91804990316740032, -1.315710784708647108 ) ) ;
#25837 = CARTESIAN_POINT ( 'NONE',  ( 9.148037756630525763, -79.79999999999999716, 7.522470651702480637 ) ) ;
#25838 = CIRCLE ( 'NONE', #39070, 12.50000000000000000 ) ;
#25839 = CARTESIAN_POINT ( 'NONE',  ( -4.817876235597053913, -80.01207991527530794, 9.609839989271527827 ) ) ;
#25840 = DIRECTION ( 'NONE',  ( 0.9957542217969250764, 0.04890179605521120104, -0.07798810240142199646 ) ) ;
#25841 = CARTESIAN_POINT ( 'NONE',  ( -1.415063685059226417, -86.17851879815596305, -3.099337804490793324 ) ) ;
#25842 = CARTESIAN_POINT ( 'NONE',  ( 3.223004389858187047, -85.82829189952225590, 1.542474583517786879 ) ) ;
#25843 = CARTESIAN_POINT ( 'NONE',  ( 5.691226796558999546, -77.84489713918000575, 11.81421328157999895 ) ) ;
#25844 = CARTESIAN_POINT ( 'NONE',  ( 1.194439549549000112, -80.29130269966999833, -0.6318903263597999143 ) ) ;
#25845 = CARTESIAN_POINT ( 'NONE',  ( 8.187817122061000319, -76.13338407210200387, 7.683968774170000238 ) ) ;
#25846 = FACE_OUTER_BOUND ( 'NONE', #15586, .T. ) ;
#25847 = CARTESIAN_POINT ( 'NONE',  ( -7.992881336352999355, -77.05258667140100215, -5.171618568468999477 ) ) ;
#25848 = CARTESIAN_POINT ( 'NONE',  ( 4.074485157876000407, -81.09906924513698812, -0.6760801638114999346 ) ) ;
#25850 = EDGE_CURVE ( 'NONE', #54702, #49897, #664, .T. ) ;
#25849 = CARTESIAN_POINT ( 'NONE',  ( 7.954951288349001004, -23.25000000000000000, -9.722718241315000398 ) ) ;
#25851 = CARTESIAN_POINT ( 'NONE',  ( 1.226192273942385391, -2.945367736052959540, 3.009049604377801224 ) ) ;
#25852 = CARTESIAN_POINT ( 'NONE',  ( -2.718796855976000071, -78.87905496681159434, -2.278127071542000337 ) ) ;
#25853 = CARTESIAN_POINT ( 'NONE',  ( -1.247385801080000078, -24.47722256257000240, -12.50301438876999960 ) ) ;
#25854 = CARTESIAN_POINT ( 'NONE',  ( 1.941194386247999892, -82.67419503318798490, 2.968716399090999936 ) ) ;
#25855 = CARTESIAN_POINT ( 'NONE',  ( -3.268529449828999844, -2.325473928489000031, -1.950076325099000085 ) ) ;
#25856 = CARTESIAN_POINT ( 'NONE',  ( -0.7579940186957824233, -80.67607680420574923, 1.024633870185459816 ) ) ;
#25857 = CARTESIAN_POINT ( 'NONE',  ( -7.758655887927999650, -60.95078616210999911, -9.996711281005000060 ) ) ;
#25858 = CARTESIAN_POINT ( 'NONE',  ( 2.486604901413133728, -78.25416666666667709, 9.252740428349007118 ) ) ;
#25859 = CIRCLE ( 'NONE', #8884, 1.250000000000000000 ) ;
#25860 = CARTESIAN_POINT ( 'NONE',  ( -0.05395919428434999693, -80.79989190857401127, -1.332567581519000122 ) ) ;
#25861 = CARTESIAN_POINT ( 'NONE',  ( -12.70926961119000076, -18.59159259619999816, -1.933875435151000133 ) ) ;
#25862 = CARTESIAN_POINT ( 'NONE',  ( 9.175280770439000477, -76.74417995138000492, -8.221808909867000636 ) ) ;
#25863 = AXIS2_PLACEMENT_3D ( 'NONE', #3084, #16082, #11658 ) ;
#25864 = DIRECTION ( 'NONE',  ( 0.000000000000000000, 1.000000000000000000, 0.000000000000000000 ) ) ;
#25865 = EDGE_CURVE ( 'NONE', #37493, #23736, #28004, .T. ) ;
#25866 = CARTESIAN_POINT ( 'NONE',  ( -9.414505844818329194, -77.40158925224952213, -0.1990887029408508757 ) ) ;
#25867 = CARTESIAN_POINT ( 'NONE',  ( 9.003374968273998746, -76.27138176936000491, -8.471312771788998219 ) ) ;
#25868 = ORIENTED_EDGE ( 'NONE', *, *, #6596, .F. ) ;
#25869 = AXIS2_PLACEMENT_3D ( 'NONE', #48278, #25815, #38527 ) ;
#25870 = CARTESIAN_POINT ( 'NONE',  ( 0.000000000000000000, -90.35000000009100063, 0.000000000000000000 ) ) ;
#25871 = DIRECTION ( 'NONE',  ( -1.000000000000000000, 0.000000000000000000, 0.000000000000000000 ) ) ;
#25872 = CARTESIAN_POINT ( 'NONE',  ( 12.49997170193999985, -59.99201514515999634, 1.666513530428000101 ) ) ;
#25873 = CARTESIAN_POINT ( 'NONE',  ( -1.667936688463999895, -19.23513569609999863, -12.53239398062000198 ) ) ;
#25874 = CARTESIAN_POINT ( 'NONE',  ( 7.742244746672000133, -79.15749084168798788, -5.543281135378999913 ) ) ;
#25875 = CARTESIAN_POINT ( 'NONE',  ( -1.752682768676000036, -84.98406384713199202, -3.786578346095999859 ) ) ;
#25876 = CARTESIAN_POINT ( 'NONE',  ( -12.65375411746000012, -21.74977139047000207, 1.750000000000000000 ) ) ;
#25877 = CARTESIAN_POINT ( 'NONE',  ( -0.2488193260981999833, -79.99172447744500403, 1.395760840247999957 ) ) ;
#25878 = ORIENTED_EDGE ( 'NONE', *, *, #3473, .F. ) ;
#25879 = CARTESIAN_POINT ( 'NONE',  ( 8.796335266379967877, -78.89791666666668846, -6.760013919724086051 ) ) ;
#25880 = CARTESIAN_POINT ( 'NONE',  ( 3.699999999670001039, -79.00321104920828930, 7.399999999340033163 ) ) ;
#25881 = EDGE_LOOP ( 'NONE', ( #24966, #41231 ) ) ;
#25882 = EDGE_CURVE ( 'NONE', #8017, #34968, #5674, .T. ) ;
#25883 = CARTESIAN_POINT ( 'NONE',  ( 0.9061038674864000386, -78.73921517645298707, 10.90260483175000061 ) ) ;
#25884 = CARTESIAN_POINT ( 'NONE',  ( 12.69619287815999975, -57.04916621739000249, 1.799475295154000065 ) ) ;
#25885 = CARTESIAN_POINT ( 'NONE',  ( -7.031693321690999809, -80.44190203517098325, -8.741081632921000377 ) ) ;
#25886 = ORIENTED_EDGE ( 'NONE', *, *, #16639, .T. ) ;
#25887 = ORIENTED_EDGE ( 'NONE', *, *, #22519, .T. ) ;
#25888 = VERTEX_POINT ( 'NONE', #18687 ) ;
#25889 = EDGE_CURVE ( 'NONE', #43183, #6045, #32235, .T. ) ;
#25890 = CARTESIAN_POINT ( 'NONE',  ( 1.089041876986236002, -80.39116380685027252, 0.6134409219567780180 ) ) ;
#25891 = CARTESIAN_POINT ( 'NONE',  ( 0.000000000000000000, -60.04999999966999980, -12.00000000000000000 ) ) ;
#25892 = DIRECTION ( 'NONE',  ( 0.5000000000000744960, -0.7071067811864422126, -0.5000000000000744960 ) ) ;
#25893 = EDGE_CURVE ( 'NONE', #18079, #27707, #991, .T. ) ;
#25894 = AXIS2_PLACEMENT_3D ( 'NONE', #8064, #21639, #12775 ) ;
#25895 = ORIENTED_EDGE ( 'NONE', *, *, #42973, .F. ) ;
#25896 = CARTESIAN_POINT ( 'NONE',  ( 10.99606201159937058, -18.31532548058919829, 0.3145367810815102305 ) ) ;
#25897 = ORIENTED_EDGE ( 'NONE', *, *, #16367, .F. ) ;
#25898 = CARTESIAN_POINT ( 'NONE',  ( -2.600000000000000089, -77.49999999999998579, 0.000000000000000000 ) ) ;
#25899 = AXIS2_PLACEMENT_3D ( 'NONE', #124, #23683, #28099 ) ;
#25900 = CARTESIAN_POINT ( 'NONE',  ( -3.740501297249256396, -79.00321104920828930, -2.113513782812399544 ) ) ;
#25901 = CARTESIAN_POINT ( 'NONE',  ( 7.659225706216000518, -55.11732795990999989, 9.963487823480999594 ) ) ;
#25902 = CARTESIAN_POINT ( 'NONE',  ( 1.499999999999999778, -78.16041666666670551, 0.1963495408493654004 ) ) ;
#25903 = CARTESIAN_POINT ( 'NONE',  ( -1.229229937364078928, -79.61588541666264973, 9.384114583424059575 ) ) ;
#25904 = AXIS2_PLACEMENT_3D ( 'NONE', #5493, #11112, #23791 ) ;
#25905 = CARTESIAN_POINT ( 'NONE',  ( 12.70455691847901214, -61.36014620563325650, -1.489817752282083463 ) ) ;
#25906 = CARTESIAN_POINT ( 'NONE',  ( 10.69384760718000038, -78.36279039943012492, -5.399785902169999652 ) ) ;
#25907 = CARTESIAN_POINT ( 'NONE',  ( 9.124907197977810469, -78.83697965493469439, -1.519474258559118329 ) ) ;
#25908 = CARTESIAN_POINT ( 'NONE',  ( -7.658900562714999971, -23.20940503079999928, 10.01676248781999945 ) ) ;
#25909 = EDGE_CURVE ( 'NONE', #4126, #49275, #38258, .T. ) ;
#25910 = CARTESIAN_POINT ( 'NONE',  ( -4.016276557929000290, -78.60958598268121023, 0.5808222549768999876 ) ) ;
#25911 = CARTESIAN_POINT ( 'NONE',  ( -9.123604098306000054, -77.28946001420199252, 3.772406241408000405 ) ) ;
#25912 = CARTESIAN_POINT ( 'NONE',  ( 0.1636246173744642929, -83.36458333333334281, 1.250000000000000888 ) ) ;
#25913 = DIRECTION ( 'NONE',  ( 3.675126883001999395E-09, -0.9999999999999997780, -2.168720882565999754E-08 ) ) ;
#25914 = CARTESIAN_POINT ( 'NONE',  ( 0.000000000000000000, -2.900000000000000355, 0.000000000000000000 ) ) ;
#25915 = CARTESIAN_POINT ( 'NONE',  ( -1.999999999936000084, -76.30000000006400285, 2.601307828485999989E-10 ) ) ;
#25916 = FACE_OUTER_BOUND ( 'NONE', #18569, .T. ) ;
#25917 = CARTESIAN_POINT ( 'NONE',  ( 0.000000000000000000, -49.87071424677999687, 0.000000000000000000 ) ) ;
#25918 = CARTESIAN_POINT ( 'NONE',  ( 0.1201377420412941266, -80.61836603707203608, 1.540619319635312401 ) ) ;
#25919 = CARTESIAN_POINT ( 'NONE',  ( 7.333430185446000671, -77.21721742767299190, -5.851948249255000789 ) ) ;
#25920 = CARTESIAN_POINT ( 'NONE',  ( 0.000000000000000000, -77.29999999999999716, 0.000000000000000000 ) ) ;
#25921 = CARTESIAN_POINT ( 'NONE',  ( 0.3926218265389220807, -78.64583333333334281, -1.460959015002473382 ) ) ;
#25922 = CARTESIAN_POINT ( 'NONE',  ( -3.247122682022999918, -2.002034555870999988, -1.453237460094999989 ) ) ;
#25923 = CARTESIAN_POINT ( 'NONE',  ( -7.806617969149999503, -78.30323394950599436, 9.479055599837000301 ) ) ;
#25924 = CARTESIAN_POINT ( 'NONE',  ( 9.250000000000000000, -78.84999999999999432, 1.340711541092999922E-14 ) ) ;
#25926 = CARTESIAN_POINT ( 'NONE',  ( -1.305945605467999870, -78.75327671425300480, -0.1872743590209999809 ) ) ;
#25925 = CARTESIAN_POINT ( 'NONE',  ( -4.000000000000000000, -74.80000000000001137, 0.5999999999999999778 ) ) ;
#25927 = CARTESIAN_POINT ( 'NONE',  ( -0.6483708932059000229, -82.29813732702999118, -1.447070110047999902 ) ) ;
#25928 = CARTESIAN_POINT ( 'NONE',  ( -8.375467055228931201, -79.54614502533394216, 6.744101667046974669 ) ) ;
#25929 = EDGE_LOOP ( 'NONE', ( #46470, #1979, #686, #48675 ) ) ;
#25930 = CARTESIAN_POINT ( 'NONE',  ( -10.87922314793346068, -78.86468826379788766, 5.174618772388030585 ) ) ;
#25931 = CARTESIAN_POINT ( 'NONE',  ( -12.04098616622999884, -79.19168562328098915, -0.08309486781487000762 ) ) ;
#25932 = VECTOR ( 'NONE', #46238, 999.9999999999998863 ) ;
#25933 = CARTESIAN_POINT ( 'NONE',  ( 7.093757948711532535, -79.05808181110914745, 6.348225669172625096 ) ) ;
#25934 = CARTESIAN_POINT ( 'NONE',  ( 8.512781221943589216, -79.71249999999999147, 8.510042318544764228 ) ) ;
#25935 = CARTESIAN_POINT ( 'NONE',  ( -5.539808784079933268, -79.01666666666669414, 9.611650271896811759 ) ) ;
#25936 = AXIS2_PLACEMENT_3D ( 'NONE', #12334, #48362, #39767 ) ;
#25937 = CARTESIAN_POINT ( 'NONE',  ( 12.70556836352000118, -62.02772277195000328, 2.424222323408999617E-09 ) ) ;
#25938 = CARTESIAN_POINT ( 'NONE',  ( 8.780551327949000395, -79.55888659510199545, 4.553845519790999496 ) ) ;
#25939 = CARTESIAN_POINT ( 'NONE',  ( 12.77656765293000163, -25.31198129913999750, -0.1555235816856000153 ) ) ;
#25940 = CARTESIAN_POINT ( 'NONE',  ( 0.000000000000000000, -74.64999999999999147, 0.000000000000000000 ) ) ;
#25941 = EDGE_LOOP ( 'NONE', ( #8048, #29850, #29586, #28108 ) ) ;
#25942 = DIRECTION ( 'NONE',  ( -1.000000000000000000, 0.000000000000000000, 0.000000000000000000 ) ) ;
#25943 = AXIS2_PLACEMENT_3D ( 'NONE', #57804, #56663, #34197 ) ;
#25944 = CARTESIAN_POINT ( 'NONE',  ( -0.6116994581832999600, -79.70066001420198631, 9.722684469059000634 ) ) ;
#25945 = DIRECTION ( 'NONE',  ( -0.7071067811865475727, 0.000000000000000000, -0.7071067811865475727 ) ) ;
#25946 = EDGE_CURVE ( 'NONE', #55197, #20755, #14530, .T. ) ;
#25947 = CARTESIAN_POINT ( 'NONE',  ( 3.399999999999999911, -78.67390000031814168, 0.000000000000000000 ) ) ;
#25948 = CARTESIAN_POINT ( 'NONE',  ( -0.6332123272625999055, -81.29485358483999846, 1.540853336418999797 ) ) ;
#25949 = ORIENTED_EDGE ( 'NONE', *, *, #2432, .T. ) ;
#25950 = ADVANCED_FACE ( 'NONE', ( #26934 ), #5106, .F. ) ;
#25951 = CARTESIAN_POINT ( 'NONE',  ( 0.000000000000000000, -9.638971321655001034, 0.000000000000000000 ) ) ;
#25952 = CARTESIAN_POINT ( 'NONE',  ( 11.74923627718826502, -77.94158813120921536, -0.7696914254377311693 ) ) ;
#25953 = CARTESIAN_POINT ( 'NONE',  ( -3.250000000000000000, -1.000000000000000000, 1.223542571470000149E-13 ) ) ;
#25954 = CARTESIAN_POINT ( 'NONE',  ( -7.619389775666999931, -55.39213701549999769, -10.35398629634000045 ) ) ;
#25955 = CARTESIAN_POINT ( 'NONE',  ( -4.373213035511999358, -79.41820881373098473, -8.733596771889999388 ) ) ;
#25956 = EDGE_LOOP ( 'NONE', ( #18342, #57478, #14274, #48078 ) ) ;
#25957 = ADVANCED_FACE ( 'NONE', ( #40825 ), #41215, .F. ) ;
#25958 = ORIENTED_EDGE ( 'NONE', *, *, #38157, .T. ) ;
#25959 = CARTESIAN_POINT ( 'NONE',  ( 11.30982802994000025, -76.54347076860699417, 5.253977129081000008 ) ) ;
#25960 = CARTESIAN_POINT ( 'NONE',  ( -0.1956594527234810643, -79.26382142333196157, -1.318569963859137495 ) ) ;
#25961 = VERTEX_POINT ( 'NONE', #23685 ) ;
#25962 = CARTESIAN_POINT ( 'NONE',  ( 9.475051992780000987, -77.93498084965399642, -0.6170397550469999270 ) ) ;
#25963 = CARTESIAN_POINT ( 'NONE',  ( -9.611650271896857944, -77.65833333333331723, 5.539808784079855997 ) ) ;
#25964 = CARTESIAN_POINT ( 'NONE',  ( -11.44417895085270942, -75.82083333333332575, -3.075537641221545826 ) ) ;
#25965 = CARTESIAN_POINT ( 'NONE',  ( -1.243328516745999979, -77.78579772561000993, -12.73826093197000020 ) ) ;
#25966 = CARTESIAN_POINT ( 'NONE',  ( 1.508420534579999917, -77.61426645450845285, 11.11497989571999767 ) ) ;
#25967 = DIRECTION ( 'NONE',  ( 0.000000000000000000, 0.000000000000000000, 1.000000000000000000 ) ) ;
#25968 = CARTESIAN_POINT ( 'NONE',  ( 3.333665159394799016, -86.36264282632899381, 2.421341216326561074 ) ) ;
#25969 = CARTESIAN_POINT ( 'NONE',  ( 11.21665020278000036, -78.65217759946699516, 0.06973997782872000395 ) ) ;
#25970 = VECTOR ( 'NONE', #17362, 1000.000000000000227 ) ;
#25971 = CARTESIAN_POINT ( 'NONE',  ( -0.7414790400310934393, -79.98147823536180567, 9.220178373586891851 ) ) ;
#25972 = CARTESIAN_POINT ( 'NONE',  ( 7.764220096248216407, -17.74399029335688383, 10.21028322255854626 ) ) ;
#25973 = EDGE_LOOP ( 'NONE', ( #53400, #16444, #40347, #43914, #2421, #52139 ) ) ;
#25974 = CARTESIAN_POINT ( 'NONE',  ( 5.874297357630430483, -77.27991952769977502, -7.146146602706561879 ) ) ;
#25975 = CARTESIAN_POINT ( 'NONE',  ( -1.260178996155999931, -80.33519065986000385, -0.6496216418182000352 ) ) ;
#25976 = CARTESIAN_POINT ( 'NONE',  ( 0.9995835529977264988, -83.19791666666662877, -0.7681833999686417114 ) ) ;
#25977 = CARTESIAN_POINT ( 'NONE',  ( 6.252156853421744209, -77.06842338808830561, -10.30345392412948158 ) ) ;
#25978 = CIRCLE ( 'NONE', #15632, 1.199999999999999734 ) ;
#25979 = CARTESIAN_POINT ( 'NONE',  ( 1.398095685538000010, -78.36595697280360184, 0.2353462009024000212 ) ) ;
#25980 = CARTESIAN_POINT ( 'NONE',  ( -12.50239399162999909, -54.11640749821000185, 1.003653728895000041 ) ) ;
#25981 = CARTESIAN_POINT ( 'NONE',  ( 12.49306752634999995, -23.28056692670000061, 1.667917367010000040 ) ) ;
#25982 = DIRECTION ( 'NONE',  ( 0.000000000000000000, 1.000000000000000000, 0.000000000000000000 ) ) ;
#25983 = DIRECTION ( 'NONE',  ( 0.000000000000000000, 0.000000000000000000, -1.000000000000000000 ) ) ;
#25984 = CARTESIAN_POINT ( 'NONE',  ( -7.035077178968999867, -79.62764829398598465, -8.660212973301998574 ) ) ;
#25985 = CARTESIAN_POINT ( 'NONE',  ( 10.01235002622999914, -18.70151115557999688, -7.653559626094000201 ) ) ;
#25986 = CARTESIAN_POINT ( 'NONE',  ( -0.9172530285194190336, -83.04126087647844656, 0.8486422117887013616 ) ) ;
#25987 = CARTESIAN_POINT ( 'NONE',  ( 3.793360466995999936, -79.32866876341660145, -1.736943300707000093 ) ) ;
#25988 = CARTESIAN_POINT ( 'NONE',  ( -2.813789756862300262, -77.89583333333332860, 10.47020627418438465 ) ) ;
#25989 = EDGE_LOOP ( 'NONE', ( #8628, #21821, #17989 ) ) ;
#25990 = DIRECTION ( 'NONE',  ( 0.000000000000000000, 1.000000000000000000, 0.000000000000000000 ) ) ;
#25991 = CARTESIAN_POINT ( 'NONE',  ( 3.321932689531000182, -77.19999999999998863, 10.22385755016999909 ) ) ;
#25992 = CARTESIAN_POINT ( 'NONE',  ( 1.539929345890999945, -80.16250488267000662, 0.3781723503825999422 ) ) ;
#25993 = CARTESIAN_POINT ( 'NONE',  ( -1.247959326960667914, -77.91666666666564822, 0.5507335004918384458 ) ) ;
#25994 = CARTESIAN_POINT ( 'NONE',  ( -0.08519377839585000334, -78.37388308536300485, 11.97951611939999950 ) ) ;
#25995 = DIRECTION ( 'NONE',  ( 0.000000000000000000, 1.000000000000000000, 0.000000000000000000 ) ) ;
#25996 = EDGE_CURVE ( 'NONE', #51746, #7307, #30688, .T. ) ;
#25997 = CARTESIAN_POINT ( 'NONE',  ( -1.324613189995999862, -83.30925904736399445, -0.7038465009425000085 ) ) ;
#25998 = CARTESIAN_POINT ( 'NONE',  ( 6.013200962235000446, -77.90957020342199257, 10.30906962990999887 ) ) ;
#25999 = CARTESIAN_POINT ( 'NONE',  ( -9.631455446501000495, -78.14100194988499481, -1.333735528292999906 ) ) ;
#26000 = CARTESIAN_POINT ( 'NONE',  ( -10.21026636380264740, -24.25606635949579371, -7.764233071689755405 ) ) ;
#26001 = CARTESIAN_POINT ( 'NONE',  ( 9.540682851482767290, -75.99946523393471409, 6.860877985616982144 ) ) ;
#26002 = CARTESIAN_POINT ( 'NONE',  ( -2.764837346328655965, -86.10000000000000853, 3.732097096069709963 ) ) ;
#26003 = ORIENTED_EDGE ( 'NONE', *, *, #40514, .F. ) ;
#26004 = DIRECTION ( 'NONE',  ( 0.000000000000000000, 1.000000000000000000, 0.000000000000000000 ) ) ;
#26005 = CARTESIAN_POINT ( 'NONE',  ( -0.9218200799623778030, -79.32708333333336270, 1.199500263597266914 ) ) ;
#26006 = CARTESIAN_POINT ( 'NONE',  ( 5.273774136544999713, -79.48694153719199562, -11.08023994795000000 ) ) ;
#26007 = CARTESIAN_POINT ( 'NONE',  ( -3.992195106911536673, -78.62148118236265759, 0.07526069398394277798 ) ) ;
#26008 = CARTESIAN_POINT ( 'NONE',  ( -1.588687380433000174, -83.30531615612299845, 0.5002921117598999601 ) ) ;
#26009 = CARTESIAN_POINT ( 'NONE',  ( -3.548303639235999896, -79.52895424076298525, -10.38621961377000069 ) ) ;
#26010 = CARTESIAN_POINT ( 'NONE',  ( 1.501534314746039600, -17.44847048340742290, 12.70455943740098803 ) ) ;
#26011 = CARTESIAN_POINT ( 'NONE',  ( -2.510140451105999926, -77.04989847029199268, -12.13002842542999993 ) ) ;
#26012 = CARTESIAN_POINT ( 'NONE',  ( -1.869988834943083544, -78.58576359787208787, 11.64790316465944819 ) ) ;
#26013 = CARTESIAN_POINT ( 'NONE',  ( -1.333333333333333259, -77.79999999999999716, 0.000000000000000000 ) ) ;
#26014 = VERTEX_POINT ( 'NONE', #31945 ) ;
#26015 = CARTESIAN_POINT ( 'NONE',  ( -9.643902624173000149, -79.18148518439899419, -5.356946570292000054 ) ) ;
#26016 = CARTESIAN_POINT ( 'NONE',  ( 0.4202526907024859981, -79.94806991484146863, 1.177036590369186397 ) ) ;
#26017 = CARTESIAN_POINT ( 'NONE',  ( 8.796335266379994522, -77.79791666666667993, -6.760013919724047859 ) ) ;
#26018 = CARTESIAN_POINT ( 'NONE',  ( -3.734118835908999845, -79.14521842720699851, 10.51417881607000027 ) ) ;
#26019 = ADVANCED_FACE ( 'NONE', ( #41698 ), #53338, .T. ) ;
#26020 = LINE ( 'NONE', #52904, #1925 ) ;
#26021 = DIRECTION ( 'NONE',  ( -0.7071067810866970005, 6.386274622742979319E-09, 0.7071067812863980340 ) ) ;
#26022 = CARTESIAN_POINT ( 'NONE',  ( 1.329645096041070840, -81.63878427981505581, 0.7189625959783054743 ) ) ;
#26023 = CARTESIAN_POINT ( 'NONE',  ( -12.15819904699000098, -78.83780308901600620, -1.724521706148000044 ) ) ;
#26024 = CIRCLE ( 'NONE', #29803, 10.05000000000000071 ) ;
#26025 = CIRCLE ( 'NONE', #13767, 12.25000000000000000 ) ;
#26026 = CARTESIAN_POINT ( 'NONE',  ( -10.75000000000000000, -79.50000000000000000, 0.000000000000000000 ) ) ;
#26027 = AXIS2_PLACEMENT_3D ( 'NONE', #50584, #54708, #36693 ) ;
#26028 = CARTESIAN_POINT ( 'NONE',  ( 2.062503053667999797, -20.24263462181000151, 12.92177931909999877 ) ) ;
#26029 = CARTESIAN_POINT ( 'NONE',  ( -11.75000000000000711, -76.28958333333332575, 1.538071403319954955 ) ) ;
#26030 = ORIENTED_EDGE ( 'NONE', *, *, #42244, .F. ) ;
#26031 = EDGE_CURVE ( 'NONE', #2177, #6475, #14694, .T. ) ;
#26032 = PRESENTATION_LAYER_ASSIGNMENT (  '', '', ( #12843 ) ) ;
#26033 = ORIENTED_EDGE ( 'NONE', *, *, #25505, .T. ) ;
#26034 = DIRECTION ( 'NONE',  ( -1.000000000000000000, 0.000000000000000000, 0.000000000000000000 ) ) ;
#26035 = ORIENTED_EDGE ( 'NONE', *, *, #9718, .T. ) ;
#26036 = CARTESIAN_POINT ( 'NONE',  ( -9.578019072079097640, -79.75346114563041056, -0.4234131151099537749 ) ) ;
#26037 = VERTEX_POINT ( 'NONE', #5390 ) ;
#26038 = CARTESIAN_POINT ( 'NONE',  ( -9.684478921172445354, -81.00000000000000000, -4.805145260639483773 ) ) ;
#26039 = CARTESIAN_POINT ( 'NONE',  ( -10.66734455299000039, -77.05636667169498821, 2.320156498608999751 ) ) ;
#26040 = ITEM_DEFINED_TRANSFORMATION ( 'NONE', 'NONE', #19717,  #43526 ) ;
#26041 = CARTESIAN_POINT ( 'NONE',  ( 0.6297217878212084674, -82.43399434138464699, 1.093297131891592278 ) ) ;
#26042 = CARTESIAN_POINT ( 'NONE',  ( -4.265506261528114962, -78.18699093222700469, -8.208995969611063259 ) ) ;
#26043 = CARTESIAN_POINT ( 'NONE',  ( 11.21485848424000054, -80.01459935801440793, -0.2123177049684000228 ) ) ;
#26044 = ORIENTED_EDGE ( 'NONE', *, *, #21945, .T. ) ;
#26045 = ORIENTED_EDGE ( 'NONE', *, *, #50594, .F. ) ;
#26046 = CARTESIAN_POINT ( 'NONE',  ( -7.039186935347679253, -77.54390228458088075, 6.000959365781699084 ) ) ;
#26047 = FACE_OUTER_BOUND ( 'NONE', #9940, .T. ) ;
#26048 = CARTESIAN_POINT ( 'NONE',  ( -2.486604901413153268, -77.50416666666664867, -9.252740428348998236 ) ) ;
#26049 = CARTESIAN_POINT ( 'NONE',  ( 5.417083560473000325, -79.00228060500298000, -8.051455326762999576 ) ) ;
#26050 = CARTESIAN_POINT ( 'NONE',  ( 7.654537085030000299, -23.28056692670000061, 10.01332844637000008 ) ) ;
#26051 = CARTESIAN_POINT ( 'NONE',  ( -4.985213779165269976, -79.48073246256258528, -8.086678520982406582 ) ) ;
#26052 = CARTESIAN_POINT ( 'NONE',  ( 12.76303204291999904, -55.53514849259999409, 1.980584515756000030 ) ) ;
#26053 = CARTESIAN_POINT ( 'NONE',  ( -8.254612054926999676, -79.81451948108198735, 6.886499823760000361 ) ) ;
#26054 = CARTESIAN_POINT ( 'NONE',  ( 12.79971535686000017, -18.20965922269000004, -2.019101350716999921 ) ) ;
#26055 = CARTESIAN_POINT ( 'NONE',  ( -9.929702205000999982, -24.63097880280000140, -7.973987073284000360 ) ) ;
#26056 = CARTESIAN_POINT ( 'NONE',  ( -5.684557159767956058, -78.57291666666664298, -7.396918292183169541 ) ) ;
#26057 = ORIENTED_EDGE ( 'NONE', *, *, #6580, .F. ) ;
#26058 = CARTESIAN_POINT ( 'NONE',  ( -9.608132404413000316, -79.02473885956399613, 7.328251847290000676 ) ) ;
#26059 = DIRECTION ( 'NONE',  ( 1.000000000000000000, 0.000000000000000000, 0.000000000000000000 ) ) ;
#26060 = CARTESIAN_POINT ( 'NONE',  ( 10.18066396183999878, -78.49586079892000612, 6.314281093748000728 ) ) ;
#26061 = CARTESIAN_POINT ( 'NONE',  ( -9.934825859755001431, -17.37633188891999936, -7.968960864700001423 ) ) ;
#26062 = CIRCLE ( 'NONE', #23258, 11.00000000000000000 ) ;
#26063 = ADVANCED_FACE ( 'NONE', ( #49400 ), #20355, .F. ) ;
#26065 = CARTESIAN_POINT ( 'NONE',  ( -1.582498447119000229, -17.84913877521999837, -12.55493832972999968 ) ) ;
#26064 = FACE_OUTER_BOUND ( 'NONE', #45524, .T. ) ;
#26066 = CARTESIAN_POINT ( 'NONE',  ( -1.243547092045951041, -78.91458333333333997, -9.500000000000000000 ) ) ;
#26067 = CARTESIAN_POINT ( 'NONE',  ( 10.55910102243999837, -59.58485473249000108, -7.642147947533000085 ) ) ;
#26068 = DIRECTION ( 'NONE',  ( -1.000000000000000000, 0.000000000000000000, 0.000000000000000000 ) ) ;
#26069 = CARTESIAN_POINT ( 'NONE',  ( 9.909229536192000865, -77.03400324167699864, -5.351741263869000065 ) ) ;
#26070 = DIRECTION ( 'NONE',  ( 0.000000000000000000, -1.000000000000000000, 0.000000000000000000 ) ) ;
#26071 = CARTESIAN_POINT ( 'NONE',  ( -3.214200885120999995, -80.72145419626957619, 10.78715111662000048 ) ) ;
#26072 = AXIS2_PLACEMENT_3D ( 'NONE', #28539, #20000, #2287 ) ;
#26073 = ADVANCED_FACE ( 'NONE', ( #14239 ), #53475, .F. ) ;
#26074 = CARTESIAN_POINT ( 'NONE',  ( -1.636392600175404999, -1.518396803410333895, 2.841196409148389890 ) ) ;
#26075 = CARTESIAN_POINT ( 'NONE',  ( 0.8537148449505999048, -54.09501854057999992, 12.43377424869000158 ) ) ;
#26076 = CARTESIAN_POINT ( 'NONE',  ( -2.858407197967999913, -77.19999999999998863, -8.797272775729998884 ) ) ;
#26077 = CIRCLE ( 'NONE', #27969, 12.50000000000000000 ) ;
#26078 = CARTESIAN_POINT ( 'NONE',  ( -3.710753042444999927, -2.736382899542999958, -0.8462355775293999294 ) ) ;
#26079 = CARTESIAN_POINT ( 'NONE',  ( 4.318672206561768867, -77.60826495664210256, -9.868970905821345951 ) ) ;
#26080 = CARTESIAN_POINT ( 'NONE',  ( -9.071080135827999769, -80.04268349419798767, -2.557679440262000448 ) ) ;
#26081 = AXIS2_PLACEMENT_3D ( 'NONE', #47514, #39189, #25041 ) ;
#26082 = CARTESIAN_POINT ( 'NONE',  ( -12.66232176271000043, -53.66513311386999874, 0.5079086068997999970 ) ) ;
#26083 = LINE ( 'NONE', #8085, #27083 ) ;
#26084 = CARTESIAN_POINT ( 'NONE',  ( -3.166600152060512929, -2.080649301304957177, 0.8522904230390753177 ) ) ;
#26085 = CARTESIAN_POINT ( 'NONE',  ( 9.372585790538634498, -79.13499999999999091, -1.790612804732438779 ) ) ;
#26086 = CARTESIAN_POINT ( 'NONE',  ( 0.2053964487923000126, -85.86974735065199127, 4.169813340600000195 ) ) ;
#26087 = CARTESIAN_POINT ( 'NONE',  ( -2.879226727952071574, -77.30416666666666003, -10.71369944335147473 ) ) ;
#26088 = B_SPLINE_CURVE_WITH_KNOTS ( 'NONE', 3,
 ( #2736, #20736, #11882, #36761, #16312, #42890, #34293, #20449, #29859, #54780, #37052, #38152, #47914, #45942, #23194, #11305, #34005, #56174, #2447, #38445, #29286, #56463, #47335, #16016, #5474, #50364, #14323, #33428, #41489, #32318, #27895, #9914, #15434, #1076, #55884, #51465, #20163, #29004, #47043, #6573, #24584, #42600, #2163, #15722, #33720, #3309, #48199, #22168, #58188, #25731, #44615, #7446, #4170, #53467, #49047, #21303, #12729, #3021, #48472, #40176, #26581, #35438, #8594, #39311, #16885, #12446, #17751, #44319, #53180, #25445, #35739, #13009, #26012, #30722, #53770, #31009 ),
 .UNSPECIFIED., .F., .F.,
 ( 4, 2, 2, 2, 2, 2, 1, 1, 2, 2, 2, 2, 1, 2, 2, 1, 1, 1, 2, 2, 2, 2, 2, 1, 1, 1, 1, 1, 2, 2, 2, 2, 2, 1, 1, 1, 2, 2, 2, 2, 1, 1, 2, 2, 2, 4 ),
 ( 0.000000000000000000, 0.06249999999998635813, 0.1249999999999727163, 0.1406249999999693023, 0.1425781249999689138, 0.1435546874999686917, 0.1445312499999684697, 0.1484374999999675815, 0.1562499999999656664, 0.1874999999999584499, 0.2499999999999439060, 0.2812499999999366618, 0.2851562499999358846, 0.2856445312499357181, 0.2861328124999355516, 0.2871093749999354405, 0.2890624999999352185, 0.2968749999999345524, 0.3124999999999332201, 0.3749999999999282241, 0.4374999999999232836, 0.4687499999999208411, 0.4843749999999195643, 0.4921874999999190092, 0.4960937499999186207, 0.4980468749999185096, 0.4990234374999184541, 0.4995117187499184541, 0.4997558593749183986, 0.4999999999999182876, 0.5624999999999316103, 0.5937499999999382716, 0.6093749999999416023, 0.6171874999999432676, 0.6210937499999440448, 0.6230468749999443778, 0.6240234374999445999, 0.6249999999999448219, 0.6874999999999542588, 0.7187499999999590328, 0.7343749999999613642, 0.7421874999999625855, 0.7460937499999631406, 0.7499999999999636957, 0.8749999999999819034, 1.000000000000000000 ),
 .UNSPECIFIED. ) ;
#26089 = DIRECTION ( 'NONE',  ( 0.000000000000000000, 1.000000000000000000, 0.000000000000000000 ) ) ;
#26090 = CARTESIAN_POINT ( 'NONE',  ( -5.822924921437000023, -77.62760228854999411, 9.505164171658000427 ) ) ;
#26091 = EDGE_CURVE ( 'NONE', #49809, #4894, #15763, .T. ) ;
#26092 = CARTESIAN_POINT ( 'NONE',  ( 1.151300139434892067, -81.88191447522581257, 0.4866929889698630163 ) ) ;
#26093 = CARTESIAN_POINT ( 'NONE',  ( 7.674614791488999721, -22.75100836106000202, 10.14948852564000070 ) ) ;
#26094 = CARTESIAN_POINT ( 'NONE',  ( -9.555818165766000405, -77.21055870928698539, -0.1257991660602000017 ) ) ;
#26095 = CARTESIAN_POINT ( 'NONE',  ( 0.1963495408493571015, -78.86458333333331439, 1.500000000000000444 ) ) ;
#26096 = DIRECTION ( 'NONE',  ( 0.000000000000000000, 0.000000000000000000, -1.000000000000000000 ) ) ;
#26097 = CARTESIAN_POINT ( 'NONE',  ( 2.601259834223990097, -80.24469330578341442, -10.43116776099581244 ) ) ;
#26098 = CARTESIAN_POINT ( 'NONE',  ( 12.65372179310999989, -20.24935286375000132, -1.750000000000000000 ) ) ;
#26099 = CARTESIAN_POINT ( 'NONE',  ( -10.10448976476253158, -17.54884052606732681, -7.864761218165275736 ) ) ;
#26100 = B_SPLINE_CURVE_WITH_KNOTS ( 'NONE', 3,
 ( #5750, #27883, #29058, #45930, #19050, #41188 ),
 .UNSPECIFIED., .F., .F.,
 ( 4, 2, 4 ),
 ( 0.000000000000000000, 0.5000000000000000000, 1.000000000000000000 ),
 .UNSPECIFIED. ) ;
#26101 = CARTESIAN_POINT ( 'NONE',  ( -8.850953919802000414, -79.55752168082800324, -8.146641040006999290 ) ) ;
#26102 = CARTESIAN_POINT ( 'NONE',  ( -0.3273598336528602548, -78.20425139990393859, -1.217721295151624750 ) ) ;
#26103 = CARTESIAN_POINT ( 'NONE',  ( 8.858182419534999852, -80.12637572403669139, 6.954620140474000678 ) ) ;
#26104 = CARTESIAN_POINT ( 'NONE',  ( -10.98363357722940314, -23.18990228819912147, -0.5998278677060955300 ) ) ;
#26105 = ORIENTED_EDGE ( 'NONE', *, *, #28870, .F. ) ;
#26106 = EDGE_CURVE ( 'NONE', #22699, #33522, #53824, .T. ) ;
#26107 = CARTESIAN_POINT ( 'NONE',  ( 1.980611416588517359, -23.52597731806571701, 12.74335092662995805 ) ) ;
#26108 = EDGE_CURVE ( 'NONE', #42165, #3688, #43111, .T. ) ;
#26109 = ORIENTED_EDGE ( 'NONE', *, *, #29073, .F. ) ;
#26110 = DIRECTION ( 'NONE',  ( 1.000000000000000000, 0.000000000000000000, 0.000000000000000000 ) ) ;
#26111 = AXIS2_PLACEMENT_3D ( 'NONE', #9666, #16851, #34833 ) ;
#26112 = ORIENTED_EDGE ( 'NONE', *, *, #10459, .F. ) ;
#26113 = DIRECTION ( 'NONE',  ( 0.000000000000000000, -1.000000000000000000, 0.000000000000000000 ) ) ;
#26114 = CARTESIAN_POINT ( 'NONE',  ( -9.254189652385859333, -79.84085386658529160, 5.469689899798553689 ) ) ;
#26115 = VECTOR ( 'NONE', #20283, 1000.000000000000000 ) ;
#26116 = CARTESIAN_POINT ( 'NONE',  ( -10.42930648941000094, -79.54953960801499591, 3.225667704544000092 ) ) ;
#26117 = CARTESIAN_POINT ( 'NONE',  ( -3.461633792564999812, -81.73994274751999001, -0.7737321657921999440 ) ) ;
#26118 = CARTESIAN_POINT ( 'NONE',  ( -0.7691824896752659235, -79.28114364237121947, 9.473166916040263175 ) ) ;
#26119 = ORIENTED_EDGE ( 'NONE', *, *, #48742, .F. ) ;
#26120 = CARTESIAN_POINT ( 'NONE',  ( -3.203604947276998960, -77.74842935028665636, 10.56508708802999941 ) ) ;
#26121 = CARTESIAN_POINT ( 'NONE',  ( -3.402929133075000223, -78.31652404215999752, 11.45270446182999891 ) ) ;
#26122 = VECTOR ( 'NONE', #18521, 1000.000000000000000 ) ;
#26123 = ORIENTED_EDGE ( 'NONE', *, *, #12471, .F. ) ;
#26124 = VERTEX_POINT ( 'NONE', #55566 ) ;
#26125 = FACE_OUTER_BOUND ( 'NONE', #28655, .T. ) ;
#26126 = FACE_BOUND ( 'NONE', #39898, .T. ) ;
#26127 = AXIS2_PLACEMENT_3D ( 'NONE', #41725, #28421, #47055 ) ;
#26128 = CARTESIAN_POINT ( 'NONE',  ( 7.720144650974280154, -79.79999999999998295, 9.058211719984365473 ) ) ;
#26129 = CARTESIAN_POINT ( 'NONE',  ( -8.684598835271984285, -80.05006380143068156, 6.335413721204657733 ) ) ;
#26130 = DIRECTION ( 'NONE',  ( 0.000000000000000000, 1.000000000000000000, 0.000000000000000000 ) ) ;
#26131 = EDGE_CURVE ( 'NONE', #34809, #22868, #26879, .T. ) ;
#26132 = CARTESIAN_POINT ( 'NONE',  ( -4.276761386645500984, -86.40321104920798234, -0.4093923530758877827 ) ) ;
#26133 = CARTESIAN_POINT ( 'NONE',  ( 8.154961773732001262, -76.21165749863600070, 7.653135223926000208 ) ) ;
#26134 = CARTESIAN_POINT ( 'NONE',  ( 1.235365857667927836, -79.04166666667985908, 11.79166666709374134 ) ) ;
#26135 = CARTESIAN_POINT ( 'NONE',  ( -3.250880417296999614, -76.64007569364000005, 12.21627067396000044 ) ) ;
#26136 = CARTESIAN_POINT ( 'NONE',  ( 9.615022378355000399, -76.16851043297199908, -5.341629093326000444 ) ) ;
#26137 = CARTESIAN_POINT ( 'NONE',  ( -6.464912241513801260E-06, -79.20362641130290626, -11.95086305119197689 ) ) ;
#26138 = CARTESIAN_POINT ( 'NONE',  ( -3.095264676899999845, -82.06107264098699261, -2.734565311734000304 ) ) ;
#26139 = CARTESIAN_POINT ( 'NONE',  ( -10.42272502862000039, -58.55453807205000061, 7.691893942725999800 ) ) ;
#26140 = CARTESIAN_POINT ( 'NONE',  ( -2.299886044274590535, -3.037960577415522945, 2.295943121830337663 ) ) ;
#26141 = CARTESIAN_POINT ( 'NONE',  ( -3.543454320287000137, -80.20180496681199145, 0.1596678892961000129 ) ) ;
#26142 = EDGE_CURVE ( 'NONE', #21397, #58285, #23302, .T. ) ;
#26143 = FACE_OUTER_BOUND ( 'NONE', #55464, .T. ) ;
#26144 = CARTESIAN_POINT ( 'NONE',  ( -3.380058860739000082, -86.16144503318800218, 0.3695796539080999921 ) ) ;
#26145 = CARTESIAN_POINT ( 'NONE',  ( -3.804208684430999909, -3.319815397808000057, -0.1186911049137999996 ) ) ;
#26146 = CARTESIAN_POINT ( 'NONE',  ( 3.399999999999999911, -78.69999999999998863, 0.000000000000000000 ) ) ;
#26147 = ADVANCED_FACE ( 'NONE', ( #35420 ), #818, .F. ) ;
#26148 = ORIENTED_EDGE ( 'NONE', *, *, #43456, .T. ) ;
#26149 = CARTESIAN_POINT ( 'NONE',  ( -6.606377239730343298, -80.07291666666665719, -8.596418555780429571 ) ) ;
#26150 = DIRECTION ( 'NONE',  ( 1.000000000000000000, 0.000000000000000000, 0.000000000000000000 ) ) ;
#26151 = CARTESIAN_POINT ( 'NONE',  ( -0.1832406609208000192, -81.79214437619499734, -1.320984106490000087 ) ) ;
#26152 = CARTESIAN_POINT ( 'NONE',  ( -12.43356773666999970, -17.28739071017999862, -0.8411682846947000636 ) ) ;
#26153 = CARTESIAN_POINT ( 'NONE',  ( -3.274010471232999819, -77.44723873689001437, 12.59444704299999884 ) ) ;
#26154 = VECTOR ( 'NONE', #5794, 1000.000000000000000 ) ;
#26155 = CARTESIAN_POINT ( 'NONE',  ( -8.058638732054999920, -78.36893127911199031, -7.451332657186999775 ) ) ;
#26156 = CARTESIAN_POINT ( 'NONE',  ( -10.42531124908000173, -60.06485148440999922, -7.624341765471999821 ) ) ;
#26157 = CARTESIAN_POINT ( 'NONE',  ( -5.178179572192000535, -75.67130441998999402, -10.91684957994999827 ) ) ;
#26158 = B_SPLINE_CURVE_WITH_KNOTS ( 'NONE', 3,
 ( #38240, #19659, #6661, #37660, #55675, #51263 ),
 .UNSPECIFIED., .F., .F.,
 ( 4, 2, 4 ),
 ( 0.000000000000000000, 0.5000000000000000000, 1.000000000000000000 ),
 .UNSPECIFIED. ) ;
#26159 = ORIENTED_EDGE ( 'NONE', *, *, #6182, .F. ) ;
#26160 = DIRECTION ( 'NONE',  ( 0.000000000000000000, 0.000000000000000000, -1.000000000000000000 ) ) ;
#26161 = FACE_OUTER_BOUND ( 'NONE', #45060, .T. ) ;
#26162 = CIRCLE ( 'NONE', #45022, 9.000000000000000000 ) ;
#26163 = CARTESIAN_POINT ( 'NONE',  ( 0.6345915023811000699, -80.90716293419500005, -1.146778027003000133 ) ) ;
#26164 = CARTESIAN_POINT ( 'NONE',  ( -1.931086388455000025, -23.29778595484999926, -12.71798280855999863 ) ) ;
#26165 = CARTESIAN_POINT ( 'NONE',  ( 4.510926502723999754, -77.72927130271399676, 8.509098192649000580 ) ) ;
#26166 = AXIS2_PLACEMENT_3D ( 'NONE', #22227, #27525, #17216 ) ;
#26167 = CARTESIAN_POINT ( 'NONE',  ( -2.684629700338999836, -83.35175613119999127, -3.197244650393999965 ) ) ;
#26168 = CARTESIAN_POINT ( 'NONE',  ( 1.808012550523518946, -79.96190839373853976, 10.59665058875179788 ) ) ;
#26169 = CARTESIAN_POINT ( 'NONE',  ( 1.061497194196000082, -80.23402853000399659, -1.082666072229000020 ) ) ;
#26170 = VERTEX_POINT ( 'NONE', #6723 ) ;
#26171 = CYLINDRICAL_SURFACE ( 'NONE', #57902, 10.14999999999999858 ) ;
#26172 = CARTESIAN_POINT ( 'NONE',  ( -8.956130479881542428, -79.07960960748528123, 2.390097164946143327 ) ) ;
#26173 = VECTOR ( 'NONE', #19388, 1000.000000000000114 ) ;
#26174 = CARTESIAN_POINT ( 'NONE',  ( -3.437187628289000152, -78.85171435493609238, -1.442231121412212840E-14 ) ) ;
#26175 = VERTEX_POINT ( 'NONE', #51896 ) ;
#26176 = ORIENTED_EDGE ( 'NONE', *, *, #18203, .T. ) ;
#26177 = CARTESIAN_POINT ( 'NONE',  ( -0.5177219211888000050, -78.99204636544698133, -10.92793577709999830 ) ) ;
#26178 = CARTESIAN_POINT ( 'NONE',  ( -10.45205659047000069, -56.03767314774999875, 7.651160337227000063 ) ) ;
#26179 = CARTESIAN_POINT ( 'NONE',  ( -7.000000000000000000, -81.10000000285099020, 0.000000000000000000 ) ) ;
#26180 = ORIENTED_EDGE ( 'NONE', *, *, #19809, .F. ) ;
#26181 = ORIENTED_EDGE ( 'NONE', *, *, #16020, .T. ) ;
#26182 = ORIENTED_EDGE ( 'NONE', *, *, #38342, .F. ) ;
#26183 = FACE_OUTER_BOUND ( 'NONE', #57131, .T. ) ;
#26184 = CARTESIAN_POINT ( 'NONE',  ( 2.030241441219323928, -1.014979566676556644, -3.469969701195170231 ) ) ;
#26185 = B_SPLINE_SURFACE_WITH_KNOTS ( 'NONE', 3, 3, ( 
 ( #25048, #29747, #47800, #34179 ),
 ( #20908, #11492, #7620, #25908 ),
 ( #38910, #52785, #21194, #12338 ),
 ( #7332, #29180, #42780, #39195 ),
 ( #57209, #47227, #43070, #6758 ),
 ( #15615, #25333, #30327, #24768 ),
 ( #15908, #20337, #38332, #33893 ),
 ( #29465, #3479, #30620, #49531 ),
 ( #57785, #13784, #53958, #40665 ),
 ( #8196, #9077, #31486, #44799 ),
 ( #49229, #9375, #31189, #8780 ),
 ( #26771, #35038, #27064, #58375 ),
 ( #13495, #30903, #45103, #4051 ),
 ( #4657, #49828, #31784, #22053 ),
 ( #35928, #21485, #4351, #40062 ),
 ( #39771, #22656, #257, #39492 ),
 ( #12903, #57495, #40367, #26475 ) ),
 .UNSPECIFIED., .F., .F., .F.,
 ( 4, 1, 1, 1, 1, 1, 1, 1, 1, 1, 1, 1, 1, 1, 4 ),
 ( 4, 4 ),
 ( -0.01011786823680000010, 0.000000000000000000, 0.08333333333333001192, 0.1666666666667000196, 0.2500000000000000000, 0.3333333333333000081, 0.4166666666666999919, 0.5000000000000000000, 0.5833333333333000637, 0.6666666666667000474, 0.7500000000000000000, 0.8333333333333000637, 0.9166666666667000474, 1.000000000000000000, 1.010371592463000123 ),
 ( -0.3559705548529999986, 1.357613344742000017 ),
 .UNSPECIFIED. ) ;
#26186 = VERTEX_POINT ( 'NONE', #50741 ) ;
#26187 = CARTESIAN_POINT ( 'NONE',  ( -0.9215901096570091600, -81.82721060988042439, 1.199517572493949524 ) ) ;
#26188 = EDGE_LOOP ( 'NONE', ( #32353, #26320, #14289, #42556, #22325, #48218, #32866, #35651 ) ) ;
#26189 = CARTESIAN_POINT ( 'NONE',  ( -11.55418265775999842, -79.02279858628688203, 4.110954701505000308 ) ) ;
#26190 = CARTESIAN_POINT ( 'NONE',  ( 2.024107680232116291, -78.91452042059378869, -3.504731529255688649 ) ) ;
#26191 = CARTESIAN_POINT ( 'NONE',  ( 12.65375411747000101, -58.54977139013999476, -1.750000000000000000 ) ) ;
#26192 = EDGE_CURVE ( 'NONE', #10827, #50383, #5397, .T. ) ;
#26193 = CARTESIAN_POINT ( 'NONE',  ( -7.705119999407000542, -21.75171076523999858, -10.24996238026999862 ) ) ;
#26194 = DIRECTION ( 'NONE',  ( 1.000000000000000000, 0.000000000000000000, 0.000000000000000000 ) ) ;
#26195 = ADVANCED_FACE ( 'NONE', ( #41864 ), #18227, .T. ) ;
#26196 = CARTESIAN_POINT ( 'NONE',  ( -3.097937178131073832, -80.45257242543718235, -10.77438633444702809 ) ) ;
#26197 = CARTESIAN_POINT ( 'NONE',  ( 7.691893942748999180, -57.04546192861999998, -10.42272502865000128 ) ) ;
#26198 = CARTESIAN_POINT ( 'NONE',  ( 9.177871051388377666, -78.84012010996477215, -1.162879483702742744 ) ) ;
#26199 = CARTESIAN_POINT ( 'NONE',  ( 4.000000000000000000, -74.80000000000001137, -0.5999999999999999778 ) ) ;
#26200 = CARTESIAN_POINT ( 'NONE',  ( -2.945894689509000131, -81.45550264934799145, 2.958260330776999680 ) ) ;
#26201 = CARTESIAN_POINT ( 'NONE',  ( 4.937899134609000207, -77.58968667140099740, 8.421832810844000150 ) ) ;
#26202 = DIRECTION ( 'NONE',  ( 0.7071067811814418791, 1.254536121802073994E-07, 0.7071067811916420531 ) ) ;
#26203 = AXIS2_PLACEMENT_3D ( 'NONE', #1159, #4697, #14697 ) ;
#26204 = DIRECTION ( 'NONE',  ( 0.000000000000000000, 0.000000000000000000, -1.000000000000000000 ) ) ;
#26205 = CARTESIAN_POINT ( 'NONE',  ( 0.000000000000000000, -81.19999999999998863, -7.000000000000000000 ) ) ;
#26206 = CARTESIAN_POINT ( 'NONE',  ( 7.137508353459041111, -79.91917351108399714, 8.454853940648142441 ) ) ;
#26207 = ADVANCED_FACE ( 'NONE', ( #13203, #35636 ), #45114, .T. ) ;
#26208 = CARTESIAN_POINT ( 'NONE',  ( -8.866178467950035724, -78.14940218639688396, -6.303320502543174442 ) ) ;
#26209 = CARTESIAN_POINT ( 'NONE',  ( -1.118791686563179066, -79.90798387919549839, -1.016611780088532591 ) ) ;
#26210 = CARTESIAN_POINT ( 'NONE',  ( -0.8247866532291000530, -77.07501358598499053, -9.454605849501000137 ) ) ;
#26211 = DIRECTION ( 'NONE',  ( -1.000000000000000000, 0.000000000000000000, 0.000000000000000000 ) ) ;
#26212 = DIRECTION ( 'NONE',  ( -1.000000000000000000, 0.000000000000000000, 0.000000000000000000 ) ) ;
#26213 = CARTESIAN_POINT ( 'NONE',  ( 7.671012283914000029, -78.19471668781000062, 9.589126640163000204 ) ) ;
#26214 = FACE_OUTER_BOUND ( 'NONE', #10741, .T. ) ;
#26215 = EDGE_CURVE ( 'NONE', #46084, #57578, #17524, .T. ) ;
#26217 = DIRECTION ( 'NONE',  ( 1.000000000000000000, 0.000000000000000000, 0.000000000000000000 ) ) ;
#26216 = FACE_OUTER_BOUND ( 'NONE', #17990, .T. ) ;
#26218 = CARTESIAN_POINT ( 'NONE',  ( -1.339567984323000172, -82.67693514403299559, -0.6016691479808000675 ) ) ;
#26219 = CARTESIAN_POINT ( 'NONE',  ( -8.824274837635110558, -79.55161701906600058, 6.149812313655782070 ) ) ;
#26220 = ORIENTED_EDGE ( 'NONE', *, *, #40283, .T. ) ;
#26221 = CARTESIAN_POINT ( 'NONE',  ( -0.1636246173744673738, -82.11458333333330017, -1.249999999999999778 ) ) ;
#26222 = CARTESIAN_POINT ( 'NONE',  ( -9.391088595540001194, -79.24495288497600143, -7.536558092107000562 ) ) ;
#26223 = ADVANCED_FACE ( 'NONE', ( #26485 ), #29762, .F. ) ;
#26224 = CARTESIAN_POINT ( 'NONE',  ( -5.908174908109000256, -80.99493105630590151, 8.927771479942999022 ) ) ;
#26225 = DIRECTION ( 'NONE',  ( -1.000000000000000000, 0.000000000000000000, 0.000000000000000000 ) ) ;
#26226 = CARTESIAN_POINT ( 'NONE',  ( -10.13694968399000018, -60.50834319308000175, 7.646073915548999622 ) ) ;
#26227 = DIRECTION ( 'NONE',  ( 0.000000000000000000, 1.000000000000000000, -1.646830819861000174E-14 ) ) ;
#26228 = CARTESIAN_POINT ( 'NONE',  ( 7.129854210758000299, -80.08175381071399102, 6.855691147963000276 ) ) ;
#26229 = CARTESIAN_POINT ( 'NONE',  ( 12.77649794757999935, -25.30831393477999924, 0.06464137375187999079 ) ) ;
#26230 = DIRECTION ( 'NONE',  ( 0.000000000000000000, -1.000000000000000000, 0.000000000000000000 ) ) ;
#26231 = ORIENTED_EDGE ( 'NONE', *, *, #41232, .T. ) ;
#26232 = CARTESIAN_POINT ( 'NONE',  ( -10.14999999998000035, -87.10000000002298748, 2.878919856867000406E-10 ) ) ;
#26233 = CARTESIAN_POINT ( 'NONE',  ( -1.500000000000000000, -78.50000000000000000, 0.000000000000000000 ) ) ;
#26234 = AXIS2_PLACEMENT_3D ( 'NONE', #3018, #2444, #24869 ) ;
#26235 = CARTESIAN_POINT ( 'NONE',  ( -1.318116285635148266, -1.693330829645463664, -3.001025458541523694 ) ) ;
#26236 = DIRECTION ( 'NONE',  ( 0.000000000000000000, -1.000000000000000000, 0.000000000000000000 ) ) ;
#26237 = CARTESIAN_POINT ( 'NONE',  ( 1.925855953377999974, -85.19317953870898918, -2.979199794438999849 ) ) ;
#26238 = ORIENTED_EDGE ( 'NONE', *, *, #28627, .T. ) ;
#26239 = B_SPLINE_CURVE_WITH_KNOTS ( 'NONE', 3,
 ( #12967, #8263, #53423, #2973, #21259, #52279, #26543, #34823, #44569, #25971, #47866, #25685, #7396, #26263, #34244, #39264, #30966, #57853, #17120, #12117, #52851, #48153, #43712, #4124, #35105, #7973, #30395, #48431, #3267, #43997, #3547, #38688, #44276, #43415, #3835, #21832, #39555, #57559, #53139, #39838, #17410, #56708, #12687, #30680, #29815, #16265, #48718, #16550, #25398, #7684, #20972, #56988, #30102, #44870, #4423, #35699, #22124, #54318, #54022, #22720, #5007, #40733, #13858, #26, #14145, #32144, #40135, #13564, #31554, #17714, #614, #45171, #50183, #18006, #53728, #18878, #10026, #35997, #9729, #4721, #9149, #40436, #31854, #49895, #9439, #22423, #45465, #324, #18302, #54607, #13267, #27133, #31258, #49300, #36295, #41312, #8851, #28007, #27430, #49602, #23012, #45762, #18596, #26841, #23304, #27718, #5296, #41023, #36585, #897, #36874 ),
 .UNSPECIFIED., .F., .F.,
 ( 4, 2, 2, 2, 1, 1, 1, 1, 1, 2, 2, 2, 2, 2, 1, 1, 1, 1, 1, 2, 2, 2, 2, 2, 1, 1, 1, 1, 1, 2, 2, 2, 2, 2, 1, 1, 1, 1, 1, 2, 2, 2, 2, 2, 1, 1, 1, 1, 1, 2, 2, 2, 2, 2, 1, 1, 1, 1, 1, 2, 2, 2, 2, 2, 1, 1, 1, 1, 1, 2, 2, 2, 4 ),
 ( 0.000000000000000000, 0.06249999999997328526, 0.09374999999995992095, 0.1093749999999532596, 0.1171874999999499428, 0.1210937499999483052, 0.1230468749999474448, 0.1240234374999469730, 0.1245117187499466260, 0.1247558593749464040, 0.1249999999999461681, 0.1874999999998897826, 0.2187499999998615552, 0.2343749999998474831, 0.2421874999998404610, 0.2460937499998369360, 0.2480468749998351596, 0.2490234374998342437, 0.2495117187498337996, 0.2497558593748335498, 0.2499999999998333000, 0.3124999999997782330, 0.3437499999997506439, 0.3593749999997368216, 0.3671874999997298827, 0.3710937499997263855, 0.3730468749997248867, 0.3740234374997239430, 0.3745117187497231659, 0.3747558593747231104, 0.3749999999997231104, 0.4374999999997050137, 0.4687499999996960764, 0.4843749999996914135, 0.4921874999996889710, 0.4960937499996877498, 0.4980468749996871392, 0.4990234374996866396, 0.4995117187496862510, 0.4997558593746861955, 0.4999999999996861400, 0.5624999999996663780, 0.5937499999996566080, 0.6093749999996517230, 0.6171874999996492805, 0.6210937499996478373, 0.6230468749996470601, 0.6240234374996471711, 0.6245117187496469491, 0.6247558593746470601, 0.6249999999996471711, 0.6874999999996908029, 0.7187499999997127853, 0.7343749999997238875, 0.7421874999997295497, 0.7460937499997323252, 0.7480468749997337685, 0.7490234374997345457, 0.7495117187497348787, 0.7497558593747349898, 0.7499999999997351008, 0.8124999999997707389, 0.8437499999997886135, 0.8593749999997974953, 0.8671874999998018252, 0.8710937499998042677, 0.8730468749998057110, 0.8740234374998065991, 0.8745117187498072653, 0.8747558593748075983, 0.8749999999998079314, 0.9374999999999040767, 1.000000000000000000 ),
 .UNSPECIFIED. ) ;
#26240 = CARTESIAN_POINT ( 'NONE',  ( 10.35453599130000057, -76.65783510652001098, -6.064947188958000446 ) ) ;
#26241 = DIRECTION ( 'NONE',  ( 0.7071067811865970887, 0.000000000000000000, 0.7071067811864981678 ) ) ;
#26242 = CARTESIAN_POINT ( 'NONE',  ( -1.618935784558787949, -54.87248831271473648, -12.52134385796515836 ) ) ;
#26243 = ORIENTED_EDGE ( 'NONE', *, *, #2763, .F. ) ;
#26244 = VECTOR ( 'NONE', #22504, 1000.000000000000000 ) ;
#26245 = CARTESIAN_POINT ( 'NONE',  ( -9.934825859728000808, -54.17633188858999915, -7.968960864672001598 ) ) ;
#26246 = CARTESIAN_POINT ( 'NONE',  ( -4.465297566879000257, -79.68263247063998733, 8.686876450551999085 ) ) ;
#26247 = VERTEX_POINT ( 'NONE', #9384 ) ;
#26248 = ORIENTED_EDGE ( 'NONE', *, *, #36092, .T. ) ;
#26249 = B_SPLINE_CURVE_WITH_KNOTS ( 'NONE', 3,
 ( #45486, #5030, #50204, #23032, #36317, #9753, #4150, #31875, #45193, #27739 ),
 .UNSPECIFIED., .F., .F.,
 ( 4, 2, 2, 2, 4 ),
 ( 0.2499999978686767710, 0.4374999984015075505, 0.6249999989343384410, 0.8124999994671692205, 1.000000000000000000 ),
 .UNSPECIFIED. ) ;
#26250 = CARTESIAN_POINT ( 'NONE',  ( -6.054010968653000369, -76.10689905944899181, 10.76718068125000016 ) ) ;
#26251 = DIRECTION ( 'NONE',  ( -0.7071067811865475727, 0.000000000000000000, -0.7071067811865475727 ) ) ;
#26252 = CARTESIAN_POINT ( 'NONE',  ( -0.5985389898873999526, -79.29977142615000218, -1.413233628500000005 ) ) ;
#26253 = ORIENTED_EDGE ( 'NONE', *, *, #30923, .F. ) ;
#26254 = CARTESIAN_POINT ( 'NONE',  ( 2.962511214703000384, -77.84040584965400456, -9.021140561863999707 ) ) ;
#26255 = FACE_OUTER_BOUND ( 'NONE', #45603, .T. ) ;
#26256 = CARTESIAN_POINT ( 'NONE',  ( 0.1323978365314348593, -80.23382476822598619, -1.243286041401693742 ) ) ;
#26257 = CARTESIAN_POINT ( 'NONE',  ( -3.226165562315000290, -77.88915923096000427, 12.71052925661000010 ) ) ;
#26258 = PRODUCT_DEFINITION_CONTEXT ( 'detailed design', #36048, 'design' ) ;
#26259 = CARTESIAN_POINT ( 'NONE',  ( 3.113304451009999863, -78.39783470746900207, -10.55022916317000181 ) ) ;
#26260 = CARTESIAN_POINT ( 'NONE',  ( 13.13047446164998711, -22.78578169018998878, -0.8260994316375004365 ) ) ;
#26261 = CARTESIAN_POINT ( 'NONE',  ( 4.093343120888133235, -86.36264282632899381, 0.4698497371738549200 ) ) ;
#26262 = CARTESIAN_POINT ( 'NONE',  ( 7.910349975595998728, -79.71439497653800288, 7.952639426948999279 ) ) ;
#26263 = CARTESIAN_POINT ( 'NONE',  ( -0.7267300686164063217, -79.98135465499143493, 9.221345538712327539 ) ) ;
#26264 = CARTESIAN_POINT ( 'NONE',  ( 9.355955347604632877, -16.82516908802490008, 8.610895743743158803 ) ) ;
#26265 = ORIENTED_EDGE ( 'NONE', *, *, #58151, .T. ) ;
#26266 = CARTESIAN_POINT ( 'NONE',  ( 2.618044012240999585, -78.76447634179098145, -10.95786383906999895 ) ) ;
#26267 = CARTESIAN_POINT ( 'NONE',  ( 10.54796701376999835, -75.81043591312999297, 6.346365727669000201 ) ) ;
#26268 = CARTESIAN_POINT ( 'NONE',  ( -0.5815971981373999622, -79.88867704943100989, -1.292982629223000002 ) ) ;
#26269 = CARTESIAN_POINT ( 'NONE',  ( 11.70615142939037590, -76.45809945638056604, 1.224787512100862230 ) ) ;
#26270 = CARTESIAN_POINT ( 'NONE',  ( 1.749899258080120479, -60.18716848725620139, -12.55433901293723586 ) ) ;
#26271 = CARTESIAN_POINT ( 'NONE',  ( -3.264119181477372678, -3.379906652641984088, -1.321296673820179457 ) ) ;
#26272 = VECTOR ( 'NONE', #7912, 1000.000000000000000 ) ;
#26273 = CARTESIAN_POINT ( 'NONE',  ( 12.58335110161999815, -21.74888345808999901, 1.667961430005999945 ) ) ;
#26274 = CARTESIAN_POINT ( 'NONE',  ( 7.958776492191999452, -24.47699850276000078, -9.723157982392999443 ) ) ;
#26275 = DIRECTION ( 'NONE',  ( 0.000000000000000000, 1.000000000000000000, 0.000000000000000000 ) ) ;
#26276 = CARTESIAN_POINT ( 'NONE',  ( -10.64215094251999894, -79.97579375008199065, 2.340290094375000240 ) ) ;
#26277 = EDGE_CURVE ( 'NONE', #46351, #37150, #17947, .T. ) ;
#26278 = CARTESIAN_POINT ( 'NONE',  ( 10.07719973192000040, -21.74888345808999901, -7.718346056094000041 ) ) ;
#26279 = CARTESIAN_POINT ( 'NONE',  ( -0.7704861717791524622, -83.02778078094171121, 0.9968608840825577966 ) ) ;
#26280 = CARTESIAN_POINT ( 'NONE',  ( -4.167881196010999822, -80.17042173478499478, 0.1879410564025000008 ) ) ;
#26281 = CARTESIAN_POINT ( 'NONE',  ( -10.75000000000000355, -77.98958333333328596, 1.407171709420384609 ) ) ;
#26282 = VERTEX_POINT ( 'NONE', #22063 ) ;
#26283 = CARTESIAN_POINT ( 'NONE',  ( -1.486328135279999962, -82.42166142315099364, -0.5524720742449998889 ) ) ;
#26284 = CARTESIAN_POINT ( 'NONE',  ( -1.320073427535999988, -80.92057293764999315, 0.6433150820290999272 ) ) ;
#26285 = LINE ( 'NONE', #57875, #9735 ) ;
#26286 = CARTESIAN_POINT ( 'NONE',  ( -11.48784787867999846, -78.02120198485400238, -3.397854551190000016 ) ) ;
#26287 = LINE ( 'NONE', #52877, #42911 ) ;
#26288 = CARTESIAN_POINT ( 'NONE',  ( 0.7311670807272000472, -82.05001763639998558, 1.496881327486000002 ) ) ;
#26289 = CIRCLE ( 'NONE', #57409, 1.250000000000000000 ) ;
#26290 = CARTESIAN_POINT ( 'NONE',  ( -3.073538647258000189, -78.18086335765900685, -11.53207971834999945 ) ) ;
#26291 = CARTESIAN_POINT ( 'NONE',  ( 1.899930039692999895, -78.54950584965399685, 9.535935523283001203 ) ) ;
#26292 = CARTESIAN_POINT ( 'NONE',  ( -7.696817093642000174, -77.59296661922998339, 5.606191475415999825 ) ) ;
#26293 = CARTESIAN_POINT ( 'NONE',  ( -9.841120606706802221, -24.83627250047061352, -8.121699444506939258 ) ) ;
#26294 = CARTESIAN_POINT ( 'NONE',  ( 10.85714576078767735, -75.98073128594312209, 4.491944191334621195 ) ) ;
#26295 = CARTESIAN_POINT ( 'NONE',  ( 3.618614839418320184, -85.83735716284300565, 2.628308734608108654 ) ) ;
#26296 = ORIENTED_EDGE ( 'NONE', *, *, #56573, .T. ) ;
#26297 = CARTESIAN_POINT ( 'NONE',  ( 0.7554284705563452107, -79.23333333333330586, 1.310679582531388609 ) ) ;
#26298 = CARTESIAN_POINT ( 'NONE',  ( 11.31412585176551389, -78.97437522268991472, 3.657762637097759395 ) ) ;
#26299 = EDGE_CURVE ( 'NONE', #29230, #11806, #53653, .T. ) ;
#26300 = CARTESIAN_POINT ( 'NONE',  ( -2.398287624620659475, -78.69999999999998863, -3.977573462190958420 ) ) ;
#26301 = CARTESIAN_POINT ( 'NONE',  ( 3.176617583302000281, -79.78178542975699372, 10.50586082162000068 ) ) ;
#26302 = DIRECTION ( 'NONE',  ( -1.000000000000000000, 3.441642669434999888E-11, 0.000000000000000000 ) ) ;
#26303 = CARTESIAN_POINT ( 'NONE',  ( 4.699868689641999886, -76.59710561063300815, -11.46072718019999925 ) ) ;
#26304 = CARTESIAN_POINT ( 'NONE',  ( -0.1955901218635645589, -79.56269089637430625, -1.318552432567616783 ) ) ;
#26305 = DIRECTION ( 'NONE',  ( -1.000000000000000000, 0.000000000000000000, 0.000000000000000000 ) ) ;
#26306 = ORIENTED_EDGE ( 'NONE', *, *, #57095, .F. ) ;
#26307 = CARTESIAN_POINT ( 'NONE',  ( 10.56933735542999919, -79.98459350986080096, 3.541701167072000445 ) ) ;
#26308 = CARTESIAN_POINT ( 'NONE',  ( 7.054366762047179940, -77.30619333359085488, 6.026930045153958027 ) ) ;
#26309 = CARTESIAN_POINT ( 'NONE',  ( -6.760013919724058518, -77.67291666666665151, -8.796335266379987416 ) ) ;
#26310 = B_SPLINE_CURVE_WITH_KNOTS ( 'NONE', 3,
 ( #34767, #16786, #30045, #17066, #7342, #3490, #11500, #56366, #6766, #12348, #47529, #21494, #29474, #25057, #47811, #57504, #39500, #30335 ),
 .UNSPECIFIED., .F., .F.,
 ( 4, 2, 2, 2, 2, 2, 2, 2, 4 ),
 ( 0.000000000000000000, 0.1250000000000000833, 0.2500000000000001110, 0.3750000000000000000, 0.4999999999999999445, 0.6249999999999998890, 0.7499999999999997780, 0.8749999999999998890, 1.000000000000000000 ),
 .UNSPECIFIED. ) ;
#26311 = CARTESIAN_POINT ( 'NONE',  ( -2.183649677207000206, -78.19776941201399723, 10.83095413486000069 ) ) ;
#26312 = CARTESIAN_POINT ( 'NONE',  ( 7.601397897754999633, -23.25000000000000000, -9.369164850722000892 ) ) ;
#26313 = CARTESIAN_POINT ( 'NONE',  ( 1.106525018319362674, -81.65902809546365404, 1.029255714463842786 ) ) ;
#26314 = EDGE_CURVE ( 'NONE', #49897, #44346, #2460, .T. ) ;
#26315 = CARTESIAN_POINT ( 'NONE',  ( -12.03507225495000199, -78.81067377359200066, 2.439839133843999974 ) ) ;
#26316 = VECTOR ( 'NONE', #7505, 1000.000000000000000 ) ;
#26317 = DIRECTION ( 'NONE',  ( 0.000000000000000000, 1.000000000000000000, 0.000000000000000000 ) ) ;
#26318 = DIRECTION ( 'NONE',  ( 0.7071067811865474617, 0.000000000000000000, -0.7071067811865474617 ) ) ;
#26319 = FACE_OUTER_BOUND ( 'NONE', #37669, .T. ) ;
#26320 = ORIENTED_EDGE ( 'NONE', *, *, #40880, .T. ) ;
#26321 = ORIENTED_EDGE ( 'NONE', *, *, #40478, .T. ) ;
#26322 = DIRECTION ( 'NONE',  ( -1.000000000000000000, 0.000000000000000000, 0.000000000000000000 ) ) ;
#26323 = VECTOR ( 'NONE', #36119, 1000.000000000000114 ) ;
#26324 = EDGE_LOOP ( 'NONE', ( #5358, #20678, #18332, #239, #18320 ) ) ;
#26325 = CARTESIAN_POINT ( 'NONE',  ( 11.81418954875000082, -78.82361295229000575, 3.289986436736999753 ) ) ;
#26326 = ORIENTED_EDGE ( 'NONE', *, *, #23149, .T. ) ;
#26327 = CARTESIAN_POINT ( 'NONE',  ( 10.15323304112999914, -24.23079616014999971, 7.760925857005999795 ) ) ;
#26328 = VECTOR ( 'NONE', #27574, 1000.000000000000000 ) ;
#26329 = CARTESIAN_POINT ( 'NONE',  ( -10.45204383622999877, -22.76256649475000060, 7.651147548059999970 ) ) ;
#26330 = CARTESIAN_POINT ( 'NONE',  ( -5.095949825044894688, -78.17859843627216776, -7.719699935279118463 ) ) ;
#26331 = CARTESIAN_POINT ( 'NONE',  ( 10.58946819037999987, -78.42157559663600352, -3.698823201301000285 ) ) ;
#26332 = EDGE_LOOP ( 'NONE', ( #40200, #8037, #57833, #47208 ) ) ;
#26333 = ORIENTED_EDGE ( 'NONE', *, *, #27126, .F. ) ;
#26334 = CARTESIAN_POINT ( 'NONE',  ( -4.209169930338003240, -77.51272233025383684, 8.236736021501149807 ) ) ;
#26335 = CARTESIAN_POINT ( 'NONE',  ( 10.42639159904000046, -77.03997040616140168, -2.617796444239999687 ) ) ;
#26336 = CARTESIAN_POINT ( 'NONE',  ( -0.5548610165507998904, -78.01090185290100010, -9.688283574444998436 ) ) ;
#26337 = CARTESIAN_POINT ( 'NONE',  ( -2.468957475121000389, -76.22189569223999683, 12.56811386993000035 ) ) ;
#26338 = CARTESIAN_POINT ( 'NONE',  ( 3.250000000000001332, -2.240126334641624695, -0.4032474491995221011 ) ) ;
#26339 = DIRECTION ( 'NONE',  ( -0.9957542233908834861, -0.04890176544943922177, 0.07798810124080873818 ) ) ;
#26340 = CARTESIAN_POINT ( 'NONE',  ( 3.942135768300999654, -80.14393115911698828, -10.54187931140000067 ) ) ;
#26341 = DIRECTION ( 'NONE',  ( 1.000000000000000000, 0.000000000000000000, 0.000000000000000000 ) ) ;
#26342 = EDGE_CURVE ( 'NONE', #54085, #40725, #4333, .T. ) ;
#26343 = DIRECTION ( 'NONE',  ( -0.9999476293090542312, 0.000000000000000000, -0.01023418971888952027 ) ) ;
#26344 = CARTESIAN_POINT ( 'NONE',  ( -7.594691572176750505, -79.24835172787872750, 5.837024335811811682 ) ) ;
#26345 = ORIENTED_EDGE ( 'NONE', *, *, #1866, .F. ) ;
#26346 = ADVANCED_FACE ( 'NONE', ( #35937 ), #2584, .F. ) ;
#26347 = CARTESIAN_POINT ( 'NONE',  ( -0.4643318395057000059, -79.19853201380200858, -12.07492461931999905 ) ) ;
#26348 = CARTESIAN_POINT ( 'NONE',  ( -8.284626357322000700, -53.75139346809000074, 9.778502130833000905 ) ) ;
#26349 = CARTESIAN_POINT ( 'NONE',  ( 12.76303204291999904, -55.53514849259999409, 1.980584515756000030 ) ) ;
#26350 = CARTESIAN_POINT ( 'NONE',  ( -9.778561352719998823, -16.95143577368999743, -8.284566532398999428 ) ) ;
#26352 = DIRECTION ( 'NONE',  ( 1.000000000000000000, 0.000000000000000000, 0.000000000000000000 ) ) ;
#26351 = DIRECTION ( 'NONE',  ( 0.6489586447440038874, 0.04890182322783028640, -0.7592504784964048126 ) ) ;
#26353 = CYLINDRICAL_SURFACE ( 'NONE', #37377, 3.250000000000000000 ) ;
#26354 = CARTESIAN_POINT ( 'NONE',  ( 0.7366363428794999724, -80.42674279837198981, 11.26767966793000042 ) ) ;
#26355 = DIRECTION ( 'NONE',  ( 0.000000000000000000, 0.000000000000000000, -1.000000000000000000 ) ) ;
#26356 = CARTESIAN_POINT ( 'NONE',  ( 6.355487164442999770, -78.15069330475100173, 9.297405415548999130 ) ) ;
#26357 = CARTESIAN_POINT ( 'NONE',  ( -2.839805762151343949, -1.958333333333333259, 1.636761686205411737 ) ) ;
#26358 = CARTESIAN_POINT ( 'NONE',  ( 9.871112813097001393, -80.53352039424419218, -5.408775127089999302 ) ) ;
#26359 = CARTESIAN_POINT ( 'NONE',  ( -8.768124086712999699, -55.64999999965999677, -7.919595949288999570 ) ) ;
#26360 = DIRECTION ( 'NONE',  ( 1.000000000000000000, 0.000000000000000000, 0.000000000000000000 ) ) ;
#26361 = CARTESIAN_POINT ( 'NONE',  ( -12.53241208773999915, -22.76462890193000277, 1.667936697358999965 ) ) ;
#26362 = EDGE_CURVE ( 'NONE', #54466, #15959, #45945, .T. ) ;
#26363 = CARTESIAN_POINT ( 'NONE',  ( 0.2795141487000000202, -3.262566639609999708, -3.635069219502999882 ) ) ;
#26364 = CARTESIAN_POINT ( 'NONE',  ( 6.329984427697000093, -78.02560107145599488, 9.260097609460000712 ) ) ;
#26365 = CIRCLE ( 'NONE', #41472, 30.49999999999998934 ) ;
#26366 = CARTESIAN_POINT ( 'NONE',  ( -0.8506806241676574398, -1.604166666666666519, -3.165411199172027068 ) ) ;
#26367 = CARTESIAN_POINT ( 'NONE',  ( 0.000000000000000000, -2.949999999935999817, 0.000000000000000000 ) ) ;
#26368 = CARTESIAN_POINT ( 'NONE',  ( -2.061649843245999758, -60.00561307554999502, 12.83797346717000210 ) ) ;
#26369 = CARTESIAN_POINT ( 'NONE',  ( 12.48375942317000131, -18.62730665102000316, 1.669542353227000175 ) ) ;
#26370 = VECTOR ( 'NONE', #37444, 1000.000000000000000 ) ;
#26371 = CARTESIAN_POINT ( 'NONE',  ( -3.328640256345000381, -85.03957450217399128, -2.445129353070000011 ) ) ;
#26372 = DIRECTION ( 'NONE',  ( 0.000000000000000000, 1.000000000000000000, 0.000000000000000000 ) ) ;
#26373 = DIRECTION ( 'NONE',  ( -0.7071067811865475727, 0.000000000000000000, -0.7071067811865475727 ) ) ;
#26374 = CARTESIAN_POINT ( 'NONE',  ( 3.871217329169000188, -77.05563908551199859, 10.45314674924000009 ) ) ;
#26375 = CARTESIAN_POINT ( 'NONE',  ( 0.6088572233645838105, -81.93455332008454661, 1.091931018960549560 ) ) ;
#26376 = CARTESIAN_POINT ( 'NONE',  ( -0.5800742227073999446, -79.54852142615000332, -1.311952909603000039 ) ) ;
#26377 = CARTESIAN_POINT ( 'NONE',  ( 9.670530767802999250, -77.13907693894029194, -0.1674091926992999912 ) ) ;
#26378 = CARTESIAN_POINT ( 'NONE',  ( -1.430508845346486702, -82.72367320741450669, 0.4901804664080808838 ) ) ;
#26379 = CARTESIAN_POINT ( 'NONE',  ( -12.54673349189000042, -61.62806887777999520, 0.9076721992840999231 ) ) ;
#26380 = CARTESIAN_POINT ( 'NONE',  ( -5.959306489951042174, -80.17831636609369639, -8.946966000018207410 ) ) ;
#26381 = CARTESIAN_POINT ( 'NONE',  ( -12.50680023853919565, -24.30414033429957499, -1.424451025645344426 ) ) ;
#26382 = CARTESIAN_POINT ( 'NONE',  ( 9.339517261602930276, -75.80000000000001137, 7.561296970547564555 ) ) ;
#26383 = ORIENTED_EDGE ( 'NONE', *, *, #171, .T. ) ;
#26384 = CARTESIAN_POINT ( 'NONE',  ( -1.178447680628000205, -80.95308451575900222, -0.9280415206345000723 ) ) ;
#26385 = CARTESIAN_POINT ( 'NONE',  ( -0.2494208061606092153, -61.79288960742086800, 12.50614183116564604 ) ) ;
#26386 = CARTESIAN_POINT ( 'NONE',  ( -10.75919966670999983, -79.79953960801499591, 3.327699969971999572 ) ) ;
#26387 = DIRECTION ( 'NONE',  ( -1.000000000000000000, 0.000000000000000000, 0.000000000000000000 ) ) ;
#26388 = ORIENTED_EDGE ( 'NONE', *, *, #56057, .F. ) ;
#26389 = ORIENTED_EDGE ( 'NONE', *, *, #12414, .F. ) ;
#26390 = CARTESIAN_POINT ( 'NONE',  ( -0.2806432552994999607, -82.10210008720301289, -1.487181012905000044 ) ) ;
#26391 = ORIENTED_EDGE ( 'NONE', *, *, #21785, .F. ) ;
#26392 = CARTESIAN_POINT ( 'NONE',  ( -2.099388381696000023E-14, -0.04999999937965000224, 0.000000000000000000 ) ) ;
#26394 = EDGE_CURVE ( 'NONE', #46546, #55386, #19118, .T. ) ;
#26393 = ORIENTED_EDGE ( 'NONE', *, *, #31524, .F. ) ;
#26395 = CARTESIAN_POINT ( 'NONE',  ( 0.000000000000000000, -79.65000000003199432, -9.349999999968000353 ) ) ;
#26396 = CARTESIAN_POINT ( 'NONE',  ( 1.199500263597268246, -78.30208333333331439, 0.9218200799623752495 ) ) ;
#26397 = CARTESIAN_POINT ( 'NONE',  ( -1.733234625524999961, -79.68572132302399780, -10.77827740047999860 ) ) ;
#26398 = CARTESIAN_POINT ( 'NONE',  ( 1.632307027708999936, -23.66927189556999878, -12.46200249212000166 ) ) ;
#26399 = CARTESIAN_POINT ( 'NONE',  ( 2.236424164684999827, -79.53195424565778637, -3.018240402847999881 ) ) ;
#26400 = CARTESIAN_POINT ( 'NONE',  ( -5.582146761189269668, -79.32488193069980298, 7.686897053185122175 ) ) ;
#26401 = VERTEX_POINT ( 'NONE', #22958 ) ;
#26402 = CARTESIAN_POINT ( 'NONE',  ( -9.546819346421999697, -24.68527546640000025, 8.130850183241999929 ) ) ;
#26403 = CARTESIAN_POINT ( 'NONE',  ( -5.574502783093999270, -79.09338212571999804, -11.02980955859000112 ) ) ;
#26404 = VERTEX_POINT ( 'NONE', #40969 ) ;
#26405 = CARTESIAN_POINT ( 'NONE',  ( 12.80088938717999980, -56.03743348177000172, -1.980532758767000301 ) ) ;
#26406 = DIRECTION ( 'NONE',  ( 0.000000000000000000, -1.000000000000000000, 0.000000000000000000 ) ) ;
#26407 = CARTESIAN_POINT ( 'NONE',  ( -0.8465867926663999121, -80.78896482857800265, -0.9556525628790000226 ) ) ;
#26408 = CIRCLE ( 'NONE', #31117, 14.00000000000000000 ) ;
#26409 = CARTESIAN_POINT ( 'NONE',  ( 0.8618009059429999619, -78.34162200021098954, -9.665816497589000633 ) ) ;
#26410 = AXIS2_PLACEMENT_3D ( 'NONE', #22553, #28128, #13685 ) ;
#26411 = CARTESIAN_POINT ( 'NONE',  ( -3.589185692315953524, -86.25171438276197478, 1.679770172568654685 ) ) ;
#26412 = FACE_BOUND ( 'NONE', #20788, .T. ) ;
#26413 = CARTESIAN_POINT ( 'NONE',  ( 12.60698020661999941, -78.23342962590999150, -3.609717992041000301 ) ) ;
#26414 = CARTESIAN_POINT ( 'NONE',  ( 5.552077009241000560, -78.08319635864999952, 11.35743496097000005 ) ) ;
#26415 = CARTESIAN_POINT ( 'NONE',  ( -2.000000000000000000, -76.29999999999999716, 0.000000000000000000 ) ) ;
#26416 = CARTESIAN_POINT ( 'NONE',  ( -9.179332505514366858, -78.61010642507874024, -1.157977033747941809 ) ) ;
#26417 = EDGE_CURVE ( 'NONE', #9574, #13712, #51478, .T. ) ;
#26418 = CARTESIAN_POINT ( 'NONE',  ( -2.914327657214999867, -81.70032136754298335, 2.926637648191000363 ) ) ;
#26419 = CARTESIAN_POINT ( 'NONE',  ( -10.07719973192999952, -58.54888345776999614, 7.718346056099999686 ) ) ;
#26420 = CARTESIAN_POINT ( 'NONE',  ( 1.173288415578912947, -2.946837913471963333, 3.030131958616116172 ) ) ;
#26421 = CARTESIAN_POINT ( 'NONE',  ( 2.784408088275000193, -80.80305496681198463, -2.197415289112000014 ) ) ;
#26422 = CARTESIAN_POINT ( 'NONE',  ( 3.399186938124000079, -81.00000000000000000, -10.46162167925000119 ) ) ;
#26423 = DIRECTION ( 'NONE',  ( 0.000000000000000000, 0.000000000000000000, -1.000000000000000000 ) ) ;
#26424 = CARTESIAN_POINT ( 'NONE',  ( 2.234646451474000095, -2.573064556719999896, 3.080979982494000069 ) ) ;
#26425 = CARTESIAN_POINT ( 'NONE',  ( -0.6380817373966316541, -79.83329071193379889, -1.104274488347721794 ) ) ;
#26426 = ORIENTED_EDGE ( 'NONE', *, *, #23368, .F. ) ;
#26427 = CARTESIAN_POINT ( 'NONE',  ( 0.000000000000000000, -83.49999999999998579, 0.000000000000000000 ) ) ;
#26428 = CARTESIAN_POINT ( 'NONE',  ( -6.760013919724056741, -79.27291666666666003, -8.796335266379987416 ) ) ;
#26429 = EDGE_CURVE ( 'NONE', #19092, #515, #52924, .T. ) ;
#26430 = CARTESIAN_POINT ( 'NONE',  ( 0.1510373474112000070, -81.58785527686900707, 1.325052402434999888 ) ) ;
#26432 = EDGE_CURVE ( 'NONE', #52835, #11445, #19409, .T. ) ;
#26431 = CARTESIAN_POINT ( 'NONE',  ( 0.1977897354609805813, -79.02666666666665662, -9.531227019568570213 ) ) ;
#26433 = CARTESIAN_POINT ( 'NONE',  ( 7.349802007153999561, -77.65542860837000205, -10.73869877321999944 ) ) ;
#26434 = CARTESIAN_POINT ( 'NONE',  ( -7.635227771907816319, -60.56609606928231671, -10.36745004612171783 ) ) ;
#26435 = CARTESIAN_POINT ( 'NONE',  ( 6.173289772713999923, -76.32831948348000140, 10.88346660266000221 ) ) ;
#26436 = ORIENTED_EDGE ( 'NONE', *, *, #12281, .T. ) ;
#26437 = FACE_OUTER_BOUND ( 'NONE', #35310, .T. ) ;
#26438 = CARTESIAN_POINT ( 'NONE',  ( -1.335058897431999902, -82.31057754807500260, -0.2280211375632000270 ) ) ;
#26439 = CARTESIAN_POINT ( 'NONE',  ( -1.667961445601999992, -21.74800977511999989, -12.58338334669999981 ) ) ;
#26440 = AXIS2_PLACEMENT_3D ( 'NONE', #18047, #54356, #49638 ) ;
#26441 = CARTESIAN_POINT ( 'NONE',  ( -9.504204889957000191, -77.45206109394898419, 0.5832244475350000235 ) ) ;
#26442 = CARTESIAN_POINT ( 'NONE',  ( -1.752505721091000002, -84.99032934161199648, -3.786195844160000323 ) ) ;
#26443 = CARTESIAN_POINT ( 'NONE',  ( -1.931086388578000079, -55.50221245779999890, -12.71798269383000068 ) ) ;
#26444 = CARTESIAN_POINT ( 'NONE',  ( 1.396889377938999921, -80.33901284111300356, -0.2424037069397000088 ) ) ;
#26445 = EDGE_LOOP ( 'NONE', ( #38027, #41150, #37663, #21718, #26914 ) ) ;
#26446 = CARTESIAN_POINT ( 'NONE',  ( -4.671140612849559837, -77.18924933319441095, -9.682078454169923631 ) ) ;
#26447 = CARTESIAN_POINT ( 'NONE',  ( -9.250265637099717608, -79.09517564970080628, 0.6034143313266543407 ) ) ;
#26448 = EDGE_CURVE ( 'NONE', #2323, #10831, #17646, .T. ) ;
#26449 = CARTESIAN_POINT ( 'NONE',  ( 3.437187628289000152, -78.85171435493609238, -4.209340827053006789E-16 ) ) ;
#26450 = VERTEX_POINT ( 'NONE', #37399 ) ;
#26451 = ORIENTED_EDGE ( 'NONE', *, *, #16660, .T. ) ;
#26452 = CARTESIAN_POINT ( 'NONE',  ( 6.657089793739999983, -79.63047948297999312, 8.818222636911000833 ) ) ;
#26453 = CARTESIAN_POINT ( 'NONE',  ( 12.49168451095999899, -55.50151115525000023, 1.667916687331000070 ) ) ;
#26454 = CARTESIAN_POINT ( 'NONE',  ( -11.30204317227000033, -80.23062822292799012, 1.780446720864000021 ) ) ;
#26455 = VERTEX_POINT ( 'NONE', #55418 ) ;
#26456 = CARTESIAN_POINT ( 'NONE',  ( 6.482586803565999922, -77.86134018205299867, -10.15735398655000132 ) ) ;
#26457 = ORIENTED_EDGE ( 'NONE', *, *, #24298, .F. ) ;
#26459 = EDGE_CURVE ( 'NONE', #46260, #30832, #25978, .T. ) ;
#26458 = ORIENTED_EDGE ( 'NONE', *, *, #37078, .T. ) ;
#26460 = EDGE_CURVE ( 'NONE', #39760, #16765, #24807, .T. ) ;
#26461 = CARTESIAN_POINT ( 'NONE',  ( -12.00000000000000355, -78.78958333333331154, 1.570796326794848596 ) ) ;
#26462 = CARTESIAN_POINT ( 'NONE',  ( 10.07627163191000008, -55.55000000278000272, 7.601397897754999633 ) ) ;
#26463 = ORIENTED_EDGE ( 'NONE', *, *, #44940, .T. ) ;
#26464 = CARTESIAN_POINT ( 'NONE',  ( 1.199237972082057846, -81.70227769186961098, 0.9216820448048951286 ) ) ;
#26465 = CIRCLE ( 'NONE', #56670, 13.89999999999999858 ) ;
#26466 = EDGE_LOOP ( 'NONE', ( #39410, #27353, #40357 ) ) ;
#26467 = FACE_OUTER_BOUND ( 'NONE', #46780, .T. ) ;
#26468 = CARTESIAN_POINT ( 'NONE',  ( -3.436577009133267691, -78.85171435493609238, 0.06478620501008579280 ) ) ;
#26469 = CYLINDRICAL_SURFACE ( 'NONE', #44369, 1.750000000000000000 ) ;
#26470 = CARTESIAN_POINT ( 'NONE',  ( 0.4820079653519915852, -18.48385402702554359, 10.98957811953277641 ) ) ;
#26471 = CARTESIAN_POINT ( 'NONE',  ( 11.67645908292204382, -77.43648248267068368, -1.539101508411103492 ) ) ;
#26472 = CARTESIAN_POINT ( 'NONE',  ( 13.98934701867000108, -46.22186981632000169, 1.420930503148999987E-05 ) ) ;
#26473 = CARTESIAN_POINT ( 'NONE',  ( 7.612971540294999784, -60.12452273675999947, -10.53003236235000095 ) ) ;
#26474 = DIRECTION ( 'NONE',  ( 0.000000000000000000, -1.000000000000000000, 0.000000000000000000 ) ) ;
#26475 = CARTESIAN_POINT ( 'NONE',  ( -10.01752098897000032, -23.19172009652000099, 7.660412494176999765 ) ) ;
#26476 = CARTESIAN_POINT ( 'NONE',  ( 0.3926218265389221362, -80.04583333333334849, -1.460959015002473160 ) ) ;
#26477 = CIRCLE ( 'NONE', #1082, 0.5000000000000000000 ) ;
#26478 = CARTESIAN_POINT ( 'NONE',  ( -2.944243145599999778, -81.52455496681199065, 2.956601854374000027 ) ) ;
#26479 = CONICAL_SURFACE ( 'NONE', #1091, 5.599999999950999729, 0.2449786631268792425 ) ;
#26480 = CARTESIAN_POINT ( 'NONE',  ( 8.780483330769000005, -76.97088667140099005, -4.267527838117000094 ) ) ;
#26481 = CARTESIAN_POINT ( 'NONE',  ( 0.6295237254636211199, -83.33333333333332860, 1.092232985442824322 ) ) ;
#26482 = CARTESIAN_POINT ( 'NONE',  ( 10.42531124905999995, -18.73514851523999880, -7.624341765453999997 ) ) ;
#26483 = CARTESIAN_POINT ( 'NONE',  ( -1.667269374596999976, -23.20939883484999910, 12.49858097730999873 ) ) ;
#26484 = CARTESIAN_POINT ( 'NONE',  ( 9.469145113845355510, -79.89323344442750852, 5.723973398464533346 ) ) ;
#26485 = FACE_OUTER_BOUND ( 'NONE', #54010, .T. ) ;
#26486 = CARTESIAN_POINT ( 'NONE',  ( 2.821058886968999868, -1.193281426753999952, 2.773385340853000258 ) ) ;
#26487 = CARTESIAN_POINT ( 'NONE',  ( 7.624341766629000539, -55.53514853726999689, -10.42531125022999916 ) ) ;
#26488 = CARTESIAN_POINT ( 'NONE',  ( 0.5215562184170206006, -80.69749268949153986, 1.459483306257267854 ) ) ;
#26489 = CARTESIAN_POINT ( 'NONE',  ( 12.48375848566000101, -60.17270426026000507, -1.669543623995999981 ) ) ;
#26490 = LINE ( 'NONE', #22068, #31578 ) ;
#26491 = CARTESIAN_POINT ( 'NONE',  ( -12.99510751537000353, -15.69705297113999443, -6.911973076623003642 ) ) ;
#26492 = EDGE_CURVE ( 'NONE', #41938, #14498, #56494, .T. ) ;
#26493 = CARTESIAN_POINT ( 'NONE',  ( -8.494907789873000326, -76.97389978589799853, 6.628721719457000283 ) ) ;
#26494 = CARTESIAN_POINT ( 'NONE',  ( -11.33781659400000130, -77.84203558730200712, 4.716958136547999558 ) ) ;
#26495 = CARTESIAN_POINT ( 'NONE',  ( -12.57042253521000141, -26.10094976978000147, 0.000000000000000000 ) ) ;
#26497 = CARTESIAN_POINT ( 'NONE',  ( 1.013266355313000133, -78.16944336237389734, 1.127933319133000101 ) ) ;
#26496 = DIRECTION ( 'NONE',  ( -1.000000000000000000, 0.000000000000000000, 0.000000000000000000 ) ) ;
#26498 = CARTESIAN_POINT ( 'NONE',  ( -1.542276019614999827, -82.23513558557998238, 0.7219429580085000575 ) ) ;
#26499 = VERTEX_POINT ( 'NONE', #12005 ) ;
#26500 = CARTESIAN_POINT ( 'NONE',  ( -10.38645071870000081, -19.22180874373999870, -7.655542440091000600 ) ) ;
#26501 = CARTESIAN_POINT ( 'NONE',  ( 7.482400665469000067, -80.95774006270789869, 8.296818276455001140 ) ) ;
#26502 = DIRECTION ( 'NONE',  ( -1.000000000000000000, 0.000000000000000000, 0.000000000000000000 ) ) ;
#26503 = CARTESIAN_POINT ( 'NONE',  ( -0.03499679800989389383, -84.32708334457048238, 3.443595259721679902 ) ) ;
#26504 = CARTESIAN_POINT ( 'NONE',  ( 8.343860018000999190, -60.54999999966955926, 8.343860018000999190 ) ) ;
#26505 = CARTESIAN_POINT ( 'NONE',  ( -1.267719250440999978, -1.620138932810000210, 3.650372561581000319 ) ) ;
#26506 = CARTESIAN_POINT ( 'NONE',  ( 8.682512087609998375, -79.49501085431899128, 4.502999560499000076 ) ) ;
#26507 = LINE ( 'NONE', #44836, #17317 ) ;
#26508 = CARTESIAN_POINT ( 'NONE',  ( -9.722718241315000398, -23.25000000000000000, 7.954951288349001004 ) ) ;
#26509 = VERTEX_POINT ( 'NONE', #47171 ) ;
#26510 = CARTESIAN_POINT ( 'NONE',  ( 0.000000000000000000, -23.15000000000000213, -12.00000000000000000 ) ) ;
#26511 = CARTESIAN_POINT ( 'NONE',  ( 9.431008681916170033, -24.80059307779984579, -8.251849286024803831 ) ) ;
#26512 = EDGE_CURVE ( 'NONE', #6742, #34745, #13493, .T. ) ;
#26513 = CARTESIAN_POINT ( 'NONE',  ( 0.000000000000000000, -18.75000000000000000, 12.50000000000000000 ) ) ;
#26514 = CARTESIAN_POINT ( 'NONE',  ( 3.851650068366999857, -78.43735716284258785, 0.000000000000000000 ) ) ;
#26515 = ADVANCED_FACE ( 'NONE', ( #56585 ), #1296, .F. ) ;
#26516 = CARTESIAN_POINT ( 'NONE',  ( -0.4240539849974000464, -80.28430614307998781, 1.611036072322000079 ) ) ;
#26517 = VERTEX_POINT ( 'NONE', #21140 ) ;
#26518 = DIRECTION ( 'NONE',  ( -1.000000000000000000, 0.000000000000000000, 0.000000000000000000 ) ) ;
#26519 = VECTOR ( 'NONE', #26770, 1000.000000000000114 ) ;
#26520 = CARTESIAN_POINT ( 'NONE',  ( 8.441176280282578048, -61.71652561705573703, -9.243148036168024717 ) ) ;
#26521 = CARTESIAN_POINT ( 'NONE',  ( 0.4254240051736215000, -1.135416666666666963, -3.250000000000000000 ) ) ;
#26522 = ORIENTED_EDGE ( 'NONE', *, *, #29814, .T. ) ;
#26523 = VERTEX_POINT ( 'NONE', #34704 ) ;
#26524 = CARTESIAN_POINT ( 'NONE',  ( -12.92181194095999963, -58.55648180022999583, 2.062502994258999856 ) ) ;
#26525 = CARTESIAN_POINT ( 'NONE',  ( -7.760941378042000238, -54.56914109158999793, -10.15321372494000052 ) ) ;
#26526 = EDGE_CURVE ( 'NONE', #23631, #15888, #52735, .T. ) ;
#26527 = CARTESIAN_POINT ( 'NONE',  ( 9.523132023602000729, -80.08931041772898141, 1.108936319727999997 ) ) ;
#26528 = VERTEX_POINT ( 'NONE', #2856 ) ;
#26529 = EDGE_LOOP ( 'NONE', ( #18008, #45522, #1433 ) ) ;
#26530 = CARTESIAN_POINT ( 'NONE',  ( 12.02981475616999951, -76.85882676113499201, -2.229486315987000200 ) ) ;
#26531 = DIRECTION ( 'NONE',  ( 0.000000000000000000, 0.000000000000000000, 1.000000000000000000 ) ) ;
#26532 = CARTESIAN_POINT ( 'NONE',  ( -1.481892012897999988, -78.73390927755998803, 0.7217217885958999712 ) ) ;
#26533 = ORIENTED_EDGE ( 'NONE', *, *, #22959, .F. ) ;
#26534 = FACE_OUTER_BOUND ( 'NONE', #51677, .T. ) ;
#26535 = CARTESIAN_POINT ( 'NONE',  ( -1.456099130830773136, -79.27085162341434454, -0.3904854336919924562 ) ) ;
#26536 = CARTESIAN_POINT ( 'NONE',  ( -0.1112851791610966062, -80.21855645632498977, -1.247194601161994543 ) ) ;
#26537 = CARTESIAN_POINT ( 'NONE',  ( 12.60698020661999941, -78.22218707672999471, -3.609717992041000301 ) ) ;
#26538 = CARTESIAN_POINT ( 'NONE',  ( -6.984027423103999155, -77.17848496647944501, 8.777327129872999123 ) ) ;
#26539 = CARTESIAN_POINT ( 'NONE',  ( 12.00000000000000000, -18.75000000000000000, 0.000000000000000000 ) ) ;
#26540 = CARTESIAN_POINT ( 'NONE',  ( -0.5608696358174141139, -86.31452044230000809, 4.510645591149716971 ) ) ;
#26541 = CARTESIAN_POINT ( 'NONE',  ( 10.93160348586000019, -79.16966811650100055, 2.513594203403000105 ) ) ;
#26542 = ADVANCED_FACE ( 'NONE', ( #11432 ), #6702, .F. ) ;
#26543 = CARTESIAN_POINT ( 'NONE',  ( -0.8350858585606752982, -79.98228243800841142, 9.212292648074781098 ) ) ;
#26544 = CARTESIAN_POINT ( 'NONE',  ( 10.20679554289463731, -17.76427274283123481, 7.770327721672145138 ) ) ;
#26545 = ORIENTED_EDGE ( 'NONE', *, *, #15903, .F. ) ;
#26546 = CARTESIAN_POINT ( 'NONE',  ( -1.331888048429999971, -78.73638398745899281, -11.18726993471000064 ) ) ;
#26547 = CARTESIAN_POINT ( 'NONE',  ( -9.662446363796000526, -76.49882503999000960, 7.627099640079999965 ) ) ;
#26548 = CARTESIAN_POINT ( 'NONE',  ( 1.377412799619999850, -79.70174468460000128, 0.8425838727997000399 ) ) ;
#26549 = CARTESIAN_POINT ( 'NONE',  ( -2.818391366050096991, -2.902451986714001286, -2.210571898668216129 ) ) ;
#26550 = CARTESIAN_POINT ( 'NONE',  ( -7.792421629684946005, -17.70899070367055472, 10.18245656324600290 ) ) ;
#26551 = CARTESIAN_POINT ( 'NONE',  ( 4.297951556683999641, -76.85513471105899441, -11.50435740523999861 ) ) ;
#26552 = CARTESIAN_POINT ( 'NONE',  ( -9.599999999916001059, -90.40000000008399184, 6.531558194539000517E-10 ) ) ;
#26553 = CARTESIAN_POINT ( 'NONE',  ( 9.458764864882999390, -79.26244768766198945, -5.918054316060000097 ) ) ;
#26554 = CARTESIAN_POINT ( 'NONE',  ( -8.488083377859000578, -76.90398832859899869, 4.545599397691000298 ) ) ;
#26555 = DIRECTION ( 'NONE',  ( 0.000000000000000000, 0.000000000000000000, 1.000000000000000000 ) ) ;
#26556 = CARTESIAN_POINT ( 'NONE',  ( 9.393203674808285442, -79.70833333333332860, -5.413904038987152667 ) ) ;
#26557 = CARTESIAN_POINT ( 'NONE',  ( 7.358951392786451606, -80.06693380409777205, 8.232011333706584111 ) ) ;
#26558 = VERTEX_POINT ( 'NONE', #42722 ) ;
#26559 = CARTESIAN_POINT ( 'NONE',  ( 0.7304821784857000733, -81.79022674571000096, 1.273910602969000161 ) ) ;
#26560 = DIRECTION ( 'NONE',  ( 0.000000000000000000, -1.000000000000000000, 0.000000000000000000 ) ) ;
#26561 = CARTESIAN_POINT ( 'NONE',  ( 7.710118476714000302, -58.54977139529999164, -10.18499221086999995 ) ) ;
#26562 = AXIS2_PLACEMENT_3D ( 'NONE', #15177, #6026, #55626 ) ;
#26563 = CARTESIAN_POINT ( 'NONE',  ( 11.81379047889000056, -77.26158115298899531, 1.987564636421000008 ) ) ;
#26564 = CARTESIAN_POINT ( 'NONE',  ( 6.218034014419081323, -77.00000000000001421, 6.922517326502717339 ) ) ;
#26565 = CARTESIAN_POINT ( 'NONE',  ( -1.508789225394999933, -82.17633606662001000, 0.7062677124845000431 ) ) ;
#26566 = CARTESIAN_POINT ( 'NONE',  ( 5.516244905679999810, -78.91335487410098892, 10.58329673088999989 ) ) ;
#26567 = CARTESIAN_POINT ( 'NONE',  ( -7.603664017118000551, -78.45629415034599674, 6.060370778711000384 ) ) ;
#26568 = CARTESIAN_POINT ( 'NONE',  ( -9.088317367618000020, -78.68010020865598619, 3.186800494491000002 ) ) ;
#26569 = CARTESIAN_POINT ( 'NONE',  ( -1.930638663168000146, -55.57877936677999742, -12.72375916870000090 ) ) ;
#26570 = CARTESIAN_POINT ( 'NONE',  ( 11.54042753142849520, -75.96480956287521735, 2.208758157258925436 ) ) ;
#26571 = CARTESIAN_POINT ( 'NONE',  ( 1.589609816837670220, -86.02148118236289065, 3.662844055364274265 ) ) ;
#26572 = ORIENTED_EDGE ( 'NONE', *, *, #26789, .F. ) ;
#26573 = CARTESIAN_POINT ( 'NONE',  ( 0.000000000000000000, -76.39999999999999147, -10.70000000000050910 ) ) ;
#26574 = CARTESIAN_POINT ( 'NONE',  ( -8.960630775719000241, -79.88644599990469430, -8.384004251637000138 ) ) ;
#26575 = CARTESIAN_POINT ( 'NONE',  ( 2.024107680232116291, -78.48547957940618858, -3.504731529255688649 ) ) ;
#26576 = CARTESIAN_POINT ( 'NONE',  ( -1.596536837631000072, -81.79343788471999233, -0.4757406268331999533 ) ) ;
#26577 = CARTESIAN_POINT ( 'NONE',  ( -10.05535668103000191, -78.29735989301799748, 4.970705447719999448 ) ) ;
#26578 = CARTESIAN_POINT ( 'NONE',  ( 6.718030245586000149, -79.10756892577299482, -8.679405866825000260 ) ) ;
#26579 = CARTESIAN_POINT ( 'NONE',  ( -1.308715794677037136, -17.25595500803412463, 12.70256747357091598 ) ) ;
#26580 = CARTESIAN_POINT ( 'NONE',  ( -12.36215275698000049, -76.44617465741299611, -0.7837170484252999891 ) ) ;
#26581 = CARTESIAN_POINT ( 'NONE',  ( 3.137847802567000688, -78.55121997915446741, 11.32185723005353495 ) ) ;
#26582 = CARTESIAN_POINT ( 'NONE',  ( -9.250000000000000000, -77.49999999999998579, -1.203901273580999948E-14 ) ) ;
#26583 = VERTEX_POINT ( 'NONE', #2288 ) ;
#26584 = CARTESIAN_POINT ( 'NONE',  ( -2.801579282652000291, -78.74570369637000056, -10.67018687299000135 ) ) ;
#26585 = CARTESIAN_POINT ( 'NONE',  ( 0.8052405978830968758, -79.91960879271107387, 0.9563048914733230932 ) ) ;
#26586 = CARTESIAN_POINT ( 'NONE',  ( 0.000000000000000000, -80.49999999999998579, 0.000000000000000000 ) ) ;
#26587 = CARTESIAN_POINT ( 'NONE',  ( -4.043784919594221705, -78.69999999999998863, 2.284880126142637913 ) ) ;
#26588 = EDGE_CURVE ( 'NONE', #46129, #18440, #56298, .T. ) ;
#26589 = CARTESIAN_POINT ( 'NONE',  ( -9.975891578018998729, -78.78001782088199434, -4.997317968730000004 ) ) ;
#26590 = CARTESIAN_POINT ( 'NONE',  ( -1.750000000000000000, -55.55000000278000272, -12.50000000000000000 ) ) ;
#26591 = CARTESIAN_POINT ( 'NONE',  ( -10.98965142020557373, -23.51557447649329191, 0.4775239249278388498 ) ) ;
#26592 = CARTESIAN_POINT ( 'NONE',  ( 2.765208115035000080, -77.96966499545499119, -11.96450597650000169 ) ) ;
#26593 = ORIENTED_EDGE ( 'NONE', *, *, #40509, .T. ) ;
#26594 = CARTESIAN_POINT ( 'NONE',  ( -12.76303204294999993, -23.26485150694999859, 1.980584515756000030 ) ) ;
#26595 = CARTESIAN_POINT ( 'NONE',  ( -12.70451647739338696, -61.35458569071866464, -1.498866844003992060 ) ) ;
#26596 = EDGE_CURVE ( 'NONE', #22868, #51104, #9958, .T. ) ;
#26597 = DIRECTION ( 'NONE',  ( -0.7071067811865475727, 0.000000000000000000, -0.7071067811865475727 ) ) ;
#26598 = VERTEX_POINT ( 'NONE', #26146 ) ;
#26599 = ORIENTED_EDGE ( 'NONE', *, *, #17890, .T. ) ;
#26600 = CARTESIAN_POINT ( 'NONE',  ( 1.001315002179000047, -24.68522411714000242, -12.50000000000000000 ) ) ;
#26601 = ORIENTED_EDGE ( 'NONE', *, *, #11831, .T. ) ;
#26602 = CARTESIAN_POINT ( 'NONE',  ( -5.950798862880000151, -78.96731654267000522, 10.72320280238000123 ) ) ;
#26603 = EDGE_LOOP ( 'NONE', ( #27928, #46600, #54299, #38756 ) ) ;
#26604 = CARTESIAN_POINT ( 'NONE',  ( 10.30458248778999852, -23.76332651811999952, 7.636263891322999875 ) ) ;
#26605 = CARTESIAN_POINT ( 'NONE',  ( -10.41264997627000000, -77.61434791013999757, 3.643961423121000021 ) ) ;
#26606 = EDGE_CURVE ( 'NONE', #55023, #43973, #28972, .T. ) ;
#26607 = CARTESIAN_POINT ( 'NONE',  ( -1.249727466589207525, -82.59024373000691810, 0.1639556666535628981 ) ) ;
#26608 = CARTESIAN_POINT ( 'NONE',  ( -4.760515938158666138, -78.18205582176251767, -7.931580567799660031 ) ) ;
#26609 = VECTOR ( 'NONE', #40987, 1000.000000000000000 ) ;
#26610 = CARTESIAN_POINT ( 'NONE',  ( -11.20683111097000051, -79.76947227099799420, -0.4743912329535999728 ) ) ;
#26611 = CARTESIAN_POINT ( 'NONE',  ( 1.250002295818805509, -79.35918108845754659, 0.1442765043559274540 ) ) ;
#26612 = EDGE_CURVE ( 'NONE', #31953, #18786, #19342, .T. ) ;
#26613 = ORIENTED_EDGE ( 'NONE', *, *, #41744, .T. ) ;
#26614 = ORIENTED_EDGE ( 'NONE', *, *, #48689, .T. ) ;
#26615 = CARTESIAN_POINT ( 'NONE',  ( 1.923959828134896410, -77.45840880865959832, 9.047739647329839485 ) ) ;
#26616 = CARTESIAN_POINT ( 'NONE',  ( 10.74764839381999870, -78.05788108345298326, -0.2248421733643000131 ) ) ;
#26617 = CARTESIAN_POINT ( 'NONE',  ( -9.500000000000000000, -78.39999999999999147, 0.000000000000000000 ) ) ;
#26618 = CARTESIAN_POINT ( 'NONE',  ( 9.045658679128999680, -79.16680423747999384, 3.115350657311999782 ) ) ;
#26619 = CIRCLE ( 'NONE', #39818, 8.500000000000000000 ) ;
#26620 = CARTESIAN_POINT ( 'NONE',  ( 11.22440497532000059, -76.55645138378999093, -3.648307665617999795 ) ) ;
#26621 = CARTESIAN_POINT ( 'NONE',  ( -8.709378738715637169, -79.43268344339898590, -3.800117602320954635 ) ) ;
#26622 = CARTESIAN_POINT ( 'NONE',  ( 7.624341766629000539, -55.53514853726999689, -10.42531125022999916 ) ) ;
#26623 = CARTESIAN_POINT ( 'NONE',  ( -1.635010352784000087, -80.60330397784099432, -10.62493487727000030 ) ) ;
#26624 = AXIS2_PLACEMENT_3D ( 'NONE', #7641, #47546, #38072 ) ;
#26625 = CARTESIAN_POINT ( 'NONE',  ( 12.57433760367000097, -18.28878254117000068, -1.760777649351999985 ) ) ;
#26626 = CARTESIAN_POINT ( 'NONE',  ( -10.01749676170999948, -23.19181054693000021, -7.660430254659999605 ) ) ;
#26627 = CARTESIAN_POINT ( 'NONE',  ( -10.82077207570563537, -76.66777856290951831, 4.579176815933520217 ) ) ;
#26628 = ORIENTED_EDGE ( 'NONE', *, *, #7631, .T. ) ;
#26629 = CARTESIAN_POINT ( 'NONE',  ( 7.613064433753999438, -78.76183641763000765, 9.349774124741999870 ) ) ;
#26630 = CARTESIAN_POINT ( 'NONE',  ( -7.756275637014999447, -54.57995361804000112, 10.15825999914999933 ) ) ;
#26631 = CARTESIAN_POINT ( 'NONE',  ( -6.121609607564330702, -78.02338199628493953, 8.836716547392137855 ) ) ;
#26632 = CARTESIAN_POINT ( 'NONE',  ( -11.06076315227999984, -78.10252046055900621, 4.601693484369000053 ) ) ;
#26633 = ADVANCED_FACE ( 'NONE', ( #37338 ), #20490, .F. ) ;
#26634 = CARTESIAN_POINT ( 'NONE',  ( -7.765024210423000284, -17.90905971384000139, -9.830784063418001040 ) ) ;
#26636 = CARTESIAN_POINT ( 'NONE',  ( -1.930009203935999951, -18.79900967682999635, -12.72537718777000038 ) ) ;
#26635 = CARTESIAN_POINT ( 'NONE',  ( 4.658432487275518064, -78.43336646302013548, 8.082308736674995941 ) ) ;
#26637 = DIRECTION ( 'NONE',  ( 0.000000000000000000, 0.000000000000000000, -1.000000000000000000 ) ) ;
#26638 = CARTESIAN_POINT ( 'NONE',  ( -11.15381322820999976, -80.61990947872999413, 0.1149043147075999999 ) ) ;
#26639 = CARTESIAN_POINT ( 'NONE',  ( 5.838193839761705917, -78.47708333333333997, -7.596835002782701629 ) ) ;
#26640 = CARTESIAN_POINT ( 'NONE',  ( -7.012165219465999577, -77.25189398569099808, 8.812689912465000219 ) ) ;
#26641 = DIRECTION ( 'NONE',  ( -0.7071067811865474617, -0.7071067811865474617, 1.396797134838093180E-09 ) ) ;
#26642 = CARTESIAN_POINT ( 'NONE',  ( 9.611650271896829523, -79.99166666667116488, 5.539808784079915505 ) ) ;
#26643 = VERTEX_POINT ( 'NONE', #40902 ) ;
#26644 = CARTESIAN_POINT ( 'NONE',  ( 2.597074403235505535, -1.403616780896163041, 1.995008052711377822 ) ) ;
#26645 = CARTESIAN_POINT ( 'NONE',  ( -1.194090706002000069, -54.35968341064000242, 12.43436538485999954 ) ) ;
#26646 = CARTESIAN_POINT ( 'NONE',  ( -12.60413670420000010, -23.30716680861999990, 1.799502287691000069 ) ) ;
#26647 = CARTESIAN_POINT ( 'NONE',  ( 3.698594611804000287, -2.026219782538000391, -1.432312655390999945 ) ) ;
#26648 = CARTESIAN_POINT ( 'NONE',  ( 8.278055182862001260, -79.24824129696499142, 4.729100463561999312 ) ) ;
#26649 = AXIS2_PLACEMENT_3D ( 'NONE', #3360, #21355, #39372 ) ;
#26650 = CARTESIAN_POINT ( 'NONE',  ( 1.997276839918477265, -1.677083333333332815, -2.598917237794082791 ) ) ;
#26651 = LINE ( 'NONE', #21658, #39323 ) ;
#26652 = CARTESIAN_POINT ( 'NONE',  ( -1.930638663164000235, -60.02122063256000217, 12.72375916875000179 ) ) ;
#26653 = CARTESIAN_POINT ( 'NONE',  ( 12.77649795263000065, -16.69168567756999977, -0.06462540730616000983 ) ) ;
#26654 = CARTESIAN_POINT ( 'NONE',  ( 3.013741045381999939, -84.31807450217398525, 2.824158001876999613 ) ) ;
#26655 = CYLINDRICAL_SURFACE ( 'NONE', #9407, 14.00000000000000000 ) ;
#26656 = B_SPLINE_CURVE_WITH_KNOTS ( 'NONE', 3,
 ( #52261, #15951, #33070, #33941, #51981, #29225, #28351, #24522, #2677, #51115 ),
 .UNSPECIFIED., .F., .F.,
 ( 4, 2, 2, 2, 4 ),
 ( 0.000000000000000000, 0.2500000000000001665, 0.5000000000000002220, 0.7500000000000001110, 1.000000000000000000 ),
 .UNSPECIFIED. ) ;
#26657 = AXIS2_PLACEMENT_3D ( 'NONE', #38913, #52218, #39197 ) ;
#26658 = CARTESIAN_POINT ( 'NONE',  ( 10.50279984750154405, -77.24346446326944715, 5.851000335417166909 ) ) ;
#26659 = CARTESIAN_POINT ( 'NONE',  ( -5.967760218777000247, -78.67259870393999677, 10.31870413016000043 ) ) ;
#26660 = B_SPLINE_SURFACE_WITH_KNOTS ( 'NONE', 3, 3, ( 
 ( #38905, #44794, #58072, #17632 ),
 ( #35621, #4346, #4937, #4650 ),
 ( #22649, #45096, #58370, #45395 ),
 ( #31779, #21760, #26193, #35033 ),
 ( #17334, #54244, #22941, #9367 ),
 ( #4045, #40659, #17932, #49224 ),
 ( #48647, #22346, #12898, #18233 ),
 ( #30613, #35922, #53649, #8773 ) ),
 .UNSPECIFIED., .F., .F., .F.,
 ( 4, 1, 1, 1, 1, 4 ),
 ( 4, 4 ),
 ( -0.01200407347463999970, 0.000000000000000000, 0.3333333333333000081, 0.6666666666667000474, 1.000000000000000000, 1.011997855551999947 ),
 ( -0.3559705542741999906, 1.355970554273999928 ),
 .UNSPECIFIED. ) ;
#26661 = CARTESIAN_POINT ( 'NONE',  ( -10.62993649278000063, -77.74980203896600983, 3.720001978191000092 ) ) ;
#26662 = CARTESIAN_POINT ( 'NONE',  ( 0.6397441051095902331, -81.93232338606405563, 1.073892556932021236 ) ) ;
#26663 = CARTESIAN_POINT ( 'NONE',  ( 0.3696045101069000416, -79.60420299592999527, -1.269527782653000036 ) ) ;
#26664 = CARTESIAN_POINT ( 'NONE',  ( 7.714905556308770507, -79.55033101189913225, -5.543136766205470245 ) ) ;
#26665 = CARTESIAN_POINT ( 'NONE',  ( -1.463637355772988258, -83.22975666182372834, 0.3812367531431999357 ) ) ;
#26666 = B_SPLINE_CURVE_WITH_KNOTS ( 'NONE', 3,
 ( #29366, #25523, #20527, #39396, #30233, #15804, #39104, #56831, #47990, #11677, #48276, #7812, #56254, #29652, #2813, #51834, #12242, #38814 ),
 .UNSPECIFIED., .F., .F.,
 ( 4, 2, 2, 2, 2, 2, 2, 2, 4 ),
 ( 0.000000000000000000, 0.1249999999999999445, 0.2499999999999998890, 0.3749999999999999445, 0.5000000000000000000, 0.6250000000000000000, 0.7500000000000001110, 0.8750000000000000000, 1.000000000000000000 ),
 .UNSPECIFIED. ) ;
#26667 = CARTESIAN_POINT ( 'NONE',  ( -12.70926857202000093, -60.20841990675999966, 1.933876778424000076 ) ) ;
#26668 = CARTESIAN_POINT ( 'NONE',  ( 0.9450957028779182201, -80.23244768896006462, -10.70949845984780957 ) ) ;
#26669 = DIRECTION ( 'NONE',  ( -0.7071067811865474617, 0.000000000000000000, 0.7071067811865474617 ) ) ;
#26670 = CARTESIAN_POINT ( 'NONE',  ( 11.14131185284651160, -79.09065718773078402, -1.301068469138584760 ) ) ;
#26671 = AXIS2_PLACEMENT_3D ( 'NONE', #24575, #42301, #20441 ) ;
#26672 = B_SPLINE_CURVE_WITH_KNOTS ( 'NONE', 3,
 ( #54189, #31724, #45336, #22884, #40895, #485, #36456, #54483, #32016, #50058 ),
 .UNSPECIFIED., .F., .F.,
 ( 4, 2, 2, 2, 4 ),
 ( 0.000000000000000000, 0.2499999999999998890, 0.5000000000000000000, 0.7500000000000001110, 1.000000000000000000 ),
 .UNSPECIFIED. ) ;
#26673 = CARTESIAN_POINT ( 'NONE',  ( 12.00000000000000000, -79.25000000000000000, 1.072514965728000067E-08 ) ) ;
#26674 = EDGE_CURVE ( 'NONE', #8817, #7824, #5041, .T. ) ;
#26675 = DIRECTION ( 'NONE',  ( -1.000000000000000000, 0.000000000000000000, 0.000000000000000000 ) ) ;
#26676 = CARTESIAN_POINT ( 'NONE',  ( -1.646570173782999857, -78.71008588794200023, 11.14103995232000166 ) ) ;
#26677 = CARTESIAN_POINT ( 'NONE',  ( 8.178338515874312264, -55.49583131490126675, 7.356278612544881135 ) ) ;
#26678 = ORIENTED_EDGE ( 'NONE', *, *, #15989, .F. ) ;
#26679 = ORIENTED_EDGE ( 'NONE', *, *, #11036, .F. ) ;
#26680 = EDGE_CURVE ( 'NONE', #10296, #5424, #48635, .T. ) ;
#26681 = CARTESIAN_POINT ( 'NONE',  ( -2.616124927519058563, -0.7500000000000001110, 2.353768604702249689 ) ) ;
#26682 = ORIENTED_EDGE ( 'NONE', *, *, #17037, .T. ) ;
#26683 = FACE_OUTER_BOUND ( 'NONE', #52196, .T. ) ;
#26684 = VERTEX_POINT ( 'NONE', #55059 ) ;
#26685 = CARTESIAN_POINT ( 'NONE',  ( 3.942135768300999654, -80.00347729592307644, -10.54187931140000067 ) ) ;
#26686 = CARTESIAN_POINT ( 'NONE',  ( 2.917534638751946741, -79.31666666146197997, -1.828613902223640286 ) ) ;
#26687 = CARTESIAN_POINT ( 'NONE',  ( 1.081678475801000072, -79.50832130042100232, 10.97869327635999781 ) ) ;
#26688 = CARTESIAN_POINT ( 'NONE',  ( 6.043427764450807871, -76.46666666664967238, -10.48543666025108934 ) ) ;
#26689 = CARTESIAN_POINT ( 'NONE',  ( 3.146268143924999983, -79.89270551910098561, 2.052405227492000162 ) ) ;
#26690 = CARTESIAN_POINT ( 'NONE',  ( -2.442127856336522296, -79.29558379175310279, 9.187477159757261091 ) ) ;
#26691 = ORIENTED_EDGE ( 'NONE', *, *, #9647, .T. ) ;
#26692 = CARTESIAN_POINT ( 'NONE',  ( -11.00724581733999941, -77.84385847628304589, 0.8512868710715000287 ) ) ;
#26694 = EDGE_CURVE ( 'NONE', #6154, #326, #10033, .T. ) ;
#26693 = CARTESIAN_POINT ( 'NONE',  ( 2.613357750217999875, -78.77637553137999760, 11.92719643999999946 ) ) ;
#26695 = ORIENTED_EDGE ( 'NONE', *, *, #46100, .F. ) ;
#26696 = VERTEX_POINT ( 'NONE', #52384 ) ;
#26697 = CARTESIAN_POINT ( 'NONE',  ( 0.1865657191063679332, -77.88443992253993997, -1.522241462990436611 ) ) ;
#26698 = VECTOR ( 'NONE', #421, 1000.000000000000114 ) ;
#26699 = B_SPLINE_SURFACE_WITH_KNOTS ( 'NONE', 3, 3, ( 
 ( #42172, #51624, #15297, #33291 ),
 ( #6437, #11178, #38019, #6732 ),
 ( #24739, #42754, #2318, #20312 ),
 ( #3456, #30303, #52476, #57473 ),
 ( #47777, #7883, #25884, #2886 ),
 ( #30597, #48067, #20882, #48629 ),
 ( #30882, #30012, #44476, #43617 ),
 ( #3180, #38886, #39469, #26453 ) ),
 .UNSPECIFIED., .F., .F., .F.,
 ( 4, 1, 1, 1, 1, 4 ),
 ( 4, 4 ),
 ( -0.01200407347464999865, 0.000000000000000000, 0.3333333333333000081, 0.6666666666667000474, 1.000000000000000000, 1.011997855551999947 ),
 ( -0.3559705542741999906, 1.355970554273999928 ),
 .UNSPECIFIED. ) ;
#26700 = CARTESIAN_POINT ( 'NONE',  ( -0.5470841013496000604, -79.85702391966199798, -1.216254552179000026 ) ) ;
#26701 = CARTESIAN_POINT ( 'NONE',  ( 8.553489385229999797, -78.99537007017698897, 4.133741566275999979 ) ) ;
#26702 = CARTESIAN_POINT ( 'NONE',  ( -3.422298439130150971, -86.39318692756695839, 1.601665484175957443 ) ) ;
#26703 = CARTESIAN_POINT ( 'NONE',  ( 2.692109722253454240, -85.85905354011360657, 2.287895808997782332 ) ) ;
#26704 = CARTESIAN_POINT ( 'NONE',  ( -10.89021090039136119, -79.10416666669993901, 4.844266348695080993 ) ) ;
#26705 = FACE_OUTER_BOUND ( 'NONE', #6159, .T. ) ;
#26706 = CARTESIAN_POINT ( 'NONE',  ( 9.442000951725852076, -77.80242193750341073, 0.3056363532403006955 ) ) ;
#26707 = DIRECTION ( 'NONE',  ( 1.000000000000000000, 0.000000000000000000, 0.000000000000000000 ) ) ;
#26708 = B_SPLINE_CURVE_WITH_KNOTS ( 'NONE', 3,
 ( #31769, #18797, #13179, #31172, #49213, #4335, #8762, #22337, #40351, #1675, #41809, #6957, #29380, #10823, #28799, #1384, #28206, #33223 ),
 .UNSPECIFIED., .F., .F.,
 ( 4, 2, 2, 2, 2, 2, 2, 2, 4 ),
 ( 0.000000000000000000, 0.06249999999999379663, 0.1249999999999875933, 0.2499999999999862332, 0.4999999999999847899, 0.7499999999999832356, 0.8124999999999849010, 0.8749999999999864553, 1.000000000000000000 ),
 .UNSPECIFIED. ) ;
#26709 = CARTESIAN_POINT ( 'NONE',  ( 1.604404035714000143, -80.85856839617498792, -3.805837802621000243 ) ) ;
#26710 = CYLINDRICAL_SURFACE ( 'NONE', #52499, 11.59999999999999964 ) ;
#26711 = DIRECTION ( 'NONE',  ( 1.000000000000000000, 0.000000000000000000, 0.000000000000000000 ) ) ;
#26712 = CARTESIAN_POINT ( 'NONE',  ( 2.968793402029999751, -79.53150264934789959, 1.936809095135999748 ) ) ;
#26713 = B_SPLINE_CURVE_WITH_KNOTS ( 'NONE', 3,
 ( #40066, #48941, #48372, #4055 ),
 .UNSPECIFIED., .F., .F.,
 ( 4, 4 ),
 ( 0.000000000000000000, 1.000000000000000000 ),
 .UNSPECIFIED. ) ;
#26714 = CIRCLE ( 'NONE', #20129, 14.00000000000000000 ) ;
#26715 = DIRECTION ( 'NONE',  ( 0.8965517241377957136, -0.4429390544366978988, 5.195107294746977201E-07 ) ) ;
#26716 = CARTESIAN_POINT ( 'NONE',  ( -0.8496252788811309298, -80.98142198267933622, 10.71628590444292328 ) ) ;
#26717 = CARTESIAN_POINT ( 'NONE',  ( 6.985849709488999970, -81.07991142482880775, -8.837815942395002011 ) ) ;
#26718 = CARTESIAN_POINT ( 'NONE',  ( -2.707053224964000027, -2.720634141345999790, 2.675433656965999774 ) ) ;
#26719 = CARTESIAN_POINT ( 'NONE',  ( -1.152722609229902551, -80.21492969711312071, 0.5434249559639973137 ) ) ;
#26720 = AXIS2_PLACEMENT_3D ( 'NONE', #20092, #51392, #10948 ) ;
#26721 = ORIENTED_EDGE ( 'NONE', *, *, #37977, .F. ) ;
#26722 = FACE_OUTER_BOUND ( 'NONE', #58358, .T. ) ;
#26723 = CARTESIAN_POINT ( 'NONE',  ( -11.00000000000000000, -79.21041666666666003, -1.439896632895322881 ) ) ;
#26724 = CARTESIAN_POINT ( 'NONE',  ( 0.6791306551168999617, -81.34563076576598917, -1.147762040996999966 ) ) ;
#26725 = CARTESIAN_POINT ( 'NONE',  ( -3.692578928296568641, -78.99333333333336782, -8.789099506565383635 ) ) ;
#26726 = CARTESIAN_POINT ( 'NONE',  ( -1.338697082642999803, -78.09946573606998754, -12.94399764267999942 ) ) ;
#26727 = ADVANCED_FACE ( 'NONE', ( #28763 ), #25212, .F. ) ;
#26728 = CARTESIAN_POINT ( 'NONE',  ( 8.461214143919999486, -79.29648667140099860, 4.596358662803000428 ) ) ;
#26729 = CARTESIAN_POINT ( 'NONE',  ( 12.92181194095000052, -21.75648180056000314, -2.062502994258999856 ) ) ;
#26730 = ORIENTED_EDGE ( 'NONE', *, *, #50522, .T. ) ;
#26731 = CARTESIAN_POINT ( 'NONE',  ( 3.938458446976999205, -79.21000000000000796, -8.369650235310999165 ) ) ;
#26732 = CARTESIAN_POINT ( 'NONE',  ( -1.272578778811999989, -80.89250696768399962, -0.6917752173717000019 ) ) ;
#26733 = CARTESIAN_POINT ( 'NONE',  ( -1.799490220168999954, -22.77129148951999937, -12.64502302235000109 ) ) ;
#26734 = CARTESIAN_POINT ( 'NONE',  ( -8.517419447173999458, -77.42363726481998754, 3.788002893487000033 ) ) ;
#26736 = CARTESIAN_POINT ( 'NONE',  ( -3.161392481395000065, -1.852626005360999972, -1.501864700490999960 ) ) ;
#26735 = CARTESIAN_POINT ( 'NONE',  ( 3.046275090675000019, -84.07325862280099216, 2.854788613758000082 ) ) ;
#26737 = CARTESIAN_POINT ( 'NONE',  ( -2.062670899361999766, -55.49360215019999742, -12.83044027758000105 ) ) ;
#26738 = CARTESIAN_POINT ( 'NONE',  ( -0.2660992726780999629, -79.93635278971700586, 1.492693313845999903 ) ) ;
#26739 = VERTEX_POINT ( 'NONE', #38503 ) ;
#26740 = CARTESIAN_POINT ( 'NONE',  ( 7.631340703017165161, -77.28798361778574133, -7.571206356639036628 ) ) ;
#26741 = CARTESIAN_POINT ( 'NONE',  ( -0.7554284705563483193, -78.98333333333333428, -1.310679582531387721 ) ) ;
#26742 = CARTESIAN_POINT ( 'NONE',  ( 0.5495870423892605938, -78.90418355198266909, -3.893366406191818729 ) ) ;
#26743 = EDGE_LOOP ( 'NONE', ( #5857, #47786, #28311, #27116 ) ) ;
#26744 = EDGE_LOOP ( 'NONE', ( #33388, #31988, #21460 ) ) ;
#26745 = CARTESIAN_POINT ( 'NONE',  ( -9.475012188928999990, -79.32915461743898788, 5.469182786826999987 ) ) ;
#26746 = VECTOR ( 'NONE', #44336, 1000.000000000000000 ) ;
#26747 =( LENGTH_UNIT ( ) NAMED_UNIT ( * ) SI_UNIT ( .MILLI., .METRE. ) );
#26748 = CARTESIAN_POINT ( 'NONE',  ( -10.61206674237698522, -80.48532644614452636, 1.982131822504892060 ) ) ;
#26749 = EDGE_LOOP ( 'NONE', ( #34729, #43322, #10893, #7537, #57991 ) ) ;
#26750 = EDGE_CURVE ( 'NONE', #7386, #27557, #56519, .T. ) ;
#26751 = CARTESIAN_POINT ( 'NONE',  ( -3.566334030200000171, -77.59004702781498963, 11.50986677841000017 ) ) ;
#26752 = ORIENTED_EDGE ( 'NONE', *, *, #15874, .T. ) ;
#26753 = VERTEX_POINT ( 'NONE', #10784 ) ;
#26754 = CARTESIAN_POINT ( 'NONE',  ( -2.982898973896713102, -2.633265934789509544, -1.289165251780844512 ) ) ;
#26755 = CARTESIAN_POINT ( 'NONE',  ( 9.722718241315000398, -18.75000000000000000, -7.954951288349001004 ) ) ;
#26756 = CARTESIAN_POINT ( 'NONE',  ( -8.448510849392999233, -79.70817963672152473, 4.901364000006999788 ) ) ;
#26757 = EDGE_LOOP ( 'NONE', ( #39824, #57528, #26816, #3468 ) ) ;
#26758 = B_SPLINE_CURVE_WITH_KNOTS ( 'NONE', 3,
 ( #5125, #41129, #27244, #5691, #14254, #19284, #27535, #45283, #49715, #36403, #9259, #4831, #55288, #18700, #40842, #436, #50880, #54431 ),
 .UNSPECIFIED., .F., .F.,
 ( 4, 2, 2, 2, 2, 2, 2, 2, 4 ),
 ( 0.000000000000000000, 0.1249999999999999445, 0.2499999999999998890, 0.3749999999999998335, 0.4999999999999998890, 0.6249999999999998890, 0.7500000000000000000, 0.8750000000000000000, 1.000000000000000000 ),
 .UNSPECIFIED. ) ;
#26760 = EDGE_CURVE ( 'NONE', #26528, #36311, #16078, .T. ) ;
#26759 = CARTESIAN_POINT ( 'NONE',  ( 1.251843065520180875, -82.06770833143092148, -0.7205419773649445192 ) ) ;
#26761 = EDGE_LOOP ( 'NONE', ( #14204, #14344, #6314, #17695 ) ) ;
#26762 = CARTESIAN_POINT ( 'NONE',  ( -0.9248060758160334682, -80.21013857831869132, -0.8761209355067355320 ) ) ;
#26763 = CARTESIAN_POINT ( 'NONE',  ( -4.000000000000000000, -5.000000000000000000, -0.5999999999999999778 ) ) ;
#26764 = FACE_OUTER_BOUND ( 'NONE', #23080, .T. ) ;
#26765 = CARTESIAN_POINT ( 'NONE',  ( 0.5999999999999999778, -18.84999999999999787, 10.98362417419999915 ) ) ;
#26766 = DIRECTION ( 'NONE',  ( 0.000000000000000000, -1.000000000000000000, 0.000000000000000000 ) ) ;
#26767 = CARTESIAN_POINT ( 'NONE',  ( 14.00000000000000000, -46.13782243168999742, 5.544480867911000210E-06 ) ) ;
#26768 = CIRCLE ( 'NONE', #33400, 12.00000000000000000 ) ;
#26769 = CARTESIAN_POINT ( 'NONE',  ( 7.654537085013999764, -55.51943307300000185, -10.01332844635999919 ) ) ;
#26770 = DIRECTION ( 'NONE',  ( -1.186310310053999794E-10, -0.9999999999999998890, 1.114594443524999723E-08 ) ) ;
#26771 = CARTESIAN_POINT ( 'NONE',  ( -10.08161778466999969, -24.71855282893000094, 7.981584069265998949 ) ) ;
#26772 = CARTESIAN_POINT ( 'NONE',  ( 8.082447335412272338, -77.80849359151311262, -4.658563211049076003 ) ) ;
#26773 = AXIS2_PLACEMENT_3D ( 'NONE', #29920, #48257, #29064 ) ;
#26774 = CARTESIAN_POINT ( 'NONE',  ( 4.118579373781999564, -80.85425264934799827, -0.6833035357645000918 ) ) ;
#26775 = CARTESIAN_POINT ( 'NONE',  ( 5.853183942465999934, -76.99826001420200328, -7.526330923816999530 ) ) ;
#26776 = CARTESIAN_POINT ( 'NONE',  ( -12.77651047532000028, -16.69104280938000073, -0.04320343284645000032 ) ) ;
#26777 = CARTESIAN_POINT ( 'NONE',  ( 0.000000000000000000, -0.09999999995300053179, 0.000000000000000000 ) ) ;
#26778 = CARTESIAN_POINT ( 'NONE',  ( -2.061649843245999758, -23.20561307587000144, 12.83797346714000120 ) ) ;
#26779 = CARTESIAN_POINT ( 'NONE',  ( -8.861449449424647185, -80.04887384436648290, 6.625956105248708816 ) ) ;
#26780 = DIRECTION ( 'NONE',  ( -0.7071067811865474617, 0.000000000000000000, 0.7071067811865474617 ) ) ;
#26781 = CARTESIAN_POINT ( 'NONE',  ( -1.113858406170999960, -0.8703954782496999831, 3.266031882984000045 ) ) ;
#26782 = CARTESIAN_POINT ( 'NONE',  ( 0.000000000000000000, -39.30476017083000073, 0.000000000000000000 ) ) ;
#26783 = CIRCLE ( 'NONE', #1375, 0.5000000000000006661 ) ;
#26784 = CARTESIAN_POINT ( 'NONE',  ( -0.2986795320787701824, -79.95859341831706502, -1.481281548820393423 ) ) ;
#26785 = CARTESIAN_POINT ( 'NONE',  ( 12.68624828431999951, -60.56426635971000394, -1.886933512377000133 ) ) ;
#26786 = CARTESIAN_POINT ( 'NONE',  ( -1.509488703453999880, -79.36014632351999865, -0.1420306293263000064 ) ) ;
#26787 = DIRECTION ( 'NONE',  ( 0.7592504788685918715, -0.04890177849870949028, 0.6489586476790929481 ) ) ;
#26788 = CARTESIAN_POINT ( 'NONE',  ( 10.72166763895999964, -77.29165712091899820, 2.054558110510000368 ) ) ;
#26789 = EDGE_CURVE ( 'NONE', #48346, #26170, #37918, .T. ) ;
#26790 = CARTESIAN_POINT ( 'NONE',  ( 11.98062200086999951, -77.17727113527298854, -2.108850158091000182 ) ) ;
#26791 = CARTESIAN_POINT ( 'NONE',  ( 10.61050599188999932, -78.32876026662599145, -2.901234667509999809 ) ) ;
#26793 = CARTESIAN_POINT ( 'NONE',  ( -1.287313221243000072, -78.26290954478920980, 0.5940404451740000091 ) ) ;
#26792 = CARTESIAN_POINT ( 'NONE',  ( -10.20000000000000107, -0.2000000000000000111, 0.000000000000000000 ) ) ;
#26794 = CARTESIAN_POINT ( 'NONE',  ( -1.596184505169000012, -82.29829480068998748, -0.5933059756569000198 ) ) ;
#26795 = VERTEX_POINT ( 'NONE', #7503 ) ;
#26796 = EDGE_CURVE ( 'NONE', #23377, #29770, #7860, .T. ) ;
#26797 = CARTESIAN_POINT ( 'NONE',  ( -0.7270703755450000916, -83.83321544543098014, -3.685475648053000430 ) ) ;
#26798 = DIRECTION ( 'NONE',  ( -0.9859154929576978699, -0.1672442547472993701, -2.241745476049995391E-11 ) ) ;
#26799 = CARTESIAN_POINT ( 'NONE',  ( 2.332976527971999836, -80.78287663268979202, -10.92616016422999969 ) ) ;
#26800 = LINE ( 'NONE', #54282, #20948 ) ;
#26801 = CARTESIAN_POINT ( 'NONE',  ( 2.209590870513934657, -85.65677084043076661, 2.597958555648024248 ) ) ;
#26802 = CARTESIAN_POINT ( 'NONE',  ( 10.29113596735999892, -77.61645131797199326, 4.462133020506000136 ) ) ;
#26803 = CARTESIAN_POINT ( 'NONE',  ( 6.760013919724039866, -78.92291666666670835, 8.796335266379998075 ) ) ;
#26804 = CARTESIAN_POINT ( 'NONE',  ( 5.110488341091000031, -78.66022958144499455, 8.291116005822999568 ) ) ;
#26805 = CARTESIAN_POINT ( 'NONE',  ( 2.970509141730999669, -1.114596044169000155, 2.718337110757000019 ) ) ;
#26806 = CARTESIAN_POINT ( 'NONE',  ( -10.10989699479836723, -76.34329898052499175, -6.122700102344563078 ) ) ;
#26807 = DIRECTION ( 'NONE',  ( -0.7026410690473252618, 0.1122098755728027641, 0.7026410690473252618 ) ) ;
#26808 = CARTESIAN_POINT ( 'NONE',  ( -1.667917367065999912, -55.51943464808999806, 12.49306764013999960 ) ) ;
#26809 = ORIENTED_EDGE ( 'NONE', *, *, #31115, .F. ) ;
#26810 = DIRECTION ( 'NONE',  ( 0.000000000000000000, 0.000000000000000000, -1.000000000000000000 ) ) ;
#26811 = CARTESIAN_POINT ( 'NONE',  ( -2.935661446561999899, -76.94999999999998863, -9.035036904803998681 ) ) ;
#26812 = CARTESIAN_POINT ( 'NONE',  ( -12.56594317984999876, -18.75000000536999778, 1.750000000000000000 ) ) ;
#26813 = CARTESIAN_POINT ( 'NONE',  ( -0.5713041596650000331, -79.48428941834998795, -1.442599867604999808 ) ) ;
#26814 = CARTESIAN_POINT ( 'NONE',  ( -12.80896991324999945, -58.55453807205000061, -1.930989179114000143 ) ) ;
#26815 = CIRCLE ( 'NONE', #8923, 11.00000000000000000 ) ;
#26816 = ORIENTED_EDGE ( 'NONE', *, *, #410, .F. ) ;
#26817 = EDGE_CURVE ( 'NONE', #58355, #51020, #50853, .T. ) ;
#26818 = CYLINDRICAL_SURFACE ( 'NONE', #30372, 0.5000000000000004441 ) ;
#26819 = DIRECTION ( 'NONE',  ( -1.000000000000000000, 0.000000000000000000, 0.000000000000000000 ) ) ;
#26820 = DIRECTION ( 'NONE',  ( 0.000000000000000000, 0.000000000000000000, -1.000000000000000000 ) ) ;
#26821 = ORIENTED_EDGE ( 'NONE', *, *, #4135, .F. ) ;
#26822 = CARTESIAN_POINT ( 'NONE',  ( -9.523369619434999933, -53.98054357652999613, -8.220347091585999522 ) ) ;
#26823 = AXIS2_PLACEMENT_3D ( 'NONE', #51836, #11391, #2527 ) ;
#26824 = CARTESIAN_POINT ( 'NONE',  ( -8.396223008680999911, -79.87282602934199360, -4.990405176070999538 ) ) ;
#26825 = ORIENTED_EDGE ( 'NONE', *, *, #2994, .F. ) ;
#26826 = ORIENTED_EDGE ( 'NONE', *, *, #48303, .T. ) ;
#26828 = ADVANCED_FACE ( 'NONE', ( #39656 ), #18706, .F. ) ;
#26827 = CARTESIAN_POINT ( 'NONE',  ( 5.491357861347999858, -76.35279548927898929, -11.06493742798000035 ) ) ;
#26829 = CARTESIAN_POINT ( 'NONE',  ( -10.74991479005951511, -78.60500528859236624, -0.6569711721753703770 ) ) ;
#26830 = CARTESIAN_POINT ( 'NONE',  ( -1.630350418686000280, -79.25822497536000810, 0.2425001497127999839 ) ) ;
#26831 = EDGE_CURVE ( 'NONE', #28437, #12549, #45874, .T. ) ;
#26832 = EDGE_LOOP ( 'NONE', ( #4037, #12831, #24306, #5369 ) ) ;
#26833 = CARTESIAN_POINT ( 'NONE',  ( 12.50240633877000107, -17.31762602171999887, 1.005381409788000058 ) ) ;
#26834 = CARTESIAN_POINT ( 'NONE',  ( 1.260662490416350812, -77.71453862646123412, 9.622086981278945572 ) ) ;
#26835 = CARTESIAN_POINT ( 'NONE',  ( 1.071781563306112961, -80.30709819530763127, -0.6451663486076436582 ) ) ;
#26836 = CARTESIAN_POINT ( 'NONE',  ( 6.944463141141999252, -76.66805712980000465, -9.899892744310998083 ) ) ;
#26837 = CARTESIAN_POINT ( 'NONE',  ( 4.275724345439000373, -76.90612153646102911, -10.36997068233999997 ) ) ;
#26838 = CARTESIAN_POINT ( 'NONE',  ( 8.096452064242996016, -22.78578169018999944, 13.15643568217000769 ) ) ;
#26839 = CARTESIAN_POINT ( 'NONE',  ( -3.649946715412064613, -86.25171438276198899, 1.543298655876290448 ) ) ;
#26840 = CARTESIAN_POINT ( 'NONE',  ( 7.808618912244999599, -79.08795908749598880, -8.052551227705000869 ) ) ;
#26841 = CARTESIAN_POINT ( 'NONE',  ( 8.994003557245340730, -79.86886930543070662, 2.160818744066264951 ) ) ;
#26842 = CARTESIAN_POINT ( 'NONE',  ( -1.250000000013809398, -82.25000000000000000, -0.2084624058389335510 ) ) ;
#26843 = ORIENTED_EDGE ( 'NONE', *, *, #2566, .F. ) ;
#26844 = CARTESIAN_POINT ( 'NONE',  ( 2.486604901413132840, -77.65416666666668277, 9.252740428349005342 ) ) ;
#26845 = CARTESIAN_POINT ( 'NONE',  ( -10.62397638184999948, -76.09413970748998679, -6.218250916117999516 ) ) ;
#26846 = CARTESIAN_POINT ( 'NONE',  ( -1.379800422845999908, -80.88668858139899953, -0.6283944928419999965 ) ) ;
#26847 = CARTESIAN_POINT ( 'NONE',  ( -0.8575312565364999751, -77.72675193319649622, -1.002634541711000082 ) ) ;
#26848 = CARTESIAN_POINT ( 'NONE',  ( 3.349726343964253061, -3.124127367323429993, 1.080338306304951201 ) ) ;
#26849 = EDGE_CURVE ( 'NONE', #22110, #37067, #24146, .T. ) ;
#26850 = CARTESIAN_POINT ( 'NONE',  ( 7.685661446562000343, -77.00000000000000000, -5.583959896779000509 ) ) ;
#26851 = CARTESIAN_POINT ( 'NONE',  ( 0.000000000000000000, -90.39999999999999147, 0.000000000000000000 ) ) ;
#26852 = CARTESIAN_POINT ( 'NONE',  ( -9.102117851653074965, -61.77186524101082910, -8.583692175771709287 ) ) ;
#26853 = CARTESIAN_POINT ( 'NONE',  ( 11.05620287758999964, -79.79620241998199504, -1.500659051079999973 ) ) ;
#26854 = CARTESIAN_POINT ( 'NONE',  ( 9.130836692535000410, -77.66741332859899671, -3.055844195858999690 ) ) ;
#26855 = CARTESIAN_POINT ( 'NONE',  ( -5.469229351563153152, -76.96241952032323752, 10.75691535272135191 ) ) ;
#26856 = CARTESIAN_POINT ( 'NONE',  ( 10.75000000000000355, -79.73958333333332860, -1.407171709420407035 ) ) ;
#26857 = CARTESIAN_POINT ( 'NONE',  ( -2.176888680478372251, -76.06416033132352084, -12.84412808549582685 ) ) ;
#26858 = CIRCLE ( 'NONE', #7073, 1.749999999999999556 ) ;
#26859 = CYLINDRICAL_SURFACE ( 'NONE', #37549, 14.00000000000000000 ) ;
#26860 = VERTEX_POINT ( 'NONE', #41998 ) ;
#26861 = CARTESIAN_POINT ( 'NONE',  ( 0.4644997175289000135, -83.30604790835199935, 1.393065715888999856 ) ) ;
#26862 = AXIS2_PLACEMENT_3D ( 'NONE', #56066, #20622, #15611 ) ;
#26863 = CARTESIAN_POINT ( 'NONE',  ( 0.6904535216592000424, -80.35229747532000033, 1.161570125514999940 ) ) ;
#26864 = LINE ( 'NONE', #40749, #12551 ) ;
#26865 = CARTESIAN_POINT ( 'NONE',  ( 11.79843486695000010, -77.23445183756500398, -2.076781258317999868 ) ) ;
#26866 = DIRECTION ( 'NONE',  ( 0.000000000000000000, -1.000000000000000000, 0.000000000000000000 ) ) ;
#26867 = CARTESIAN_POINT ( 'NONE',  ( -7.587128856971000701, -78.50641514274398958, 9.212544607993001122 ) ) ;
#26868 = CARTESIAN_POINT ( 'NONE',  ( 9.345760913908002010, -78.34219805011500171, 2.683384691900000174 ) ) ;
#26869 = CARTESIAN_POINT ( 'NONE',  ( -7.562571750566999818, -77.19503301142388807, -5.786002763631000079 ) ) ;
#26870 = CARTESIAN_POINT ( 'NONE',  ( -1.930009203937000040, -55.59900967650000325, -12.72537718775000037 ) ) ;
#26871 = CARTESIAN_POINT ( 'NONE',  ( 8.992038628173702364, -76.00517836237398228, 7.564405201256904299 ) ) ;
#26872 = CARTESIAN_POINT ( 'NONE',  ( 10.36875976864000037, -78.73659464476099856, 3.767035497191999927 ) ) ;
#26873 = DIRECTION ( 'NONE',  ( 0.000000000000000000, 0.000000000000000000, 1.000000000000000000 ) ) ;
#26874 = EDGE_LOOP ( 'NONE', ( #34802, #18795, #48002, #21167 ) ) ;
#26875 = ADVANCED_FACE ( 'NONE', ( #10716 ), #14728, .T. ) ;
#26876 = CARTESIAN_POINT ( 'NONE',  ( 9.249999999999998224, -78.76041666666667140, 1.210822168571084934 ) ) ;
#26877 = DIRECTION ( 'NONE',  ( 0.000000000000000000, -1.000000000000000000, 0.000000000000000000 ) ) ;
#26878 = CIRCLE ( 'NONE', #33458, 0.5000000000000006661 ) ;
#26879 = B_SPLINE_CURVE_WITH_KNOTS ( 'NONE', 3,
 ( #24854, #41991, #42870, #20430, #20145, #7135, #55866, #29556, #1559, #46440, #55272, #38425, #15115, #15998, #25136, #43162, #24563, #10408, #19851, #6555, #51154, #19551, #10709, #28393, #37258, #47024, #28687, #37846, #38132, #42580, #15416, #56443, #2718, #33699, #51738, #5968, #11287, #6258, #42290, #33409, #2144, #51447, #56155, #29267, #47315, #17435, #30991, #44302, #7713, #53450, #56736, #39865, #47893, #3293, #43443, #44597, #3004, #57014, #16296, #12995, #57585, #21000, #21285, #34273, #49030 ),
 .UNSPECIFIED., .F., .F.,
 ( 4, 2, 2, 2, 2, 2, 2, 2, 2, 2, 2, 2, 2, 2, 2, 2, 1, 2, 2, 2, 2, 2, 2, 2, 2, 2, 2, 2, 2, 2, 2, 2, 4 ),
 ( 0.000000000000000000, 0.03125000000000000000, 0.06250000000000000000, 0.09375000000000000000, 0.1250000000000000000, 0.1562500000000000000, 0.1875000000000000000, 0.2187500000000000000, 0.2500000000000000000, 0.2812500000000000000, 0.3125000000000000000, 0.3437500000000000000, 0.3750000000000000000, 0.4062500000000000000, 0.4375000000000000000, 0.4687500000000000000, 0.5000000000000000000, 0.5312500000000000000, 0.5625000000000000000, 0.5937500000000000000, 0.6250000000000000000, 0.6562500000000000000, 0.6875000000000000000, 0.7187500000000000000, 0.7500000000000000000, 0.7812500000000000000, 0.8125000000000000000, 0.8437500000000000000, 0.8750000000000000000, 0.9062500000000000000, 0.9375000000000000000, 0.9687500000000000000, 1.000000000000000000 ),
 .UNSPECIFIED. ) ;
#26880 = CARTESIAN_POINT ( 'NONE',  ( -0.03211093172565320647, -78.62148120184446043, -3.406944224254372600 ) ) ;
#26881 = CARTESIAN_POINT ( 'NONE',  ( 10.28103400416999946, -78.26891651279798623, 3.842432268884000024 ) ) ;
#26882 = CARTESIAN_POINT ( 'NONE',  ( 5.539808784079871984, -79.26666666666666572, -9.611650271896849063 ) ) ;
#26883 = CARTESIAN_POINT ( 'NONE',  ( -2.577162953934999834, -76.40070350691199508, 11.99607385716000074 ) ) ;
#26884 = DIRECTION ( 'NONE',  ( 0.000000000000000000, -1.000000000000000000, 1.786847118832000041E-14 ) ) ;
#26885 = DIRECTION ( 'NONE',  ( 0.000000000000000000, 1.000000000000000000, 0.000000000000000000 ) ) ;
#26886 = VERTEX_POINT ( 'NONE', #38721 ) ;
#26887 = CARTESIAN_POINT ( 'NONE',  ( 2.301467643382999917, -78.35041292975199667, -10.90676452780999917 ) ) ;
#26888 = CARTESIAN_POINT ( 'NONE',  ( 0.7858904643604428530, -79.92117315916847531, 0.9723009331349696804 ) ) ;
#26889 = DIRECTION ( 'NONE',  ( -0.7071067811865474617, 3.444154817369226517E-11, 0.7071067811865474617 ) ) ;
#26890 = CARTESIAN_POINT ( 'NONE',  ( -3.999999999993000266, -77.30000000000720206, 8.632643823722999667E-11 ) ) ;
#26891 = CARTESIAN_POINT ( 'NONE',  ( 4.529234587808285362, -76.35572474536435550, -10.87075400981678541 ) ) ;
#26892 = CARTESIAN_POINT ( 'NONE',  ( 9.458764864882999390, -78.94857194687799051, -5.918054316060000097 ) ) ;
#26893 = CARTESIAN_POINT ( 'NONE',  ( -4.392572548562998058, -76.40833333333333144, 9.875985572401290824 ) ) ;
#26894 = CARTESIAN_POINT ( 'NONE',  ( 1.502971460259269421, -81.60841855634211583, 0.1731872554293665267 ) ) ;
#26895 = CARTESIAN_POINT ( 'NONE',  ( 11.48873525783000105, -78.10531157257399570, 4.336443399433000501 ) ) ;
#26896 = LINE ( 'NONE', #26594, #16070 ) ;
#26897 = CARTESIAN_POINT ( 'NONE',  ( -1.407171709420465211, -78.38541666666665719, 10.74999999999999467 ) ) ;
#26898 = CIRCLE ( 'NONE', #24093, 14.00000000000000000 ) ;
#26899 = CARTESIAN_POINT ( 'NONE',  ( 11.99999999999999822, -77.06041666666665435, 1.570796326794923203 ) ) ;
#26900 = VERTEX_POINT ( 'NONE', #25144 ) ;
#26901 = VERTEX_POINT ( 'NONE', #52314 ) ;
#26902 = LINE ( 'NONE', #35461, #26746 ) ;
#26903 = CARTESIAN_POINT ( 'NONE',  ( -9.193191990781000911, -77.60773998579799127, 2.558485205664000173 ) ) ;
#26904 = ORIENTED_EDGE ( 'NONE', *, *, #29814, .F. ) ;
#26905 = CARTESIAN_POINT ( 'NONE',  ( -8.834209325778934030, -79.71953728951929463, 3.560217370319449071 ) ) ;
#26906 = ORIENTED_EDGE ( 'NONE', *, *, #51975, .T. ) ;
#26907 = CARTESIAN_POINT ( 'NONE',  ( 9.205846894750999709, -25.00798911347999720, 8.541134278086001785 ) ) ;
#26908 = CARTESIAN_POINT ( 'NONE',  ( 7.553727747526362890, -55.11418618783646650, -7.997114030208058111 ) ) ;
#26909 = CARTESIAN_POINT ( 'NONE',  ( -8.988089064694998243, -78.16051332859899503, 3.902915570549000179 ) ) ;
#26910 = DIRECTION ( 'NONE',  ( 0.000000000000000000, -1.000000000000000000, 0.000000000000000000 ) ) ;
#26911 = CARTESIAN_POINT ( 'NONE',  ( 7.808618912244999599, -78.88459342766699933, -8.052551227705000869 ) ) ;
#26912 = CARTESIAN_POINT ( 'NONE',  ( 1.218717449224264060, -80.99999999999998579, 10.73986708482796004 ) ) ;
#26913 = ORIENTED_EDGE ( 'NONE', *, *, #39082, .T. ) ;
#26914 = ORIENTED_EDGE ( 'NONE', *, *, #21743, .F. ) ;
#26915 = CARTESIAN_POINT ( 'NONE',  ( 4.449028115235954317, -77.43534773065439936, 8.140145073587429891 ) ) ;
#26916 = CARTESIAN_POINT ( 'NONE',  ( 1.160587285869999929, -77.79677043080998544, 10.97894289003999901 ) ) ;
#26917 = CARTESIAN_POINT ( 'NONE',  ( 5.838193839761703252, -77.57708333333330586, -7.596835002782702517 ) ) ;
#26918 = CARTESIAN_POINT ( 'NONE',  ( -6.766389538252999714, -77.95405419464299257, -6.956053621355001049 ) ) ;
#26919 = CARTESIAN_POINT ( 'NONE',  ( -1.848949294450000114, -76.44493281993999290, -12.67465850452999909 ) ) ;
#26920 = EDGE_CURVE ( 'NONE', #2879, #55386, #42380, .T. ) ;
#26921 = CARTESIAN_POINT ( 'NONE',  ( -6.690353498881652428, -79.46262472211189731, -6.744430746908721908 ) ) ;
#26922 = DIRECTION ( 'NONE',  ( 0.000000000000000000, -1.000000000000000000, 0.000000000000000000 ) ) ;
#26923 = DIRECTION ( 'NONE',  ( -1.776356839400000238E-14, 1.000000000000000000, 0.000000000000000000 ) ) ;
#26924 = CARTESIAN_POINT ( 'NONE',  ( 12.66322081671000177, -16.81838367322000138, -0.1487102037789999887 ) ) ;
#26925 = CARTESIAN_POINT ( 'NONE',  ( -10.53559655517000060, -23.20569178316999981, -7.620036226160999959 ) ) ;
#26926 = DIRECTION ( 'NONE',  ( 0.000000000000000000, 0.000000000000000000, -1.000000000000000000 ) ) ;
#26927 = CARTESIAN_POINT ( 'NONE',  ( 3.430579573749999778, -83.83275779226799784, -0.8922415104712000389 ) ) ;
#26928 = ORIENTED_EDGE ( 'NONE', *, *, #2515, .F. ) ;
#26929 = CARTESIAN_POINT ( 'NONE',  ( 2.810698055981000198, -79.58445734768899626, -11.99191332196000026 ) ) ;
#26930 = CARTESIAN_POINT ( 'NONE',  ( -3.256465705460000137, -76.60672286667698927, 11.02300886902000165 ) ) ;
#26931 = CARTESIAN_POINT ( 'NONE',  ( -6.868574835607371476, -78.03023875518719876, 8.269499650932843338 ) ) ;
#26932 = CARTESIAN_POINT ( 'NONE',  ( -3.085175050843000477, -78.23816703767799652, -11.57574012064000080 ) ) ;
#26933 = CARTESIAN_POINT ( 'NONE',  ( 2.839805762151335511, -3.291666666666666963, 1.636761686205429278 ) ) ;
#26934 = FACE_OUTER_BOUND ( 'NONE', #52189, .T. ) ;
#26935 = CARTESIAN_POINT ( 'NONE',  ( 1.250000000000000000, -80.34999999999999432, 0.000000000000000000 ) ) ;
#26936 = CARTESIAN_POINT ( 'NONE',  ( 9.284235709610999976, -80.42009620847800022, 6.618340736769000365 ) ) ;
#26937 = CARTESIAN_POINT ( 'NONE',  ( -0.4831833036036000117, -82.27957484316098657, -1.158768654956999988 ) ) ;
#26938 = CARTESIAN_POINT ( 'NONE',  ( -10.47919054151000040, -77.91882059614400191, -3.800153439748000128 ) ) ;
#26939 = CARTESIAN_POINT ( 'NONE',  ( -11.68767212001979594, -78.27916666666664014, 3.140974612311315806 ) ) ;
#26940 = CARTESIAN_POINT ( 'NONE',  ( -6.515767037275000284, -80.39928196422599171, -9.178153216127999059 ) ) ;
#26941 = B_SPLINE_CURVE_WITH_KNOTS ( 'NONE', 3,
 ( #19981, #33536, #50699, #23807, #37680, #1688, #33238, #19678, #55696, #51282 ),
 .UNSPECIFIED., .F., .F.,
 ( 4, 2, 2, 2, 4 ),
 ( 0.000000000000000000, 0.2500000000000001110, 0.5000000000000002220, 0.7500000000000001110, 1.000000000000000000 ),
 .UNSPECIFIED. ) ;
#26942 = CARTESIAN_POINT ( 'NONE',  ( 3.066117107042321432, -78.29792545123773095, -10.39032517820746904 ) ) ;
#26943 = EDGE_CURVE ( 'NONE', #14108, #13029, #620, .T. ) ;
#26944 = CARTESIAN_POINT ( 'NONE',  ( -0.9781264271459999549, -53.85968856090000401, 12.65967462873999949 ) ) ;
#26945 = CARTESIAN_POINT ( 'NONE',  ( -8.123853732960998997, -77.10669903538303060, 4.915330883505999893 ) ) ;
#26946 = CARTESIAN_POINT ( 'NONE',  ( 3.961774695119000267, -3.559381257025999723, 0.1872869280730999897 ) ) ;
#26947 = CARTESIAN_POINT ( 'NONE',  ( -8.728447447808001414, -76.64562635936398749, 6.810956705545000212 ) ) ;
#26948 = CARTESIAN_POINT ( 'NONE',  ( -2.486604901413152824, -77.40416666666668277, -9.252740428349003565 ) ) ;
#26949 = CARTESIAN_POINT ( 'NONE',  ( -2.886976430161214413, -83.01666665310567339, 2.786905270152955083 ) ) ;
#26950 = CARTESIAN_POINT ( 'NONE',  ( -1.295048492659000017, -61.32893519093000378, 12.54716442239999985 ) ) ;
#26951 = CARTESIAN_POINT ( 'NONE',  ( 12.54976795933000133, -16.95224500006000312, -0.05636009750358999398 ) ) ;
#26952 = CIRCLE ( 'NONE', #57138, 0.8000000000000011546 ) ;
#26953 = CARTESIAN_POINT ( 'NONE',  ( -3.351664308082999977, -83.10399735065199422, 2.489165784748999855 ) ) ;
#26954 = DIRECTION ( 'NONE',  ( 0.000000000000000000, -1.000000000000000000, 0.000000000000000000 ) ) ;
#26955 = EDGE_CURVE ( 'NONE', #2048, #670, #16873, .T. ) ;
#26956 = CARTESIAN_POINT ( 'NONE',  ( 11.52046713918511678, -76.67862562347951894, -3.639311417233032309 ) ) ;
#26958 = EDGE_CURVE ( 'NONE', #13118, #30023, #29848, .T. ) ;
#26957 = CARTESIAN_POINT ( 'NONE',  ( -1.784936172681000022, -79.28226414830000124, -12.51137403398999837 ) ) ;
#26959 = CARTESIAN_POINT ( 'NONE',  ( -4.503658352096000073, -77.30076617252800020, -10.19664954867000084 ) ) ;
#26960 = CARTESIAN_POINT ( 'NONE',  ( -0.5432945554243000519, -81.30668225856999243, -1.398152719143000100 ) ) ;
#26961 = CARTESIAN_POINT ( 'NONE',  ( 1.427761453950999959, -79.21443200746999480, 0.1399187141794999978 ) ) ;
#26962 = CARTESIAN_POINT ( 'NONE',  ( -1.003693376006966176, -61.76223992080762315, 12.70247752668375085 ) ) ;
#26963 = CARTESIAN_POINT ( 'NONE',  ( 1.136477888908663081, -82.44026647294511179, -1.048016447884216662 ) ) ;
#26964 = CARTESIAN_POINT ( 'NONE',  ( -12.54705830253000087, -61.33699017322999936, 1.287129557046000183 ) ) ;
#26965 = CARTESIAN_POINT ( 'NONE',  ( -8.308818416638949600, -80.15545485398178016, -6.893652871022299067 ) ) ;
#26966 = CARTESIAN_POINT ( 'NONE',  ( -10.75000000000000000, -77.00000000000000000, 0.000000000000000000 ) ) ;
#26967 = CARTESIAN_POINT ( 'NONE',  ( -7.301296477453766087, -79.28131158874371920, 8.515437670024562422 ) ) ;
#26968 = CARTESIAN_POINT ( 'NONE',  ( 0.9664454468687677657, -81.79568272211004398, -0.7933871688991031013 ) ) ;
#26969 = DIRECTION ( 'NONE',  ( 0.000000000000000000, 0.000000000000000000, -1.000000000000000000 ) ) ;
#26970 = CARTESIAN_POINT ( 'NONE',  ( 8.767647372505999570, -80.19410278844959805, 6.883540450345000394 ) ) ;
#26971 = CARTESIAN_POINT ( 'NONE',  ( 7.387512494710292366, -55.38467666605775008, 8.150146600852341550 ) ) ;
#26972 = ORIENTED_EDGE ( 'NONE', *, *, #3651, .F. ) ;
#26973 = ORIENTED_EDGE ( 'NONE', *, *, #46120, .F. ) ;
#26974 = CARTESIAN_POINT ( 'NONE',  ( -12.05000000000000071, -80.60000000000000853, 0.000000000000000000 ) ) ;
#26975 = EDGE_CURVE ( 'NONE', #19162, #10981, #26024, .T. ) ;
#26976 = ORIENTED_EDGE ( 'NONE', *, *, #13474, .F. ) ;
#26977 = DIRECTION ( 'NONE',  ( 0.000000000000000000, -1.000000000000000000, 0.000000000000000000 ) ) ;
#26978 = ORIENTED_EDGE ( 'NONE', *, *, #36033, .F. ) ;
#26979 = DIRECTION ( 'NONE',  ( 0.000000000000000000, 0.000000000000000000, -1.000000000000000000 ) ) ;
#26980 = CARTESIAN_POINT ( 'NONE',  ( -5.000000000000000000, -80.49999999999998579, 0.000000000000000000 ) ) ;
#26981 = CARTESIAN_POINT ( 'NONE',  ( -0.3926218265389255779, -78.39583333333334281, 1.460959015002472494 ) ) ;
#26982 = CARTESIAN_POINT ( 'NONE',  ( 8.413030999918001740, -79.83515741644239938, -7.136010437995999212 ) ) ;
#26983 = CARTESIAN_POINT ( 'NONE',  ( 1.466594960159999905, -24.08158199052000015, -12.44238958332999800 ) ) ;
#26984 = CARTESIAN_POINT ( 'NONE',  ( -2.879473469535999808, -79.17120297221410397, -2.412504731407000058 ) ) ;
#26985 = CARTESIAN_POINT ( 'NONE',  ( -7.966670494143397008, -79.35374996792596392, 5.181185574044002706 ) ) ;
#26986 = CARTESIAN_POINT ( 'NONE',  ( 9.507661145905998978, -77.55757109829465890, -5.611464101879999333 ) ) ;
#26987 = CARTESIAN_POINT ( 'NONE',  ( 0.4463049390680999817, -78.54644978676999756, -12.20198613296999923 ) ) ;
#26988 = ORIENTED_EDGE ( 'NONE', *, *, #46678, .T. ) ;
#26989 = EDGE_LOOP ( 'NONE', ( #6853, #12878, #15004, #14712, #54206, #48450 ) ) ;
#26990 = LINE ( 'NONE', #45025, #19742 ) ;
#26991 = CARTESIAN_POINT ( 'NONE',  ( -12.50000000000000000, -17.31762331506999786, -1.005384022379999909 ) ) ;
#26992 = VECTOR ( 'NONE', #19569, 1000.000000000000000 ) ;
#26993 = CARTESIAN_POINT ( 'NONE',  ( 1.199918086393000127, -80.50782662941900014, 0.5820416783086000967 ) ) ;
#26994 = CARTESIAN_POINT ( 'NONE',  ( -8.592320330817999618, -78.17107902543699538, 4.510292750937000328 ) ) ;
#26995 = CARTESIAN_POINT ( 'NONE',  ( -3.351152128423308785, -86.40321104920796813, 1.568368390946520918 ) ) ;
#26996 = CARTESIAN_POINT ( 'NONE',  ( 3.148955979375664960, -85.83315908744809519, 1.668297098845500592 ) ) ;
#26997 = AXIS2_PLACEMENT_3D ( 'NONE', #7571, #20575, #30278 ) ;
#26998 = CIRCLE ( 'NONE', #23220, 1.000000000000000000 ) ;
#26999 = CARTESIAN_POINT ( 'NONE',  ( 7.317687889309999250, -77.59130236656999102, -10.69177725920999933 ) ) ;
#27000 = CARTESIAN_POINT ( 'NONE',  ( -1.214718215476999985, -80.54393956010999034, 0.5919720313516000365 ) ) ;
#27001 = CARTESIAN_POINT ( 'NONE',  ( 5.039215783544999994, -76.86328604711199830, 9.647628555108001436 ) ) ;
#27002 = CARTESIAN_POINT ( 'NONE',  ( -0.6014246001485028525, -79.18513522466939492, -1.095746199531517862 ) ) ;
#27003 = VECTOR ( 'NONE', #27882, 1000.000000000000000 ) ;
#27004 = DIRECTION ( 'NONE',  ( 0.000000000000000000, -1.000000000000000000, 0.000000000000000000 ) ) ;
#27005 = CARTESIAN_POINT ( 'NONE',  ( -2.970023312147000105, -82.17746358424498965, -2.623918653887999941 ) ) ;
#27006 = CARTESIAN_POINT ( 'NONE',  ( 9.755626371838998168, -81.04222055755619181, -5.633583086437000453 ) ) ;
#27007 = CARTESIAN_POINT ( 'NONE',  ( -10.18589234707000202, -55.51082434643999619, 7.641012386020999969 ) ) ;
#27008 = CARTESIAN_POINT ( 'NONE',  ( 12.00000000000000000, 0.000000000000000000, 0.000000000000000000 ) ) ;
#27009 = CARTESIAN_POINT ( 'NONE',  ( 3.383438395877000016, -82.49282046129098944, 0.3412908512157999952 ) ) ;
#27010 = DIRECTION ( 'NONE',  ( 0.7071067811865474617, 0.7071067811865474617, -7.319351672370483695E-10 ) ) ;
#27011 = CARTESIAN_POINT ( 'NONE',  ( -12.00000000000000000, -23.15000000002000036, -0.7999999999999001243 ) ) ;
#27012 = CARTESIAN_POINT ( 'NONE',  ( 0.000000000000000000, -75.10000000019110189, 0.000000000000000000 ) ) ;
#27013 = CARTESIAN_POINT ( 'NONE',  ( -3.054513261463999818, -2.902870392637999952, -2.270689576097000284 ) ) ;
#27014 = CARTESIAN_POINT ( 'NONE',  ( 0.8977011673350683285, -80.43755243846868552, -0.9055672397132533691 ) ) ;
#27015 = ORIENTED_EDGE ( 'NONE', *, *, #36838, .F. ) ;
#27016 = CARTESIAN_POINT ( 'NONE',  ( -0.5962167095188449784, -23.22841244209519473, 10.98383273456533260 ) ) ;
#27017 = EDGE_CURVE ( 'NONE', #19308, #54154, #29701, .T. ) ;
#27018 = CARTESIAN_POINT ( 'NONE',  ( -11.00000000000000000, -79.19999999999998863, 0.000000000000000000 ) ) ;
#27019 = CARTESIAN_POINT ( 'NONE',  ( 1.193978368322000216, -81.97891765811500875, -0.5941311122250999555 ) ) ;
#27020 = CARTESIAN_POINT ( 'NONE',  ( -12.77651065923999951, -16.69103388611000227, 0.04307580168117999125 ) ) ;
#27021 = CARTESIAN_POINT ( 'NONE',  ( 5.715297388934000189, -78.32148429990999716, 11.69132169264999987 ) ) ;
#27022 = CARTESIAN_POINT ( 'NONE',  ( -7.770369683918966430, -61.03583903303037772, -10.20674856005918940 ) ) ;
#27023 = CARTESIAN_POINT ( 'NONE',  ( 12.71658872085999903, -18.68415268018999953, -1.931087888240000217 ) ) ;
#27024 = EDGE_LOOP ( 'NONE', ( #44058, #32565, #4860, #40946, #30894, #53946 ) ) ;
#27025 = CARTESIAN_POINT ( 'NONE',  ( -9.700000000000001066, -87.70000000000000284, 0.000000000000000000 ) ) ;
#27026 = EDGE_CURVE ( 'NONE', #8613, #17621, #39790, .T. ) ;
#27027 = CARTESIAN_POINT ( 'NONE',  ( 1.496078468352999957, -81.11195581612699357, 0.1750711238899000100 ) ) ;
#27028 = CARTESIAN_POINT ( 'NONE',  ( 3.938458446976999205, -79.30999999999998806, -8.369650235310999165 ) ) ;
#27029 = CARTESIAN_POINT ( 'NONE',  ( 3.187402732789999860, -78.30477596781798866, 8.972783294553000388 ) ) ;
#27031 = CARTESIAN_POINT ( 'NONE',  ( -1.180494763713999973, -0.7191883867189999835, 3.461421590595000097 ) ) ;
#27030 = CARTESIAN_POINT ( 'NONE',  ( 2.260318168362000169, -82.49842648807799605, 3.456791565332999916 ) ) ;
#27032 = CARTESIAN_POINT ( 'NONE',  ( -1.799502287743000029, -55.49283065365000311, -12.60413652829999975 ) ) ;
#27033 = CARTESIAN_POINT ( 'NONE',  ( 0.6554565090088000368, -79.88674016633599706, 1.367230381797000183 ) ) ;
#27034 = EDGE_LOOP ( 'NONE', ( #45024, #53405, #6006, #51945, #11456 ) ) ;
#27035 = CARTESIAN_POINT ( 'NONE',  ( 0.07998295410073143208, -77.22568207807030660, -10.74969477503664628 ) ) ;
#27036 = FACE_OUTER_BOUND ( 'NONE', #33750, .T. ) ;
#27037 = EDGE_LOOP ( 'NONE', ( #56122, #23647, #51456, #21980 ) ) ;
#27038 = ORIENTED_EDGE ( 'NONE', *, *, #12268, .F. ) ;
#27039 = CARTESIAN_POINT ( 'NONE',  ( -0.7406579117306999471, -79.58158555557200486, 12.00660533699000077 ) ) ;
#27040 = B_SPLINE_CURVE_WITH_KNOTS ( 'NONE', 3,
 ( #40073, #4061, #4668, #35940, #53968, #12913, #57795, #4365, #53666, #58089, #31200, #22365, #17351, #44225, #13206, #31497 ),
 .UNSPECIFIED., .F., .F.,
 ( 4, 1, 1, 1, 1, 1, 1, 1, 1, 1, 1, 1, 1, 4 ),
 ( 0.000000000000000000, 0.06727065942882816396, 0.1470435203315429151, 0.2268163812345619923, 0.3065892421372763965, 0.3863621030402955014, 0.4661349639430099057, 0.5459078248460289551, 0.6256806857487438034, 0.7054535466517628528, 0.7852264075544772570, 0.8649992684571919943, 0.9447721293602107107, 1.000000000000000000 ),
 .UNSPECIFIED. ) ;
#27041 = CARTESIAN_POINT ( 'NONE',  ( -9.667451473995011924, -80.46331611536132300, 4.804704892540419436 ) ) ;
#27042 = CONICAL_SURFACE ( 'NONE', #24236, 9.649999999909001147, 0.7853981633972997312 ) ;
#27043 = ORIENTED_EDGE ( 'NONE', *, *, #43151, .T. ) ;
#27044 = CARTESIAN_POINT ( 'NONE',  ( 11.86727826211999925, -77.42727113527298854, -2.088899193827999934 ) ) ;
#27045 = AXIS2_PLACEMENT_3D ( 'NONE', #55962, #6653, #37062 ) ;
#27046 = EDGE_CURVE ( 'NONE', #44555, #47200, #26952, .T. ) ;
#27047 = ORIENTED_EDGE ( 'NONE', *, *, #34546, .T. ) ;
#27048 = ORIENTED_EDGE ( 'NONE', *, *, #31274, .T. ) ;
#27049 = CARTESIAN_POINT ( 'NONE',  ( -3.000189226121413810, -2.632099266311925145, -1.248401069550000297 ) ) ;
#27050 = CARTESIAN_POINT ( 'NONE',  ( -7.374560639699022424, -78.72708333333335418, 9.596002108778135309 ) ) ;
#27051 = CARTESIAN_POINT ( 'NONE',  ( -0.7832439075705196485, -1.738450387085815896, 3.943800212226620694 ) ) ;
#27052 = ORIENTED_EDGE ( 'NONE', *, *, #50958, .T. ) ;
#27053 = CARTESIAN_POINT ( 'NONE',  ( -1.311000177045137827, -81.85844383938299984, 0.7555961656110528057 ) ) ;
#27054 = ORIENTED_EDGE ( 'NONE', *, *, #16360, .T. ) ;
#27055 = CARTESIAN_POINT ( 'NONE',  ( 0.6791567373625641002, -80.48046376981821481, 1.078384872319655186 ) ) ;
#27056 = CARTESIAN_POINT ( 'NONE',  ( -11.79643810520695268, -79.79999999999996874, -2.072837582963935166 ) ) ;
#27057 = EDGE_CURVE ( 'NONE', #33164, #38869, #12923, .T. ) ;
#27058 = DIRECTION ( 'NONE',  ( 0.000000000000000000, 1.000000000000000000, 0.000000000000000000 ) ) ;
#27059 = CARTESIAN_POINT ( 'NONE',  ( 0.5812841321856091481, -18.69583131522389507, 10.98463311464191605 ) ) ;
#27060 = CARTESIAN_POINT ( 'NONE',  ( 11.79999999999999893, -23.15000000000000213, 0.5999999999999999778 ) ) ;
#27061 = LINE ( 'NONE', #50406, #33661 ) ;
#27062 = CARTESIAN_POINT ( 'NONE',  ( 7.641012305205999056, -55.51082276539999327, -10.18589226629999978 ) ) ;
#27063 = CARTESIAN_POINT ( 'NONE',  ( 0.004634250437275883386, -78.72518518586632297, -9.249911725680748376 ) ) ;
#27064 = CARTESIAN_POINT ( 'NONE',  ( -9.788011744275999959, -24.52881292764999799, 7.956359616222000497 ) ) ;
#27065 = CARTESIAN_POINT ( 'NONE',  ( 1.500000000000001110, -80.13958333333334849, -0.1963495408493590721 ) ) ;
#27066 = CARTESIAN_POINT ( 'NONE',  ( -10.71369944335148183, -78.57916666666665151, 2.879226727952040932 ) ) ;
#27067 = CARTESIAN_POINT ( 'NONE',  ( -11.03276040983153550, -77.98620529984978589, -4.895327290354793526 ) ) ;
#27068 = CARTESIAN_POINT ( 'NONE',  ( 0.9277797337941999789, -81.21500264934797997, 4.070482101575999323 ) ) ;
#27069 = CARTESIAN_POINT ( 'NONE',  ( 8.879470778449000790, -77.03466001420198950, -4.315638138276999491 ) ) ;
#27070 = CARTESIAN_POINT ( 'NONE',  ( -12.82229880959000035, -18.57735182838000298, 2.065917129154000165 ) ) ;
#27071 = PLANE ( 'NONE',  #49982 ) ;
#27072 = CARTESIAN_POINT ( 'NONE',  ( 0.4701041210474999898, -25.00796934423999929, 12.54901038416000070 ) ) ;
#27073 = CARTESIAN_POINT ( 'NONE',  ( 10.03798773386740351, -79.88458675554201704, 4.654823617294056248 ) ) ;
#27074 = CARTESIAN_POINT ( 'NONE',  ( 1.078609919318999966, -83.66757477367698925, -3.379520766710000235 ) ) ;
#27075 = CARTESIAN_POINT ( 'NONE',  ( -0.1236500535340000068, -0.6721180847798000624, 3.590573661457999943 ) ) ;
#27076 = EDGE_CURVE ( 'NONE', #25463, #38188, #53091, .T. ) ;
#27077 = CARTESIAN_POINT ( 'NONE',  ( -5.770029083771401446, -78.18019031253406581, -9.108371886169937426 ) ) ;
#27078 = CARTESIAN_POINT ( 'NONE',  ( 1.405334848747999743, -54.48507051966527115, -12.50716844827338825 ) ) ;
#27080 = EDGE_CURVE ( 'NONE', #9151, #33152, #57104, .T. ) ;
#27079 = CARTESIAN_POINT ( 'NONE',  ( 1.349333182780099394, -81.06188137117389658, -0.6856402333970393892 ) ) ;
#27081 = CARTESIAN_POINT ( 'NONE',  ( -0.9976490992766898769, -78.54879995622603417, 0.7538695216397535148 ) ) ;
#27082 = DIRECTION ( 'NONE',  ( 0.000000000000000000, 0.7071067811866525998, -0.7071067811864425456 ) ) ;
#27083 = VECTOR ( 'NONE', #44107, 1000.000000000000114 ) ;
#27084 = FACE_OUTER_BOUND ( 'NONE', #35139, .T. ) ;
#27085 = CARTESIAN_POINT ( 'NONE',  ( -7.595061814885000651, -78.46281986999699143, 7.841581601742999119 ) ) ;
#27086 = CARTESIAN_POINT ( 'NONE',  ( 10.43567240482000003, -78.16758737238698984, 6.472443173969999464 ) ) ;
#27087 = DIRECTION ( 'NONE',  ( 2.678911359553000079E-11, 1.000000000000000000, 2.678924269122999951E-11 ) ) ;
#27088 = CIRCLE ( 'NONE', #44091, 0.6000000000000008660 ) ;
#27090 = CARTESIAN_POINT ( 'NONE',  ( 1.391768007815999963, -78.07021811561179447, -0.6016011292324999760 ) ) ;
#27089 = CARTESIAN_POINT ( 'NONE',  ( -1.823750004803999641E-14, -80.79999999999999716, 0.000000000000000000 ) ) ;
#27091 = CARTESIAN_POINT ( 'NONE',  ( -0.7976765672644999805, -81.85618029491999437, -1.504502914139000058 ) ) ;
#27092 = ORIENTED_EDGE ( 'NONE', *, *, #27920, .F. ) ;
#27093 = CARTESIAN_POINT ( 'NONE',  ( 3.635538803723000090, -84.19396544543099026, -0.9456319026059999411 ) ) ;
#27094 = CARTESIAN_POINT ( 'NONE',  ( 11.65878804082999842, -79.39029486734300178, 2.511675558105000317 ) ) ;
#27095 = CARTESIAN_POINT ( 'NONE',  ( 8.467741319088000651, -79.87580510418969482, 6.550495500029000162 ) ) ;
#27096 = EDGE_CURVE ( 'NONE', #3055, #1033, #19436, .T. ) ;
#27097 = PLANE ( 'NONE',  #13439 ) ;
#27098 = CARTESIAN_POINT ( 'NONE',  ( -3.423353336519171286, -84.67395834349072459, 0.3700115578796988047 ) ) ;
#27099 = CARTESIAN_POINT ( 'NONE',  ( -10.08161778468999970, -61.51855282861000518, 7.981584069293999661 ) ) ;
#27100 = CARTESIAN_POINT ( 'NONE',  ( 5.436864099232999514, -79.00131553099198811, -8.080855302300999909 ) ) ;
#27101 = CARTESIAN_POINT ( 'NONE',  ( 0.7999999999999001243, -23.15000000002000036, -12.00000000000000000 ) ) ;
#27102 = CARTESIAN_POINT ( 'NONE',  ( 8.664753834735311244, -76.49051551431000462, -8.038626423221995054 ) ) ;
#27103 = CARTESIAN_POINT ( 'NONE',  ( 12.83836862999999973, -23.20626272212999908, -2.062146390630000159 ) ) ;
#27104 = CARTESIAN_POINT ( 'NONE',  ( -2.062502994258999856, -57.04351820043999766, 12.92181194098999875 ) ) ;
#27105 = ORIENTED_EDGE ( 'NONE', *, *, #12341, .T. ) ;
#27106 = CARTESIAN_POINT ( 'NONE',  ( -10.42531124908000173, -60.06485148440999922, -7.624341765471999821 ) ) ;
#27107 = CARTESIAN_POINT ( 'NONE',  ( -0.5999999999999999778, -23.15000000000000213, 10.98362417419999915 ) ) ;
#27108 = CARTESIAN_POINT ( 'NONE',  ( 12.76303204513999923, -55.53514852210999919, -1.980584515753000208 ) ) ;
#27109 = CARTESIAN_POINT ( 'NONE',  ( -3.515151790187000191, -83.14892953870898396, 0.4777662710532999957 ) ) ;
#27110 = CARTESIAN_POINT ( 'NONE',  ( -12.49306752636999995, -60.08056692637000396, -1.667917367010000040 ) ) ;
#27111 = DIRECTION ( 'NONE',  ( -3.944178317128000824E-11, 1.000000000000000000, 1.496715873672999954E-09 ) ) ;
#27112 = EDGE_LOOP ( 'NONE', ( #8454, #38890, #5556, #12893, #34311 ) ) ;
#27113 = CARTESIAN_POINT ( 'NONE',  ( -4.464053075535999504, -77.40064930226400008, 10.28489246429000126 ) ) ;
#27114 = CARTESIAN_POINT ( 'NONE',  ( 2.839805762151339952, -1.208333333333333481, -1.636761686205418176 ) ) ;
#27115 = ORIENTED_EDGE ( 'NONE', *, *, #42314, .F. ) ;
#27116 = ORIENTED_EDGE ( 'NONE', *, *, #34513, .F. ) ;
#27117 = CARTESIAN_POINT ( 'NONE',  ( -10.35410226329999794, -55.39601732791000188, -7.619716344056000068 ) ) ;
#27118 = CARTESIAN_POINT ( 'NONE',  ( 6.728605944993000243, -79.51562678850498855, -7.080011783993000130 ) ) ;
#27119 = CONICAL_SURFACE ( 'NONE', #1710, 13.94999999959000014, 0.7853981633972997312 ) ;
#27120 = EDGE_LOOP ( 'NONE', ( #41016, #56520, #54378, #36199 ) ) ;
#27121 = CARTESIAN_POINT ( 'NONE',  ( 12.31302258087999846, -76.43476096588899793, -0.9885975245223000973 ) ) ;
#27122 = CARTESIAN_POINT ( 'NONE',  ( -9.562223587057937735, -78.63793111567514416, -4.911682745217511581 ) ) ;
#27123 = CARTESIAN_POINT ( 'NONE',  ( 1.437308235806999956, -78.98518200747000151, 0.5384467711458000849 ) ) ;
#27124 = ORIENTED_EDGE ( 'NONE', *, *, #14268, .T. ) ;
#27125 = CARTESIAN_POINT ( 'NONE',  ( -4.802567994450000377, -77.21285194988500677, -8.191018798270000900 ) ) ;
#27126 = EDGE_CURVE ( 'NONE', #53713, #10870, #45831, .T. ) ;
#27127 = CIRCLE ( 'NONE', #1718, 1.250000000000000444 ) ;
#27128 = CARTESIAN_POINT ( 'NONE',  ( 1.046031006193842927, -80.30401498017664608, -0.6871684749293296424 ) ) ;
#27129 = CARTESIAN_POINT ( 'NONE',  ( -1.258617752331000039, -77.69871687587999531, -12.89490358089000033 ) ) ;
#27130 = CARTESIAN_POINT ( 'NONE',  ( -4.531904799950999596, -77.34190302449002274, -10.26060180864999971 ) ) ;
#27131 = CARTESIAN_POINT ( 'NONE',  ( -0.5188809666114609920, -86.39318692614398287, 4.172962832911258246 ) ) ;
#27132 = CARTESIAN_POINT ( 'NONE',  ( -5.351292223237999579, -77.67148113580876156, 8.095330809056001442 ) ) ;
#27133 = CARTESIAN_POINT ( 'NONE',  ( 8.528027178079026882, -79.88239481433151923, 3.637236233294601995 ) ) ;
#27134 = FACE_OUTER_BOUND ( 'NONE', #56480, .T. ) ;
#27135 = ORIENTED_EDGE ( 'NONE', *, *, #3920, .F. ) ;
#27136 = CARTESIAN_POINT ( 'NONE',  ( 9.500000000000000000, -77.54999999999999716, 0.000000000000000000 ) ) ;
#27137 = CARTESIAN_POINT ( 'NONE',  ( 11.50190934395000042, -76.77899180865000517, -3.421415122956000143 ) ) ;
#27138 = CARTESIAN_POINT ( 'NONE',  ( -1.158153954042000056, -80.34670878855399678, 1.125119257983999921 ) ) ;
#27139 = CARTESIAN_POINT ( 'NONE',  ( 0.7248607164131247727, -3.490744342946634937, -3.444725236542351521 ) ) ;
#27140 = CARTESIAN_POINT ( 'NONE',  ( 12.83044039274999903, -18.69360374348000065, 2.062670899148999926 ) ) ;
#27141 = DIRECTION ( 'NONE',  ( 0.000000000000000000, 1.000000000000000000, 0.000000000000000000 ) ) ;
#27142 = CARTESIAN_POINT ( 'NONE',  ( -12.00000000000000000, -78.39999999999999147, 0.000000000000000000 ) ) ;
#27143 = CARTESIAN_POINT ( 'NONE',  ( 9.370759595542999421, -77.15123998579800002, 2.646005887749999896 ) ) ;
#27144 = DIRECTION ( 'NONE',  ( -0.7071067811865475727, 0.000000000000000000, -0.7071067811865475727 ) ) ;
#27145 = LINE ( 'NONE', #8567, #43626 ) ;
#27146 = B_SPLINE_SURFACE_WITH_KNOTS ( 'NONE', 3, 3, ( 
 ( #9996, #40400, #293, #31519, #17972, #40992, #4689, #583, #22687, #40699, #18271, #54286, #5266, #14118, #864, #50155, #9698, #23275, #41280, #47581, #7107, #38395, #24823, #43706, #34525, #57272, #2398, #16545, #25393, #30389, #21543, #3262, #21253, #39549, #39258 ),
 ( #16835, #47861, #52846, #20684, #20398, #57554, #11548, #17115, #35101, #48426, #11828, #53134, #56414, #43989, #51993, #33956, #38971, #25107, #25965, #34818, #12683, #15964, #29525, #52560, #42840, #48148, #29808, #20967, #43133, #3542, #2691, #7390, #7967, #12399, #38683 ),
 ( #56703, #16260, #56983, #43409, #52274, #2967, #34239, #12112, #30675, #30097, #7678, #25679, #48712, #36583, #8545, #54314, #31252, #44271, #27129, #9144, #41020, #36292, #23009, #30960, #49294, #21828, #18593, #4417, #54605, #54017, #17403, #53723, #35387, #13854, #3828 ),
 ( #26836, #53416, #31550, #4118, #31850, #17709, #13261, #612, #45167, #35992, #8845, #44864, #22419, #40431, #13558, #14142, #4717, #32142, #49892, #8258, #48998, #22, #39833, #26257, #18002, #57846, #49597, #12963, #22716, #26537, #9436, #44564, #40729, #22119, #27427 ) ),
 .UNSPECIFIED., .F., .F., .F.,
 ( 4, 4 ),
 ( 4, 1, 1, 1, 1, 1, 1, 1, 1, 1, 1, 1, 1, 1, 1, 1, 1, 1, 1, 1, 1, 1, 1, 1, 1, 1, 1, 1, 1, 1, 1, 1, 4 ),
 ( -0.3708084972814000291, 1.370808497280999960 ),
 ( -0.02000000000000000042, 0.01250000000000000069, 0.04499999999999999833, 0.07749999999999999944, 0.1100000000000000006, 0.1424999999999999878, 0.1749999999999999889, 0.2074999999999999900, 0.2399999999999999911, 0.2725000000000000200, 0.3049999999999999933, 0.3375000000000000222, 0.3699999999999999956, 0.4025000000000000244, 0.4349999999999999978, 0.4675000000000000266, 0.5000000000000000000, 0.5324999999999999734, 0.5649999999999999467, 0.5975000000000000311, 0.6300000000000000044, 0.6624999999999999778, 0.6949999999999999512, 0.7275000000000000355, 0.7600000000000000089, 0.7924999999999999822, 0.8249999999999999556, 0.8575000000000000400, 0.8900000000000000133, 0.9224999999999999867, 0.9549999999999999600, 0.9875000000000000444, 1.020000000000000018 ),
 .UNSPECIFIED. ) ;
#27147 = ORIENTED_EDGE ( 'NONE', *, *, #24826, .T. ) ;
#27149 = EDGE_CURVE ( 'NONE', #37361, #2615, #3413, .T. ) ;
#27148 = CARTESIAN_POINT ( 'NONE',  ( 0.5770204343780001022, -82.54797985337199862, -1.476971271490000071 ) ) ;
#27150 = FACE_OUTER_BOUND ( 'NONE', #4514, .T. ) ;
#27151 = CARTESIAN_POINT ( 'NONE',  ( -1.500000000000000000, -80.51769483858633691, -0.3335398494528040159 ) ) ;
#27152 = CARTESIAN_POINT ( 'NONE',  ( -7.167604382870000457, -77.42435704553099640, 9.599037027053000770 ) ) ;
#27153 = CARTESIAN_POINT ( 'NONE',  ( 5.778006553106726173, -77.00000000000000000, 7.287267006099804156 ) ) ;
#27154 = CARTESIAN_POINT ( 'NONE',  ( -0.6572886123566999972, -82.67766689626199650, 1.530761476772000140 ) ) ;
#27155 = CARTESIAN_POINT ( 'NONE',  ( 11.49150497439000063, -78.80483761240600415, -3.221926464390000078 ) ) ;
#27156 = CARTESIAN_POINT ( 'NONE',  ( 9.377128579935000374, -78.23854415034598730, -2.571625947824999869 ) ) ;
#27157 = CARTESIAN_POINT ( 'NONE',  ( -8.968424590936999508, -77.11923613374659681, 2.773906523901999766 ) ) ;
#27158 = AXIS2_PLACEMENT_3D ( 'NONE', #24343, #48443, #12978 ) ;
#27159 = CARTESIAN_POINT ( 'NONE',  ( 1.641871293650414065, -76.06380281422384826, 11.64119219785805193 ) ) ;
#27160 = CARTESIAN_POINT ( 'NONE',  ( -6.220196401501000061, -79.03619441778099031, -9.111031286755999048 ) ) ;
#27161 = CARTESIAN_POINT ( 'NONE',  ( 12.50000000000000000, -60.04999999657000131, 1.750000000000000000 ) ) ;
#27162 = VERTEX_POINT ( 'NONE', #25925 ) ;
#27163 = CARTESIAN_POINT ( 'NONE',  ( 3.007117222848000093, -75.90536276733411114, 11.93703523519999443 ) ) ;
#27164 = CARTESIAN_POINT ( 'NONE',  ( -3.699342691684420537, -78.39678895079168797, 0.06973985258851372881 ) ) ;
#27165 = EDGE_CURVE ( 'NONE', #49174, #27720, #7638, .T. ) ;
#27166 = CARTESIAN_POINT ( 'NONE',  ( -5.413904038987206846, -77.41666666666665719, 9.393203674808249914 ) ) ;
#27167 = CARTESIAN_POINT ( 'NONE',  ( 7.318097147681000614, -79.61323130376099755, -8.179820946710000484 ) ) ;
#27168 = EDGE_CURVE ( 'NONE', #56093, #52467, #52429, .T. ) ;
#27169 = CARTESIAN_POINT ( 'NONE',  ( -1.061497411238000010, -76.49164580791499191, -12.45902078201000052 ) ) ;
#27170 = CARTESIAN_POINT ( 'NONE',  ( 1.249029712508835432, -79.33891269701508975, -0.1789285167953770239 ) ) ;
#27171 = CARTESIAN_POINT ( 'NONE',  ( 10.53044221640268674, -76.76847933843360750, 2.496041332906649757 ) ) ;
#27172 = ORIENTED_EDGE ( 'NONE', *, *, #28163, .F. ) ;
#27173 = CARTESIAN_POINT ( 'NONE',  ( -10.27879708628000088, -78.67724904577400480, 4.312879667924000238 ) ) ;
#27174 = CARTESIAN_POINT ( 'NONE',  ( 12.70457850616319284, -53.62128713286528381, 0.5106122238224051202 ) ) ;
#27175 = CARTESIAN_POINT ( 'NONE',  ( -8.796335266379978535, -77.65208333333332291, -6.760013919724068288 ) ) ;
#27176 = CARTESIAN_POINT ( 'NONE',  ( -3.819913395574868531, -78.40681307243320930, 2.158384873251588232 ) ) ;
#27177 = CARTESIAN_POINT ( 'NONE',  ( -1.250000000000000000, -81.59999999999999432, 0.000000000000000000 ) ) ;
#27178 = CARTESIAN_POINT ( 'NONE',  ( -6.511242784100999437, -78.66764840355199340, 9.060646613982999753 ) ) ;
#27179 = B_SPLINE_CURVE_WITH_KNOTS ( 'NONE', 3,
 ( #2476, #25185, #56493, #29316, #51788, #24902, #52638, #55918, #52358, #6896, #34031, #16048, #38476, #34321, #7185, #56206, #11909, #12194 ),
 .UNSPECIFIED., .F., .F.,
 ( 4, 2, 2, 2, 2, 2, 2, 2, 4 ),
 ( 0.000000000000000000, 0.1250000000000000833, 0.2500000000000001110, 0.3750000000000001110, 0.5000000000000001110, 0.6250000000000002220, 0.7500000000000001110, 0.8750000000000001110, 1.000000000000000000 ),
 .UNSPECIFIED. ) ;
#27180 = DIRECTION ( 'NONE',  ( 0.000000000000000000, -1.000000000000000000, 0.000000000000000000 ) ) ;
#27181 = CARTESIAN_POINT ( 'NONE',  ( 1.519477976411357734, -81.58817474069346076, -0.2151540744559326535 ) ) ;
#27182 = ADVANCED_FACE ( 'NONE', ( #26216 ), #32632, .F. ) ;
#27183 = CARTESIAN_POINT ( 'NONE',  ( 8.596418555780418913, -79.30208333333332860, 6.606377239730356621 ) ) ;
#27184 = DIRECTION ( 'NONE',  ( -0.7071067811865475727, 0.000000000000000000, -0.7071067811865475727 ) ) ;
#27185 = CARTESIAN_POINT ( 'NONE',  ( 9.596002108778145967, -77.10208333333332575, 7.374560639699001996 ) ) ;
#27186 = ORIENTED_EDGE ( 'NONE', *, *, #12994, .T. ) ;
#27187 = ORIENTED_EDGE ( 'NONE', *, *, #17867, .T. ) ;
#27188 = CARTESIAN_POINT ( 'NONE',  ( -9.252740428349001789, -78.42083333333334849, -2.486604901413163926 ) ) ;
#27189 = CARTESIAN_POINT ( 'NONE',  ( 8.681495883089000998, -76.90711332859899585, -4.219417537955999720 ) ) ;
#27190 = EDGE_LOOP ( 'NONE', ( #10401, #17613, #45651, #58060 ) ) ;
#27191 = CARTESIAN_POINT ( 'NONE',  ( -10.99972769911000015, -76.23554795518754190, 2.019869862886000345 ) ) ;
#27192 = ORIENTED_EDGE ( 'NONE', *, *, #42497, .T. ) ;
#27193 = LINE ( 'NONE', #31033, #42461 ) ;
#27194 = EDGE_CURVE ( 'NONE', #42621, #22170, #6227, .T. ) ;
#27195 = CARTESIAN_POINT ( 'NONE',  ( -10.37098203719999923, -77.66882059614400191, -3.760912916518000415 ) ) ;
#27196 = VECTOR ( 'NONE', #56012, 1000.000000000000000 ) ;
#27197 = EDGE_CURVE ( 'NONE', #30305, #26900, #53676, .T. ) ;
#27198 = DIRECTION ( 'NONE',  ( -1.000000000000000000, 0.000000000000000000, 0.000000000000000000 ) ) ;
#27199 = CARTESIAN_POINT ( 'NONE',  ( -3.327183877592000183, -78.53223998579800025, 9.097860994781999722 ) ) ;
#27200 = CARTESIAN_POINT ( 'NONE',  ( -4.418675353760038504, -78.18548855279971121, -8.128508495965080627 ) ) ;
#27201 = CARTESIAN_POINT ( 'NONE',  ( 7.808618912244999599, -78.95238198094399706, -8.052551227705000869 ) ) ;
#27202 = CARTESIAN_POINT ( 'NONE',  ( 0.1719510004633373057, -81.00000000000000000, 10.80697498056500727 ) ) ;
#27203 = VERTEX_POINT ( 'NONE', #9982 ) ;
#27204 = CARTESIAN_POINT ( 'NONE',  ( 0.000000000000000000, -74.64999999999999147, 0.000000000000000000 ) ) ;
#27205 = VERTEX_POINT ( 'NONE', #9396 ) ;
#27206 = CARTESIAN_POINT ( 'NONE',  ( 1.445980050911830794, -77.46252241678527639, 9.136273426141869436 ) ) ;
#27207 = CARTESIAN_POINT ( 'NONE',  ( -7.062685404271999978, -77.86038984814099706, 8.485436034813998774 ) ) ;
#27208 = CARTESIAN_POINT ( 'NONE',  ( 11.00000000000000000, -76.04999999999999716, -1.235097113410999977E-09 ) ) ;
#27209 = CARTESIAN_POINT ( 'NONE',  ( -8.771427373352999268, -77.92563036551399591, -4.151237309591000013 ) ) ;
#27210 = CARTESIAN_POINT ( 'NONE',  ( 6.368865985159000154, -76.34029810977999375, 11.47429970984000036 ) ) ;
#27211 = CIRCLE ( 'NONE', #22507, 30.49999999999999289 ) ;
#27212 = CARTESIAN_POINT ( 'NONE',  ( -9.376751323929733317, -79.41245819630034930, -1.524018823012485813 ) ) ;
#27213 = CARTESIAN_POINT ( 'NONE',  ( -0.7004323366084000968, -78.30077033992999702, -1.469032877812000093 ) ) ;
#27214 = DIRECTION ( 'NONE',  ( -1.000000000000000000, 0.000000000000000000, 0.000000000000000000 ) ) ;
#27215 = CARTESIAN_POINT ( 'NONE',  ( -9.781527233834999890, -78.96614208009899016, -4.899953194656999855 ) ) ;
#27216 = CARTESIAN_POINT ( 'NONE',  ( 0.7681833999686451531, -78.17708333333332860, -0.9995835529977240563 ) ) ;
#27217 = CARTESIAN_POINT ( 'NONE',  ( -11.52225979636347653, -76.68411619956043523, 2.301538105231448306 ) ) ;
#27218 = CARTESIAN_POINT ( 'NONE',  ( 2.586461584802999703, -84.07325862280099216, 2.423878626333000330 ) ) ;
#27219 = ORIENTED_EDGE ( 'NONE', *, *, #6279, .F. ) ;
#27220 = B_SPLINE_CURVE_WITH_KNOTS ( 'NONE', 3,
 ( #22301, #49776, #40317, #1938, #55647, #15495, #54772, #50357, #50940, #781, #24054, #33485, #19930, #36753, #33187, #37044, #23761, #24357 ),
 .UNSPECIFIED., .F., .F.,
 ( 4, 2, 2, 2, 2, 2, 2, 2, 4 ),
 ( 0.000000000000000000, 0.1250000000000000000, 0.2500000000000000000, 0.3750000000000000000, 0.5000000000000000000, 0.6250000000000000000, 0.7500000000000000000, 0.8750000000000000000, 1.000000000000000000 ),
 .UNSPECIFIED. ) ;
#27221 = CARTESIAN_POINT ( 'NONE',  ( 4.777753054944000155, -79.09783651582300479, -11.35249243745999870 ) ) ;
#27222 = CARTESIAN_POINT ( 'NONE',  ( -11.23528222893999917, -76.07829378204800719, -0.6904789760584999492 ) ) ;
#27223 = CARTESIAN_POINT ( 'NONE',  ( -4.891664181267372236, -78.01261750250401406, 9.574615555345795670 ) ) ;
#27224 = CARTESIAN_POINT ( 'NONE',  ( -7.167604382869000368, -77.62772270536000008, 9.599037027053000770 ) ) ;
#27225 = CARTESIAN_POINT ( 'NONE',  ( -12.70305380117054916, -61.83154493736395096, 0.8725910144712079042 ) ) ;
#27227 = CARTESIAN_POINT ( 'NONE',  ( -10.40634239505360092, -79.07933785801452586, 2.787274298367601766 ) ) ;
#27226 = CARTESIAN_POINT ( 'NONE',  ( -11.75000000000000355, -78.31041666666666856, -1.538071403320004249 ) ) ;
#27228 = DIRECTION ( 'NONE',  ( -1.000000000000000000, 0.000000000000000000, 0.000000000000000000 ) ) ;
#27229 = CARTESIAN_POINT ( 'NONE',  ( 1.614104026830686323, -80.96338606111143577, 10.62792533169992737 ) ) ;
#27230 = CARTESIAN_POINT ( 'NONE',  ( 10.53003223724999948, -60.12452529330000317, -7.612971414731999786 ) ) ;
#27231 = CARTESIAN_POINT ( 'NONE',  ( 12.00000000000000000, -79.54999999999999716, 0.000000000000000000 ) ) ;
#27232 = CARTESIAN_POINT ( 'NONE',  ( -7.755223252044999960, -78.32736574117099337, 8.006941543446998821 ) ) ;
#27233 = DIRECTION ( 'NONE',  ( 0.000000000000000000, -1.000000000000000000, 0.000000000000000000 ) ) ;
#27234 = CARTESIAN_POINT ( 'NONE',  ( 7.447355024223999642, -80.57439977265350706, -8.285777444469999864 ) ) ;
#27235 = ORIENTED_EDGE ( 'NONE', *, *, #29485, .F. ) ;
#27236 = CARTESIAN_POINT ( 'NONE',  ( -2.015551294784000191, -54.99652295122999845, 12.79857978891999970 ) ) ;
#27237 = CARTESIAN_POINT ( 'NONE',  ( -7.591316436381998933, -77.20127403538302246, -5.703451837412999659 ) ) ;
#27238 = CARTESIAN_POINT ( 'NONE',  ( 1.960212941618999949, -2.639484372332999929, 3.447996340602999865 ) ) ;
#27239 = CARTESIAN_POINT ( 'NONE',  ( 12.48375848564000101, -23.37270426058999817, -1.669543623995999981 ) ) ;
#27240 = CARTESIAN_POINT ( 'NONE',  ( 3.895497176768000003, -77.04509272339099368, 10.51870773133999926 ) ) ;
#27241 = CARTESIAN_POINT ( 'NONE',  ( 1.500000000000001110, -79.63137852148993545, -0.3510066005171248449 ) ) ;
#27242 = CARTESIAN_POINT ( 'NONE',  ( -1.636761686205420396, -1.583333333333333481, -2.839805762151339508 ) ) ;
#27243 = CARTESIAN_POINT ( 'NONE',  ( -10.07627163191000008, -18.75000000310999937, -7.601397897754999633 ) ) ;
#27244 = CARTESIAN_POINT ( 'NONE',  ( 1.418935787216653033, -78.63551514851324953, -10.68838327614559347 ) ) ;
#27245 = DIRECTION ( 'NONE',  ( 0.000000000000000000, 1.000000000000000000, 0.000000000000000000 ) ) ;
#27246 = CARTESIAN_POINT ( 'NONE',  ( 3.031356706570000448, -83.82549735065198604, -2.870622980746000419 ) ) ;
#27247 = CIRCLE ( 'NONE', #30054, 3.000000000000000000 ) ;
#27248 = CARTESIAN_POINT ( 'NONE',  ( 5.209924070321410916, -77.41110552564472869, -10.71737987758433697 ) ) ;
#27249 = CARTESIAN_POINT ( 'NONE',  ( 9.516265623847999677, -53.97460635707999899, -8.227505979398999969 ) ) ;
#27250 = CARTESIAN_POINT ( 'NONE',  ( 0.5439554104848000060, -76.83774834149699018, -11.13367472273999859 ) ) ;
#27251 = CARTESIAN_POINT ( 'NONE',  ( -0.9131908197385000259, -81.28562918685999250, -1.254418330386999791 ) ) ;
#27252 = CARTESIAN_POINT ( 'NONE',  ( -0.9160157088357999688, -77.75144095521999077, 1.388507278780999998 ) ) ;
#27253 = CARTESIAN_POINT ( 'NONE',  ( 0.000000000000000000, 0.000000000000000000, 0.000000000000000000 ) ) ;
#27254 = CARTESIAN_POINT ( 'NONE',  ( -0.3124162970411396567, -82.35929312023905879, -1.516261523662276511 ) ) ;
#27255 = CIRCLE ( 'NONE', #16904, 14.00000000000000000 ) ;
#27256 = CARTESIAN_POINT ( 'NONE',  ( -3.165411199172024848, -2.520833333333333037, -0.8506806241676611036 ) ) ;
#27257 = CARTESIAN_POINT ( 'NONE',  ( -6.446809110249994923, -80.17411999622585483, -8.621120003473629723 ) ) ;
#27258 = CARTESIAN_POINT ( 'NONE',  ( 12.56594317984999876, -18.75000000536999778, -1.750000000000000000 ) ) ;
#27259 = CARTESIAN_POINT ( 'NONE',  ( 1.272221273747917714, -77.90442370964647978, 0.06754771032932266328 ) ) ;
#27260 = AXIS2_PLACEMENT_3D ( 'NONE', #3766, #22353, #58079 ) ;
#27261 = EDGE_CURVE ( 'NONE', #21583, #27787, #41270, .T. ) ;
#27262 = ORIENTED_EDGE ( 'NONE', *, *, #53342, .F. ) ;
#27263 = CARTESIAN_POINT ( 'NONE',  ( 0.9259190077282706266, -81.79188721789226690, -0.8394937396800135065 ) ) ;
#27264 = EDGE_CURVE ( 'NONE', #2615, #36484, #11930, .T. ) ;
#27265 = CARTESIAN_POINT ( 'NONE',  ( -10.71369944335148006, -79.57916666666666572, 2.879226727952048037 ) ) ;
#27266 = CARTESIAN_POINT ( 'NONE',  ( -10.38493632045999959, -78.79179491694800674, 4.357414620914999759 ) ) ;
#27267 = B_SPLINE_CURVE_WITH_KNOTS ( 'NONE', 3,
 ( #27258, #36417, #26098, #40857, #49430, #9272 ),
 .UNSPECIFIED., .F., .F.,
 ( 4, 1, 1, 4 ),
 ( 0.000000000000000000, 0.3333333333333000081, 0.6666666666667000474, 1.000000000000000000 ),
 .UNSPECIFIED. ) ;
#27268 = CARTESIAN_POINT ( 'NONE',  ( 1.250000000000000000, -80.25000000000000000, 0.000000000000000000 ) ) ;
#27269 = ORIENTED_EDGE ( 'NONE', *, *, #23023, .F. ) ;
#27270 = ORIENTED_EDGE ( 'NONE', *, *, #57438, .F. ) ;
#27271 = CARTESIAN_POINT ( 'NONE',  ( -0.8558294506340999863, -80.91139712605799161, 1.369222347861999811 ) ) ;
#27272 = ORIENTED_EDGE ( 'NONE', *, *, #57608, .T. ) ;
#27273 = CYLINDRICAL_SURFACE ( 'NONE', #39609, 12.50000000000000000 ) ;
#27274 = ORIENTED_EDGE ( 'NONE', *, *, #54253, .F. ) ;
#27275 = CARTESIAN_POINT ( 'NONE',  ( 0.000000000000000000, -5.000000000000000000, 0.000000000000000000 ) ) ;
#27276 = CARTESIAN_POINT ( 'NONE',  ( 10.52776997023000050, -80.12876079193905809, 3.979665013433000720 ) ) ;
#27277 = DIRECTION ( 'NONE',  ( 5.381131437589000085E-11, -1.000000000000000000, -8.802795847113000035E-11 ) ) ;
#27278 = ADVANCED_FACE ( 'NONE', ( #854 ), #20394, .F. ) ;
#27279 = CARTESIAN_POINT ( 'NONE',  ( -0.5045596072229999729, -25.13528913037999857, -12.66210649709999991 ) ) ;
#27280 = CARTESIAN_POINT ( 'NONE',  ( -3.606241821240999901, -81.93696273528199470, 1.051851009248000013 ) ) ;
#27281 = CARTESIAN_POINT ( 'NONE',  ( 1.160587285869999707, -77.71661964162117897, 10.97894289003999901 ) ) ;
#27282 = CARTESIAN_POINT ( 'NONE',  ( -5.780852911904999836, -78.65969526808000012, 10.41696410405000073 ) ) ;
#27283 = EDGE_LOOP ( 'NONE', ( #9004, #31616, #999, #5009, #8831 ) ) ;
#27284 = VERTEX_POINT ( 'NONE', #35950 ) ;
#27285 = CARTESIAN_POINT ( 'NONE',  ( -2.858407197967999913, -79.75000000000000000, -8.797272775729998884 ) ) ;
#27286 = CARTESIAN_POINT ( 'NONE',  ( -12.50412681322478292, -17.48010473091721195, -1.235016000439554062 ) ) ;
#27287 = CARTESIAN_POINT ( 'NONE',  ( -1.308081345731999967, -80.70627712294299272, 0.2599445073669000017 ) ) ;
#27288 = CARTESIAN_POINT ( 'NONE',  ( 5.417083560473000325, -78.88167475366098813, -8.051455326762999576 ) ) ;
#27289 = AXIS2_PLACEMENT_3D ( 'NONE', #23832, #33560, #32672 ) ;
#27290 = CARTESIAN_POINT ( 'NONE',  ( -1.645868681893847718, -86.25171438276198899, -3.604857562864015375 ) ) ;
#27291 = CARTESIAN_POINT ( 'NONE',  ( -2.687989892693834815, -86.04954200792612085, 2.984330770045349635 ) ) ;
#27292 = CARTESIAN_POINT ( 'NONE',  ( 12.47598273373999866, -77.64680700753000053, -3.494640443823999743 ) ) ;
#27293 = CARTESIAN_POINT ( 'NONE',  ( -1.223477145616999939, -79.59670880711999530, 0.8121269926547999285 ) ) ;
#27294 = EDGE_CURVE ( 'NONE', #26886, #47367, #13807, .T. ) ;
#27295 = CARTESIAN_POINT ( 'NONE',  ( -4.721011358650000211, -76.36916596888400477, 9.934480763307000473 ) ) ;
#27296 = CARTESIAN_POINT ( 'NONE',  ( 12.76303204294000082, -18.73514849292999784, 1.980584515756000030 ) ) ;
#27297 = B_SPLINE_CURVE_WITH_KNOTS ( 'NONE', 3,
 ( #16984, #58300, #9293, #36151, #8120, #49455, #35252, #21977, #22574, #35850, #40586, #39699, #9001, #26986, #44724, #8702, #17861, #53578, #27281, #26120, #17558, #39988, #26692, #4277, #13116, #54168, #53880, #30829, #22866, #44141, #3689, #21691 ),
 .UNSPECIFIED., .F., .F.,
 ( 4, 1, 1, 1, 1, 1, 1, 1, 1, 1, 1, 1, 1, 1, 1, 1, 1, 1, 1, 1, 1, 1, 1, 1, 1, 1, 1, 1, 1, 4 ),
 ( 0.000000000000000000, 0.008721705557737447975, 0.04492002831815160996, 0.08111835107876277928, 0.1173166738391771546, 0.1535149965995915300, 0.1897133193600056833, 0.2259116421206168734, 0.2621099648810312210, 0.2983082876414456241, 0.3345066104018599717, 0.3707049331624711619, 0.4069032559228853430, 0.4431015786832996906, 0.4792999014439106586, 0.5154982242043252283, 0.5516965469647395759, 0.5878948697251540345, 0.6240931924857650026, 0.6602915152461791282, 0.6964898380065934758, 0.7326881607672046659, 0.7688864835276190135, 0.8050848062880334721, 0.8412831290484478197, 0.8774814518090590099, 0.9136797745694731354, 0.9498780973298874830, 0.9860764200904986732, 1.000000000000000000 ),
 .UNSPECIFIED. ) ;
#27298 = CARTESIAN_POINT ( 'NONE',  ( 4.118565555109999998, -80.96724209361498481, -0.6833944332293000468 ) ) ;
#27300 = AXIS2_PLACEMENT_3D ( 'NONE', #51689, #42527, #29215 ) ;
#27299 = CARTESIAN_POINT ( 'NONE',  ( -2.612980907336999614, -80.30468973093108787, -10.95817168551000087 ) ) ;
#27301 = B_SPLINE_CURVE_WITH_KNOTS ( 'NONE', 3,
 ( #36402, #10139, #5124, #4537, #4830, #22829, #40549, #8964, #18991, #18410, #23120, #28114, #46165, #5690, #23700, #1289, #19282, #37272, #14836, #32832, #50005, #26949, #15432, #20447, #20161, #38150, #15131, #19568, #24582, #55882, #19867, #51463, #10423, #37861, #6862, #33426, #15720, #23991, #51753, #20734, #42306, #34003, #38443, #33129, #28703, #28408, #25153, #29284, #29572, #2734, #2160, #47628, #38731, #24870, #43179, #56461, #1873, #56172, #56750, #46755, #7151, #16310, #11596, #47333, #6273, #47041, #16014, #11018, #50877, #29002, #24290, #37568, #52039, #6571, #42598, #46455, #42888, #5983, #33718, #10725, #42006, #11303, #2445, #1574, #55583, #51171, #43463 ),
 .UNSPECIFIED., .F., .F.,
 ( 4, 2, 2, 2, 2, 2, 1, 2, 2, 2, 2, 2, 2, 2, 2, 2, 2, 2, 2, 2, 2, 2, 1, 2, 2, 2, 2, 2, 2, 2, 2, 2, 2, 2, 2, 2, 2, 2, 1, 2, 2, 2, 2, 2, 4 ),
 ( 0.000000000000000000, 0.01562500000000004510, 0.03125000000000009021, 0.04687500000000014572, 0.06250000000000019429, 0.07812500000000024980, 0.09375000000000030531, 0.1093750000000003608, 0.1250000000000004163, 0.1406250000000004718, 0.1562500000000004996, 0.1718750000000005551, 0.1875000000000006106, 0.2187500000000006384, 0.2500000000000006661, 0.2812500000000007216, 0.3125000000000007216, 0.3437500000000007216, 0.3750000000000006661, 0.4062500000000007216, 0.4375000000000007772, 0.4687500000000007216, 0.5000000000000006661, 0.5312500000000007772, 0.5625000000000007772, 0.5937500000000006661, 0.6250000000000006661, 0.6562500000000006661, 0.6875000000000006661, 0.7187500000000006661, 0.7500000000000005551, 0.7812500000000005551, 0.8125000000000005551, 0.8281250000000005551, 0.8437500000000004441, 0.8593750000000003331, 0.8750000000000003331, 0.8906250000000002220, 0.9062500000000002220, 0.9218750000000002220, 0.9375000000000002220, 0.9531250000000002220, 0.9687500000000001110, 0.9843750000000001110, 1.000000000000000000 ),
 .UNSPECIFIED. ) ;
#27302 = CARTESIAN_POINT ( 'NONE',  ( -10.01234990230000044, -60.09849137196000157, 7.653559502293999728 ) ) ;
#27303 = CARTESIAN_POINT ( 'NONE',  ( -10.11087014619704760, -76.74276732863665984, -6.123559706077069009 ) ) ;
#27304 = CARTESIAN_POINT ( 'NONE',  ( -1.281696068931000188, -79.00557046129088690, -3.307832847245999464 ) ) ;
#27305 = VECTOR ( 'NONE', #7747, 1000.000000000000114 ) ;
#27307 = CARTESIAN_POINT ( 'NONE',  ( 0.2725326480772000126, -79.08050961830200265, 1.305490477442999842 ) ) ;
#27306 = CARTESIAN_POINT ( 'NONE',  ( 4.100000000000000533, -77.49999999999998579, 0.000000000000000000 ) ) ;
#27308 = DIRECTION ( 'NONE',  ( -1.000000000000000000, 0.000000000000000000, 0.000000000000000000 ) ) ;
#27309 = CARTESIAN_POINT ( 'NONE',  ( 1.618170588614999961, -80.53815307676340751, -11.14857479085000058 ) ) ;
#27310 = CARTESIAN_POINT ( 'NONE',  ( 3.665025684363000025, -3.580287900391999845, -1.025097465345000236 ) ) ;
#27311 = CARTESIAN_POINT ( 'NONE',  ( 9.535425472282794246, -77.20000000000000284, -5.121398017412860604 ) ) ;
#27312 = ORIENTED_EDGE ( 'NONE', *, *, #10114, .T. ) ;
#27313 = CARTESIAN_POINT ( 'NONE',  ( -10.47020627418439354, -80.02083333333330017, -2.813789756862258518 ) ) ;
#27314 = CARTESIAN_POINT ( 'NONE',  ( 10.32296845096999860, -78.33546437446798905, -4.912869655601999952 ) ) ;
#27315 = CARTESIAN_POINT ( 'NONE',  ( -8.796335266379976758, -79.25208333333334565, -6.760013919724066511 ) ) ;
#27316 = DIRECTION ( 'NONE',  ( 0.7071067811865475727, 0.000000000000000000, -0.7071067811865475727 ) ) ;
#27317 = CARTESIAN_POINT ( 'NONE',  ( 1.799502287743000029, -55.49283065365000311, 12.60413652829999975 ) ) ;
#27318 = CARTESIAN_POINT ( 'NONE',  ( -10.64207148833999916, -76.93386827587001164, 7.489034475093999887 ) ) ;
#27319 = CARTESIAN_POINT ( 'NONE',  ( -9.211339595762906285, -79.55700502563119869, 5.542666473294825202 ) ) ;
#27320 = CARTESIAN_POINT ( 'NONE',  ( -6.100417943526999842, -79.57728667140099788, -7.450071050714999643 ) ) ;
#27321 = CARTESIAN_POINT ( 'NONE',  ( 4.447441989892999992, -76.14829627867000283, -11.69528159757000019 ) ) ;
#27322 = VERTEX_POINT ( 'NONE', #18838 ) ;
#27323 = DIRECTION ( 'NONE',  ( 0.000000000000000000, -1.000000000000000000, 0.000000000000000000 ) ) ;
#27324 = DIRECTION ( 'NONE',  ( 0.000000000000000000, -1.000000000000000000, -3.788556036780999566E-11 ) ) ;
#27325 = CARTESIAN_POINT ( 'NONE',  ( 1.407325970645999957, -82.04410394639400295, -0.05680320185105999786 ) ) ;
#27326 = DIRECTION ( 'NONE',  ( -1.000000000000000000, 0.000000000000000000, 0.000000000000000000 ) ) ;
#27327 = CARTESIAN_POINT ( 'NONE',  ( -5.574784109570000368, -78.53216660084999035, -7.719595738358999704 ) ) ;
#27329 = CARTESIAN_POINT ( 'NONE',  ( 4.010845454633999552, -1.528571010530000107, -0.2065758488482999922 ) ) ;
#27328 = CARTESIAN_POINT ( 'NONE',  ( 4.129966972622000299, -85.26418603921399608, 0.04343303146570000328 ) ) ;
#27330 = CARTESIAN_POINT ( 'NONE',  ( 1.250000000000000000, -82.24999999999998579, 0.000000000000000000 ) ) ;
#27331 = CARTESIAN_POINT ( 'NONE',  ( -1.235017835984000056, -79.15406894431399110, 0.06195353447049999768 ) ) ;
#27332 = ORIENTED_EDGE ( 'NONE', *, *, #51357, .F. ) ;
#27333 = CARTESIAN_POINT ( 'NONE',  ( -3.167063118518172793, -77.20133984698613006, -10.27319447007710806 ) ) ;
#27334 = DIRECTION ( 'NONE',  ( -0.7071067811864980568, 0.7071067811865969777, -8.066391409586970286E-09 ) ) ;
#27335 = VERTEX_POINT ( 'NONE', #26792 ) ;
#27336 = ORIENTED_EDGE ( 'NONE', *, *, #34851, .T. ) ;
#27337 = CARTESIAN_POINT ( 'NONE',  ( -4.385047663734000345, -79.77863228676199014, 10.02292886995000032 ) ) ;
#27338 = CARTESIAN_POINT ( 'NONE',  ( 12.50000000000000000, -18.75000000310999937, -1.750000000000000000 ) ) ;
#27339 = CARTESIAN_POINT ( 'NONE',  ( 7.601397897754999633, -60.04999999657000131, 10.07627163191000008 ) ) ;
#27340 = ORIENTED_EDGE ( 'NONE', *, *, #24433, .T. ) ;
#27341 = CARTESIAN_POINT ( 'NONE',  ( -9.747171129529000666, -78.24115059798600669, -7.084379058567000342 ) ) ;
#27342 = CONICAL_SURFACE ( 'NONE', #9446, 11.90000000008999947, 0.7853981633972997312 ) ;
#27343 = ORIENTED_EDGE ( 'NONE', *, *, #21214, .F. ) ;
#27344 = B_SPLINE_SURFACE_WITH_KNOTS ( 'NONE', 3, 3, ( 
 ( #2469, #52630, #12185, #2184 ),
 ( #56483, #16617, #29307, #38755 ),
 ( #3044, #48494, #7466, #11617 ),
 ( #51777, #29592, #6884, #16334 ),
 ( #11327, #47648, #52062, #29879 ),
 ( #8034, #47935, #25464, #7176 ),
 ( #21039, #25176, #16040, #34602 ),
 ( #39043, #42910, #47354, #57055 ),
 ( #43199, #2752, #30170, #7751 ),
 ( #34887, #25756, #33740, #43776 ),
 ( #34023, #3328, #20754, #56195 ) ),
 .UNSPECIFIED., .F., .F., .F.,
 ( 4, 1, 1, 1, 1, 1, 1, 1, 4 ),
 ( 4, 4 ),
 ( -0.02001211456242000045, 0.000000000000000000, 0.1666666666667000196, 0.3333333333333000081, 0.5000000000000000000, 0.6666666666667000474, 0.8333333333333000637, 1.000000000000000000, 1.020273719995999917 ),
 ( -0.3582002740308999900, 1.358863140970000050 ),
 .UNSPECIFIED. ) ;
#27345 = EDGE_LOOP ( 'NONE', ( #595, #14068, #36140, #2406 ) ) ;
#27346 = AXIS2_PLACEMENT_3D ( 'NONE', #16621, #7179, #7756 ) ;
#27347 = CARTESIAN_POINT ( 'NONE',  ( -1.154017715338188976, -2.697074207813733082, -3.037772683525615580 ) ) ;
#27348 = EDGE_CURVE ( 'NONE', #12253, #22602, #54566, .T. ) ;
#27349 = CARTESIAN_POINT ( 'NONE',  ( 7.000000000000000000, -81.99999999999998579, 0.000000000000000000 ) ) ;
#27350 = CARTESIAN_POINT ( 'NONE',  ( 0.000000000000000000, -76.00000000000000000, 0.000000000000000000 ) ) ;
#27351 = ORIENTED_EDGE ( 'NONE', *, *, #27495, .F. ) ;
#27352 = CARTESIAN_POINT ( 'NONE',  ( 0.000000000000000000, -77.49999999999998579, 0.000000000000000000 ) ) ;
#27353 = ORIENTED_EDGE ( 'NONE', *, *, #37116, .F. ) ;
#27354 = CARTESIAN_POINT ( 'NONE',  ( -0.04771499852550991488, -80.52816821537712144, 1.273416777469591477 ) ) ;
#27355 = CARTESIAN_POINT ( 'NONE',  ( -2.398287624620617287, -78.72610001270986402, -3.977573462190889586 ) ) ;
#27356 = DIRECTION ( 'NONE',  ( 0.7071067811865474617, 0.000000000000000000, 0.7071067811865474617 ) ) ;
#27357 = CARTESIAN_POINT ( 'NONE',  ( -0.5999381870725719601, -18.76980390684870059, 10.98362755083785203 ) ) ;
#27358 = CARTESIAN_POINT ( 'NONE',  ( 10.75000000000000000, -78.25000000000000000, 1.005550720961999908E-14 ) ) ;
#27359 = CARTESIAN_POINT ( 'NONE',  ( 0.000000000000000000, -55.54999999966999980, 12.50000000000000000 ) ) ;
#27360 = EDGE_CURVE ( 'NONE', #32930, #27527, #3565, .T. ) ;
#27361 = CARTESIAN_POINT ( 'NONE',  ( -9.964549960865001665, -77.60316956756497575, 6.650098383618001208 ) ) ;
#27362 = CARTESIAN_POINT ( 'NONE',  ( 6.543270582036108785, -78.78770373343947142, -6.538043958785086041 ) ) ;
#27363 = CARTESIAN_POINT ( 'NONE',  ( -12.56594317823000040, -18.74999998606000062, -1.750000000000000000 ) ) ;
#27364 = VECTOR ( 'NONE', #52026, 1000.000000000000000 ) ;
#27365 = CARTESIAN_POINT ( 'NONE',  ( 10.07627163191000008, -18.75000000240999753, -7.601397897754999633 ) ) ;
#27366 = DIRECTION ( 'NONE',  ( 1.044282280788000023E-09, -1.000000000000000000, -6.141137129051000072E-09 ) ) ;
#27367 = CARTESIAN_POINT ( 'NONE',  ( 11.93555832086495805, -78.19079259615151045, -1.854496582926224546 ) ) ;
#27368 = CARTESIAN_POINT ( 'NONE',  ( -1.963540946778999929, -79.64403455456849201, 3.442453740513999882 ) ) ;
#27369 = LINE ( 'NONE', #45700, #57927 ) ;
#27370 = DIRECTION ( 'NONE',  ( 0.000000000000000000, 1.000000000000000000, 0.000000000000000000 ) ) ;
#27371 = FACE_OUTER_BOUND ( 'NONE', #29663, .T. ) ;
#27372 = CARTESIAN_POINT ( 'NONE',  ( -1.466594960159999905, -24.08158199052000015, 12.44238958332999800 ) ) ;
#27373 = CARTESIAN_POINT ( 'NONE',  ( -3.318451405660999942, -86.15275002252400327, 0.9370259671568000881 ) ) ;
#27374 = CARTESIAN_POINT ( 'NONE',  ( -0.7382763017137000672, -1.859138932810000089, 3.717378721030999866 ) ) ;
#27375 = CARTESIAN_POINT ( 'NONE',  ( -0.6295237254636286695, -80.91666666666667140, 1.092232985442819881 ) ) ;
#27376 = CARTESIAN_POINT ( 'NONE',  ( 10.55910102243999837, -56.01514526721999943, 7.642147947524999374 ) ) ;
#27377 = CARTESIAN_POINT ( 'NONE',  ( -1.513474386345976086, -80.33310400781647331, 0.3226607623109409295 ) ) ;
#27378 = CARTESIAN_POINT ( 'NONE',  ( 12.43356840166999788, -61.51269674456000303, -0.8410229959425999935 ) ) ;
#27379 = CARTESIAN_POINT ( 'NONE',  ( -0.9465222407332000154, -81.55663953507000485, -0.8164530897714000757 ) ) ;
#27380 = LINE ( 'NONE', #40078, #6890 ) ;
#27381 = EDGE_CURVE ( 'NONE', #27979, #49445, #7204, .T. ) ;
#27382 = AXIS2_PLACEMENT_3D ( 'NONE', #32012, #17766, #7746 ) ;
#27383 = DIRECTION ( 'NONE',  ( 0.000000000000000000, 1.000000000000000000, 0.000000000000000000 ) ) ;
#27384 = CARTESIAN_POINT ( 'NONE',  ( -7.919595949288999570, -55.64999999965999677, 8.768124086712999699 ) ) ;
#27386 = CARTESIAN_POINT ( 'NONE',  ( 1.301389418711000223, -78.01484642788379631, -0.5625343731648000389 ) ) ;
#27385 = CARTESIAN_POINT ( 'NONE',  ( 1.199500263597268246, -79.70208333333333428, 0.9218200799623752495 ) ) ;
#27387 = CARTESIAN_POINT ( 'NONE',  ( -1.405367936307999832, -81.30880043062998652, -0.7351702954167999016 ) ) ;
#27388 = ORIENTED_EDGE ( 'NONE', *, *, #58205, .T. ) ;
#27389 = B_SPLINE_SURFACE_WITH_KNOTS ( 'NONE', 3, 3, ( 
 ( #28847, #25299, #24440, #43317 ),
 ( #38874, #20020, #15869, #56894 ),
 ( #33855, #43607, #49190, #25873 ),
 ( #53922, #17902, #12866, #30585 ),
 ( #31150, #8444, #21448, #26439 ),
 ( #35006, #39457, #26733, #44183 ),
 ( #44462, #26164, #57748, #3444 ),
 ( #35589, #25585, #57461, #53617 ) ),
 .UNSPECIFIED., .F., .F., .F.,
 ( 4, 1, 1, 1, 1, 4 ),
 ( 4, 4 ),
 ( -0.01200407345745999922, 0.000000000000000000, 0.3333333333333000081, 0.6666666666667000474, 1.000000000000000000, 1.011997855551999947 ),
 ( -0.3559705542741999906, 1.355970554273999928 ),
 .UNSPECIFIED. ) ;
#27390 = CARTESIAN_POINT ( 'NONE',  ( 0.1765916470397999871, -86.00157450217399457, 3.585038641099000056 ) ) ;
#27391 = CARTESIAN_POINT ( 'NONE',  ( -11.54988438476000034, -79.60336391412299406, 2.972544889149000280 ) ) ;
#27392 = CARTESIAN_POINT ( 'NONE',  ( 7.777826874032999882, -80.26050465022970570, -7.857352429981999009 ) ) ;
#27393 = DIRECTION ( 'NONE',  ( -0.7071067812087692417, 2.829525585096875613E-07, 0.7071067811642691714 ) ) ;
#27394 = CARTESIAN_POINT ( 'NONE',  ( -1.116640241144032153, -84.40416667766366743, 3.258149010649826316 ) ) ;
#27395 = CARTESIAN_POINT ( 'NONE',  ( -6.884807209879999057, -78.47409381830098596, -8.855368954042999619 ) ) ;
#27396 = CARTESIAN_POINT ( 'NONE',  ( 12.77651047528000028, -53.49104280904999342, 0.04320343284637000181 ) ) ;
#27397 = CARTESIAN_POINT ( 'NONE',  ( -11.79999999999999893, -18.84999999999999787, 0.000000000000000000 ) ) ;
#27398 = CARTESIAN_POINT ( 'NONE',  ( -3.685431006892999850, -1.816964919272999968, -0.5541339066752000164 ) ) ;
#27399 = CARTESIAN_POINT ( 'NONE',  ( -2.898344733286999819, -79.37214830381199704, -9.457017945469999631 ) ) ;
#27400 = CARTESIAN_POINT ( 'NONE',  ( -7.958776490640000034, -61.27699850015999772, 9.723157983991999487 ) ) ;
#27401 = CARTESIAN_POINT ( 'NONE',  ( -5.818047344251811026, -77.00000000000000000, 7.195567332808626482 ) ) ;
#27402 = ORIENTED_EDGE ( 'NONE', *, *, #568, .T. ) ;
#27403 = DIRECTION ( 'NONE',  ( 0.000000000000000000, -1.000000000000000000, 0.000000000000000000 ) ) ;
#27404 = LINE ( 'NONE', #36848, #39174 ) ;
#27405 = DIRECTION ( 'NONE',  ( -0.7071067811704841999, -1.939412262328955489E-07, 0.7071067812025843002 ) ) ;
#27406 = CARTESIAN_POINT ( 'NONE',  ( 1.500000000000001110, -81.63958333333334849, -0.1963495408493590721 ) ) ;
#27407 = CARTESIAN_POINT ( 'NONE',  ( -12.50659830547393980, -17.02653383374055807, -0.3508384619336013532 ) ) ;
#27408 = CARTESIAN_POINT ( 'NONE',  ( -1.250000000000000000, -77.10000000000000853, 0.000000000000000000 ) ) ;
#27409 = ORIENTED_EDGE ( 'NONE', *, *, #22352, .T. ) ;
#27410 = AXIS2_PLACEMENT_3D ( 'NONE', #18125, #18705, #27830 ) ;
#27411 = CARTESIAN_POINT ( 'NONE',  ( -2.815325398627000375, -78.03378302612298967, -10.73870018959999939 ) ) ;
#27412 = CARTESIAN_POINT ( 'NONE',  ( -1.931043742978000077, -19.22204592323999961, 12.75763395699000036 ) ) ;
#27413 = ORIENTED_EDGE ( 'NONE', *, *, #6993, .T. ) ;
#27414 = VERTEX_POINT ( 'NONE', #31210 ) ;
#27415 = CARTESIAN_POINT ( 'NONE',  ( -1.249603222883986842, -80.59829424211288540, 0.03721083154114489255 ) ) ;
#27416 = EDGE_CURVE ( 'NONE', #23213, #3012, #2494, .T. ) ;
#27417 = CARTESIAN_POINT ( 'NONE',  ( -4.373213035511999358, -79.47851173940198066, -8.733596771889999388 ) ) ;
#27418 = VERTEX_POINT ( 'NONE', #4679 ) ;
#27419 = CARTESIAN_POINT ( 'NONE',  ( -4.913725554697999875, -76.59869191910898678, 11.33327627240999824 ) ) ;
#27420 = DIRECTION ( 'NONE',  ( -0.7071067811865474617, -0.7071067811865474617, 1.721800171537113669E-09 ) ) ;
#27421 = ADVANCED_FACE ( 'NONE', ( #4375 ), #31509, .F. ) ;
#27422 = AXIS2_PLACEMENT_3D ( 'NONE', #42415, #1686, #28810 ) ;
#27423 = CARTESIAN_POINT ( 'NONE',  ( -0.1614608359008000149, -79.09004514702999700, 1.526338918310999881 ) ) ;
#27424 = CARTESIAN_POINT ( 'NONE',  ( -6.013262726775999489, -77.55962694988500061, 7.348341287529000176 ) ) ;
#27425 = AXIS2_PLACEMENT_3D ( 'NONE', #10240, #50403, #51572 ) ;
#27426 = DIRECTION ( 'NONE',  ( 1.000000000000000000, 0.000000000000000000, 0.000000000000000000 ) ) ;
#27427 = CARTESIAN_POINT ( 'NONE',  ( -9.767718346792999995, -78.44420564057999457, 7.129174073149000534 ) ) ;
#27428 = CARTESIAN_POINT ( 'NONE',  ( -3.399999999999999911, -78.69999997992952956, 5.715921273723000819E-07 ) ) ;
#27429 = CARTESIAN_POINT ( 'NONE',  ( 7.256139241522999939, -77.55778581929276072, 6.443535727668999513 ) ) ;
#27430 = CARTESIAN_POINT ( 'NONE',  ( 8.982775494571313857, -79.86926930857234197, 2.207202376408675892 ) ) ;
#27431 = CARTESIAN_POINT ( 'NONE',  ( -1.750000000000000000, -77.50000000000000000, 0.000000000000000000 ) ) ;
#27432 = ORIENTED_EDGE ( 'NONE', *, *, #36754, .F. ) ;
#27433 = CARTESIAN_POINT ( 'NONE',  ( 9.499999999999998224, -77.56041666666668277, 1.243547092045980129 ) ) ;
#27434 = CARTESIAN_POINT ( 'NONE',  ( 2.859599080648278946, -77.25018204720734616, -8.796768031835178192 ) ) ;
#27435 = CARTESIAN_POINT ( 'NONE',  ( -0.1931516691869999969, -80.73785071125600155, 1.503874604587000174 ) ) ;
#27436 = CARTESIAN_POINT ( 'NONE',  ( -3.453171399369999950, -1.863032031399000088, -0.5706200895263999762 ) ) ;
#27437 = DIRECTION ( 'NONE',  ( 1.000000000000000000, 0.000000000000000000, 0.000000000000000000 ) ) ;
#27438 = CARTESIAN_POINT ( 'NONE',  ( 11.93255069029000026, -79.28346444151000583, -2.830763026309000008 ) ) ;
#27439 = CARTESIAN_POINT ( 'NONE',  ( 0.000000000000000000, -76.75499999999999545, 0.000000000000000000 ) ) ;
#27440 = CARTESIAN_POINT ( 'NONE',  ( -2.799999999997999645, -75.99999999999799627, -5.978147109672000789E-11 ) ) ;
#27441 = CARTESIAN_POINT ( 'NONE',  ( -5.759424782279999988, -77.01708832859898735, -7.716175674550000529 ) ) ;
#27442 = CARTESIAN_POINT ( 'NONE',  ( 2.689698932207084336, -77.40716824597529921, 11.76506754417692413 ) ) ;
#27443 = CARTESIAN_POINT ( 'NONE',  ( -13.99936781018472232, -9.295797029142999435, -0.1330447863085613691 ) ) ;
#27444 = VERTEX_POINT ( 'NONE', #18550 ) ;
#27445 = CARTESIAN_POINT ( 'NONE',  ( 1.457613149566999944, -82.61113906848200372, -0.6243081169531999874 ) ) ;
#27446 = CARTESIAN_POINT ( 'NONE',  ( 1.194439549549000112, -80.73125276597998834, -0.6318903263597999143 ) ) ;
#27447 = CARTESIAN_POINT ( 'NONE',  ( 7.770369683894697843, -24.23583903337609158, 10.20674856003130948 ) ) ;
#27448 = CARTESIAN_POINT ( 'NONE',  ( 4.000000000000000000, -75.00000000000001421, -0.5999999999999999778 ) ) ;
#27449 = CARTESIAN_POINT ( 'NONE',  ( 9.438215368887679091, -77.00000000000000000, -0.5776839348911854133 ) ) ;
#27450 = CARTESIAN_POINT ( 'NONE',  ( 0.4826013546558999279, -77.44837184121800533, 11.92487309688999986 ) ) ;
#27451 = CARTESIAN_POINT ( 'NONE',  ( -0.5312504855272001114, -78.69059805011499975, -9.708839960653000034 ) ) ;
#27452 = CARTESIAN_POINT ( 'NONE',  ( -7.648940337505000464, -77.25890875220699172, -5.852081988951999492 ) ) ;
#27453 = CARTESIAN_POINT ( 'NONE',  ( 8.312408207604118360, -76.01187192366691647, 8.304083412923050744 ) ) ;
#27454 = CARTESIAN_POINT ( 'NONE',  ( 2.143349548760000278, -78.81830367376599611, 10.82163513946999878 ) ) ;
#27455 = CARTESIAN_POINT ( 'NONE',  ( 1.473002020459392547, -85.79678895079199208, 3.394151594327925014 ) ) ;
#27456 = ORIENTED_EDGE ( 'NONE', *, *, #48114, .F. ) ;
#27457 = CYLINDRICAL_SURFACE ( 'NONE', #20091, 9.500000000000000000 ) ;
#27458 = CARTESIAN_POINT ( 'NONE',  ( 5.929749634243999701, -79.92525345888189747, -10.35361343416000146 ) ) ;
#27459 = CARTESIAN_POINT ( 'NONE',  ( 3.851650068367000745, -78.43735716284258785, -1.429791614965258972E-15 ) ) ;
#27460 = CIRCLE ( 'NONE', #2049, 1.000000000000000000 ) ;
#27461 = CARTESIAN_POINT ( 'NONE',  ( -10.44304457033000055, -78.46556299312698002, 3.377400876517000050 ) ) ;
#27462 = DIRECTION ( 'NONE',  ( -1.000000000000000000, 0.000000000000000000, 0.000000000000000000 ) ) ;
#27463 = CARTESIAN_POINT ( 'NONE',  ( 9.503324371801999959, -76.56711128452499793, -8.126549174466999759 ) ) ;
#27464 = CYLINDRICAL_SURFACE ( 'NONE', #26440, 11.75000000000000000 ) ;
#27465 = CARTESIAN_POINT ( 'NONE',  ( 9.499157866768639380, -79.10080562451891240, 0.1004279358040388037 ) ) ;
#27466 = ORIENTED_EDGE ( 'NONE', *, *, #12940, .T. ) ;
#27467 = EDGE_CURVE ( 'NONE', #42030, #25015, #13764, .T. ) ;
#27468 = VECTOR ( 'NONE', #36482, 1000.000000000000000 ) ;
#27469 = CARTESIAN_POINT ( 'NONE',  ( 4.801746450173999925, -79.61653908624499820, 10.18710928510000002 ) ) ;
#27470 = CARTESIAN_POINT ( 'NONE',  ( 12.76303204294000082, -18.73514849292999784, 1.980584515756000030 ) ) ;
#27471 = CARTESIAN_POINT ( 'NONE',  ( 8.596418555780418913, -79.80208333333331439, 6.606377239730356621 ) ) ;
#27472 = CARTESIAN_POINT ( 'NONE',  ( -3.962108367559339595, -78.54828561723799396, -0.07469304045245830914 ) ) ;
#27473 = CARTESIAN_POINT ( 'NONE',  ( -0.4814337422054900673, -81.50665477282878157, 1.153442787083076793 ) ) ;
#27474 = CARTESIAN_POINT ( 'NONE',  ( -12.00000000000000000, -55.54999999966999980, -1.250000000000000000 ) ) ;
#27475 = CARTESIAN_POINT ( 'NONE',  ( -8.060167320296210747, -17.37936585541824996, -9.621722526397146424 ) ) ;
#27476 = CARTESIAN_POINT ( 'NONE',  ( -0.1963495408493605987, -81.11458333333332860, -1.500000000000000444 ) ) ;
#27477 = DIRECTION ( 'NONE',  ( -1.000000000000000000, 0.000000000000000000, 0.000000000000000000 ) ) ;
#27478 = CARTESIAN_POINT ( 'NONE',  ( 10.74999999999999645, -78.26041666666667140, 1.407171709420451666 ) ) ;
#27479 = CARTESIAN_POINT ( 'NONE',  ( -12.43569926716000040, -24.88202093001000037, 0.4277578398255000303 ) ) ;
#27480 = ORIENTED_EDGE ( 'NONE', *, *, #36109, .T. ) ;
#27481 = ORIENTED_EDGE ( 'NONE', *, *, #26091, .F. ) ;
#27482 = COLOUR_RGB ( '', 0.08235294, 0.09019608, 0.10196078) ;
#27483 = CARTESIAN_POINT ( 'NONE',  ( 9.933944441255952995, -78.81885939776891803, -4.108317294789329388 ) ) ;
#27484 = EDGE_CURVE ( 'NONE', #1025, #2377, #41130, .T. ) ;
#27485 = CARTESIAN_POINT ( 'NONE',  ( -2.489097927752999873, -77.02533998579799857, 9.212221160641000495 ) ) ;
#27486 = ORIENTED_EDGE ( 'NONE', *, *, #8150, .T. ) ;
#27487 = CARTESIAN_POINT ( 'NONE',  ( 8.899186938125001944, -76.04999999999999716, 6.465637775217000005 ) ) ;
#27488 = CARTESIAN_POINT ( 'NONE',  ( 8.533826143225001104, -25.00526450249999755, 9.213084459905999779 ) ) ;
#27489 = CARTESIAN_POINT ( 'NONE',  ( -8.494907789873000326, -76.52071859265899434, 6.628721719457000283 ) ) ;
#27490 = CARTESIAN_POINT ( 'NONE',  ( 7.756281347497000489, -61.02006031080999549, 10.15825374577000062 ) ) ;
#27491 = CARTESIAN_POINT ( 'NONE',  ( -11.74999252561975993, -76.05421570306441481, -0.7144598671462676354 ) ) ;
#27492 = CARTESIAN_POINT ( 'NONE',  ( -5.261570549498088667, -77.63871931694440320, -10.76270721987074985 ) ) ;
#27493 = CARTESIAN_POINT ( 'NONE',  ( -11.04065564778000130, -79.25198175396400302, 1.980412446595999798 ) ) ;
#27494 = CARTESIAN_POINT ( 'NONE',  ( 7.219057816503211100, -81.00000000000001421, 8.170402670078926732 ) ) ;
#27495 = EDGE_CURVE ( 'NONE', #7896, #14715, #11895, .T. ) ;
#27496 = ORIENTED_EDGE ( 'NONE', *, *, #32747, .T. ) ;
#27497 = CARTESIAN_POINT ( 'NONE',  ( -8.121699804427876757, -24.83626205760389993, 9.841121124182388158 ) ) ;
#27498 = VERTEX_POINT ( 'NONE', #2229 ) ;
#27499 = CARTESIAN_POINT ( 'NONE',  ( 3.727203065783209368, -77.44229855731178702, 8.514839819890244854 ) ) ;
#27500 = CARTESIAN_POINT ( 'NONE',  ( 8.680753609988000719, -77.67284808780799210, 6.821192461343000168 ) ) ;
#27501 = ADVANCED_FACE ( 'NONE', ( #11948 ), #54324, .T. ) ;
#27502 = DIRECTION ( 'NONE',  ( -1.000000000000000000, 0.000000000000000000, 0.000000000000000000 ) ) ;
#27503 = CARTESIAN_POINT ( 'NONE',  ( 9.367484565636001292, -79.11943118893098870, -2.533990228858999938 ) ) ;
#27504 = CARTESIAN_POINT ( 'NONE',  ( 6.842107050174999650, -76.58777295158999721, -11.01216002263999982 ) ) ;
#27505 = CARTESIAN_POINT ( 'NONE',  ( -1.681307385754345685, -2.082147688907624694, -2.810393918989617212 ) ) ;
#27506 = CARTESIAN_POINT ( 'NONE',  ( -0.8961266428360998848, -77.63259150256999419, 1.358359200922999888 ) ) ;
#27507 = CARTESIAN_POINT ( 'NONE',  ( -7.054457466615000172, -80.56154281250199745, -8.769379688592000122 ) ) ;
#27508 = CARTESIAN_POINT ( 'NONE',  ( 8.999546809828999017, -78.13273556822998955, -5.951127176402999375 ) ) ;
#27509 = CARTESIAN_POINT ( 'NONE',  ( 12.76303204525000012, -60.06485147653999945, 1.980584515753000208 ) ) ;
#27510 = CARTESIAN_POINT ( 'NONE',  ( 12.49168433577000137, -55.50150862742999891, -1.667916687244999974 ) ) ;
#27511 = CARTESIAN_POINT ( 'NONE',  ( 3.232998297510000008, -82.30958586555499323, -1.191365385135000121 ) ) ;
#27512 = VERTEX_POINT ( 'NONE', #29926 ) ;
#27513 = CARTESIAN_POINT ( 'NONE',  ( 1.505038102365999997, -79.30638830090799729, 12.22460098059000089 ) ) ;
#27514 = CARTESIAN_POINT ( 'NONE',  ( -4.507826919401000332, -76.16562155000400480, -10.31444853584999954 ) ) ;
#27515 = CARTESIAN_POINT ( 'NONE',  ( -6.954863410765665499, -78.03105792949766339, 8.197110803945740543 ) ) ;
#27516 = CARTESIAN_POINT ( 'NONE',  ( 1.634596122093999959, -78.99778786954298937, 11.63574645295999943 ) ) ;
#27517 = CARTESIAN_POINT ( 'NONE',  ( -10.19019671031999863, -18.80356357339999818, 7.646965722246000574 ) ) ;
#27519 = CARTESIAN_POINT ( 'NONE',  ( -10.75000000000000000, -79.50000000000000000, 0.000000000000000000 ) ) ;
#27518 = CARTESIAN_POINT ( 'NONE',  ( 3.075537641221555596, -78.44583333333332575, -11.44417895085270587 ) ) ;
#27520 = FACE_OUTER_BOUND ( 'NONE', #8186, .T. ) ;
#27521 = CARTESIAN_POINT ( 'NONE',  ( 7.971085775996931133, -80.90878701328509237, 7.212855077932124104 ) ) ;
#27522 = CARTESIAN_POINT ( 'NONE',  ( 7.993200843029001135, -77.78490534060698280, -4.971914600080000746 ) ) ;
#27523 = CARTESIAN_POINT ( 'NONE',  ( 0.3995786188288962815, -86.02148118236289065, -8.919459997437842347 ) ) ;
#27524 = CARTESIAN_POINT ( 'NONE',  ( 3.947457275559000500, -78.61298354959900792, -10.30140706531999939 ) ) ;
#27525 = DIRECTION ( 'NONE',  ( 0.000000000000000000, 1.000000000000000000, 0.000000000000000000 ) ) ;
#27526 = CARTESIAN_POINT ( 'NONE',  ( 0.5321997431402999412, -80.76233357467889107, 11.12807117834999993 ) ) ;
#27527 = VERTEX_POINT ( 'NONE', #12228 ) ;
#27528 = CYLINDRICAL_SURFACE ( 'NONE', #41973, 11.00000000000000000 ) ;
#27529 = CARTESIAN_POINT ( 'NONE',  ( -0.7479529023059999782, -77.76872403538301626, -9.465622776916999825 ) ) ;
#27530 = DIRECTION ( 'NONE',  ( 0.000000000000000000, 1.000000000000000000, 0.000000000000000000 ) ) ;
#27531 = CARTESIAN_POINT ( 'NONE',  ( -9.524774638983998898, -77.15403809539800761, 5.924253427062000199 ) ) ;
#27532 = DIRECTION ( 'NONE',  ( 0.7071067811865969777, -0.7071067811864980568, -1.305609853748994042E-09 ) ) ;
#27533 = CARTESIAN_POINT ( 'NONE',  ( 10.75000000000000000, -76.85000000000000853, 0.000000000000000000 ) ) ;
#27534 = CARTESIAN_POINT ( 'NONE',  ( -1.750000000000000000, -60.04999999657000131, 12.50000000000000000 ) ) ;
#27535 = CARTESIAN_POINT ( 'NONE',  ( -3.518896154528292186, -78.59855647164599191, -10.19177539389869658 ) ) ;
#27536 = DIRECTION ( 'NONE',  ( 0.9936845293270585300, 0.1122098755727947705, 0.000000000000000000 ) ) ;
#27537 = EDGE_CURVE ( 'NONE', #39723, #42409, #9217, .T. ) ;
#27538 = CARTESIAN_POINT ( 'NONE',  ( 2.264963459394000012, -85.19317953870898918, -3.503781609835999955 ) ) ;
#27539 = CARTESIAN_POINT ( 'NONE',  ( -7.651160336710000287, -19.23767313813999991, -10.45205658995999976 ) ) ;
#27540 = EDGE_CURVE ( 'NONE', #25253, #26404, #27917, .T. ) ;
#27541 = CARTESIAN_POINT ( 'NONE',  ( 9.101506735319000896, -53.91932813864999474, -8.485532457216999447 ) ) ;
#27542 = CARTESIAN_POINT ( 'NONE',  ( -9.340344124447998553, -76.82376637690499876, -6.292213870087999261 ) ) ;
#27543 = CARTESIAN_POINT ( 'NONE',  ( -12.89999999994999769, -2.999999999951000085, -1.886268936261000296E-09 ) ) ;
#27544 = CARTESIAN_POINT ( 'NONE',  ( 1.251226418338000190, -78.09316549288999454, -0.9133082017320000023 ) ) ;
#27545 = CARTESIAN_POINT ( 'NONE',  ( -0.1380878921325282283, -62.02734402296150762, 12.70555840936477310 ) ) ;
#27546 = CARTESIAN_POINT ( 'NONE',  ( 1.290261244888944558, -82.95647159644285296, -0.7858742426583964491 ) ) ;
#27547 = CONICAL_SURFACE ( 'NONE', #1167, 3.471875000818999801, 0.7853981633972997312 ) ;
#27548 = CARTESIAN_POINT ( 'NONE',  ( -12.66314513620999804, -61.97864743329000703, -0.04033065750138999789 ) ) ;
#27549 = CARTESIAN_POINT ( 'NONE',  ( -10.13785388426000011, -78.38129286498505621, -4.205702700205000255 ) ) ;
#27550 = CARTESIAN_POINT ( 'NONE',  ( 1.250000000000000000, -55.35321828636000419, 12.50000000000000000 ) ) ;
#27551 = EDGE_LOOP ( 'NONE', ( #55217, #1198, #39013, #55165 ) ) ;
#27552 = CARTESIAN_POINT ( 'NONE',  ( 0.6127881360814133593, -81.76611797205174526, -1.089408548475932381 ) ) ;
#27553 = VECTOR ( 'NONE', #2985, 1000.000000000000000 ) ;
#27554 = CARTESIAN_POINT ( 'NONE',  ( 1.103931350763639241, -61.42083747905927993, 12.50298439261563388 ) ) ;
#27555 = CARTESIAN_POINT ( 'NONE',  ( -6.167563198928999846, -79.81279398642419665, 9.285244464097999639 ) ) ;
#27556 = CARTESIAN_POINT ( 'NONE',  ( 8.140250184777904963, -55.34839576619644674, 7.398464061250712653 ) ) ;
#27557 = VERTEX_POINT ( 'NONE', #52106 ) ;
#27558 = ORIENTED_EDGE ( 'NONE', *, *, #30419, .T. ) ;
#27559 = CARTESIAN_POINT ( 'NONE',  ( 1.560799078659000028, -80.76255925591399887, 0.4136666654166999413 ) ) ;
#27560 = VERTEX_POINT ( 'NONE', #7513 ) ;
#27561 = DIRECTION ( 'NONE',  ( 0.000000000000000000, 1.000000000000000000, 0.000000000000000000 ) ) ;
#27562 = EDGE_LOOP ( 'NONE', ( #17385, #51410, #51626, #12475 ) ) ;
#27563 = CARTESIAN_POINT ( 'NONE',  ( -4.000000000000000000, -5.000000000000000000, -0.5999999999999999778 ) ) ;
#27564 = AXIS2_PLACEMENT_3D ( 'NONE', #2673, #42245, #20950 ) ;
#27565 = FACE_OUTER_BOUND ( 'NONE', #44482, .T. ) ;
#27566 = CARTESIAN_POINT ( 'NONE',  ( 1.750000000001000089, -55.55000001292999912, 12.56594318049000059 ) ) ;
#27567 = CARTESIAN_POINT ( 'NONE',  ( 2.062323307449999810, -23.22713153192000135, -12.83634826442999888 ) ) ;
#27568 = CARTESIAN_POINT ( 'NONE',  ( 1.459243437995999981, -80.97495933943199020, -3.461499544958999586 ) ) ;
#27569 = CARTESIAN_POINT ( 'NONE',  ( 7.624341766656999475, -60.06485146221000093, 10.42531125026000005 ) ) ;
#27570 = CARTESIAN_POINT ( 'NONE',  ( -3.846946059935000051, -78.43062821897001413, -11.43190855169999942 ) ) ;
#27571 = ADVANCED_FACE ( 'NONE', ( #11663 ), #16666, .F. ) ;
#27572 = ORIENTED_EDGE ( 'NONE', *, *, #22427, .T. ) ;
#27573 = ORIENTED_EDGE ( 'NONE', *, *, #22764, .T. ) ;
#27574 = DIRECTION ( 'NONE',  ( 0.7071067811864980568, 0.7071067811865969777, -2.302419900729990164E-09 ) ) ;
#27575 = CARTESIAN_POINT ( 'NONE',  ( 0.000000000000000000, -75.10000000284179578, 7.200000000000000178 ) ) ;
#27576 = CARTESIAN_POINT ( 'NONE',  ( 0.000000000000000000, -75.67500000000001137, 0.000000000000000000 ) ) ;
#27577 = ADVANCED_FACE ( 'NONE', ( #20229 ), #44589, .F. ) ;
#27578 = CARTESIAN_POINT ( 'NONE',  ( 1.021809889922000059, -79.46012293261399861, -0.8570204080543000202 ) ) ;
#27579 = FACE_OUTER_BOUND ( 'NONE', #40291, .T. ) ;
#27580 = CARTESIAN_POINT ( 'NONE',  ( 0.000000000000000000, -76.19999999999998863, 0.000000000000000000 ) ) ;
#27581 = CARTESIAN_POINT ( 'NONE',  ( -10.42272502862000039, -21.75453807238000081, 7.691893942719999266 ) ) ;
#27582 = CARTESIAN_POINT ( 'NONE',  ( 5.421352887295999956, -76.67165190241000516, 11.59375966951999892 ) ) ;
#27583 = CARTESIAN_POINT ( 'NONE',  ( 1.426111243542000029, -79.91250488267000662, 0.3502211593775000353 ) ) ;
#27584 = CARTESIAN_POINT ( 'NONE',  ( -9.359285000798275078, -77.03899693750341271, 1.284050242927868624 ) ) ;
#27585 = DIRECTION ( 'NONE',  ( 0.000000000000000000, 0.000000000000000000, 1.000000000000000000 ) ) ;
#27586 = CARTESIAN_POINT ( 'NONE',  ( 1.960320388553999926, -79.69568553133959199, 3.683370289565999656 ) ) ;
#27588 = CONICAL_SURFACE ( 'NONE', #46468, 9.649999999948999374, 0.7853981633972997312 ) ;
#27587 = CARTESIAN_POINT ( 'NONE',  ( 10.78853149093999875, -80.49286902822179002, -3.242959171380999983 ) ) ;
#27589 = CARTESIAN_POINT ( 'NONE',  ( 9.310971084499998440, -78.34291001420200473, 2.673395725080999874 ) ) ;
#27590 = CARTESIAN_POINT ( 'NONE',  ( -11.00000000000000000, -23.75000000000000000, 0.000000000000000000 ) ) ;
#27591 = CARTESIAN_POINT ( 'NONE',  ( 2.784738954513000131, -80.80932046129099433, -2.197676404043999998 ) ) ;
#27592 = CARTESIAN_POINT ( 'NONE',  ( 0.6849175148897999055, -77.88980665715600082, -1.144319635748999975 ) ) ;
#27593 = EDGE_CURVE ( 'NONE', #27414, #30828, #53371, .T. ) ;
#27594 = FACE_OUTER_BOUND ( 'NONE', #8891, .T. ) ;
#27595 = CARTESIAN_POINT ( 'NONE',  ( 8.440675369999999234, -80.20707853072349280, 7.053722371789000967 ) ) ;
#27596 = CARTESIAN_POINT ( 'NONE',  ( 3.772660615778999915, -2.077883300257999721, 0.5031134774969999723 ) ) ;
#27597 = CARTESIAN_POINT ( 'NONE',  ( 0.3271848554491016414, -79.14583333333330017, -1.217465845835393967 ) ) ;
#27598 = ORIENTED_EDGE ( 'NONE', *, *, #16619, .T. ) ;
#27599 = DIRECTION ( 'NONE',  ( 0.000000000000000000, 0.000000000000000000, -1.000000000000000000 ) ) ;
#27600 = CARTESIAN_POINT ( 'NONE',  ( 0.4515105396355221234, -18.45278097531555161, -10.99076531923743083 ) ) ;
#27601 = VECTOR ( 'NONE', #40651, 1000.000000000000000 ) ;
#27602 = CARTESIAN_POINT ( 'NONE',  ( 11.74514291648612918, -77.45731891081528886, 1.539200744266281173 ) ) ;
#27603 = CARTESIAN_POINT ( 'NONE',  ( -1.127489577578000057, -80.80475223809600038, -0.5989559841152000130 ) ) ;
#27604 = CARTESIAN_POINT ( 'NONE',  ( -5.192407727267999817, -79.90950158836399453, -8.254012402074000221 ) ) ;
#27605 = CARTESIAN_POINT ( 'NONE',  ( -9.234979314279001983, -77.04487755778998803, -9.168119495123999485 ) ) ;
#27606 = CARTESIAN_POINT ( 'NONE',  ( -4.854729178351636421, -79.51242566855798088, 9.591276152018627599 ) ) ;
#27607 = CARTESIAN_POINT ( 'NONE',  ( 1.828070329658999960, -79.36668667140099842, 9.453928736856999748 ) ) ;
#27608 = CARTESIAN_POINT ( 'NONE',  ( -10.75000000000000000, -76.59999999999999432, 0.000000000000000000 ) ) ;
#27609 = ORIENTED_EDGE ( 'NONE', *, *, #56755, .F. ) ;
#27610 = EDGE_CURVE ( 'NONE', #35538, #5930, #22321, .T. ) ;
#27611 = CIRCLE ( 'NONE', #6894, 1.250000000000000444 ) ;
#27612 = CARTESIAN_POINT ( 'NONE',  ( -9.502896617869424745, -24.74094210337188926, -8.179425869181063291 ) ) ;
#27613 = CARTESIAN_POINT ( 'NONE',  ( 4.837141563511999642, -77.90371847557099727, -10.06315987337999829 ) ) ;
#27614 = CARTESIAN_POINT ( 'NONE',  ( 0.9313429465132000429, -81.47980690754000932, -1.056595210376000127 ) ) ;
#27615 = PLANE ( 'NONE',  #12530 ) ;
#27616 = CARTESIAN_POINT ( 'NONE',  ( -9.108272167377998940, -77.48048492307799506, -2.776672910959999907 ) ) ;
#27618 = CARTESIAN_POINT ( 'NONE',  ( -0.4617212151683000032, -1.132168933658999954, 3.989551193614000013 ) ) ;
#27617 = CARTESIAN_POINT ( 'NONE',  ( 1.290002129988000235, -84.19350903806798669, 3.970579864698999817 ) ) ;
#27619 = CARTESIAN_POINT ( 'NONE',  ( -1.799475304559999822, -57.04828923575999511, -12.69616050746999925 ) ) ;
#27620 = CARTESIAN_POINT ( 'NONE',  ( -1.500000000000000000, -81.50000000000000000, 0.000000000000000000 ) ) ;
#27621 = ORIENTED_EDGE ( 'NONE', *, *, #24448, .F. ) ;
#27622 = CARTESIAN_POINT ( 'NONE',  ( 1.333500915678079490, -77.23504576798873700, -10.67566761252578011 ) ) ;
#27623 = CARTESIAN_POINT ( 'NONE',  ( -1.500000000000000000, -79.39999999999999147, 0.000000000000000000 ) ) ;
#27624 = ORIENTED_EDGE ( 'NONE', *, *, #20710, .F. ) ;
#27625 = ORIENTED_EDGE ( 'NONE', *, *, #34452, .F. ) ;
#27626 = CARTESIAN_POINT ( 'NONE',  ( -0.6493855936264999462, -79.75053993242899253, 10.92090362500000111 ) ) ;
#27627 =( NAMED_UNIT ( * ) SI_UNIT ( $, .STERADIAN. ) SOLID_ANGLE_UNIT ( ) );
#27628 = CARTESIAN_POINT ( 'NONE',  ( 4.766258734843114908, -80.33859090758983257, 9.686463997712579044 ) ) ;
#27629 = ORIENTED_EDGE ( 'NONE', *, *, #53205, .F. ) ;
#27630 = CARTESIAN_POINT ( 'NONE',  ( -0.08569088068254999968, -78.56670238307098941, 12.04941611642000154 ) ) ;
#27631 = AXIS2_PLACEMENT_3D ( 'NONE', #34190, #52512, #52228 ) ;
#27632 = ORIENTED_EDGE ( 'NONE', *, *, #51138, .F. ) ;
#27633 = ORIENTED_EDGE ( 'NONE', *, *, #18739, .T. ) ;
#27634 = CARTESIAN_POINT ( 'NONE',  ( 0.05356364311145376395, -2.727063383492749349, -3.249227035622031856 ) ) ;
#27635 = CIRCLE ( 'NONE', #44632, 10.05000000000000071 ) ;
#27636 = CARTESIAN_POINT ( 'NONE',  ( -10.41501344424586151, -76.44116683086167541, -6.014273019200089720 ) ) ;
#27637 = DIRECTION ( 'NONE',  ( -1.000000000000000000, -1.534448722697999916E-11, -3.998226783829999760E-14 ) ) ;
#27638 = B_SPLINE_SURFACE_WITH_KNOTS ( 'NONE', 3, 3, ( 
 ( #26335, #3620, #38768, #44351, #52362, #7480, #3905, #16919, #34615, #49080, #30758, #17487, #43792, #57069, #21907, #39916, #48232, #34898, #29891, #47948, #43497, #3058, #53214, #39631, #21053, #57932, #12761, #16629, #48791, #7767, #35474, #52928, #52643, #53503, #26616 ),
 ( #12478, #12198, #30479, #57638, #48506, #8051, #13045, #31043, #8630, #44651, #30182, #25770, #3341, #44071, #46131, #31926, #10101, #23082, #32503, #27500, #5371, #50548, #17788, #54961, #8927, #40513, #49971, #54394, #13931, #22502, #45541, #397, #18374, #54677, #13340 ),
 ( #9514, #22203, #5086, #14512, #23379, #58225, #14219, #108, #45246, #45836, #688, #31336, #41389, #32216, #9807, #41096, #18670, #36659, #36368, #50258, #27790, #26916, #9222, #27207, #40214, #972, #54098, #18955, #36948, #35777, #28081, #4503, #18083, #53805, #49380 ),
 ( #36077, #44947, #13638, #31634, #49676, #4794, #22794, #40803, #10689, #33093, #42270, #23664, #51135, #20125, #46719, #15396, #55845, #37825, #15684, #47005, #37527, #33680, #52003, #24544, #6532, #38403, #51718, #20409, #28373, #1836, #19245, #46418, #11268, #2125, #29248 ) ),
 .UNSPECIFIED., .F., .F., .F.,
 ( 4, 4 ),
 ( 4, 1, 1, 1, 1, 1, 1, 1, 1, 1, 1, 1, 1, 1, 1, 1, 1, 1, 1, 1, 1, 1, 1, 1, 1, 1, 1, 1, 1, 1, 1, 1, 4 ),
 ( -0.4045438850611000059, 1.404543885061000141 ),
 ( 0.4225136409995000064, 0.4409139416538999656, 0.4593142423082999803, 0.4777145429628000262, 0.4961148436172000409, 0.5145151442715999446, 0.5329154449260999904, 0.5513157455805000051, 0.5697160462349000198, 0.5881163468892999235, 0.6065166475437999694, 0.6249169481981999841, 0.6433172488525999988, 0.6617175495070000135, 0.6801178501615000593, 0.6985181508158999630, 0.7169184514702999778, 0.7353187521247999126, 0.7537190527792000383, 0.7721193534336000530, 0.7905196540880000677, 0.8089199547425000025, 0.8273202553968999062, 0.8457205560512999210, 0.8641208567057999668, 0.8825211573601999815, 0.9009214580145999962, 0.9193217586690000109, 0.9377220593235000567, 0.9561223599778999604, 0.9745226606322999752, 0.9929229612868000210, 1.011323261940999974 ),
 .UNSPECIFIED. ) ;
#27639 = VERTEX_POINT ( 'NONE', #3939 ) ;
#27640 = CARTESIAN_POINT ( 'NONE',  ( -1.500000000000000000, -80.50000000000000000, 0.000000000000000000 ) ) ;
#27641 = ORIENTED_EDGE ( 'NONE', *, *, #33229, .F. ) ;
#27642 = CARTESIAN_POINT ( 'NONE',  ( -1.152422862266062609, -80.11472968720097754, 0.5432694035117214826 ) ) ;
#27643 = ADVANCED_FACE ( 'NONE', ( #39386 ), #8965, .F. ) ;
#27644 = FACE_OUTER_BOUND ( 'NONE', #12461, .T. ) ;
#27645 = TOROIDAL_SURFACE ( 'NONE', #22938, 26.50000000000000000, 14.00000000000000000 ) ;
#27646 = CYLINDRICAL_SURFACE ( 'NONE', #53823, 9.599999999999999645 ) ;
#27647 = CARTESIAN_POINT ( 'NONE',  ( -5.279550234765999939, -76.35198175396399733, -9.859017853534000508 ) ) ;
#27648 = CARTESIAN_POINT ( 'NONE',  ( -8.872958366904050820, -25.01010144684924086, 8.813896669003202788 ) ) ;
#27649 = AXIS2_PLACEMENT_3D ( 'NONE', #25449, #7157, #25159 ) ;
#27650 = CARTESIAN_POINT ( 'NONE',  ( 13.94241847916999966, -46.33997059779999717, 4.312626734956999977E-05 ) ) ;
#27651 = CARTESIAN_POINT ( 'NONE',  ( -7.892176027305001007, -76.76043262182999172, 7.987326983142001069 ) ) ;
#27652 = CARTESIAN_POINT ( 'NONE',  ( -1.785035796832132426, -78.70961624886150787, -9.076082582026554491 ) ) ;
#27653 = CARTESIAN_POINT ( 'NONE',  ( 3.878365675696000103, -77.22946001420200446, -8.575257901267999472 ) ) ;
#27654 = CARTESIAN_POINT ( 'NONE',  ( 0.000000000000000000, -80.99999999999998579, 7.000000000000000000 ) ) ;
#27655 = CARTESIAN_POINT ( 'NONE',  ( -9.090730535106020582, -80.14771101264726383, -6.193863875913084627 ) ) ;
#27656 = FACE_OUTER_BOUND ( 'NONE', #46481, .T. ) ;
#27657 = CARTESIAN_POINT ( 'NONE',  ( 4.118783384051000418, -79.27942549782629555, 0.3068013588580000284 ) ) ;
#27658 = CARTESIAN_POINT ( 'NONE',  ( 7.574740816159999390, -77.88991332859899330, -5.983027492110999823 ) ) ;
#27659 = CARTESIAN_POINT ( 'NONE',  ( -1.750000000001000089, -60.04999998641999781, 12.56594318054000148 ) ) ;
#27660 = EDGE_CURVE ( 'NONE', #26860, #20749, #11323, .T. ) ;
#27661 = FACE_BOUND ( 'NONE', #21609, .T. ) ;
#27662 = CARTESIAN_POINT ( 'NONE',  ( -1.632307027708999936, -23.66927189556999878, 12.46200249212000166 ) ) ;
#27663 = CARTESIAN_POINT ( 'NONE',  ( 2.194848540722183827, -79.99999999999997158, 9.090985499525780611 ) ) ;
#27664 = CARTESIAN_POINT ( 'NONE',  ( -1.528023617186000216, -0.8891593309027000513, -3.828850291668000061 ) ) ;
#27665 = CARTESIAN_POINT ( 'NONE',  ( 1.092232985442820992, -80.79166666666665719, 0.6295237254636267821 ) ) ;
#27666 = DIRECTION ( 'NONE',  ( 0.9957542233426779354, 0.04890176637353889355, 0.07798810127684829840 ) ) ;
#27667 = CARTESIAN_POINT ( 'NONE',  ( 1.024957315614702491, -79.66505809141212069, 1.112825025314110539 ) ) ;
#27668 = CARTESIAN_POINT ( 'NONE',  ( -1.250000000000000000, -81.51887984502332074, -0.2965639121358149555 ) ) ;
#27669 = DIRECTION ( 'NONE',  ( 0.000000000000000000, 0.000000000000000000, -1.000000000000000000 ) ) ;
#27670 = CARTESIAN_POINT ( 'NONE',  ( 7.036824827271694005, -79.54050048329402500, -6.487746313484107574 ) ) ;
#27671 = CARTESIAN_POINT ( 'NONE',  ( -5.393290222407999934, -77.46222517136899910, -11.03214393298000040 ) ) ;
#27672 = CARTESIAN_POINT ( 'NONE',  ( 1.250000000000000000, -82.24999999999998579, 0.000000000000000000 ) ) ;
#27674 = CARTESIAN_POINT ( 'NONE',  ( 0.9474668951539000350, -78.11407167464599866, 1.054687619119999864 ) ) ;
#27673 = DIRECTION ( 'NONE',  ( 0.000000000000000000, 1.000000000000000000, 0.000000000000000000 ) ) ;
#27675 = CARTESIAN_POINT ( 'NONE',  ( -1.392304720662999928, -81.22443067016000384, -0.3162235598901000366 ) ) ;
#27676 = VERTEX_POINT ( 'NONE', #18412 ) ;
#27677 = EDGE_CURVE ( 'NONE', #48697, #46616, #25158, .T. ) ;
#27678 = CARTESIAN_POINT ( 'NONE',  ( 1.948614114418999899, -85.40032450217400140, -3.014405495351000219 ) ) ;
#27679 = TOROIDAL_SURFACE ( 'NONE', #55045, 1.250000000000000000, 0.5000000000000000000 ) ;
#27680 = CARTESIAN_POINT ( 'NONE',  ( 11.83689625619999930, -79.36366123649499116, -1.457305633747999929 ) ) ;
#27681 = CARTESIAN_POINT ( 'NONE',  ( -10.32512362061000033, -80.67574026708460622, 4.564420309708999923 ) ) ;
#27682 = CARTESIAN_POINT ( 'NONE',  ( -1.750000000000000000, -18.75000000310999937, -12.50000000000000000 ) ) ;
#27683 = CARTESIAN_POINT ( 'NONE',  ( 1.500000000000000888, -81.73958333333332860, -0.1963495408493590444 ) ) ;
#27684 = CARTESIAN_POINT ( 'NONE',  ( -9.950000000000001066, -86.20000000000000284, 0.000000000000000000 ) ) ;
#27685 = CARTESIAN_POINT ( 'NONE',  ( 0.000000000000000000, -76.29999999999999716, 0.000000000000000000 ) ) ;
#27686 = LINE ( 'NONE', #27101, #24183 ) ;
#27687 = CARTESIAN_POINT ( 'NONE',  ( 11.55824937009300868, -79.80000000000001137, -2.451020469013467817 ) ) ;
#27688 = CLOSED_SHELL ( 'NONE', ( #8698, #37315, #12420, #1371, #56624, #26073, #26346, #3095, #28658, #9343, #28734, #34152, #13633, #44629, #35839, #5604, #56697, #23541, #52166, #23218, #35341, #48609, #31185, #52956, #28115, #11544, #35324, #7646, #26828, #16092, #57761, #1985, #22767, #43642, #7940, #55312, #32074, #26223, #6255, #20341, #51716, #29414, #36185, #50176, #34872, #33638, #13136, #29595, #4304, #16642, #21961, #47442, #49177, #14901, #45622, #80, #33876, #33, #29702, #32044, #13191, #16840, #18319, #41242, #1737, #30386, #24500, #7287, #40922, #46863, #54351, #1702, #55017, #47661, #9322, #34053, #25020, #34024, #9826, #29705, #41772, #27898, #19190, #42132, #45687, #37233, #30863, #51647, #44420, #47724, #58280, #49434, #29394, #39554, #41948, #15439, #3977, #7106, #42183, #33909, #13804, #34759, #58223, #335, #12739, #12705 ) ) ;
#27689 = CARTESIAN_POINT ( 'NONE',  ( -10.70506908183094197, -76.16458333332448660, 2.279133419649182368 ) ) ;
#27690 = ORIENTED_EDGE ( 'NONE', *, *, #42111, .F. ) ;
#27691 = CIRCLE ( 'NONE', #20176, 1.750000000000000000 ) ;
#27692 = CARTESIAN_POINT ( 'NONE',  ( -1.583004792650378079, -54.34790758811381295, -12.70616254407330104 ) ) ;
#27693 = CARTESIAN_POINT ( 'NONE',  ( -0.5912419659665999472, -79.50933998579799322, 9.397521941627999809 ) ) ;
#27694 = CARTESIAN_POINT ( 'NONE',  ( -7.601397897754999633, -18.75000000310999937, 10.07627163191000008 ) ) ;
#27695 = EDGE_CURVE ( 'NONE', #30078, #30606, #23992, .T. ) ;
#27696 = CARTESIAN_POINT ( 'NONE',  ( -1.500000000000000000, -81.40000000000000568, 0.000000000000000000 ) ) ;
#27697 = EDGE_CURVE ( 'NONE', #36041, #7374, #28227, .T. ) ;
#27698 = DIRECTION ( 'NONE',  ( 0.000000000000000000, 0.000000000000000000, -1.000000000000000000 ) ) ;
#27699 = EDGE_LOOP ( 'NONE', ( #56022, #31980, #16942, #18286 ) ) ;
#27700 = CARTESIAN_POINT ( 'NONE',  ( 10.71380177098999908, -78.18052186078398336, 0.1798162837734999797 ) ) ;
#27701 = CARTESIAN_POINT ( 'NONE',  ( -1.799502287691000069, -18.69283319134000010, 12.60413670420000010 ) ) ;
#27702 = ORIENTED_EDGE ( 'NONE', *, *, #29166, .T. ) ;
#27703 = ORIENTED_EDGE ( 'NONE', *, *, #50223, .T. ) ;
#27704 = CARTESIAN_POINT ( 'NONE',  ( -7.624341766647000362, -18.73514853758999976, 10.42531125024999916 ) ) ;
#27705 = CARTESIAN_POINT ( 'NONE',  ( 9.630577183392999174, -79.15378515682199634, 1.628483183780000010 ) ) ;
#27706 = AXIS2_PLACEMENT_3D ( 'NONE', #3475, #21480, #26194 ) ;
#27707 = VERTEX_POINT ( 'NONE', #27826 ) ;
#27708 = CARTESIAN_POINT ( 'NONE',  ( 12.70926961117000076, -55.39159259587000150, 1.933875435151000133 ) ) ;
#27709 = CARTESIAN_POINT ( 'NONE',  ( 8.485281374238999419, -55.54999999966999980, -8.485281374238999419 ) ) ;
#27710 = B_SPLINE_CURVE_WITH_KNOTS ( 'NONE', 3,
 ( #10559, #11936, #19411, #43519, #42439, #16365, #6116, #21357, #55720, #20003, #43817, #16653, #24123, #57380, #12218, #3362, #25501, #29915, #3080, #34346, #34637, #42141, #38789, #16940, #30500 ),
 .UNSPECIFIED., .F., .F.,
 ( 4, 1, 1, 1, 1, 1, 2, 2, 1, 1, 1, 2, 2, 1, 2, 2, 4 ),
 ( 0.000000000000000000, 0.1250000000000003331, 0.1875000000000004996, 0.2187500000000005829, 0.2343750000000006106, 0.2421875000000006384, 0.2460937500000006661, 0.2500000000000006661, 0.3750000000000012768, 0.4375000000000016098, 0.4687500000000017764, 0.4843750000000017764, 0.5000000000000017764, 0.6250000000000014433, 0.6875000000000012212, 0.7500000000000011102, 1.000000000000000000 ),
 .UNSPECIFIED. ) ;
#27711 = CARTESIAN_POINT ( 'NONE',  ( -0.9961134219653000610, -78.77545572834999632, -1.167706195293999993 ) ) ;
#27712 = ORIENTED_EDGE ( 'NONE', *, *, #18085, .F. ) ;
#27713 = CARTESIAN_POINT ( 'NONE',  ( 5.807838419657000095, -77.30742694988499863, -7.511754867730999763 ) ) ;
#27714 = CARTESIAN_POINT ( 'NONE',  ( -1.250000000000000000, -80.09999999999999432, 0.000000000000000000 ) ) ;
#27715 = CARTESIAN_POINT ( 'NONE',  ( -1.811016405462517076, -17.93826444627195116, -12.71771640064051034 ) ) ;
#27716 = CARTESIAN_POINT ( 'NONE',  ( 11.68767212001979594, -79.02916666666666856, -3.140974612311341563 ) ) ;
#27717 = VECTOR ( 'NONE', #55082, 1000.000000000000000 ) ;
#27718 = CARTESIAN_POINT ( 'NONE',  ( 8.993876985514928535, -79.86887379514664076, 2.161346897475597828 ) ) ;
#27719 = CARTESIAN_POINT ( 'NONE',  ( 2.539779680857219279, -79.66354165636154505, 3.155564599645395596 ) ) ;
#27720 = VERTEX_POINT ( 'NONE', #22830 ) ;
#27721 = CARTESIAN_POINT ( 'NONE',  ( -9.722718241315000398, -23.25000000000000000, -7.247844507162001015 ) ) ;
#27722 = CARTESIAN_POINT ( 'NONE',  ( 11.50190934395000042, -76.70965847532001192, -3.421415122956000143 ) ) ;
#27723 = CARTESIAN_POINT ( 'NONE',  ( -0.6885369103866999518, -80.44017497096899660, -1.350873448928000098 ) ) ;
#27724 = DIRECTION ( 'NONE',  ( 0.07798810159119662355, -0.04890177459382791247, 0.9957542229143573342 ) ) ;
#27725 = CARTESIAN_POINT ( 'NONE',  ( 3.313940609516682123, -2.126588154580539403, 1.183591495650892833 ) ) ;
#27726 = CARTESIAN_POINT ( 'NONE',  ( 7.605690822197999523, -60.22565082124000213, -10.52682217037000001 ) ) ;
#27727 = CARTESIAN_POINT ( 'NONE',  ( 11.03890801094999929, -78.73146484947000090, -5.342433469444999972 ) ) ;
#27728 = CARTESIAN_POINT ( 'NONE',  ( 11.61133755414000035, -76.97808292597399316, 3.999933378912999604 ) ) ;
#27729 = CARTESIAN_POINT ( 'NONE',  ( 12.71536175402335722, -17.87444297183331088, -1.781227265980052099 ) ) ;
#27730 = CARTESIAN_POINT ( 'NONE',  ( 9.267785752250999209, -78.32436279057898787, -6.128505448192000493 ) ) ;
#27731 = CARTESIAN_POINT ( 'NONE',  ( 0.6755009196905999991, -77.00986498579798933, -9.713710972472000549 ) ) ;
#27732 = CARTESIAN_POINT ( 'NONE',  ( -8.421892176740767511, -77.11363408704187350, -8.655124593329036387 ) ) ;
#27733 = CARTESIAN_POINT ( 'NONE',  ( 10.49311453041000064, -79.97125767581903233, -3.963918880051000126 ) ) ;
#27734 = EDGE_LOOP ( 'NONE', ( #36718, #34813, #48990 ) ) ;
#27735 = DIRECTION ( 'NONE',  ( 0.000000000000000000, 1.000000000000000000, 0.000000000000000000 ) ) ;
#27736 = CARTESIAN_POINT ( 'NONE',  ( -0.2566745418018999692, -79.91018296954999300, 1.326684981396999863 ) ) ;
#27737 = CARTESIAN_POINT ( 'NONE',  ( 7.624341766639000539, -23.26485146254000114, 10.42531125024000005 ) ) ;
#27738 = CARTESIAN_POINT ( 'NONE',  ( 0.6295237254636211199, -82.83333333333334281, 1.092232985442824322 ) ) ;
#27739 = CARTESIAN_POINT ( 'NONE',  ( 7.685661446562000343, -76.94999999999998863, -5.583959896778000420 ) ) ;
#27740 = CARTESIAN_POINT ( 'NONE',  ( 9.505630310840999186, -77.70619656188999613, -7.405319984134000499 ) ) ;
#27741 = CARTESIAN_POINT ( 'NONE',  ( -1.944889849486000077, -77.31575641046499925, -9.432423272878001086 ) ) ;
#27742 = CARTESIAN_POINT ( 'NONE',  ( 4.496626815610547112, -76.04321716337622661, 10.85519476661798777 ) ) ;
#27743 = CARTESIAN_POINT ( 'NONE',  ( -5.182070223403000497, -78.87277635977000045, 9.738987759633999985 ) ) ;
#27744 = CARTESIAN_POINT ( 'NONE',  ( 3.308356911591979088, -85.80681307385599155, -1.472975398279045667 ) ) ;
#27745 = ORIENTED_EDGE ( 'NONE', *, *, #12032, .F. ) ;
#27746 = EDGE_CURVE ( 'NONE', #51020, #49432, #32833, .T. ) ;
#27747 = DIRECTION ( 'NONE',  ( -0.2425356250363094601, 0.9701425001453377606, -4.828653421726189663E-10 ) ) ;
#27748 = B_SPLINE_CURVE_WITH_KNOTS ( 'NONE', 3,
 ( #47693, #47402, #39666, #11664, #16951, #52395, #34932, #8087, #29640, #17228, #2802, #21085, #56529, #24937, #35218, #38801, #11376, #52965 ),
 .UNSPECIFIED., .F., .F.,
 ( 4, 2, 2, 2, 2, 2, 2, 2, 4 ),
 ( 0.000000000000000000, 0.1250000000000000000, 0.2500000000000000000, 0.3750000000000000000, 0.5000000000000000000, 0.6250000000000000000, 0.7500000000000000000, 0.8750000000000000000, 1.000000000000000000 ),
 .UNSPECIFIED. ) ;
#27749 = VECTOR ( 'NONE', #24537, 1000.000000000000000 ) ;
#27750 = CARTESIAN_POINT ( 'NONE',  ( 3.621447497675000182, -78.40681307385639798, -1.355252715606880543E-15 ) ) ;
#27751 = EDGE_CURVE ( 'NONE', #38434, #13166, #26758, .T. ) ;
#27752 = CARTESIAN_POINT ( 'NONE',  ( 6.612939829087000732, -79.81399600109497783, 8.759739992124000452 ) ) ;
#27753 = CARTESIAN_POINT ( 'NONE',  ( -6.760013919724072728, -79.17291666666666572, -8.796335266379973206 ) ) ;
#27754 = CARTESIAN_POINT ( 'NONE',  ( 12.42265170273000052, -76.11431842486598498, -1.425377385046999956 ) ) ;
#27755 = CARTESIAN_POINT ( 'NONE',  ( -12.50000000000000000, -39.30476012429000576, 0.000000000000000000 ) ) ;
#27756 = CARTESIAN_POINT ( 'NONE',  ( 9.029856014872001069, -16.66737842935999936, -9.038878718683999836 ) ) ;
#27757 = CARTESIAN_POINT ( 'NONE',  ( -8.096452064242996016, -59.58578169018998949, -13.15643568217000769 ) ) ;
#27758 = B_SPLINE_CURVE_WITH_KNOTS ( 'NONE', 3,
 ( #46273, #32938, #37085, #41233, #46565, #11126, #6089, #27929 ),
 .UNSPECIFIED., .F., .F.,
 ( 4, 2, 2, 4 ),
 ( 0.000000000000000000, 0.5000000000000000000, 0.7500000000000000000, 1.000000000000000000 ),
 .UNSPECIFIED. ) ;
#27759 = ORIENTED_EDGE ( 'NONE', *, *, #9040, .F. ) ;
#27760 = CARTESIAN_POINT ( 'NONE',  ( -0.2704138798119000153, -79.08579419080099626, 11.14367429999999892 ) ) ;
#27761 = CARTESIAN_POINT ( 'NONE',  ( 12.72924182828753636, -55.02450359957972381, 1.930521792060713837 ) ) ;
#27762 = CARTESIAN_POINT ( 'NONE',  ( -11.66814978394733338, -79.56040689563938884, -1.554668868100800738 ) ) ;
#27763 = CARTESIAN_POINT ( 'NONE',  ( -3.484880022881380768, -78.48547957940618858, -0.06569640715844060619 ) ) ;
#27765 = CARTESIAN_POINT ( 'NONE',  ( -0.7940971814358512848, -81.53031153321056479, 0.9681523155726415863 ) ) ;
#27764 = CARTESIAN_POINT ( 'NONE',  ( -0.8130050274896999385, -80.73022382557400078, -1.038954733251000073 ) ) ;
#27766 = EDGE_CURVE ( 'NONE', #33521, #35763, #50293, .T. ) ;
#27767 = CARTESIAN_POINT ( 'NONE',  ( -9.569149049473001156, -79.26527887665599792, 5.523520626929999899 ) ) ;
#27768 = CARTESIAN_POINT ( 'NONE',  ( -9.218146263507760452, -77.00000000000000000, -1.688195841058859559 ) ) ;
#27769 = CARTESIAN_POINT ( 'NONE',  ( -8.872949060675491495, -16.98989818440328392, -8.813905828572767831 ) ) ;
#27770 = CARTESIAN_POINT ( 'NONE',  ( -1.500000000000000222, -81.01041666666667140, -0.1963495408493622085 ) ) ;
#27771 = CARTESIAN_POINT ( 'NONE',  ( 9.249999999999998224, -79.76041666666667140, 1.210822168571084934 ) ) ;
#27772 = CARTESIAN_POINT ( 'NONE',  ( -6.405151242761908392, -78.87468806584735148, 8.913016123664291968 ) ) ;
#27773 = DIRECTION ( 'NONE',  ( 1.000000000000000000, 0.000000000000000000, 0.000000000000000000 ) ) ;
#27774 = ORIENTED_EDGE ( 'NONE', *, *, #7357, .T. ) ;
#27775 = ORIENTED_EDGE ( 'NONE', *, *, #47199, .T. ) ;
#27776 = CARTESIAN_POINT ( 'NONE',  ( -3.133069020688000084, -78.97903998579799634, -9.520158728599000142 ) ) ;
#27777 = CARTESIAN_POINT ( 'NONE',  ( 7.708894260666084186, -78.78865531770708230, -7.492582358052589875 ) ) ;
#27778 = ORIENTED_EDGE ( 'NONE', *, *, #204, .T. ) ;
#27779 = DIRECTION ( 'NONE',  ( -1.000000000000000000, 0.000000000000000000, 0.000000000000000000 ) ) ;
#27780 = CARTESIAN_POINT ( 'NONE',  ( -0.8140818358313716141, -83.51770834709049041, -3.346713179724626563 ) ) ;
#27781 = CARTESIAN_POINT ( 'NONE',  ( 7.633403016722000167, -60.18650073818000124, 10.18126993295000027 ) ) ;
#27782 = CARTESIAN_POINT ( 'NONE',  ( 4.543288497605388443, -76.89401257029606995, 11.32213107881294789 ) ) ;
#27783 = CARTESIAN_POINT ( 'NONE',  ( 4.458804082352973097, -77.39455547813037128, 11.11931012016017917 ) ) ;
#27784 = CARTESIAN_POINT ( 'NONE',  ( 10.58946819037999987, -78.48936414991298705, -3.698823201301000285 ) ) ;
#27785 = CARTESIAN_POINT ( 'NONE',  ( 2.475061660928486784, -81.00000000000001421, 10.54437239986970809 ) ) ;
#27786 = VECTOR ( 'NONE', #42284, 1000.000000000000000 ) ;
#27787 = VERTEX_POINT ( 'NONE', #723 ) ;
#27788 = ORIENTED_EDGE ( 'NONE', *, *, #27870, .F. ) ;
#27789 = CARTESIAN_POINT ( 'NONE',  ( 8.894028069796958036, -77.37240033373954873, 2.560412268026674987 ) ) ;
#27790 = CARTESIAN_POINT ( 'NONE',  ( 5.341789944771999643, -77.76496072214499122, 9.661750877468000098 ) ) ;
#27791 = AXIS2_PLACEMENT_3D ( 'NONE', #25681, #11829, #43707 ) ;
#27792 = DIRECTION ( 'NONE',  ( 0.000000000000000000, -1.000000000000000000, 0.000000000000000000 ) ) ;
#27793 = EDGE_CURVE ( 'NONE', #15664, #21408, #38807, .T. ) ;
#27794 = CARTESIAN_POINT ( 'NONE',  ( 0.8292593438864999111, -77.65986211677478934, -1.385477418387000004 ) ) ;
#27795 = CARTESIAN_POINT ( 'NONE',  ( 1.570796326794910547, -77.53541666666666288, -11.99999999999999822 ) ) ;
#27796 = CARTESIAN_POINT ( 'NONE',  ( -7.374560639698973574, -78.47291666666666288, -9.596002108778167283 ) ) ;
#27797 = CARTESIAN_POINT ( 'NONE',  ( -1.472167250137000005, -78.80543922203000307, -0.6938203229310999642 ) ) ;
#27798 = FACE_BOUND ( 'NONE', #44131, .T. ) ;
#27799 = CARTESIAN_POINT ( 'NONE',  ( -6.999846649096999940, -79.35943504075699195, 8.407732347380999727 ) ) ;
#27800 = CARTESIAN_POINT ( 'NONE',  ( 1.931086388578000079, -60.09778754156999980, -12.71798269388000158 ) ) ;
#27801 = CARTESIAN_POINT ( 'NONE',  ( -7.434020715870205187, -60.31691643837059758, 8.107762507646519623 ) ) ;
#27802 = CARTESIAN_POINT ( 'NONE',  ( 1.077770122336999981, -83.59225696173399456, -3.376889499103000070 ) ) ;
#27803 = ORIENTED_EDGE ( 'NONE', *, *, #20840, .T. ) ;
#27804 = CARTESIAN_POINT ( 'NONE',  ( -11.90098819343999992, -79.02652905684600171, -2.686189377354999852 ) ) ;
#27805 = CARTESIAN_POINT ( 'NONE',  ( -10.47968562137999982, -76.74722307105399466, 4.029083465249000184 ) ) ;
#27806 = CARTESIAN_POINT ( 'NONE',  ( 10.45204020799386946, -77.86881889335130325, 2.513295852507721584 ) ) ;
#27807 = CARTESIAN_POINT ( 'NONE',  ( -10.61596739836999959, -78.67223608445800664, -5.551333230057999835 ) ) ;
#27808 = CARTESIAN_POINT ( 'NONE',  ( -1.997276839918484148, -3.427083333333333925, 2.598917237794077018 ) ) ;
#27810 = DIRECTION ( 'NONE',  ( 1.000000000000000000, 0.000000000000000000, 0.000000000000000000 ) ) ;
#27809 = CARTESIAN_POINT ( 'NONE',  ( 11.75000000000000000, -78.54999999999999716, 0.000000000000000000 ) ) ;
#27811 = CARTESIAN_POINT ( 'NONE',  ( 1.001315001700999963, -54.11477588220000001, 12.50000000000000000 ) ) ;
#27812 = CARTESIAN_POINT ( 'NONE',  ( -2.117690490098999678, -77.47224322018799114, 9.172054377053999730 ) ) ;
#27813 = CARTESIAN_POINT ( 'NONE',  ( 0.3402453830697489967, -86.07390000031791999, -7.595013698426734017 ) ) ;
#27814 = CARTESIAN_POINT ( 'NONE',  ( 5.230327773973000305, -78.05500231115298959, -9.843691987646998598 ) ) ;
#27815 = CARTESIAN_POINT ( 'NONE',  ( -4.885220488697999741, -76.55755186839822102, 11.26753068192000029 ) ) ;
#27816 = CARTESIAN_POINT ( 'NONE',  ( -10.23652643648999927, -80.92341969070069752, -4.396672205467000438 ) ) ;
#27817 = ORIENTED_EDGE ( 'NONE', *, *, #18492, .F. ) ;
#27818 = ADVANCED_FACE ( 'NONE', ( #54998 ), #14547, .T. ) ;
#27819 = CARTESIAN_POINT ( 'NONE',  ( -1.269916711065999904, -77.26432403538302651, -9.409822520238998678 ) ) ;
#27820 = CARTESIAN_POINT ( 'NONE',  ( -1.322675138774000114, -1.903566864579000040, -3.739459546867000217 ) ) ;
#27821 = EDGE_CURVE ( 'NONE', #14217, #36091, #52040, .T. ) ;
#27822 = CARTESIAN_POINT ( 'NONE',  ( -10.96060824219999930, -77.18127443839999557, 2.383941600041999731 ) ) ;
#27823 = CARTESIAN_POINT ( 'NONE',  ( -0.5193979750644999172, -78.93077836576598827, -10.96331347381999954 ) ) ;
#27824 = CARTESIAN_POINT ( 'NONE',  ( 8.260136572111999698, -24.94034376567000066, -9.643347111174000119 ) ) ;
#27825 = CARTESIAN_POINT ( 'NONE',  ( 0.000000000000000000, -75.67500000000001137, 0.000000000000000000 ) ) ;
#27826 = CARTESIAN_POINT ( 'NONE',  ( 3.250000000000000000, -1.350000000000000089, 0.000000000000000000 ) ) ;
#27827 = LINE ( 'NONE', #1875, #14379 ) ;
#27828 = CARTESIAN_POINT ( 'NONE',  ( -4.136990165604000680, -84.71217953870899464, -0.5402383595598000410 ) ) ;
#27829 = CARTESIAN_POINT ( 'NONE',  ( 0.9218200799623694763, -80.32291666666667140, 1.199500263597272465 ) ) ;
#27830 = DIRECTION ( 'NONE',  ( -1.000000000000000000, 0.000000000000000000, 0.000000000000000000 ) ) ;
#27831 = AXIS2_PLACEMENT_3D ( 'NONE', #35367, #16811, #44538 ) ;
#27832 = EDGE_CURVE ( 'NONE', #29780, #42095, #11023, .T. ) ;
#27833 = DIRECTION ( 'NONE',  ( 0.000000000000000000, 1.000000000000000000, 0.000000000000000000 ) ) ;
#27834 = CARTESIAN_POINT ( 'NONE',  ( -0.4240539849974000464, -80.16587349533999429, 1.611036072322000079 ) ) ;
#27835 = CARTESIAN_POINT ( 'NONE',  ( -1.265859449240000156, -77.99707259131000114, 0.3747096735211999929 ) ) ;
#27836 = CIRCLE ( 'NONE', #23131, 13.89999999999999858 ) ;
#27837 = FACE_OUTER_BOUND ( 'NONE', #42694, .T. ) ;
#27838 = CARTESIAN_POINT ( 'NONE',  ( 0.8891700687157699790, -82.07588638577088602, 1.268013924794865188 ) ) ;
#27839 = CARTESIAN_POINT ( 'NONE',  ( 1.510174625183769548, -83.09633900652015370, -0.05656285966305413943 ) ) ;
#27840 = CARTESIAN_POINT ( 'NONE',  ( -9.719853332338134422, -80.13579794343719698, -4.669139681347004078 ) ) ;
#27841 = DIRECTION ( 'NONE',  ( 0.000000000000000000, 0.000000000000000000, -1.000000000000000000 ) ) ;
#27842 = ORIENTED_EDGE ( 'NONE', *, *, #58074, .T. ) ;
#27843 = CARTESIAN_POINT ( 'NONE',  ( -1.095039581810170581, -81.64041251720371406, -0.6026378644521110939 ) ) ;
#27844 = DIRECTION ( 'NONE',  ( 0.000000000000000000, 0.000000000000000000, 1.000000000000000000 ) ) ;
#27845 = CARTESIAN_POINT ( 'NONE',  ( 1.081678475801000072, -79.82604836483349686, 10.97869327635999781 ) ) ;
#27846 = FACE_OUTER_BOUND ( 'NONE', #11046, .T. ) ;
#27847 = ORIENTED_EDGE ( 'NONE', *, *, #21236, .T. ) ;
#27848 = EDGE_LOOP ( 'NONE', ( #8836, #32129, #46265, #33662 ) ) ;
#27849 = CARTESIAN_POINT ( 'NONE',  ( -0.9913219194069000650, -81.11560668392900197, -1.147267625202000207 ) ) ;
#27850 = VERTEX_POINT ( 'NONE', #11304 ) ;
#27851 = CARTESIAN_POINT ( 'NONE',  ( 0.000000000000000000, -80.69999999999998863, 0.000000000000000000 ) ) ;
#27852 = ORIENTED_EDGE ( 'NONE', *, *, #18338, .F. ) ;
#27853 = DIRECTION ( 'NONE',  ( -0.7071067811865475727, 0.000000000000000000, 0.7071067811865475727 ) ) ;
#27854 = CARTESIAN_POINT ( 'NONE',  ( 0.000000000000000000, 4.040000000000000036, 0.000000000000000000 ) ) ;
#27855 = CARTESIAN_POINT ( 'NONE',  ( -1.621160707165126613, -81.95677081782697826, -3.000586557583472480 ) ) ;
#27856 = CARTESIAN_POINT ( 'NONE',  ( 9.596002108778172612, -76.49791666665605305, -7.374560639698962028 ) ) ;
#27857 = CARTESIAN_POINT ( 'NONE',  ( 2.095844585997434173, -78.24334418708741623, -9.009563528218526685 ) ) ;
#27858 = LINE ( 'NONE', #41160, #52063 ) ;
#27859 = ORIENTED_EDGE ( 'NONE', *, *, #44633, .F. ) ;
#27860 = ORIENTED_EDGE ( 'NONE', *, *, #42023, .F. ) ;
#27861 = LINE ( 'NONE', #472, #21577 ) ;
#27862 = CARTESIAN_POINT ( 'NONE',  ( -1.750000000000000000, -60.04999999725999515, -12.50000000000000000 ) ) ;
#27863 = EDGE_CURVE ( 'NONE', #56311, #34611, #47913, .T. ) ;
#27864 = CARTESIAN_POINT ( 'NONE',  ( 1.980610890454856055, -60.32073889451354631, -12.74374574609741018 ) ) ;
#27865 = CARTESIAN_POINT ( 'NONE',  ( -0.5548610165507998904, -77.89029600155998878, -9.688283574444998436 ) ) ;
#27866 = CARTESIAN_POINT ( 'NONE',  ( 10.42531124908000173, -60.06485148440999922, 7.624341765471999821 ) ) ;
#27867 = CARTESIAN_POINT ( 'NONE',  ( 2.372446516949769268, -85.88464632347285033, 3.106461528215548107 ) ) ;
#27868 =( BOUNDED_SURFACE ( )  B_SPLINE_SURFACE ( 3, 3, ( 
 ( #54258, #28239, #14090, #13791 ),
 ( #37106, #18825, #54835, #23532 ),
 ( #10854, #56582, #47744, #15559 ),
 ( #52162, #38276, #56008, #56874 ),
 ( #16431, #7277, #20850, #47463 ),
 ( #25279, #24991, #6403, #43011 ),
 ( #47169, #34414, #11430, #38854 ) ),
 .UNSPECIFIED., .F., .F., .F. ) 
 B_SPLINE_SURFACE_WITH_KNOTS ( ( 4, 3, 4 ),
 ( 4, 4 ),
 ( 0.000000000000000000, 1.000000000000000000, 2.000000000000000000 ),
 ( 0.000000000000000000, 1.000000000000000000 ),
 .UNSPECIFIED. ) 
 GEOMETRIC_REPRESENTATION_ITEM ( )  RATIONAL_B_SPLINE_SURFACE ( (
 ( 1.196373642248999891, 1.184225762575999985, 1.184225762575999985, 1.196373642248999891),
 ( 0.9447739570234999773, 0.9351807998836999536, 0.9351807998836999536, 0.9447739570234999773),
 ( 0.9447739570234999773, 0.9351807998836999536, 0.9351807998836999536, 0.9447739570234999773),
 ( 1.196373642248999891, 1.184225762575999985, 1.184225762575999985, 1.196373642248999891),
 ( 0.9447739570234999773, 0.9351807998836999536, 0.9351807998836999536, 0.9447739570234999773),
 ( 0.9447739570234999773, 0.9351807998836999536, 0.9351807998836999536, 0.9447739570234999773),
 ( 1.196373642248999891, 1.184225762575999985, 1.184225762575999985, 1.196373642248999891) ) ) 
 REPRESENTATION_ITEM ( '' )  SURFACE ( )  );
#27869 = CARTESIAN_POINT ( 'NONE',  ( 11.80688451001000061, -77.70231164849001004, 5.334804138346999736 ) ) ;
#27870 = EDGE_CURVE ( 'NONE', #3967, #6729, #54297, .T. ) ;
#27871 = CARTESIAN_POINT ( 'NONE',  ( -0.4670233199325999895, -80.54409703377000085, 1.392241846115000126 ) ) ;
#27872 = AXIS2_PLACEMENT_3D ( 'NONE', #55275, #42294, #32527 ) ;
#27873 = CARTESIAN_POINT ( 'NONE',  ( -12.80896991324000034, -21.75453807238000081, -1.930989179114000143 ) ) ;
#27874 = DIRECTION ( 'NONE',  ( 1.000000000000000000, 0.000000000000000000, 0.000000000000000000 ) ) ;
#27875 = CARTESIAN_POINT ( 'NONE',  ( -1.151447527804999815, -81.37919147407698972, 4.010516339146000142 ) ) ;
#27876 = CARTESIAN_POINT ( 'NONE',  ( -4.454457568640999732, -80.67345514424359010, 10.34731867136000005 ) ) ;
#27877 = CARTESIAN_POINT ( 'NONE',  ( 9.797588846018999931, -78.75818667140099194, 0.1600704101387999956 ) ) ;
#27878 = FACE_BOUND ( 'NONE', #54109, .T. ) ;
#27879 = CARTESIAN_POINT ( 'NONE',  ( 2.185995097243000007, -82.25232046129099217, -2.793946140691999869 ) ) ;
#27880 = AXIS2_PLACEMENT_3D ( 'NONE', #9828, #10122, #27810 ) ;
#27881 = CARTESIAN_POINT ( 'NONE',  ( 0.6284244718204999858, -78.42970690854529892, -1.176290284212999859 ) ) ;
#27882 = DIRECTION ( 'NONE',  ( -9.562128866322998892E-12, 1.000000000000000000, -3.007558296593999951E-10 ) ) ;
#27883 = CARTESIAN_POINT ( 'NONE',  ( 10.44683666364205266, -79.24999999999997158, 6.036782290497776593 ) ) ;
#27884 = CARTESIAN_POINT ( 'NONE',  ( 5.066607476199531668, -77.20000000000000284, -9.683877171469156053 ) ) ;
#27885 = EDGE_LOOP ( 'NONE', ( #27456, #19660, #30712, #35718 ) ) ;
#27886 = CARTESIAN_POINT ( 'NONE',  ( -4.801183948427951265, -78.89166666666666572, -10.79468190471831690 ) ) ;
#27887 = CARTESIAN_POINT ( 'NONE',  ( -7.515954563004000555, -78.18872553980699536, -8.614663944174999699 ) ) ;
#27888 = PLANE ( 'NONE',  #39257 ) ;
#27889 = B_SPLINE_CURVE_WITH_KNOTS ( 'NONE', 3,
 ( #21604, #39608, #31311, #34878, #23571, #12738 ),
 .UNSPECIFIED., .F., .F.,
 ( 4, 2, 4 ),
 ( 0.000000000000000000, 0.5000000000000000000, 1.000000000000000000 ),
 .UNSPECIFIED. ) ;
#27890 = EDGE_CURVE ( 'NONE', #20252, #20752, #43464, .T. ) ;
#27891 = CARTESIAN_POINT ( 'NONE',  ( -9.738223894236998746, -79.32504842320498994, 0.5068368411314999600 ) ) ;
#27892 = CARTESIAN_POINT ( 'NONE',  ( -3.201433918554999813, -77.84278050555001016, 12.61309089657999927 ) ) ;
#27893 = CARTESIAN_POINT ( 'NONE',  ( 5.512944058422025506, -79.43216301949462377, 9.240081554467723279 ) ) ;
#27894 = CARTESIAN_POINT ( 'NONE',  ( 1.918320629100999763, -79.51993998579798983, -9.660030828008999038 ) ) ;
#27895 = CARTESIAN_POINT ( 'NONE',  ( 9.532736212859026281, -78.49731003545609553, 6.867370139290200015 ) ) ;
#27896 = DIRECTION ( 'NONE',  ( 0.000000000000000000, 0.000000000000000000, -1.000000000000000000 ) ) ;
#27897 = CARTESIAN_POINT ( 'NONE',  ( 2.991086974322999747, -77.38964371959498578, -10.75725820134999999 ) ) ;
#27898 = ADVANCED_FACE ( 'NONE', ( #2446 ), #35125, .F. ) ;
#27899 = CARTESIAN_POINT ( 'NONE',  ( 0.5145135761085000148, -82.00542612764600392, -1.415689478406999990 ) ) ;
#27900 = DIRECTION ( 'NONE',  ( 1.000000000000000000, 0.000000000000000000, 0.000000000000000000 ) ) ;
#27901 = CARTESIAN_POINT ( 'NONE',  ( 1.442464609972999856, -77.65805598037698587, -9.302176701096998457 ) ) ;
#27902 = EDGE_CURVE ( 'NONE', #28197, #7888, #14760, .T. ) ;
#27904 = CARTESIAN_POINT ( 'NONE',  ( 2.028166799595999770, -0.9151276875359000140, -3.466423845304999585 ) ) ;
#27903 = CARTESIAN_POINT ( 'NONE',  ( -3.978352630842000082, -86.11751568233700027, 0.4347780226346000254 ) ) ;
#27905 = CARTESIAN_POINT ( 'NONE',  ( 8.150225256662000817, -79.78074805011499393, -4.374508917085999649 ) ) ;
#27906 = CARTESIAN_POINT ( 'NONE',  ( 0.3271848554491016414, -82.64583333333331439, -1.217465845835393967 ) ) ;
#27907 = CARTESIAN_POINT ( 'NONE',  ( -1.250000000000000000, -23.25000000000000000, 12.00000000000000000 ) ) ;
#27908 = DIRECTION ( 'NONE',  ( 0.000000000000000000, -1.000000000000000000, -2.483745111066999960E-13 ) ) ;
#27909 = VERTEX_POINT ( 'NONE', #14474 ) ;
#27910 = EDGE_LOOP ( 'NONE', ( #9587, #13711, #53044, #21539 ) ) ;
#27911 = CARTESIAN_POINT ( 'NONE',  ( 3.714552462503000196, -79.55170192472400004, 11.44155784250999908 ) ) ;
#27912 = CARTESIAN_POINT ( 'NONE',  ( -3.093366010725773219, -76.11510416600961548, -11.50726245973735473 ) ) ;
#27913 = CARTESIAN_POINT ( 'NONE',  ( -6.000000002940000243, -81.20000000293998710, 1.734976710454000070E-08 ) ) ;
#27914 = ORIENTED_EDGE ( 'NONE', *, *, #47501, .T. ) ;
#27915 = FACE_OUTER_BOUND ( 'NONE', #45081, .T. ) ;
#27916 = ORIENTED_EDGE ( 'NONE', *, *, #51695, .T. ) ;
#27917 = CIRCLE ( 'NONE', #18504, 2.799999999999999822 ) ;
#27918 = ORIENTED_EDGE ( 'NONE', *, *, #35705, .T. ) ;
#27919 = CARTESIAN_POINT ( 'NONE',  ( -1.423977246384270590, -2.689414678050281893, -2.927659162848880392 ) ) ;
#27920 = EDGE_CURVE ( 'NONE', #22076, #12674, #40907, .T. ) ;
#27921 = ORIENTED_EDGE ( 'NONE', *, *, #4777, .T. ) ;
#27922 = AXIS2_PLACEMENT_3D ( 'NONE', #5332, #359, #31594 ) ;
#27923 = CARTESIAN_POINT ( 'NONE',  ( 3.383438022436999759, -82.45517979992798985, 0.3412945533484999516 ) ) ;
#27924 = DIRECTION ( 'NONE',  ( 0.000000000000000000, 0.000000000000000000, -1.000000000000000000 ) ) ;
#27925 = ORIENTED_EDGE ( 'NONE', *, *, #11634, .T. ) ;
#27926 = CARTESIAN_POINT ( 'NONE',  ( 0.000000000000000000, -2.660000000000000142, 0.000000000000000000 ) ) ;
#27927 = AXIS2_PLACEMENT_3D ( 'NONE', #31272, #44887, #53155 ) ;
#27928 = ORIENTED_EDGE ( 'NONE', *, *, #27076, .F. ) ;
#27929 = CARTESIAN_POINT ( 'NONE',  ( 1.750000000001000089, -18.75000001325000198, 12.56594318051000059 ) ) ;
#27930 = CARTESIAN_POINT ( 'NONE',  ( 4.187011524236304183, -78.51040584207294160, -8.754585214959869077 ) ) ;
#27931 = CARTESIAN_POINT ( 'NONE',  ( -0.03763201836869552869, -78.77851881763731967, -3.992727109996482060 ) ) ;
#27932 = EDGE_CURVE ( 'NONE', #26558, #46040, #5650, .T. ) ;
#27933 = CARTESIAN_POINT ( 'NONE',  ( -1.484271920566999698E-14, -80.79999999999999716, 0.000000000000000000 ) ) ;
#27934 = CARTESIAN_POINT ( 'NONE',  ( -12.99510751537000353, -15.69705297113999443, 6.911973076623003642 ) ) ;
#27935 = CARTESIAN_POINT ( 'NONE',  ( -9.939389728518001732, -76.72821088380000276, 5.126617716248000001 ) ) ;
#27936 = CARTESIAN_POINT ( 'NONE',  ( 11.75000000000000000, -77.04999999999999716, 0.000000000000000000 ) ) ;
#27937 = EDGE_CURVE ( 'NONE', #47434, #23068, #40151, .T. ) ;
#27938 = CARTESIAN_POINT ( 'NONE',  ( -8.108261698375999416, -76.38420349199300574, -7.767871074888999416 ) ) ;
#27939 = CARTESIAN_POINT ( 'NONE',  ( 7.695212739268346702, -78.80320820975849472, -5.132832367546954266 ) ) ;
#27940 = CARTESIAN_POINT ( 'NONE',  ( 2.740029395673595047, -76.55575388350786170, 11.42608732962110984 ) ) ;
#27941 = CARTESIAN_POINT ( 'NONE',  ( 8.813612208106999191, -77.78773667140100656, 3.598911935278999774 ) ) ;
#27942 = CARTESIAN_POINT ( 'NONE',  ( 0.2020314717676000016, -80.27144072411900311, -1.318241039644999946 ) ) ;
#27943 = CARTESIAN_POINT ( 'NONE',  ( -9.548515496062343288, -80.14175696964518636, -5.470885215208376451 ) ) ;
#27944 = CARTESIAN_POINT ( 'NONE',  ( 10.65674263929012788, -78.16410729663259360, -5.672678603144905018 ) ) ;
#27945 = CARTESIAN_POINT ( 'NONE',  ( 4.074498828648000170, -80.72242549782599497, -0.6759902392087999701 ) ) ;
#27946 = DIRECTION ( 'NONE',  ( 0.000000000000000000, -1.000000000000000000, 0.000000000000000000 ) ) ;
#27947 = CARTESIAN_POINT ( 'NONE',  ( -2.810647185591240049, -76.29609374999736815, 11.70020478678804565 ) ) ;
#27948 = CARTESIAN_POINT ( 'NONE',  ( 2.813789756862274505, -79.64583333333330017, -10.47020627418438821 ) ) ;
#27949 = CARTESIAN_POINT ( 'NONE',  ( 0.7491852396053489960, -77.03125000000001421, -9.499759410111733970 ) ) ;
#27950 = LINE ( 'NONE', #41546, #30784 ) ;
#27951 = CARTESIAN_POINT ( 'NONE',  ( -12.00000000000000000, -79.39999999999999147, 0.000000000000000000 ) ) ;
#27952 = CARTESIAN_POINT ( 'NONE',  ( -10.36289662403999756, -60.00106470408999826, -7.633500902345000227 ) ) ;
#27953 = CARTESIAN_POINT ( 'NONE',  ( 12.70556836322084315, -25.22772277445464439, -0.2597962961525307479 ) ) ;
#27954 = CARTESIAN_POINT ( 'NONE',  ( -1.667260628941999778, -23.20942012473999938, -12.49858003894999925 ) ) ;
#27955 = CARTESIAN_POINT ( 'NONE',  ( 13.86363636363000218, -69.16102867818000277, 1.277888278513000037E-05 ) ) ;
#27956 = CARTESIAN_POINT ( 'NONE',  ( -2.239251858213000101, -3.482118084780000178, 2.225821419444999893 ) ) ;
#27957 = CARTESIAN_POINT ( 'NONE',  ( -7.770369683894697843, -24.23583903337609158, -10.20674856003130948 ) ) ;
#27958 = CARTESIAN_POINT ( 'NONE',  ( 1.250000000000000000, -80.74999999999998579, 0.000000000000000000 ) ) ;
#27959 = AXIS2_PLACEMENT_3D ( 'NONE', #16229, #20370, #41934 ) ;
#27960 = CARTESIAN_POINT ( 'NONE',  ( -9.014397739498770434, -77.40433534373462976, 5.897194292687825801 ) ) ;
#27961 = LINE ( 'NONE', #46011, #37323 ) ;
#27963 = CARTESIAN_POINT ( 'NONE',  ( 9.694840914897000062, -79.56117174695758365, -5.145296513660000848 ) ) ;
#27962 = DIRECTION ( 'NONE',  ( 0.000000000000000000, 1.000000000000000000, 0.000000000000000000 ) ) ;
#27964 = CARTESIAN_POINT ( 'NONE',  ( 3.752244608269999837, -75.81839300465999543, -11.62132640531999961 ) ) ;
#27965 = ORIENTED_EDGE ( 'NONE', *, *, #24845, .F. ) ;
#27966 = AXIS2_PLACEMENT_3D ( 'NONE', #13275, #17135, #1194 ) ;
#27967 = CARTESIAN_POINT ( 'NONE',  ( 3.086375682183999825, -85.62924735065199400, 1.743343585014999864 ) ) ;
#27968 = CARTESIAN_POINT ( 'NONE',  ( 6.901085230909000501, -80.95330344751930340, -9.080895641036999422 ) ) ;
#27969 = AXIS2_PLACEMENT_3D ( 'NONE', #53598, #46516, #1061 ) ;
#27970 = CARTESIAN_POINT ( 'NONE',  ( 8.587978511495325762, -78.31970074046702734, -3.439774535247742904 ) ) ;
#27971 = CARTESIAN_POINT ( 'NONE',  ( 7.610436392395274474, -55.27459049260378521, 10.41144384036934056 ) ) ;
#27972 = CARTESIAN_POINT ( 'NONE',  ( 11.01642476345000077, -77.16674935421400505, 2.111041454437999842 ) ) ;
#27973 = CARTESIAN_POINT ( 'NONE',  ( 12.56594317823000040, -23.25000001387000026, -1.750000000000000000 ) ) ;
#27974 = CARTESIAN_POINT ( 'NONE',  ( 9.296715471869999803, -79.12203893003398036, -2.514846541900999988 ) ) ;
#27975 = VECTOR ( 'NONE', #30030, 1000.000000000000000 ) ;
#27976 = CARTESIAN_POINT ( 'NONE',  ( -2.473380543883999749, -1.377984372333000085, -3.177361517278999958 ) ) ;
#27977 = CARTESIAN_POINT ( 'NONE',  ( 9.249483092228999226, -78.85084128437098627, 0.09778817195952001218 ) ) ;
#27978 = CARTESIAN_POINT ( 'NONE',  ( 8.225372035788822700, -81.00000000000000000, -7.395153854250120062 ) ) ;
#27979 = VERTEX_POINT ( 'NONE', #1796 ) ;
#27980 = DIRECTION ( 'NONE',  ( 0.000000000000000000, -1.000000000000000000, 0.000000000000000000 ) ) ;
#27981 = CARTESIAN_POINT ( 'NONE',  ( 8.200000000000001066, -80.99999999999998579, 0.000000000000000000 ) ) ;
#27982 = CARTESIAN_POINT ( 'NONE',  ( 6.121779332999000900, -79.43668667140099160, -7.438015166080000462 ) ) ;
#27983 = DIRECTION ( 'NONE',  ( 1.000000000000000000, 0.000000000000000000, 0.000000000000000000 ) ) ;
#27984 = EDGE_LOOP ( 'NONE', ( #44638, #54990, #46773, #25579 ) ) ;
#27985 = CARTESIAN_POINT ( 'NONE',  ( -12.60552522433000000, -55.51082434643999619, -1.799501877760999902 ) ) ;
#27986 = CARTESIAN_POINT ( 'NONE',  ( 8.768124086712999699, -55.64999999965999677, 7.919595949288999570 ) ) ;
#27987 = ORIENTED_EDGE ( 'NONE', *, *, #48162, .T. ) ;
#27988 = CARTESIAN_POINT ( 'NONE',  ( 4.023394881099000564, -78.67502719647299614, 11.60207191892000012 ) ) ;
#27989 = CARTESIAN_POINT ( 'NONE',  ( -9.676120737181999942, -77.95091993224397697, 5.663874116999999764 ) ) ;
#27990 = CARTESIAN_POINT ( 'NONE',  ( -1.667961430005999945, -21.74888345808999901, 12.58335110161999815 ) ) ;
#27991 = VERTEX_POINT ( 'NONE', #51963 ) ;
#27992 = EDGE_CURVE ( 'NONE', #13108, #24608, #24795, .T. ) ;
#27993 = CARTESIAN_POINT ( 'NONE',  ( 8.485281374238999419, -18.75000000000000000, 8.485281374238999419 ) ) ;
#27994 = EDGE_CURVE ( 'NONE', #11369, #17717, #6494, .T. ) ;
#27995 = CARTESIAN_POINT ( 'NONE',  ( -5.726462542197000793, -79.96560161327099081, -7.912542777261000637 ) ) ;
#27996 = ORIENTED_EDGE ( 'NONE', *, *, #14827, .T. ) ;
#27997 = CARTESIAN_POINT ( 'NONE',  ( 12.46083735077000121, -55.11664398755999628, 1.628985986890000071 ) ) ;
#27998 = CARTESIAN_POINT ( 'NONE',  ( 3.535142739574999915, -79.92176962903970150, 10.17871189313000002 ) ) ;
#27999 = CARTESIAN_POINT ( 'NONE',  ( -12.79972228482999874, -23.79021513454000214, -2.019125729023000027 ) ) ;
#28000 = CARTESIAN_POINT ( 'NONE',  ( 9.426477049435000310, -77.37047694988500268, -1.139727483088999849 ) ) ;
#28001 = AXIS2_PLACEMENT_3D ( 'NONE', #48873, #192, #21417 ) ;
#28002 = CARTESIAN_POINT ( 'NONE',  ( -1.152121943227528034, -80.13187642228581353, -0.4845792447579237994 ) ) ;
#28003 = CARTESIAN_POINT ( 'NONE',  ( -7.674614791499999811, -56.04899163905999870, 10.14948852566000070 ) ) ;
#28004 = CIRCLE ( 'NONE', #56188, 10.50000000000000000 ) ;
#28005 = DIRECTION ( 'NONE',  ( -0.9999463328794432337, 0.000000000000000000, 0.01036008498777044214 ) ) ;
#28006 = EDGE_CURVE ( 'NONE', #15123, #46904, #37408, .T. ) ;
#28007 = CARTESIAN_POINT ( 'NONE',  ( 8.976219693957377288, -79.86950217340086056, 2.233771530619390155 ) ) ;
#28008 = AXIS2_PLACEMENT_3D ( 'NONE', #22804, #21634, #39639 ) ;
#28009 = CARTESIAN_POINT ( 'NONE',  ( -1.050373044531177857, -78.78472797553973805, 1.124121219058911159 ) ) ;
#28010 = CARTESIAN_POINT ( 'NONE',  ( 3.813617437220001793, -79.37447915313912006, -1.247836695960566900 ) ) ;
#28011 = ORIENTED_EDGE ( 'NONE', *, *, #34201, .T. ) ;
#28012 = CARTESIAN_POINT ( 'NONE',  ( 5.491552160713999875, -77.07695060022997779, 7.961786551375001686 ) ) ;
#28013 = CARTESIAN_POINT ( 'NONE',  ( -11.91862232004000077, -75.96254709223001100, 3.079279237876999531 ) ) ;
#28014 = CONICAL_SURFACE ( 'NONE', #11070, 1.099999997158000120, 0.7853981633972997312 ) ;
#28015 = CARTESIAN_POINT ( 'NONE',  ( -2.268810067667969221, -2.280055725771751085, 2.689892472967077008 ) ) ;
#28016 = CARTESIAN_POINT ( 'NONE',  ( 7.631896413346999530, -60.02122715173999978, -10.36221694968000051 ) ) ;
#28017 = B_SPLINE_CURVE_WITH_KNOTS ( 'NONE', 3,
 ( #35087, #44260, #53121, #12670, #21817, #9283, #21968, #57697 ),
 .UNSPECIFIED., .F., .F.,
 ( 4, 2, 2, 4 ),
 ( 0.000000000000000000, 0.5000000000000000000, 0.7500000000000000000, 1.000000000000000000 ),
 .UNSPECIFIED. ) ;
#28019 = ADVANCED_FACE ( 'NONE', ( #28630 ), #19793, .T. ) ;
#28018 = CARTESIAN_POINT ( 'NONE',  ( 8.438902753042999194, -78.70272413139998946, -8.898539530003999332 ) ) ;
#28020 = CARTESIAN_POINT ( 'NONE',  ( -11.94395460750000204, -77.04741951094599983, 2.857367593729999822 ) ) ;
#28021 = CARTESIAN_POINT ( 'NONE',  ( 12.70451544424452450, -17.44534321913721797, -1.498804046739477869 ) ) ;
#28022 = CARTESIAN_POINT ( 'NONE',  ( 8.538884422081000736, -78.42736808979898910, 7.349585687664999867 ) ) ;
#28023 = CARTESIAN_POINT ( 'NONE',  ( 2.910828549648142527, -2.813461382813009948, -1.464431053388650650 ) ) ;
#28024 = CARTESIAN_POINT ( 'NONE',  ( 11.32629911350350049, -77.32711347535936852, 4.017011466391305241 ) ) ;
#28025 = CARTESIAN_POINT ( 'NONE',  ( -11.19989528650999944, -78.74562224073753214, 0.6168112860373000661 ) ) ;
#28026 = ADVANCED_FACE ( 'NONE', ( #2661 ), #6200, .F. ) ;
#28027 = ORIENTED_EDGE ( 'NONE', *, *, #11013, .T. ) ;
#28028 = CARTESIAN_POINT ( 'NONE',  ( 0.000000000000000000, -76.14999999999999147, 0.000000000000000000 ) ) ;
#28029 = CARTESIAN_POINT ( 'NONE',  ( -3.845277600207000379, -76.92115273745038451, -8.724914968965999051 ) ) ;
#28030 = CARTESIAN_POINT ( 'NONE',  ( 10.41144098943260055, -23.52546312060280798, 7.610433527965647649 ) ) ;
#28031 = B_SPLINE_CURVE_WITH_KNOTS ( 'NONE', 3,
 ( #50217, #40473, #933, #9765, #49341, #27753, #41351, #18915, #40765, #14473, #5615, #26882, #23626, #41638, #44906, #4462, #22461, #67 ),
 .UNSPECIFIED., .F., .F.,
 ( 4, 2, 2, 2, 2, 2, 2, 2, 4 ),
 ( 0.000000000000000000, 0.1250000000000000000, 0.2500000000000000000, 0.3750000000000000000, 0.5000000000000000000, 0.6250000000000000000, 0.7500000000000000000, 0.8750000000000000000, 1.000000000000000000 ),
 .UNSPECIFIED. ) ;
#28032 = CARTESIAN_POINT ( 'NONE',  ( -5.099999999822000696, -75.20000000017779485, 7.533999751109999828E-10 ) ) ;
#28033 = CARTESIAN_POINT ( 'NONE',  ( 3.018378881891000010, -2.180961001041000102, 2.164217357939999697 ) ) ;
#28034 = CARTESIAN_POINT ( 'NONE',  ( -7.660291894363999710, -78.43868807833099766, 9.301381605274000819 ) ) ;
#28035 = CARTESIAN_POINT ( 'NONE',  ( -3.877711979005999954, -77.79896150565798507, -8.815699619024998768 ) ) ;
#28036 = CARTESIAN_POINT ( 'NONE',  ( 8.622285323087540476, -76.00886100035398840, 7.982628424629189645 ) ) ;
#28037 = CARTESIAN_POINT ( 'NONE',  ( 5.650974246042000715, -78.79106733076498870, 9.474609463724998903 ) ) ;
#28038 = CARTESIAN_POINT ( 'NONE',  ( -0.5301359684281606865, -85.79678895079199208, 4.263478205968141310 ) ) ;
#28039 = ORIENTED_EDGE ( 'NONE', *, *, #53277, .T. ) ;
#28040 = CARTESIAN_POINT ( 'NONE',  ( 8.130813118010999929, -17.31476110167000115, -9.546856411651999608 ) ) ;
#28041 = DIRECTION ( 'NONE',  ( 0.000000000000000000, -1.000000000000000000, 0.000000000000000000 ) ) ;
#28042 = CARTESIAN_POINT ( 'NONE',  ( 7.788493169598000421, -78.80267124511898658, 7.733265204867000087 ) ) ;
#28043 = DIRECTION ( 'NONE',  ( 0.000000000000000000, -1.000000000000000000, 0.000000000000000000 ) ) ;
#28044 = CARTESIAN_POINT ( 'NONE',  ( 11.70294133920999968, -76.15205116317100931, 4.403991283866000472 ) ) ;
#28045 = LINE ( 'NONE', #36911, #44365 ) ;
#28046 = CARTESIAN_POINT ( 'NONE',  ( 10.19019671031999863, -18.80356357339999818, -7.646965722246000574 ) ) ;
#28047 = CARTESIAN_POINT ( 'NONE',  ( -5.786987246029717369, -78.26865275249193132, 10.31969880544682105 ) ) ;
#28048 = ORIENTED_EDGE ( 'NONE', *, *, #3561, .F. ) ;
#28049 = AXIS2_PLACEMENT_3D ( 'NONE', #38833, #33812, #29100 ) ;
#28050 = CARTESIAN_POINT ( 'NONE',  ( -8.235122208958999934, -78.65001270277200263, 7.512480467459000444 ) ) ;
#28051 = CARTESIAN_POINT ( 'NONE',  ( 12.76303204291999904, -55.53514849259999409, 1.980584515756000030 ) ) ;
#28052 = CARTESIAN_POINT ( 'NONE',  ( 1.407171709420391936, -79.86458333333330017, 10.75000000000000178 ) ) ;
#28053 = CARTESIAN_POINT ( 'NONE',  ( 2.194290416744271610, -78.40681307243320930, 3.799401686813050905 ) ) ;
#28054 = CARTESIAN_POINT ( 'NONE',  ( 11.81845385912002833, -77.71935230467143185, 2.469272334833096494 ) ) ;
#28055 = CARTESIAN_POINT ( 'NONE',  ( 11.51387517028932983, -76.43373939162262332, -2.343431589605189380 ) ) ;
#28056 = AXIS2_PLACEMENT_3D ( 'NONE', #55903, #33148, #50898 ) ;
#28057 = CARTESIAN_POINT ( 'NONE',  ( -12.50728617043997382, -53.80024476438079262, -0.1757989195630510482 ) ) ;
#28058 = CARTESIAN_POINT ( 'NONE',  ( -1.624989163556999772E-14, -74.69999999881999031, -11.09999999881999955 ) ) ;
#28059 = VECTOR ( 'NONE', #58203, 1000.000000000000114 ) ;
#28060 = CARTESIAN_POINT ( 'NONE',  ( 1.201541383778999883, -77.86234880411998915, 0.5167982821483999567 ) ) ;
#28061 = DIRECTION ( 'NONE',  ( 0.07798810297990088625, -0.04890180925216059543, -0.9957542211035118607 ) ) ;
#28062 = CARTESIAN_POINT ( 'NONE',  ( 4.038850543673305538, -79.60508927849706140, -10.20566044646936099 ) ) ;
#28063 = DIRECTION ( 'NONE',  ( 0.000000000000000000, 0.000000000000000000, -1.000000000000000000 ) ) ;
#28064 = EDGE_LOOP ( 'NONE', ( #32975, #40932, #31512, #6080 ) ) ;
#28065 = EDGE_LOOP ( 'NONE', ( #35673, #13811, #22927 ) ) ;
#28066 = CARTESIAN_POINT ( 'NONE',  ( -9.943323471430000282, -78.36933998579799265, 1.256133873833999992 ) ) ;
#28067 = CARTESIAN_POINT ( 'NONE',  ( 9.298325636522646320, -78.80826077773562588, -5.396105918537423385 ) ) ;
#28068 = ORIENTED_EDGE ( 'NONE', *, *, #48882, .F. ) ;
#28069 = DIRECTION ( 'NONE',  ( 0.000000000000000000, -1.000000000000000000, 0.000000000000000000 ) ) ;
#28070 = CARTESIAN_POINT ( 'NONE',  ( 2.818472100349270981, -84.09583334529067145, 1.979553588263253783 ) ) ;
#28071 = CARTESIAN_POINT ( 'NONE',  ( -9.048147692728329972, -79.37506682946143144, 2.894494549572617093 ) ) ;
#28072 = CARTESIAN_POINT ( 'NONE',  ( 7.969039355710000549, -61.42377467811000002, 9.934746417661001416 ) ) ;
#28074 = ADVANCED_FACE ( 'NONE', ( #15359 ), #24504, .F. ) ;
#28073 = CARTESIAN_POINT ( 'NONE',  ( -11.51862140649527433, -76.07163159476074554, -3.285871775498967473 ) ) ;
#28075 = CARTESIAN_POINT ( 'NONE',  ( 8.273086841016404236, -78.23556425626672706, -8.664642258571072730 ) ) ;
#28076 = CARTESIAN_POINT ( 'NONE',  ( 10.12058791103999944, -79.55158152698399476, 4.836508133599999759 ) ) ;
#28077 = ORIENTED_EDGE ( 'NONE', *, *, #40025, .T. ) ;
#28078 = LINE ( 'NONE', #32791, #44412 ) ;
#28079 = ORIENTED_EDGE ( 'NONE', *, *, #55001, .F. ) ;
#28080 = CARTESIAN_POINT ( 'NONE',  ( 9.220724224615148401, -77.35639230030703573, 0.7348276087542371382 ) ) ;
#28081 = CARTESIAN_POINT ( 'NONE',  ( 3.792698199283999649, -78.08305780879798874, -10.36819406884000117 ) ) ;
#28082 = FACE_OUTER_BOUND ( 'NONE', #41229, .T. ) ;
#28083 = CARTESIAN_POINT ( 'NONE',  ( -1.959694873104000257, -77.49927292857998395, -9.504225410855001499 ) ) ;
#28084 = CARTESIAN_POINT ( 'NONE',  ( -8.813906588467560255, -16.98989792586478131, 8.872948313426432421 ) ) ;
#28085 = CYLINDRICAL_SURFACE ( 'NONE', #24744, 0.5000000000000006661 ) ;
#28086 = CARTESIAN_POINT ( 'NONE',  ( -0.9536002873971000104, -79.25442653435999318, 1.318830682536000110 ) ) ;
#28087 = DIRECTION ( 'NONE',  ( 0.9999999999999994449, -3.428898372810997945E-08, -7.232769369940996221E-12 ) ) ;
#28088 = CONICAL_SURFACE ( 'NONE', #55461, 3.699999993671000187, 0.7853981633972997312 ) ;
#28089 = CARTESIAN_POINT ( 'NONE',  ( -10.40934573790000073, -78.40429499344598696, 3.366502286031999969 ) ) ;
#28090 = CARTESIAN_POINT ( 'NONE',  ( -8.870414880995999951, -25.06963060262999932, -8.878264461096000204 ) ) ;
#28091 = EDGE_CURVE ( 'NONE', #15092, #42165, #38654, .T. ) ;
#28092 = CARTESIAN_POINT ( 'NONE',  ( 4.784911713602124195, -79.13352425759953235, 8.302150867234010079 ) ) ;
#28093 = CARTESIAN_POINT ( 'NONE',  ( -3.348269392590999871, -83.09967856441200240, -1.293382021977999896 ) ) ;
#28094 = ORIENTED_EDGE ( 'NONE', *, *, #10165, .T. ) ;
#28095 = CARTESIAN_POINT ( 'NONE',  ( -5.688772062455999645, -78.96059218971498694, -11.05567345541000002 ) ) ;
#28096 = CARTESIAN_POINT ( 'NONE',  ( 9.797622870535001027, -75.99542849098199326, 4.847984067100000516 ) ) ;
#28097 = CARTESIAN_POINT ( 'NONE',  ( 4.872804577377794821, -77.93772164444546036, 9.582789123844438706 ) ) ;
#28098 = CARTESIAN_POINT ( 'NONE',  ( 11.20799393363000007, -77.91261525259299958, 4.230477091134000389 ) ) ;
#28099 = DIRECTION ( 'NONE',  ( 1.000000000000000000, 0.000000000000000000, 0.000000000000000000 ) ) ;
#28100 = CARTESIAN_POINT ( 'NONE',  ( 8.485281374238999419, -55.64999999967000122, -8.485281374238999419 ) ) ;
#28101 = CARTESIAN_POINT ( 'NONE',  ( -3.372337180869588558, -2.721983097397393081, 1.223328859044781503 ) ) ;
#28102 = CARTESIAN_POINT ( 'NONE',  ( 10.75000000000000000, -76.75000000000000000, 0.000000000000000000 ) ) ;
#28103 = CARTESIAN_POINT ( 'NONE',  ( 8.981578277711999903, -78.35338192318698702, 2.818234580162000125 ) ) ;
#28104 = CARTESIAN_POINT ( 'NONE',  ( 0.3624061150339111803, -85.80681307385599155, -8.089689221462933233 ) ) ;
#28105 = CARTESIAN_POINT ( 'NONE',  ( -2.172168385828000314, -78.00052962514999422, -10.93326506925000174 ) ) ;
#28106 = CARTESIAN_POINT ( 'NONE',  ( 5.459501886381000091, -76.31165543856863565, -11.00074850082999767 ) ) ;
#28107 = CARTESIAN_POINT ( 'NONE',  ( 5.392198052114999918, -81.12538518513179042, -9.378990218028999237 ) ) ;
#28108 = ORIENTED_EDGE ( 'NONE', *, *, #31993, .T. ) ;
#28109 = FACE_OUTER_BOUND ( 'NONE', #11340, .T. ) ;
#28110 = CARTESIAN_POINT ( 'NONE',  ( -7.674627477122999863, -19.24922971947000150, -10.14950121128000049 ) ) ;
#28111 = CARTESIAN_POINT ( 'NONE',  ( 9.144378690012999300, -77.39916518241399501, -6.496033325431000094 ) ) ;
#28112 = CARTESIAN_POINT ( 'NONE',  ( 4.634563706678000550, -78.64985482243899639, 9.949112313689999709 ) ) ;
#28113 = CARTESIAN_POINT ( 'NONE',  ( 9.650948395506999233, -24.93402498662999989, -8.252474012539000370 ) ) ;
#28114 = CARTESIAN_POINT ( 'NONE',  ( 1.884805892303897945, -82.70833331645327746, 3.542755432913997193 ) ) ;
#28115 = ADVANCED_FACE ( 'NONE', ( #52245 ), #51386, .F. ) ;
#28116 = CARTESIAN_POINT ( 'NONE',  ( 2.842489150044962720, -1.893179537874919438, 1.637331356070920396 ) ) ;
#28117 = CARTESIAN_POINT ( 'NONE',  ( 1.980584515752000119, -23.26485146623999967, -12.76303204602000108 ) ) ;
#28118 = CARTESIAN_POINT ( 'NONE',  ( -3.892258265018999630, -83.27544503318799229, -1.503458620679999802 ) ) ;
#28119 = CARTESIAN_POINT ( 'NONE',  ( 0.000000000000000000, -74.70999999999999375, 0.000000000000000000 ) ) ;
#28120 = CARTESIAN_POINT ( 'NONE',  ( -1.828834964158999821, -79.10810244884000042, -12.81907926638999839 ) ) ;
#28121 = B_SPLINE_SURFACE_WITH_KNOTS ( 'NONE', 3, 3, ( 
 ( #16119, #56849, #7253, #16408, #30546, #48293, #17559, #43860, #16985, #8406, #30830, #48864, #57423, #21978, #35253, #53284, #31111, #7832, #44142, #25832, #3408, #12830, #17862, #30252, #45021, #26403, #12547, #17263, #34967, #22575, #9002, #44425, #3976, #21406, #39418 ),
 ( #26121, #57708, #16698, #3690, #13117, #21692, #39989, #52998, #58003, #26987, #48579, #44725, #39700, #34679, #35551, #53579, #31413, #26693, #13414, #8121, #49152, #12260, #4575, #8703, #57132, #4278, #22274, #40290, #58301, #35851, #52708, #53881, #49456, #2115, #19823 ),
 ( #46995, #50039, #45614, #33670, #37814, #10679, #23156, #41161, #27570, #755, #28660, #29239, #28953, #45318, #6524, #10972, #24245, #11258, #18734, #56125, #4868, #49751, #184, #24535, #40876, #20115, #47286, #51708, #46708, #5155, #36728, #42547, #42261, #15086, #38105 ),
 ( #40587, #1827, #51126, #15386, #18158, #33082, #54742, #15673, #6814, #55836, #33381, #36152, #51417, #22867, #54169, #13709, #6229, #31704, #9294, #27282, #468, #18447, #36436, #54464, #14000, #31998, #9586, #6906, #56215, #51796, #51507, #55928, #47087, #1919, #2205 ) ),
 .UNSPECIFIED., .F., .F., .F.,
 ( 4, 4 ),
 ( 4, 1, 1, 1, 1, 1, 1, 1, 1, 1, 1, 1, 1, 1, 1, 1, 1, 1, 1, 1, 1, 1, 1, 1, 1, 1, 1, 1, 1, 1, 1, 1, 4 ),
 ( -0.3708084972812999980, 1.370808497280999960 ),
 ( -0.01035614953205000154, 0.006472593457530000441, 0.02330133644711000068, 0.04013007943667999677, 0.05695882242625999875, 0.07378756541584000073, 0.09061630840541999576, 0.1074450513949999908, 0.1242737943845999976, 0.1411025373741000011, 0.1579312803636999940, 0.1747600233533000147, 0.1915887663428999799, 0.2084175093325000006, 0.2252462523220000179, 0.2420749953115999831, 0.2589037383012000038, 0.2757324812907999689, 0.2925612242803000140, 0.3093899672698999792, 0.3262187102594999999, 0.3430474532491000206, 0.3598761962386999858, 0.3767049392282000309, 0.3935336822177999960, 0.4103624252073999612, 0.4271911681970000374, 0.4440199111864999715, 0.4608486541761000477, 0.4776773971657000128, 0.4945061401552999780, 0.5113348831447999121, 0.5281636261344000438 ),
 .UNSPECIFIED. ) ;
#28122 = CARTESIAN_POINT ( 'NONE',  ( 11.06080859785000037, -77.04165712091899820, 2.119546583493000291 ) ) ;
#28123 = CARTESIAN_POINT ( 'NONE',  ( -0.7048934085577001074, -80.80140853768000397, -1.509431780672999990 ) ) ;
#28124 = CARTESIAN_POINT ( 'NONE',  ( 1.077250838572999969, -78.72093299843999148, -0.7630258981648999628 ) ) ;
#28125 = DIRECTION ( 'NONE',  ( 1.000000000000000000, 0.000000000000000000, 0.000000000000000000 ) ) ;
#28126 = CARTESIAN_POINT ( 'NONE',  ( 0.7766941700662266523, -81.41797789504143168, -1.295155736999946461 ) ) ;
#28127 = CARTESIAN_POINT ( 'NONE',  ( 0.000000000000000000, 0.000000000000000000, -10.40000000000006963 ) ) ;
#28128 = DIRECTION ( 'NONE',  ( 0.000000000000000000, 1.000000000000000000, 0.000000000000000000 ) ) ;
#28129 = CARTESIAN_POINT ( 'NONE',  ( 1.183919390960944007, -79.82443352179983265, -0.4012659760898111827 ) ) ;
#28130 = AXIS2_PLACEMENT_3D ( 'NONE', #51462, #14835, #9844 ) ;
#28131 = CARTESIAN_POINT ( 'NONE',  ( -7.730439324398687972, -54.67809618926516890, 10.25198230927261456 ) ) ;
#28132 = ORIENTED_EDGE ( 'NONE', *, *, #9852, .T. ) ;
#28133 = CARTESIAN_POINT ( 'NONE',  ( 0.06645687873235063547, -81.72973678372032680, -1.248208688943512001 ) ) ;
#28134 = CARTESIAN_POINT ( 'NONE',  ( 6.654794014482000364, -79.63539396382098801, -8.798605060253001042 ) ) ;
#28135 = CARTESIAN_POINT ( 'NONE',  ( -1.092232985442822102, -80.04166666666664298, -0.6295237254636245616 ) ) ;
#28136 = ORIENTED_EDGE ( 'NONE', *, *, #20316, .T. ) ;
#28137 = VERTEX_POINT ( 'NONE', #23916 ) ;
#28138 = CARTESIAN_POINT ( 'NONE',  ( 0.7219739802542000096, -81.27020361841898932, -1.220169230883999978 ) ) ;
#28139 = ORIENTED_EDGE ( 'NONE', *, *, #14552, .T. ) ;
#28140 = ORIENTED_EDGE ( 'NONE', *, *, #58078, .F. ) ;
#28141 = CARTESIAN_POINT ( 'NONE',  ( 1.930009203935999951, -18.79900967682999635, 12.72537718777000038 ) ) ;
#28142 = DIRECTION ( 'NONE',  ( -1.000000000000000000, 0.000000000000000000, 0.000000000000000000 ) ) ;
#28143 = CARTESIAN_POINT ( 'NONE',  ( 1.808130592854080065, -82.20729165018273932, -2.930395587151967796 ) ) ;
#28144 = B_SPLINE_CURVE_WITH_KNOTS ( 'NONE', 3,
 ( #8093, #12518, #17528, #48831 ),
 .UNSPECIFIED., .F., .F.,
 ( 4, 4 ),
 ( 0.000000000000000000, 0.9996434014792530132 ),
 .UNSPECIFIED. ) ;
#28146 = EDGE_CURVE ( 'NONE', #35842, #32930, #37489, .T. ) ;
#28145 = CARTESIAN_POINT ( 'NONE',  ( 8.642645349805999189, -79.02841001420199518, -5.074666031188000304 ) ) ;
#28147 = CARTESIAN_POINT ( 'NONE',  ( 6.718422235614084137, -78.28969101729559554, -6.358450322077904282 ) ) ;
#28148 = CARTESIAN_POINT ( 'NONE',  ( 10.47020627418439531, -78.22916666666665719, -2.813789756862242974 ) ) ;
#28149 = ORIENTED_EDGE ( 'NONE', *, *, #50687, .F. ) ;
#28151 = ORIENTED_EDGE ( 'NONE', *, *, #40608, .F. ) ;
#28150 = EDGE_CURVE ( 'NONE', #25175, #7399, #41168, .T. ) ;
#28152 = CARTESIAN_POINT ( 'NONE',  ( -8.635538383447757482, -77.57078966990042090, 3.323345330289224631 ) ) ;
#28153 = CARTESIAN_POINT ( 'NONE',  ( 1.387435826181646847, -77.03417277704993182, -11.96237581351085488 ) ) ;
#28154 = CARTESIAN_POINT ( 'NONE',  ( 1.500000000000000000, -79.25000000000000000, 0.000000000000000000 ) ) ;
#28155 = PRODUCT_DEFINITION_SHAPE ( 'NONE', 'NONE',  #58412 ) ;
#28156 = CARTESIAN_POINT ( 'NONE',  ( -0.9356112518082062568, -17.25892169759421080, 12.50329130247410880 ) ) ;
#28157 = CARTESIAN_POINT ( 'NONE',  ( -5.681372509047000641, -78.34507726762299740, -7.867192369580999767 ) ) ;
#28158 = DIRECTION ( 'NONE',  ( 0.000000000000000000, 1.000000000000000000, -1.093719250013000041E-14 ) ) ;
#28159 = CARTESIAN_POINT ( 'NONE',  ( -10.55910102242999926, -22.78485473281999774, 7.642147947518999729 ) ) ;
#28160 = CARTESIAN_POINT ( 'NONE',  ( 11.60238327475000197, -76.61614726144999565, 5.404242916298000132 ) ) ;
#28161 = CARTESIAN_POINT ( 'NONE',  ( -1.425428639595999858, -80.67057293764999315, 0.6946581327067000711 ) ) ;
#28162 = CARTESIAN_POINT ( 'NONE',  ( 3.892964293701162592, -77.20864693750340280, -8.607536166100398844 ) ) ;
#28163 = EDGE_CURVE ( 'NONE', #13927, #31547, #11973, .T. ) ;
#28164 = CARTESIAN_POINT ( 'NONE',  ( -9.380331153422687862, -76.64831997961195498, 7.077055143005254401 ) ) ;
#28165 = CARTESIAN_POINT ( 'NONE',  ( -1.405983071794000061, -82.04949591394598940, -3.931009852230000323 ) ) ;
#28166 = CARTESIAN_POINT ( 'NONE',  ( 1.328862289696999932, -80.13169679617828933, 11.18676134159000135 ) ) ;
#28167 = CARTESIAN_POINT ( 'NONE',  ( -7.374059913654000376, -79.12681001420199323, -6.282030610069000431 ) ) ;
#28168 = CARTESIAN_POINT ( 'NONE',  ( 12.00000000000000000, -77.16041666666669130, 1.570796326794922093 ) ) ;
#28169 = CARTESIAN_POINT ( 'NONE',  ( 3.344834401207000152, -81.04355496681199611, 1.180527502125999773 ) ) ;
#28171 = CARTESIAN_POINT ( 'NONE',  ( 1.166929042523999982, -78.93167174815900466, -0.6456414311070999279 ) ) ;
#28170 = CARTESIAN_POINT ( 'NONE',  ( 5.137083998358000336, -77.21100733245999947, -10.56753840748999984 ) ) ;
#28172 = CIRCLE ( 'NONE', #10289, 0.8000000000000000444 ) ;
#28173 = DIRECTION ( 'NONE',  ( -1.000000000000000000, 0.000000000000000000, 0.000000000000000000 ) ) ;
#28174 = DIRECTION ( 'NONE',  ( 1.000000000000000000, 0.000000000000000000, 0.000000000000000000 ) ) ;
#28175 = DIRECTION ( 'NONE',  ( 0.000000000000000000, 0.000000000000000000, -1.000000000000000000 ) ) ;
#28176 = ORIENTED_EDGE ( 'NONE', *, *, #2361, .T. ) ;
#28177 = CARTESIAN_POINT ( 'NONE',  ( 8.251802458185739653, -61.60055625091321474, 9.431055091036006033 ) ) ;
#28178 = CARTESIAN_POINT ( 'NONE',  ( 8.190836719257466925, -59.98964892062851106, -7.342356150419175442 ) ) ;
#28179 = DIRECTION ( 'NONE',  ( 1.000000000000000000, 0.000000000000000000, -1.156375342703997101E-13 ) ) ;
#28180 = CARTESIAN_POINT ( 'NONE',  ( 3.902330291231000281, -79.98742867705199444, -8.777487365357000471 ) ) ;
#28181 = CARTESIAN_POINT ( 'NONE',  ( 1.250000000000000000, -79.25000000000000000, 0.000000000000000000 ) ) ;
#28182 = CARTESIAN_POINT ( 'NONE',  ( 8.488409410023923130, -79.40273845399939034, 6.622596058701640587 ) ) ;
#28183 = CARTESIAN_POINT ( 'NONE',  ( 7.000000000000000000, -81.10000000285099020, 0.000000000000000000 ) ) ;
#28184 = CARTESIAN_POINT ( 'NONE',  ( -9.723199427802001082, -54.32306055813000256, 7.958735710007999842 ) ) ;
#28185 = CARTESIAN_POINT ( 'NONE',  ( 6.578861079155999825, -77.41820342825998580, -9.021296591805000986 ) ) ;
#28186 = CARTESIAN_POINT ( 'NONE',  ( -1.562814397797999799, -82.38997108803900460, 0.3613598533091000320 ) ) ;
#28187 = CARTESIAN_POINT ( 'NONE',  ( -1.750000000001000089, -18.74999999009000007, 12.56594317857000043 ) ) ;
#28188 = CARTESIAN_POINT ( 'NONE',  ( -9.395661821092000210, -77.51593683473198837, 0.5765637145115000139 ) ) ;
#28190 = CARTESIAN_POINT ( 'NONE',  ( 2.839805762151335511, -2.791666666666667407, 1.636761686205429278 ) ) ;
#28189 = CARTESIAN_POINT ( 'NONE',  ( 0.1947808891803000098, -85.50854634175698266, 3.958280990209000372 ) ) ;
#28191 = CARTESIAN_POINT ( 'NONE',  ( 4.067416459488999436, -79.29095194988499884, -8.418325902196000854 ) ) ;
#28192 = CARTESIAN_POINT ( 'NONE',  ( -1.250000000000000000, -77.10000000000000853, 0.000000000000000000 ) ) ;
#28193 = CARTESIAN_POINT ( 'NONE',  ( -0.5991125319583999742, -80.24554665869699477, -1.175427489992000085 ) ) ;
#28194 = EDGE_CURVE ( 'NONE', #43036, #48350, #17085, .T. ) ;
#28195 = DIRECTION ( 'NONE',  ( -1.000000000000000000, 0.000000000000000000, 0.000000000000000000 ) ) ;
#28196 = CARTESIAN_POINT ( 'NONE',  ( -9.500000000000000000, -77.39999999999999147, 0.000000000000000000 ) ) ;
#28197 = VERTEX_POINT ( 'NONE', #35068 ) ;
#28198 = CARTESIAN_POINT ( 'NONE',  ( -12.02912753549999891, -79.63333152568600326, 0.08506824670321999626 ) ) ;
#28199 = DIRECTION ( 'NONE',  ( 1.000000000000000000, 0.000000000000000000, 0.000000000000000000 ) ) ;
#28200 = CARTESIAN_POINT ( 'NONE',  ( 8.500000000000000000, -75.00000000000001421, 0.000000000000000000 ) ) ;
#28201 = ORIENTED_EDGE ( 'NONE', *, *, #13889, .T. ) ;
#28202 = CARTESIAN_POINT ( 'NONE',  ( 9.500000000000000000, -78.04999999999999716, 0.000000000000000000 ) ) ;
#28203 = CARTESIAN_POINT ( 'NONE',  ( 1.714448272638999793, -77.26006991430598703, -11.65560625356000024 ) ) ;
#28204 = ORIENTED_EDGE ( 'NONE', *, *, #9956, .T. ) ;
#28205 = EDGE_LOOP ( 'NONE', ( #45539, #24682, #34376, #23284, #37895 ) ) ;
#28206 = CARTESIAN_POINT ( 'NONE',  ( 8.190817883596542615, -60.03019609282340951, 7.342377162853137129 ) ) ;
#28207 = VECTOR ( 'NONE', #17866, 1000.000000000000114 ) ;
#28208 = ORIENTED_EDGE ( 'NONE', *, *, #27484, .F. ) ;
#28209 = CARTESIAN_POINT ( 'NONE',  ( 0.4739133679264000421, -79.08816791445418914, -3.515676078802999704 ) ) ;
#28210 = CARTESIAN_POINT ( 'NONE',  ( 0.000000000000000000, -46.43897132165000130, 0.000000000000000000 ) ) ;
#28211 = VERTEX_POINT ( 'NONE', #4086 ) ;
#28212 = DIRECTION ( 'NONE',  ( 0.000000000000000000, 1.000000000000000000, 0.000000000000000000 ) ) ;
#28213 = CARTESIAN_POINT ( 'NONE',  ( -7.655542440077000244, -56.02180874340999850, 10.38645071868999992 ) ) ;
#28215 = ADVANCED_FACE ( 'NONE', ( #30930 ), #48832, .F. ) ;
#28214 = ORIENTED_EDGE ( 'NONE', *, *, #39753, .T. ) ;
#28216 = CARTESIAN_POINT ( 'NONE',  ( -1.407171709420418138, -80.61458333333331439, -10.75000000000000000 ) ) ;
#28217 = CARTESIAN_POINT ( 'NONE',  ( -0.1538830739163870864, -78.22616755078296080, 9.703099906196978708 ) ) ;
#28218 = VECTOR ( 'NONE', #50363, 1000.000000000000000 ) ;
#28219 = CARTESIAN_POINT ( 'NONE',  ( 0.000000000000000000, -75.00000000000000000, 6.000000000000230038 ) ) ;
#28220 = DIRECTION ( 'NONE',  ( 1.000000000000000000, 0.000000000000000000, 0.000000000000000000 ) ) ;
#28221 = VECTOR ( 'NONE', #9581, 1000.000000000000000 ) ;
#28222 = CARTESIAN_POINT ( 'NONE',  ( -3.911457351643479186, -78.54938062601392801, -11.62361573341717857 ) ) ;
#28223 = CARTESIAN_POINT ( 'NONE',  ( -1.432420283025999996, -76.15132621805099689, 11.09153081809999897 ) ) ;
#28224 = FACE_OUTER_BOUND ( 'NONE', #33430, .T. ) ;
#28225 = DIRECTION ( 'NONE',  ( 0.000000000000000000, -1.000000000000000000, 0.000000000000000000 ) ) ;
#28226 = CARTESIAN_POINT ( 'NONE',  ( -7.642147947533000085, -59.58485473249000108, -10.55910102243999837 ) ) ;
#28227 = B_SPLINE_CURVE_WITH_KNOTS ( 'NONE', 3,
 ( #55584, #41424, #37569, #32539, #31668, #36985 ),
 .UNSPECIFIED., .F., .F.,
 ( 4, 2, 4 ),
 ( 0.000000000000000000, 0.5000000000000000000, 1.000000000000000000 ),
 .UNSPECIFIED. ) ;
#28228 = ADVANCED_FACE ( 'NONE', ( #32114 ), #23557, .T. ) ;
#28229 = CARTESIAN_POINT ( 'NONE',  ( 6.615973074419398969, -78.78858769152571995, -6.464602604579136269 ) ) ;
#28230 = CARTESIAN_POINT ( 'NONE',  ( 8.309590093900645513, -76.51194161182486653, 8.306937813281372485 ) ) ;
#28231 = CARTESIAN_POINT ( 'NONE',  ( 9.406593443539000177, -77.82323501420199818, 0.3044902167661999726 ) ) ;
#28232 = CARTESIAN_POINT ( 'NONE',  ( -10.50000000000000000, -76.19999999999998863, 0.000000000000000000 ) ) ;
#28233 = EDGE_CURVE ( 'NONE', #41078, #43698, #49864, .T. ) ;
#28234 = DIRECTION ( 'NONE',  ( 2.582635147408000164E-11, 0.000000000000000000, -1.000000000000000000 ) ) ;
#28235 = CARTESIAN_POINT ( 'NONE',  ( 11.75000000000000000, -76.55000000000001137, 0.000000000000000000 ) ) ;
#28236 = CARTESIAN_POINT ( 'NONE',  ( 3.242172098794999791, -80.60217549782598212, -2.558676140119000131 ) ) ;
#28237 = DIRECTION ( 'NONE',  ( 0.9999999999995751176, 0.000000000000000000, 9.217549097710770925E-07 ) ) ;
#28238 = CARTESIAN_POINT ( 'NONE',  ( 1.087185650191391462, -82.89120236429288013, 0.6181942457068143604 ) ) ;
#28239 = CARTESIAN_POINT ( 'NONE',  ( 13.13047446164998711, -56.01421830981000483, -0.8260994316375004365 ) ) ;
#28240 = CARTESIAN_POINT ( 'NONE',  ( -3.140974612311405512, -79.29583333333334849, 11.68767212001977640 ) ) ;
#28241 = CARTESIAN_POINT ( 'NONE',  ( 0.5999999998848000171, -23.14999999478999726, 11.79999999988000070 ) ) ;
#28242 = CARTESIAN_POINT ( 'NONE',  ( 12.70619440579097770, -24.46151788318003995, -1.571771935829441968 ) ) ;
#28243 = CARTESIAN_POINT ( 'NONE',  ( -1.930628539545000022, -23.22124444086000139, -12.72375828104000028 ) ) ;
#28244 = CARTESIAN_POINT ( 'NONE',  ( 1.500000000000000000, -81.65000000000000568, 0.000000000000000000 ) ) ;
#28245 = PLANE ( 'NONE',  #14461 ) ;
#28246 = CARTESIAN_POINT ( 'NONE',  ( 12.77657007940999989, -25.31210281330999834, 0.1589025507404999982 ) ) ;
#28247 = CARTESIAN_POINT ( 'NONE',  ( -0.6295237254636235624, -80.58333333333332860, -1.092232985442822990 ) ) ;
#28248 = CARTESIAN_POINT ( 'NONE',  ( 8.206048927592433984, -77.25648637437664945, 6.978187335436623506 ) ) ;
#28249 = CARTESIAN_POINT ( 'NONE',  ( -11.00000000000000000, -78.09999999999999432, 2.733298954964999989E-14 ) ) ;
#28250 = EDGE_CURVE ( 'NONE', #43973, #32937, #26062, .T. ) ;
#28252 = CARTESIAN_POINT ( 'NONE',  ( 4.038786804788999873, -79.50498703829204317, -10.20549938644000321 ) ) ;
#28251 = CARTESIAN_POINT ( 'NONE',  ( 1.886823409074000146, -60.56319684329000097, 12.68610076208999971 ) ) ;
#28253 = CARTESIAN_POINT ( 'NONE',  ( -4.047764079874000664, -76.07042549139001153, 11.52168212187000051 ) ) ;
#28254 = ORIENTED_EDGE ( 'NONE', *, *, #29266, .T. ) ;
#28255 = CARTESIAN_POINT ( 'NONE',  ( 3.297965217643000102, -82.63071544543198854, -1.885706124222999991 ) ) ;
#28256 = CARTESIAN_POINT ( 'NONE',  ( -10.71935382865999919, -80.11839559862080762, 3.149475271190000036 ) ) ;
#28257 = CARTESIAN_POINT ( 'NONE',  ( 9.047822906991040526, -78.33349585849774144, -1.923928064677009608 ) ) ;
#28258 = CARTESIAN_POINT ( 'NONE',  ( 7.624341764906000130, -55.53514850498000044, 10.42531124851000079 ) ) ;
#28259 = CARTESIAN_POINT ( 'NONE',  ( -11.16975252231999960, -76.89438592419598706, 1.027088271520000040 ) ) ;
#28260 = CARTESIAN_POINT ( 'NONE',  ( 10.35453599130000057, -76.65783510652001098, -6.064947188958000446 ) ) ;
#28261 = CARTESIAN_POINT ( 'NONE',  ( -3.921497456393000292, -77.92121002409098196, -8.915242756422999904 ) ) ;
#28262 = VECTOR ( 'NONE', #14482, 1000.000000000000000 ) ;
#28263 = CARTESIAN_POINT ( 'NONE',  ( 0.000000000000000000, -55.54999999966999980, -12.50000000000000000 ) ) ;
#28264 = CARTESIAN_POINT ( 'NONE',  ( 3.399999999999999911, -78.72609999968186401, 0.000000000000000000 ) ) ;
#28265 = CARTESIAN_POINT ( 'NONE',  ( 7.390111938209032338, -76.06041666666433798, 8.214641434548898502 ) ) ;
#28266 = ORIENTED_EDGE ( 'NONE', *, *, #25804, .F. ) ;
#28267 = EDGE_CURVE ( 'NONE', #21151, #44472, #27686, .T. ) ;
#28268 = DIRECTION ( 'NONE',  ( 0.000000000000000000, -1.000000000000000000, 0.000000000000000000 ) ) ;
#28269 = AXIS2_PLACEMENT_3D ( 'NONE', #45301, #3956, #58281 ) ;
#28270 = CARTESIAN_POINT ( 'NONE',  ( 6.985849709488999970, -80.87654576500008829, -8.837815942395002011 ) ) ;
#28271 = DIRECTION ( 'NONE',  ( 0.000000000000000000, 1.000000000000000000, 0.000000000000000000 ) ) ;
#28272 = VERTEX_POINT ( 'NONE', #4974 ) ;
#28273 = EDGE_CURVE ( 'NONE', #29770, #43853, #45138, .T. ) ;
#28274 = CARTESIAN_POINT ( 'NONE',  ( 1.166929042523999982, -78.88789773057999355, -0.6456414311070000078 ) ) ;
#28275 = CARTESIAN_POINT ( 'NONE',  ( -5.572401197671056572, -77.57410848619153398, -7.480459026222967545 ) ) ;
#28276 = CARTESIAN_POINT ( 'NONE',  ( -1.239625094629522195, -80.61368471397051394, -0.2079133391517598850 ) ) ;
#28277 = ORIENTED_EDGE ( 'NONE', *, *, #36593, .T. ) ;
#28278 = CARTESIAN_POINT ( 'NONE',  ( 0.4965625967630000193, -77.69837184121800533, 12.26984941905000071 ) ) ;
#28279 = CARTESIAN_POINT ( 'NONE',  ( 3.720647276146999971, -77.77699006546498595, 10.45956222008999781 ) ) ;
#28280 = DIRECTION ( 'NONE',  ( 0.000000000000000000, 0.000000000000000000, -1.000000000000000000 ) ) ;
#28281 = ORIENTED_EDGE ( 'NONE', *, *, #31123, .F. ) ;
#28282 = EDGE_LOOP ( 'NONE', ( #17549, #16831, #28027, #40622 ) ) ;
#28283 = CARTESIAN_POINT ( 'NONE',  ( -10.00844281756000065, -55.43109810584000030, -7.647097920671999560 ) ) ;
#28284 =( NAMED_UNIT ( * ) PLANE_ANGLE_UNIT ( ) SI_UNIT ( $, .RADIAN. ) );
#28285 = CARTESIAN_POINT ( 'NONE',  ( 5.496668217546000434, -80.18287243149549681, -8.073860231047000013 ) ) ;
#28286 = ORIENTED_EDGE ( 'NONE', *, *, #23943, .F. ) ;
#28287 = CARTESIAN_POINT ( 'NONE',  ( 12.57354471034999932, -55.07622323954000620, 1.757967544833999973 ) ) ;
#28288 = DIRECTION ( 'NONE',  ( -0.9999999999999992228, 4.158392524217991108E-08, -7.899477153235985639E-12 ) ) ;
#28289 = VECTOR ( 'NONE', #36817, 1000.000000000000000 ) ;
#28290 = ORIENTED_EDGE ( 'NONE', *, *, #28425, .F. ) ;
#28291 = CARTESIAN_POINT ( 'NONE',  ( -12.77657007940999989, -25.31210281330999834, -0.1589025507404999982 ) ) ;
#28292 = CARTESIAN_POINT ( 'NONE',  ( 2.459440699436000077, -77.27590194988499661, -9.171074077620000153 ) ) ;
#28293 = CARTESIAN_POINT ( 'NONE',  ( -0.9219487215672478309, -80.15967048775068804, -0.8452775506683704032 ) ) ;
#28294 = CARTESIAN_POINT ( 'NONE',  ( -1.318114156675707971, -17.26427522807030712, -12.70261578162816996 ) ) ;
#28295 = CARTESIAN_POINT ( 'NONE',  ( -9.318755185595000157, -77.17535770753909219, -0.9064345995222999885 ) ) ;
#28296 = CARTESIAN_POINT ( 'NONE',  ( 1.041440387436121107, -78.03515770762014370, -1.092726133770612229 ) ) ;
#28297 = CARTESIAN_POINT ( 'NONE',  ( -2.531415867984625034, -78.91197914798334523, -3.112890062190800222 ) ) ;
#28298 = ORIENTED_EDGE ( 'NONE', *, *, #24662, .T. ) ;
#28299 = CARTESIAN_POINT ( 'NONE',  ( -12.22985280536000019, -76.52641765524998618, -1.402219185755000153 ) ) ;
#28300 = ADVANCED_FACE ( 'NONE', ( #50444 ), #27146, .F. ) ;
#28301 = B_SPLINE_SURFACE_WITH_KNOTS ( 'NONE', 3, 3, ( 
 ( #41708, #14828, #32826, #22533 ),
 ( #9253, #8960, #44978, #40543 ),
 ( #18114, #36108, #45276, #46748 ),
 ( #5978, #6268, #52034, #47327 ),
 ( #46450, #24283, #6566, #20727 ),
 ( #37856, #47036, #1569, #29567 ),
 ( #15427, #16009, #29278, #19561 ),
 ( #42883, #38437, #38145, #42592 ),
 ( #24576, #6856, #2155, #55577 ),
 ( #56454, #38725, #56746, #47623 ),
 ( #33421, #15126, #10417, #28995 ),
 ( #7146, #24865, #25148, #23984 ),
 ( #20156, #33124, #16306, #42001 ),
 ( #56167, #1867, #11011, #51166 ),
 ( #50871, #15715, #33709, #10720 ),
 ( #51748, #55877, #19861, #51458 ),
 ( #11298, #2440, #20442, #33996 ) ),
 .UNSPECIFIED., .F., .F., .F.,
 ( 4, 1, 1, 1, 1, 1, 1, 1, 1, 1, 1, 1, 1, 1, 4 ),
 ( 4, 4 ),
 ( -0.01011408452875999994, 0.000000000000000000, 0.08333333333333001192, 0.1666666666667000196, 0.2500000000000000000, 0.3333333333333000081, 0.4166666666666999919, 0.5000000000000000000, 0.5833333333333000637, 0.6666666666667000474, 0.7500000000000000000, 0.8333333333333000637, 0.9166666666667000474, 1.000000000000000000, 1.010362559108000102 ),
 ( -0.3559705546268999710, 1.357612419623000166 ),
 .UNSPECIFIED. ) ;
#28302 = CIRCLE ( 'NONE', #43405, 4.000000000000000000 ) ;
#28303 = CARTESIAN_POINT ( 'NONE',  ( -12.69999999999999929, 0.000000000000000000, 0.000000000000000000 ) ) ;
#28304 = CARTESIAN_POINT ( 'NONE',  ( 7.646788277353000041, -60.17228598344999568, -10.00831419132999933 ) ) ;
#28305 = CARTESIAN_POINT ( 'NONE',  ( -5.950798862880000151, -78.93264987601000371, 10.72320280238000123 ) ) ;
#28306 = CARTESIAN_POINT ( 'NONE',  ( 5.459501886381000091, -76.29555329812299647, -11.00074850082999767 ) ) ;
#28307 = LINE ( 'NONE', #41613, #2540 ) ;
#28308 = CARTESIAN_POINT ( 'NONE',  ( 9.546819346760999636, -61.48527546573999558, -8.130850182902999990 ) ) ;
#28309 = CARTESIAN_POINT ( 'NONE',  ( -1.770201408374824092, -78.16324107959532341, -11.94606885956166842 ) ) ;
#28310 = CARTESIAN_POINT ( 'NONE',  ( 0.000000000000000000, 4.040000000000000036, 0.000000000000000000 ) ) ;
#28311 = ORIENTED_EDGE ( 'NONE', *, *, #36363, .F. ) ;
#28312 = FACE_OUTER_BOUND ( 'NONE', #43920, .T. ) ;
#28313 = CARTESIAN_POINT ( 'NONE',  ( 3.075537641221555596, -77.94583333333332575, -11.44417895085270587 ) ) ;
#28314 = CARTESIAN_POINT ( 'NONE',  ( -1.750000000001000089, -55.55000001292999912, -12.56594318049000059 ) ) ;
#28315 = CARTESIAN_POINT ( 'NONE',  ( 1.249999999999999778, -78.76041666666667140, 0.1636246173744711763 ) ) ;
#28316 = CARTESIAN_POINT ( 'NONE',  ( -3.370529087814999603, -2.253484528251000096, 1.902593404626000018 ) ) ;
#28317 = CARTESIAN_POINT ( 'NONE',  ( -0.08569088068253999380, -78.38442944748399555, 12.04941611642000154 ) ) ;
#28318 = CARTESIAN_POINT ( 'NONE',  ( -8.527407416480999203, -78.16847128433398950, 4.476218573567000369 ) ) ;
#28319 = EDGE_CURVE ( 'NONE', #15053, #33154, #44965, .T. ) ;
#28320 = CARTESIAN_POINT ( 'NONE',  ( -10.80861225507516821, -76.16775967368776890, 4.608194527468379320 ) ) ;
#28321 = CARTESIAN_POINT ( 'NONE',  ( -3.912255148455999976, -79.43075759821599036, 10.19164489391000217 ) ) ;
#28322 = CARTESIAN_POINT ( 'NONE',  ( -2.355016251977294583, -86.02148120184399716, 3.178902848251809576 ) ) ;
#28323 = ORIENTED_EDGE ( 'NONE', *, *, #15507, .F. ) ;
#28324 = CARTESIAN_POINT ( 'NONE',  ( 1.401388975520860170, -81.11718075262649563, -0.6178868534844423888 ) ) ;
#28325 = EDGE_CURVE ( 'NONE', #26401, #40202, #4643, .T. ) ;
#28326 = CARTESIAN_POINT ( 'NONE',  ( -5.655986146074000409, -79.84535256633930089, -10.76033745225999994 ) ) ;
#28327 = CARTESIAN_POINT ( 'NONE',  ( -1.250000000000000000, -79.10000000000000853, 0.000000000000000000 ) ) ;
#28328 = CIRCLE ( 'NONE', #54732, 14.00000000000000000 ) ;
#28329 = B_SPLINE_CURVE_WITH_KNOTS ( 'NONE', 3,
 ( #30132, #7714, #25715, #43741, #3294, #21286, #51739, #17147, #12996, #35134 ),
 .UNSPECIFIED., .F., .F.,
 ( 4, 2, 2, 2, 4 ),
 ( 0.000000000000000000, 0.07142685916348760766, 0.1428537183269752153, 0.2142805774904628369, 0.2857074366539503751 ),
 .UNSPECIFIED. ) ;
#28330 = CARTESIAN_POINT ( 'NONE',  ( -0.4254240051736286610, -2.385416666666666075, 3.249999999999997780 ) ) ;
#28331 = CARTESIAN_POINT ( 'NONE',  ( -1.297526016723000053, -78.60602476478999279, -10.89864408161000142 ) ) ;
#28332 = CARTESIAN_POINT ( 'NONE',  ( 3.140974612311326908, -77.75416666666663446, 11.68767212001979772 ) ) ;
#28333 = CARTESIAN_POINT ( 'NONE',  ( 4.287008109733999817, -79.80461169611500338, -8.668125945862000137 ) ) ;
#28334 = CARTESIAN_POINT ( 'NONE',  ( 10.18114972182000066, -18.60990354280999881, -7.633087078986000584 ) ) ;
#28335 = CARTESIAN_POINT ( 'NONE',  ( 8.096452064242996016, -59.58578169018998949, -13.15643568217000769 ) ) ;
#28336 = ORIENTED_EDGE ( 'NONE', *, *, #58364, .F. ) ;
#28337 = FACE_OUTER_BOUND ( 'NONE', #29521, .T. ) ;
#28338 = CARTESIAN_POINT ( 'NONE',  ( -11.12012002604264893, -79.52207733847474458, 4.052612807419244234 ) ) ;
#28339 = CARTESIAN_POINT ( 'NONE',  ( -14.00000000000000000, -45.89236309322999574, -1.352041732758999914E-05 ) ) ;
#28340 = CARTESIAN_POINT ( 'NONE',  ( -5.581034037647778057, -77.86612145202063573, 10.76842700904854411 ) ) ;
#28341 = ADVANCED_FACE ( 'NONE', ( #15610 ), #41310, .F. ) ;
#28343 = CARTESIAN_POINT ( 'NONE',  ( -1.121649604080707796, -81.56336073363873140, 0.5583008101125926936 ) ) ;
#28342 = CARTESIAN_POINT ( 'NONE',  ( 1.302090486218000054, -81.92092678672000261, 0.2124289815698000017 ) ) ;
#28344 = B_SPLINE_CURVE_WITH_KNOTS ( 'NONE', 3,
 ( #28954, #3263, #25394, #37815, #24536, #42549 ),
 .UNSPECIFIED., .F., .F.,
 ( 4, 1, 1, 4 ),
 ( 0.000000000000000000, 0.3333333333333000081, 0.6666666666667000474, 0.9999998688569219363 ),
 .UNSPECIFIED. ) ;
#28345 = CARTESIAN_POINT ( 'NONE',  ( 3.507204654865230697, -79.19960255973779795, 10.65462925082876922 ) ) ;
#28346 = AXIS2_PLACEMENT_3D ( 'NONE', #5617, #4464, #4755 ) ;
#28347 = CARTESIAN_POINT ( 'NONE',  ( -9.331242083993144476, -76.99999999999998579, -0.3638479554798288440 ) ) ;
#28348 = CARTESIAN_POINT ( 'NONE',  ( -8.179400486886379440, -17.25908162456390471, -9.502921779309215111 ) ) ;
#28349 = CIRCLE ( 'NONE', #51937, 4.299999999999999822 ) ;
#28350 = CARTESIAN_POINT ( 'NONE',  ( 0.6336387951535999985, -77.91478037390000111, 1.144239716453000044 ) ) ;
#28351 = CARTESIAN_POINT ( 'NONE',  ( 10.65280642239534181, -76.21655266097438641, 2.270707054235461264 ) ) ;
#28352 = B_SPLINE_SURFACE_WITH_KNOTS ( 'NONE', 3, 3, ( 
 ( #27230, #36389, #48526, #4818 ),
 ( #49102, #53233, #8071, #30779 ),
 ( #26067, #22817, #21927, #4525 ),
 ( #44969, #3642, #21645, #39652 ),
 ( #17213, #57952, #17810, #35201 ),
 ( #17506, #53526, #44673, #22224 ),
 ( #40235, #58249, #35796, #53826 ),
 ( #8952, #31359, #49403, #14533 ) ),
 .UNSPECIFIED., .F., .F., .F.,
 ( 4, 1, 1, 1, 1, 4 ),
 ( 4, 4 ),
 ( -0.01200407347463999970, 0.000000000000000000, 0.3333333333333000081, 0.6666666666667000474, 1.000000000000000000, 1.011997855551999947 ),
 ( -0.3559705542741999906, 1.355970554273999928 ),
 .UNSPECIFIED. ) ;
#28353 = CARTESIAN_POINT ( 'NONE',  ( -8.058765910997506055, -78.50948745952305785, -7.451450251813944270 ) ) ;
#28354 = EDGE_CURVE ( 'NONE', #40118, #6488, #12364, .T. ) ;
#28355 = CARTESIAN_POINT ( 'NONE',  ( 3.250000000000000000, -1.750000000000000000, 0.000000000000000000 ) ) ;
#28356 = ORIENTED_EDGE ( 'NONE', *, *, #7484, .F. ) ;
#28357 = ORIENTED_EDGE ( 'NONE', *, *, #28832, .T. ) ;
#28358 = CARTESIAN_POINT ( 'NONE',  ( -5.773189589619000195, -77.80318998579799938, 8.192511063987998554 ) ) ;
#28359 = CARTESIAN_POINT ( 'NONE',  ( 7.031078451151031139, -78.78178807021924968, -8.132049469059730029 ) ) ;
#28360 = VERTEX_POINT ( 'NONE', #5870 ) ;
#28361 = CARTESIAN_POINT ( 'NONE',  ( -1.250000000000000000, -18.75000000000000000, -12.00000000000000000 ) ) ;
#28362 = CARTESIAN_POINT ( 'NONE',  ( -7.678698829008310689, -79.34948846491148799, 5.593101447762748535 ) ) ;
#28363 = CARTESIAN_POINT ( 'NONE',  ( 9.389195554442999025, -61.51043214172000262, 8.194863653299998774 ) ) ;
#28364 = CARTESIAN_POINT ( 'NONE',  ( 11.86917441439930521, -76.78081435538106803, -2.820429242449539853 ) ) ;
#28365 = B_SPLINE_CURVE_WITH_KNOTS ( 'NONE', 3,
 ( #36486, #5206, #8751, #14052, #32047, #36776, #26741, #50091, #9636, #4322, #41214, #9050, #54795, #13463, #32334, #22323, #50381, #31459 ),
 .UNSPECIFIED., .F., .F.,
 ( 4, 2, 2, 2, 2, 2, 2, 2, 4 ),
 ( 0.000000000000000000, 0.1250000000000000000, 0.2500000000000000000, 0.3750000000000000000, 0.5000000000000000000, 0.6250000000000000000, 0.7500000000000000000, 0.8750000000000000000, 1.000000000000000000 ),
 .UNSPECIFIED. ) ;
#28366 = CARTESIAN_POINT ( 'NONE',  ( 0.9627606596332135558, -78.18130562541935547, -11.94123457856478510 ) ) ;
#28367 = CARTESIAN_POINT ( 'NONE',  ( -4.019809786096000259, -79.17027272495799650, 10.47183077952999852 ) ) ;
#28368 = ORIENTED_EDGE ( 'NONE', *, *, #4311, .F. ) ;
#28369 = CARTESIAN_POINT ( 'NONE',  ( -7.624341764926000131, -23.26485149464000202, 10.42531124853000080 ) ) ;
#28370 = AXIS2_PLACEMENT_3D ( 'NONE', #23211, #523, #22631 ) ;
#28371 = ORIENTED_EDGE ( 'NONE', *, *, #15370, .F. ) ;
#28372 = CARTESIAN_POINT ( 'NONE',  ( 8.239502079663772349, -77.38765822479125234, 4.203768253517201181 ) ) ;
#28373 = CARTESIAN_POINT ( 'NONE',  ( -4.789974786805000662, -78.07974131713798727, -9.946872946892002076 ) ) ;
#28374 = FACE_OUTER_BOUND ( 'NONE', #51485, .T. ) ;
#28375 = B_SPLINE_CURVE_WITH_KNOTS ( 'NONE', 3,
 ( #38305, #15585, #51620, #20028, #29151, #56327, #20879, #20598, #37727, #38598, #2601, #15878, #51326, #51902, #38882, #11459, #29436, #47490, #47198, #56612, #11744, #25018, #10883, #16170, #2028, #34148, #6728, #42168, #52188, #28856, #56037, #29722, #47772, #1736, #7305, #25306, #43325, #2883, #24736, #56902, #32991, #51036, #38013, #10584, #46615, #6142, #24150, #19730, #55748, #15292, #6433, #33286, #46907, #24447, #42462, #49200, #44471, #31162, #39170, #57469, #30009, #4323, #48912, #8752, #4022, #7878, #3739, #26742, #12312, #13164, #30878, #35014, #3175, #39746, #30300, #22027, #21459, #8453, #48064, #21165, #44192, #40035 ),
 .UNSPECIFIED., .F., .F.,
 ( 4, 2, 2, 2, 2, 2, 2, 2, 1, 1, 1, 2, 2, 2, 2, 2, 1, 1, 1, 2, 2, 2, 2, 2, 2, 2, 1, 1, 1, 1, 2, 2, 2, 2, 2, 1, 1, 1, 1, 2, 2, 2, 2, 2, 2, 2, 2, 4 ),
 ( 0.000000000000000000, 0.01562499999999716893, 0.03124999999999433786, 0.04687499999999150679, 0.06249999999998866185, 0.09374999999998295808, 0.1093749999999800993, 0.1171874999999786837, 0.1210937499999779760, 0.1230468749999776290, 0.1240234374999774764, 0.1245117187499773931, 0.1249999999999773237, 0.1874999999999681088, 0.2187499999999635014, 0.2343749999999611144, 0.2421874999999600042, 0.2460937499999593936, 0.2480468749999591160, 0.2490234374999589773, 0.2499999999999588662, 0.3749999999999662492, 0.4999999999999736877, 0.6249999999999811262, 0.6874999999999849010, 0.7187499999999867883, 0.7343749999999877875, 0.7421874999999883427, 0.7460937499999885647, 0.7480468749999886757, 0.7490234374999887867, 0.7499999999999887867, 0.8124999999999883427, 0.8437499999999881206, 0.8593749999999880096, 0.8671874999999881206, 0.8710937499999880096, 0.8730468749999880096, 0.8740234374999881206, 0.8745117187499881206, 0.8749999999999881206, 0.9062499999999911182, 0.9218749999999925615, 0.9374999999999941158, 0.9531249999999955591, 0.9687499999999971134, 0.9843749999999985567, 1.000000000000000000 ),
 .UNSPECIFIED. ) ;
#28376 = CARTESIAN_POINT ( 'NONE',  ( 1.190716386653000169, -78.80095245453999553, 1.090600000265000036 ) ) ;
#28377 = CARTESIAN_POINT ( 'NONE',  ( -10.99980394231345926, -80.10023817985064909, 1.711188753626703361E-06 ) ) ;
#28378 = CARTESIAN_POINT ( 'NONE',  ( 1.788035749175998834, -2.171010677132999334, -2.743726783948167380 ) ) ;
#28379 = CARTESIAN_POINT ( 'NONE',  ( 1.153380192234999990, -78.52349661904999323, 1.148206073167999941 ) ) ;
#28380 = CARTESIAN_POINT ( 'NONE',  ( -4.094030986447999787, -78.76507046129088963, -0.8031144277722999103 ) ) ;
#28381 = CARTESIAN_POINT ( 'NONE',  ( 4.619608356761999879, -78.76949559976999637, 9.917007359391000421 ) ) ;
#28382 = CARTESIAN_POINT ( 'NONE',  ( -7.606021324597999289, -23.42158946275000275, -10.52692925327000140 ) ) ;
#28383 = CARTESIAN_POINT ( 'NONE',  ( 12.75763395697999947, -59.57795407677000554, -1.931043742978000077 ) ) ;
#28384 = CARTESIAN_POINT ( 'NONE',  ( 1.925748864890999945, -85.22456467766599530, -2.978768362480000320 ) ) ;
#28385 = VERTEX_POINT ( 'NONE', #14721 ) ;
#28386 = CARTESIAN_POINT ( 'NONE',  ( 9.218059003579000432, -79.06486808225800189, -8.343706100361000466 ) ) ;
#28387 = VECTOR ( 'NONE', #8126, 1000.000000000000114 ) ;
#28388 = CARTESIAN_POINT ( 'NONE',  ( -0.5839839591423000575, -79.42548989939000137, -1.474617623361999863 ) ) ;
#28389 = CARTESIAN_POINT ( 'NONE',  ( 9.954879088412631916, -77.88099781617175665, 4.068718871676561655 ) ) ;
#28390 = CARTESIAN_POINT ( 'NONE',  ( 10.69384760718000038, -78.27889574609699253, -5.399785902169999652 ) ) ;
#28391 = CARTESIAN_POINT ( 'NONE',  ( -8.533817832784000856, -16.99473856456000220, 9.213092693308000847 ) ) ;
#28392 = CIRCLE ( 'NONE', #54796, 1.199999999999999956 ) ;
#28393 = CARTESIAN_POINT ( 'NONE',  ( -1.113300763112903935, -78.29084682967156539, -0.6200230202612950769 ) ) ;
#28394 = CARTESIAN_POINT ( 'NONE',  ( 0.6142349777637159391, -3.110991548698613496, 3.465482938499039545 ) ) ;
#28395 = CARTESIAN_POINT ( 'NONE',  ( 9.474936504858838759, -80.88936561845106610, 5.078570178447623817 ) ) ;
#28396 = CARTESIAN_POINT ( 'NONE',  ( 7.653824198668000456, -78.77973936012098477, -5.479973919995999587 ) ) ;
#28398 = EDGE_CURVE ( 'NONE', #19870, #23895, #5990, .T. ) ;
#28397 = CARTESIAN_POINT ( 'NONE',  ( -3.308356911591993743, -85.80681307385599155, 1.472975398279013692 ) ) ;
#28399 = CARTESIAN_POINT ( 'NONE',  ( 6.035973157159999936, -78.69886817601300777, -8.925829823522999362 ) ) ;
#28400 = CARTESIAN_POINT ( 'NONE',  ( -11.94395460750000204, -77.13131020466720145, 2.857367593729999822 ) ) ;
#28401 = CARTESIAN_POINT ( 'NONE',  ( -3.148499409464999843, -80.85690832509547477, 10.56665097621000093 ) ) ;
#28402 = VERTEX_POINT ( 'NONE', #51348 ) ;
#28403 = CARTESIAN_POINT ( 'NONE',  ( 6.233047529871999615, -78.88050366622999832, 9.960502923565000444 ) ) ;
#28404 = CARTESIAN_POINT ( 'NONE',  ( -10.46965315338386482, -80.57920048190398177, 2.813976240919467298 ) ) ;
#28405 = CARTESIAN_POINT ( 'NONE',  ( 6.201912463541000342, -78.50617185603199744, -9.171216270948999494 ) ) ;
#28406 = CARTESIAN_POINT ( 'NONE',  ( 9.981840466370998755, -78.59367011377399592, 4.563647388395000171 ) ) ;
#28407 = CARTESIAN_POINT ( 'NONE',  ( -12.80090744918999945, -22.76232687447999936, 1.980532734072999901 ) ) ;
#28408 = CARTESIAN_POINT ( 'NONE',  ( -1.313693873217006924, -84.40416666804125612, 3.833116371664651023 ) ) ;
#28409 = CARTESIAN_POINT ( 'NONE',  ( 1.996168837740194935, -1.924424498446639209, 2.598685398968098248 ) ) ;
#28410 = CARTESIAN_POINT ( 'NONE',  ( -7.610436392397138761, -55.27459049263858759, -10.41144384037119153 ) ) ;
#28411 = CARTESIAN_POINT ( 'NONE',  ( 0.2924848206110000071, -85.07292953870899055, -4.161850282066000162 ) ) ;
#28412 = CARTESIAN_POINT ( 'NONE',  ( -1.500000000000000000, -80.50000000000000000, 0.000000000000000000 ) ) ;
#28413 = EDGE_CURVE ( 'NONE', #22110, #29384, #32718, .T. ) ;
#28414 = CARTESIAN_POINT ( 'NONE',  ( 11.00823205989000009, -78.70025095962000705, -6.817946738202000034 ) ) ;
#28415 = PRESENTATION_LAYER_ASSIGNMENT (  '', '', ( #53896 ) ) ;
#28416 = CARTESIAN_POINT ( 'NONE',  ( 9.181220278661999856, -77.47743860894799184, -6.522205052974000772 ) ) ;
#28417 = CARTESIAN_POINT ( 'NONE',  ( -0.8981901762082999952, -79.85007741978999718, -1.403037214508999986 ) ) ;
#28418 = CARTESIAN_POINT ( 'NONE',  ( -12.00000000000000000, -76.79999999999999716, 1.164316068523999942E-14 ) ) ;
#28419 = CARTESIAN_POINT ( 'NONE',  ( -1.980584515752000119, -60.06485146591000301, 12.76303204605000197 ) ) ;
#28420 = CARTESIAN_POINT ( 'NONE',  ( -1.135826688880000157, -81.30663953507000485, -0.9797437077257000748 ) ) ;
#28421 = DIRECTION ( 'NONE',  ( 0.000000000000000000, 1.000000000000000000, 0.000000000000000000 ) ) ;
#28422 = ORIENTED_EDGE ( 'NONE', *, *, #44653, .T. ) ;
#28423 = CARTESIAN_POINT ( 'NONE',  ( -5.869402599192000025, -78.46567021303999923, 10.46661899222999992 ) ) ;
#28424 = CARTESIAN_POINT ( 'NONE',  ( -0.6296721830724527624, -81.01735300594884848, 1.093406895717950800 ) ) ;
#28425 = EDGE_CURVE ( 'NONE', #6475, #1066, #41601, .T. ) ;
#28426 = ORIENTED_EDGE ( 'NONE', *, *, #11328, .T. ) ;
#28427 = CARTESIAN_POINT ( 'NONE',  ( -1.153358918101035524, -81.63163289808623801, -0.4816960858994225880 ) ) ;
#28428 = FILL_AREA_STYLE ('',( #10442 ) ) ;
#28429 = EDGE_CURVE ( 'NONE', #11038, #19532, #56265, .T. ) ;
#28430 = CARTESIAN_POINT ( 'NONE',  ( 10.71899861749000138, -79.68986664982399759, -2.608601736514999825 ) ) ;
#28431 = DIRECTION ( 'NONE',  ( -1.000000000000000000, 0.000000000000000000, 0.000000000000000000 ) ) ;
#28432 = EDGE_LOOP ( 'NONE', ( #47782, #37728, #23909 ) ) ;
#28433 = ORIENTED_EDGE ( 'NONE', *, *, #52693, .T. ) ;
#28434 = CARTESIAN_POINT ( 'NONE',  ( -0.2464170302977999882, -82.21284346265900922, -1.305809855734000102 ) ) ;
#28435 = VERTEX_POINT ( 'NONE', #20055 ) ;
#28436 = CARTESIAN_POINT ( 'NONE',  ( 7.624341764926000131, -23.26485149464000202, -10.42531124853000080 ) ) ;
#28437 = VERTEX_POINT ( 'NONE', #28882 ) ;
#28438 = AXIS2_PLACEMENT_3D ( 'NONE', #47420, #55379, #46256 ) ;
#28439 = CARTESIAN_POINT ( 'NONE',  ( 1.798368564625000054, -18.80363242954000214, 12.61278090841000044 ) ) ;
#28440 = CYLINDRICAL_SURFACE ( 'NONE', #53737, 3.250000000000000000 ) ;
#28441 = SHAPE_DEFINITION_REPRESENTATION ( #11610, #4074 ) ;
#28442 = CARTESIAN_POINT ( 'NONE',  ( 2.942028868608097536, -80.81979165559693001, -1.791020663990882111 ) ) ;
#28443 = CARTESIAN_POINT ( 'NONE',  ( 12.00000000000000000, -76.54999999999999716, 0.000000000000000000 ) ) ;
#28444 = CARTESIAN_POINT ( 'NONE',  ( 3.546526562939293914, -78.25635398785173891, -8.543071106479906973 ) ) ;
#28445 = CARTESIAN_POINT ( 'NONE',  ( -10.07627163191000008, -55.55000000209000177, 7.601397897754999633 ) ) ;
#28446 = VERTEX_POINT ( 'NONE', #46931 ) ;
#28447 = ORIENTED_EDGE ( 'NONE', *, *, #31708, .T. ) ;
#28448 = CARTESIAN_POINT ( 'NONE',  ( -7.603718805262172253, -77.55178371867702936, 5.267967937869231676 ) ) ;
#28449 = CARTESIAN_POINT ( 'NONE',  ( -10.00716890277074356, -76.94696047196750044, -6.699252482692386934 ) ) ;
#28450 = LINE ( 'NONE', #27862, #30789 ) ;
#28451 = EDGE_CURVE ( 'NONE', #31238, #42268, #43986, .T. ) ;
#28452 = CARTESIAN_POINT ( 'NONE',  ( -5.051502324002999760E-14, -80.79999999999999716, 0.000000000000000000 ) ) ;
#28453 = CARTESIAN_POINT ( 'NONE',  ( 1.882180247600000245, -78.62931555891299240, 9.519879562373999349 ) ) ;
#28454 = DIRECTION ( 'NONE',  ( 0.000000000000000000, -1.000000000000000000, 0.000000000000000000 ) ) ;
#28455 = CARTESIAN_POINT ( 'NONE',  ( 3.440052570659030806, -85.82990816067768947, 1.702406959663651076 ) ) ;
#28456 = CARTESIAN_POINT ( 'NONE',  ( -11.87139580924456439, -77.31341727770499972, -2.023209039049734148 ) ) ;
#28457 = CARTESIAN_POINT ( 'NONE',  ( 0.5769282351073999893, -80.98621153953999396, 1.350407801515999928 ) ) ;
#28458 = CARTESIAN_POINT ( 'NONE',  ( -7.011176471748147954, -77.49139693750339575, 6.331528591067105971 ) ) ;
#28459 = COLOUR_RGB ( '', 0.31764706, 0.68627451, 0.89019608) ;
#28460 = CARTESIAN_POINT ( 'NONE',  ( -4.074342574665000605, -81.80899506498398921, -0.9106826699133000469 ) ) ;
#28461 = CARTESIAN_POINT ( 'NONE',  ( -10.18948933931000234, -55.58467389893999666, 7.645397892281000196 ) ) ;
#28462 = CARTESIAN_POINT ( 'NONE',  ( 9.685875573750999834, -78.82196001420199138, 0.1582452683012000039 ) ) ;
#28463 = CARTESIAN_POINT ( 'NONE',  ( -10.47023603244697121, -76.62094508224406297, -2.813753789789203541 ) ) ;
#28464 = CARTESIAN_POINT ( 'NONE',  ( -7.618394506893999996, -18.77286435802000142, -10.53494428259999971 ) ) ;
#28466 = CARTESIAN_POINT ( 'NONE',  ( 0.9834589317531000630, -79.07467101249899599, 0.9007689179829999615 ) ) ;
#28465 = CARTESIAN_POINT ( 'NONE',  ( -1.199500263597274241, -78.84791666666667709, 0.9218200799623669228 ) ) ;
#28467 = LINE ( 'NONE', #24049, #9107 ) ;
#28468 = CARTESIAN_POINT ( 'NONE',  ( 1.500000000000000000, -77.75000000000000000, 0.000000000000000000 ) ) ;
#28469 = DIRECTION ( 'NONE',  ( 0.000000000000000000, -1.000000000000000000, 0.000000000000000000 ) ) ;
#28470 = CARTESIAN_POINT ( 'NONE',  ( 8.097270260564613409, -77.19999999999998863, -7.230186543639936403 ) ) ;
#28471 = VERTEX_POINT ( 'NONE', #56350 ) ;
#28472 = CARTESIAN_POINT ( 'NONE',  ( 9.505949683908001546, -79.00000000000000000, -6.906476714433999575 ) ) ;
#28473 = DIRECTION ( 'NONE',  ( 0.000000000000000000, 0.000000000000000000, -1.000000000000000000 ) ) ;
#28474 = CARTESIAN_POINT ( 'NONE',  ( 5.918882701593904727, -77.53100531885093005, 10.27291346163489827 ) ) ;
#28475 = CARTESIAN_POINT ( 'NONE',  ( 12.77297283019000140, -61.52822696498000710, -1.476112654660999723 ) ) ;
#28476 = FACE_OUTER_BOUND ( 'NONE', #15889, .T. ) ;
#28477 = CONICAL_SURFACE ( 'NONE', #21853, 13.94999999959000014, 0.7853981633972997312 ) ;
#28478 = CARTESIAN_POINT ( 'NONE',  ( -9.287618194362000423, -77.50975265977999129, -9.114789584104999065 ) ) ;
#28479 = CARTESIAN_POINT ( 'NONE',  ( 10.75000000000000000, -79.35000000000000853, 0.000000000000000000 ) ) ;
#28480 = CARTESIAN_POINT ( 'NONE',  ( 0.7999999999999001243, -18.84999999997999964, 12.00000000000000000 ) ) ;
#28481 = ADVANCED_FACE ( 'NONE', ( #2337 ), #56637, .F. ) ;
#28482 = DIRECTION ( 'NONE',  ( -0.009503199022040095811, 0.000000000000000000, 0.9999548435846228323 ) ) ;
#28483 = CARTESIAN_POINT ( 'NONE',  ( 6.642950389325999794, -77.35432768747699583, -9.109179383135000307 ) ) ;
#28484 = EDGE_CURVE ( 'NONE', #30832, #38602, #12872, .T. ) ;
#28485 = CARTESIAN_POINT ( 'NONE',  ( 0.9960226344442998370, -81.53517859526800748, -1.129973388342000007 ) ) ;
#28486 = CARTESIAN_POINT ( 'NONE',  ( -0.1807450410261203788, -81.98705298514224182, 1.237523090201967157 ) ) ;
#28487 = DIRECTION ( 'NONE',  ( -0.7071067811865474617, 0.000000000000000000, 0.7071067811865474617 ) ) ;
#28489 = LINE ( 'NONE', #15213, #37676 ) ;
#28488 = CARTESIAN_POINT ( 'NONE',  ( 3.450559865080999877, -85.26804551122299358, 1.949262422280000129 ) ) ;
#28490 = CARTESIAN_POINT ( 'NONE',  ( 1.813979036992999783, -79.42974805011499484, 9.381055131006998948 ) ) ;
#28491 = CARTESIAN_POINT ( 'NONE',  ( 1.250000000000000222, -82.73958333333331439, -0.1636246173744659582 ) ) ;
#28492 = FACE_BOUND ( 'NONE', #30755, .T. ) ;
#28493 = CARTESIAN_POINT ( 'NONE',  ( -6.217716982067981846, -77.17607982036621195, -8.769278404477413247 ) ) ;
#28494 = DIRECTION ( 'NONE',  ( 0.000000000000000000, 1.000000000000000000, 0.000000000000000000 ) ) ;
#28495 = VECTOR ( 'NONE', #17685, 1000.000000000000000 ) ;
#28496 = ORIENTED_EDGE ( 'NONE', *, *, #2208, .T. ) ;
#28497 = EDGE_LOOP ( 'NONE', ( #40655, #31178, #48065, #11838 ) ) ;
#28498 = CARTESIAN_POINT ( 'NONE',  ( -0.7406579117306999471, -79.51379700229598768, 12.00660533699000077 ) ) ;
#28499 = DIRECTION ( 'NONE',  ( -1.000000000000000000, 0.000000000000000000, 0.000000000000000000 ) ) ;
#28500 = EDGE_CURVE ( 'NONE', #23510, #49361, #25755, .T. ) ;
#28501 = CYLINDRICAL_SURFACE ( 'NONE', #20899, 12.50000000000000000 ) ;
#28502 = ORIENTED_EDGE ( 'NONE', *, *, #9972, .T. ) ;
#28503 = CARTESIAN_POINT ( 'NONE',  ( -11.81636186152999990, -78.63462189577700201, -1.676035442350999993 ) ) ;
#28504 = ORIENTED_EDGE ( 'NONE', *, *, #20260, .T. ) ;
#28505 = ORIENTED_EDGE ( 'NONE', *, *, #25016, .T. ) ;
#28506 = CARTESIAN_POINT ( 'NONE',  ( 5.413904038987143785, -78.83333333333330017, 9.393203674808290771 ) ) ;
#28507 = ORIENTED_EDGE ( 'NONE', *, *, #25555, .T. ) ;
#28508 = CARTESIAN_POINT ( 'NONE',  ( 3.499206421942000045, -80.89818977615198037, -0.5806240443371000204 ) ) ;
#28509 = CARTESIAN_POINT ( 'NONE',  ( 10.45204383628000144, -56.03743350618999841, 7.651147548114000330 ) ) ;
#28510 = B_SPLINE_CURVE_WITH_KNOTS ( 'NONE', 3,
 ( #14685, #29139, #19133, #37128, #28844, #32395 ),
 .UNSPECIFIED., .F., .F.,
 ( 4, 2, 4 ),
 ( 0.000000000000000000, 0.5000000000000000000, 1.000000000000000000 ),
 .UNSPECIFIED. ) ;
#28511 = VERTEX_POINT ( 'NONE', #38327 ) ;
#28512 = CARTESIAN_POINT ( 'NONE',  ( 0.8982459645321505537, -82.78945047064037510, -0.8686774761259995481 ) ) ;
#28513 = CARTESIAN_POINT ( 'NONE',  ( -7.668936932630000314, -56.02847221959000024, 10.21380041493999968 ) ) ;
#28514 = ORIENTED_EDGE ( 'NONE', *, *, #44103, .F. ) ;
#28515 = CARTESIAN_POINT ( 'NONE',  ( -9.248792011962317261, -79.11076594009642804, -1.210867610392123428 ) ) ;
#28516 = CARTESIAN_POINT ( 'NONE',  ( 9.131180374627371421, -77.57241948081694716, -3.285631257141331307 ) ) ;
#28517 = AXIS2_PLACEMENT_3D ( 'NONE', #16561, #52289, #19835 ) ;
#28518 = CARTESIAN_POINT ( 'NONE',  ( 1.035792215605076949, -79.80000000000001137, -11.73450628681306718 ) ) ;
#28519 = CARTESIAN_POINT ( 'NONE',  ( -10.62888400727746863, -80.08839518812462188, 1.609190229725424803 ) ) ;
#28520 = CARTESIAN_POINT ( 'NONE',  ( -1.307248514406967876, -79.06671355138394119, -12.19422169117518173 ) ) ;
#28521 = CARTESIAN_POINT ( 'NONE',  ( -1.959694873104000257, -77.35881901538978411, -9.504225410855001499 ) ) ;
#28522 = CARTESIAN_POINT ( 'NONE',  ( -5.007180289739999068, -76.61025844654599837, 10.00009952528999868 ) ) ;
#28523 = CARTESIAN_POINT ( 'NONE',  ( 7.550822941564469204, -76.41427617356011126, 7.692254321527583372 ) ) ;
#28524 = AXIS2_PLACEMENT_3D ( 'NONE', #3564, #55932, #55633 ) ;
#28525 = CARTESIAN_POINT ( 'NONE',  ( -10.90146613631999983, -76.81059650580800735, 1.770589923316999936 ) ) ;
#28526 = CARTESIAN_POINT ( 'NONE',  ( -5.129512087222791727, -78.67834954393102009, -7.697348747938988822 ) ) ;
#28527 = CARTESIAN_POINT ( 'NONE',  ( 4.546247888304588258, -76.54303117012038626, 10.83464402558239037 ) ) ;
#28528 = CARTESIAN_POINT ( 'NONE',  ( 0.6529096706351000812, -77.20118501420199664, -9.388848551955000232 ) ) ;
#28529 = CARTESIAN_POINT ( 'NONE',  ( 0.2659376973789999710, -79.77531449030800559, -1.306848610430999980 ) ) ;
#28530 = CARTESIAN_POINT ( 'NONE',  ( -5.704086182078374812, -80.18177924709463866, -9.405421966457751637 ) ) ;
#28531 = CARTESIAN_POINT ( 'NONE',  ( 1.001315002657000131, -61.48522411647999775, -12.50000000000000000 ) ) ;
#28532 = CARTESIAN_POINT ( 'NONE',  ( 3.952128152273000516, -79.16303455456849747, 0.2943874864100000099 ) ) ;
#28533 = CARTESIAN_POINT ( 'NONE',  ( 4.882231352572000027, -77.52591332859900319, 8.326888637120999803 ) ) ;
#28534 = AXIS2_PLACEMENT_3D ( 'NONE', #49632, #19205, #41346 ) ;
#28535 = CARTESIAN_POINT ( 'NONE',  ( 8.474185241649847100, -76.24531250000731575, 8.471026285512541776 ) ) ;
#28536 = CARTESIAN_POINT ( 'NONE',  ( 0.09741388862448860375, -82.96925805188962499, 1.246036882942684887 ) ) ;
#28537 = SURFACE_SIDE_STYLE ('',( #10554 ) ) ;
#28538 = CARTESIAN_POINT ( 'NONE',  ( -3.548349909811000291, -78.96264282632948550, -1.488874400533411562E-14 ) ) ;
#28539 = CARTESIAN_POINT ( 'NONE',  ( 0.000000000000000000, -2.900000000000000355, 0.000000000000000000 ) ) ;
#28540 = CARTESIAN_POINT ( 'NONE',  ( 1.570796326794856590, -79.26458333333330586, 12.00000000000000711 ) ) ;
#28541 = LINE ( 'NONE', #15266, #45145 ) ;
#28542 = CARTESIAN_POINT ( 'NONE',  ( 1.210555553064095236, -79.73586375669722770, -9.250525361423333592 ) ) ;
#28543 = CARTESIAN_POINT ( 'NONE',  ( 12.74331206681030793, -23.52649290803818616, -1.980611467279665305 ) ) ;
#28544 = CARTESIAN_POINT ( 'NONE',  ( -1.301142965806426632, -79.80676480095245040, 0.7731589486237497866 ) ) ;
#28545 = DIRECTION ( 'NONE',  ( 1.000000000000000000, 0.000000000000000000, 0.000000000000000000 ) ) ;
#28546 = CARTESIAN_POINT ( 'NONE',  ( 5.279327442448000340, -79.18212748368000575, -7.780650776298999816 ) ) ;
#28547 = FACE_OUTER_BOUND ( 'NONE', #34247, .T. ) ;
#28548 = CARTESIAN_POINT ( 'NONE',  ( 8.500000000000000000, -73.00000000000001421, 0.000000000000000000 ) ) ;
#28549 = CARTESIAN_POINT ( 'NONE',  ( 0.4965625967630000193, -77.24519064797900114, 12.26984941905000071 ) ) ;
#28550 = CARTESIAN_POINT ( 'NONE',  ( 3.303001513109999898, -78.99932466030405465, -10.46681410870000128 ) ) ;
#28551 = CARTESIAN_POINT ( 'NONE',  ( 8.894005208714999000, -76.35846261908999111, -8.368406312348000142 ) ) ;
#28552 = ORIENTED_EDGE ( 'NONE', *, *, #52260, .F. ) ;
#28553 = CARTESIAN_POINT ( 'NONE',  ( -3.579657239220000342, -86.47871544543099276, 0.3914039778855000207 ) ) ;
#28554 = CARTESIAN_POINT ( 'NONE',  ( -7.478374335766999614, -80.70849464549387164, 8.611710654069998583 ) ) ;
#28555 = EDGE_CURVE ( 'NONE', #14936, #31290, #21479, .T. ) ;
#28556 = CARTESIAN_POINT ( 'NONE',  ( 8.164293671790550988, -78.31111438883360165, -4.349583488888277394 ) ) ;
#28557 = CARTESIAN_POINT ( 'NONE',  ( -1.500000000000000000, -81.50000000000000000, 0.000000000000000000 ) ) ;
#28558 = CARTESIAN_POINT ( 'NONE',  ( -6.659967121051000305, -76.97609495320099882, -9.025682433062998555 ) ) ;
#28559 = CARTESIAN_POINT ( 'NONE',  ( 9.998727717461520115, -23.92738947620295065, -7.709134076961339233 ) ) ;
#28560 = CARTESIAN_POINT ( 'NONE',  ( 0.8552902072924000176, -78.52513851832499370, -9.592793577801000282 ) ) ;
#28561 = CIRCLE ( 'NONE', #33279, 1.000000000000000000 ) ;
#28562 = CARTESIAN_POINT ( 'NONE',  ( 3.805232043948999721, -82.38490367749800214, -1.402234496399000108 ) ) ;
#28563 = CARTESIAN_POINT ( 'NONE',  ( -8.414570695956999913, -59.94999999967000548, -8.414570695956999913 ) ) ;
#28564 = CARTESIAN_POINT ( 'NONE',  ( -10.87500000000999911, -76.17499999999400018, 1.221063213659000093E-09 ) ) ;
#28565 = ORIENTED_EDGE ( 'NONE', *, *, #22726, .T. ) ;
#28566 = DIRECTION ( 'NONE',  ( -1.000000000000000000, 0.000000000000000000, 0.000000000000000000 ) ) ;
#28567 = CARTESIAN_POINT ( 'NONE',  ( 10.24999999991999999, -82.10000000007899246, -6.817370023903000320E-10 ) ) ;
#28568 = DIRECTION ( 'NONE',  ( 0.6489586469528968449, -0.04890178981565979077, -0.7592504787603958638 ) ) ;
#28569 = ORIENTED_EDGE ( 'NONE', *, *, #3092, .F. ) ;
#28570 = CARTESIAN_POINT ( 'NONE',  ( -0.1765672563250000049, -78.24877223242859259, -1.321892640673999919 ) ) ;
#28571 = AXIS2_PLACEMENT_3D ( 'NONE', #25891, #43918, #3464 ) ;
#28572 = ADVANCED_FACE ( 'NONE', ( #39487 ), #25328, .F. ) ;
#28573 = CARTESIAN_POINT ( 'NONE',  ( 10.42531125074000009, -18.73514854687000053, 7.624341767140999870 ) ) ;
#28574 = ORIENTED_EDGE ( 'NONE', *, *, #35443, .T. ) ;
#28575 = CARTESIAN_POINT ( 'NONE',  ( 7.024610939158000278, -78.93285191714500115, -9.931634882699999167 ) ) ;
#28576 = CARTESIAN_POINT ( 'NONE',  ( 0.5884124957372001141, -77.49171607516498739, 11.41734628011000119 ) ) ;
#28577 = DIRECTION ( 'NONE',  ( -0.4045837979900098746, 0.8201365135195225475, -0.4045837979900098746 ) ) ;
#28578 = ORIENTED_EDGE ( 'NONE', *, *, #29087, .F. ) ;
#28579 = ORIENTED_EDGE ( 'NONE', *, *, #28398, .T. ) ;
#28580 = CONICAL_SURFACE ( 'NONE', #34255, 9.400000000000000355, 0.7853981633972997312 ) ;
#28581 = CARTESIAN_POINT ( 'NONE',  ( -1.156113623258839818, -80.56903096784071749, 0.4752053836311996848 ) ) ;
#28582 = CIRCLE ( 'NONE', #25724, 5.100000000000000533 ) ;
#28583 = CARTESIAN_POINT ( 'NONE',  ( -9.392812284823671476, -77.64167586065022419, -5.413627597448644302 ) ) ;
#28584 = CARTESIAN_POINT ( 'NONE',  ( 9.534323188421000239, -79.07183379231298659, -1.008198710029000189 ) ) ;
#28585 = ORIENTED_EDGE ( 'NONE', *, *, #15251, .F. ) ;
#28586 = CARTESIAN_POINT ( 'NONE',  ( 12.66737112512999985, -54.56697834100999955, 1.690666607834999891 ) ) ;
#28587 = CARTESIAN_POINT ( 'NONE',  ( 9.697372265328400687, -24.97233735039882063, -8.266620275706634047 ) ) ;
#28588 = ORIENTED_EDGE ( 'NONE', *, *, #13535, .T. ) ;
#28589 = CARTESIAN_POINT ( 'NONE',  ( -12.77651047016999897, -25.30895689136000115, 0.04321256188109000307 ) ) ;
#28590 = DIRECTION ( 'NONE',  ( -1.000000000000000000, 0.000000000000000000, 0.000000000000000000 ) ) ;
#28591 = CARTESIAN_POINT ( 'NONE',  ( -12.00000000000000000, -60.04999999966999980, 0.000000000000000000 ) ) ;
#28592 = CARTESIAN_POINT ( 'NONE',  ( -1.135996409638392768, -80.13451362626204855, -0.5214161241409958070 ) ) ;
#28593 = CARTESIAN_POINT ( 'NONE',  ( -1.217390015621637067, -17.18106975071298237, -12.70229597940931399 ) ) ;
#28594 = CARTESIAN_POINT ( 'NONE',  ( -12.70395600760253352, -17.39327811307525451, -1.447166682405202298 ) ) ;
#28595 = CARTESIAN_POINT ( 'NONE',  ( 1.321891224999238723, -78.64195268641222469, 0.7850651250095550537 ) ) ;
#28596 = CARTESIAN_POINT ( 'NONE',  ( 1.828892197797149732, -82.18802085116996636, -3.571177028183664337 ) ) ;
#28597 = CARTESIAN_POINT ( 'NONE',  ( 1.623944433304999935, -76.11819529704000331, -12.20239005717999881 ) ) ;
#28598 = CARTESIAN_POINT ( 'NONE',  ( -1.024999350969000078, -80.97513535138099883, -1.157050009743000096 ) ) ;
#28599 = EDGE_CURVE ( 'NONE', #14715, #54222, #43636, .T. ) ;
#28600 = CARTESIAN_POINT ( 'NONE',  ( 9.500000000000001776, -78.13958333333333428, -1.243547092045940827 ) ) ;
#28601 = CARTESIAN_POINT ( 'NONE',  ( 10.18949719147000010, -60.01529250184999853, -7.645392405676999736 ) ) ;
#28602 = CARTESIAN_POINT ( 'NONE',  ( -5.531768889155999958, -79.13976085113000636, -10.94525552207000096 ) ) ;
#28603 = CARTESIAN_POINT ( 'NONE',  ( -11.38972971424999869, -76.66439794286800691, -4.593112662244999811 ) ) ;
#28604 = CARTESIAN_POINT ( 'NONE',  ( 12.70228859454079817, -17.17803615246131699, -1.213484947661823909 ) ) ;
#28605 = EDGE_CURVE ( 'NONE', #55607, #31248, #52468, .T. ) ;
#28606 = CARTESIAN_POINT ( 'NONE',  ( 12.50657368821661741, -24.97245458995924849, 0.3553454087122077110 ) ) ;
#28607 = CARTESIAN_POINT ( 'NONE',  ( 10.49970183384550637, -78.34114056985468721, 5.963879664039239969 ) ) ;
#28608 = CARTESIAN_POINT ( 'NONE',  ( -1.639962962630000076, -78.63667686873010609, 11.09633417262999977 ) ) ;
#28609 = CIRCLE ( 'NONE', #21991, 9.000000000000000000 ) ;
#28610 = B_SPLINE_SURFACE_WITH_KNOTS ( 'NONE', 3, 3, ( 
 ( #45549, #27508, #13939, #19253, #36668, #31641, #980, #18677, #50267, #54401, #10108, #28089, #18092, #49978, #5094, #13646, #54969, #41103, #46139, #31935, #49684, #14808, #4802, #32802, #28381, #41686, #23090, #50850, #54104, #37247, #45253, #27215, #32224, #18382, #55260, #14519, #10396, #9230, #9521, #9814, #46427, #40814, #5958, #22803, #695, #27799, #23959, #404, #54685, #14226, #36375, #45844, #5378, #23386, #1265, #32511, #41397, #18965, #5663, #23672, #36957, #50556, #42857, #56144, #56433, #15693, #6245 ),
 ( #33100, #2417, #29831, #1845, #47600, #24552, #37537, #20419, #38414, #34262, #29544, #7126, #6543, #20134, #52293, #11853, #33688, #47882, #47305, #10698, #47013, #28675, #25126, #55552, #42566, #7413, #20704, #1549, #15984, #55852, #46728, #10989, #25418, #2132, #37832, #24262, #43150, #38121, #15405, #19540, #52012, #38702, #51726, #19837, #2709, #56724, #28970, #42278, #15102, #11278, #16281, #29256, #51143, #33397, #51436, #6831, #33974, #24843, #11566, #58158, #43431, #39280, #39570, #8861, #44291, #26276, #35407 ),
 ( #20989, #35120, #44010, #49016, #40146, #21844, #39851, #35712, #57867, #25700, #57002, #2990, #53153, #31269, #3846, #53741, #48731, #52866, #16855, #34549, #17420, #30119, #3281, #12700, #17136, #30695, #43729, #8274, #21564, #57572, #7986, #8563, #53438, #52581, #44582, #12980, #30978, #26553, #4139, #13276, #49311, #38994, #16565, #48169, #30410, #12132, #7700, #21273, #57291, #34836, #25984, #12421, #48445, #3560, #4733, #41, #26853, #5019, #910, #54621, #41326, #5589, #18017, #18894, #36009, #14448, #9742 ),
 ( #54035, #27730, #5311, #46067, #32443, #28022, #23602, #25403, #43718, #4127, #16844, #52570, #43419, #3838, #57280, #12121, #26546, #26266, #53428, #21263, #34537, #44279, #21836, #3271, #56992, #44572, #52854, #39841, #3550, #17413, #35396, #57856, #12971, #12690, #30106, #30969, #49006, #16269, #48157, #12408, #40138, #17124, #57562, #8554, #53143, #21553, #22127, #52283, #39558, #34826, #34248, #11839, #30684, #29820, #47870, #7400, #16554, #2978, #20977, #38981, #7688, #39269, #30398, #5010, #9152, #31557, #49303 ) ),
 .UNSPECIFIED., .F., .F., .F.,
 ( 4, 4 ),
 ( 4, 1, 1, 1, 1, 1, 1, 1, 1, 1, 1, 1, 1, 1, 1, 1, 1, 1, 1, 1, 1, 1, 1, 1, 1, 1, 1, 1, 1, 1, 1, 1, 1, 1, 1, 1, 1, 1, 1, 1, 1, 1, 1, 1, 1, 1, 1, 1, 1, 1, 1, 1, 1, 1, 1, 1, 1, 1, 1, 1, 1, 1, 1, 1, 4 ),
 ( -0.1387574078320000237, 1.138757407831999968 ),
 ( -0.02000000000000000042, -0.003749999999999999861, 0.01250000000000000069, 0.02875000000000000125, 0.04499999999999999833, 0.06124999999999999889, 0.07749999999999999944, 0.09375000000000000000, 0.1100000000000000006, 0.1262500000000000011, 0.1424999999999999878, 0.1587500000000000022, 0.1749999999999999889, 0.1912500000000000033, 0.2074999999999999900, 0.2237500000000000044, 0.2399999999999999911, 0.2562499999999999778, 0.2725000000000000200, 0.2887500000000000067, 0.3049999999999999933, 0.3212499999999999800, 0.3375000000000000222, 0.3537500000000000089, 0.3699999999999999956, 0.3862499999999999822, 0.4025000000000000244, 0.4187500000000000111, 0.4349999999999999978, 0.4512499999999999845, 0.4675000000000000266, 0.4837500000000000133, 0.5000000000000000000, 0.5162499999999999867, 0.5324999999999999734, 0.5487499999999999600, 0.5649999999999999467, 0.5812500000000000444, 0.5975000000000000311, 0.6137500000000000178, 0.6300000000000000044, 0.6462499999999999911, 0.6624999999999999778, 0.6787499999999999645, 0.6949999999999999512, 0.7112500000000000488, 0.7275000000000000355, 0.7437500000000000222, 0.7600000000000000089, 0.7762499999999999956, 0.7924999999999999822, 0.8087499999999999689, 0.8249999999999999556, 0.8412500000000000533, 0.8575000000000000400, 0.8737500000000000266, 0.8900000000000000133, 0.9062500000000000000, 0.9224999999999999867, 0.9387499999999999734, 0.9549999999999999600, 0.9712499999999999467, 0.9875000000000000444, 1.003749999999999920, 1.020000000000000018 ),
 .UNSPECIFIED. ) ;
#28611 = ORIENTED_EDGE ( 'NONE', *, *, #41967, .T. ) ;
#28612 = CARTESIAN_POINT ( 'NONE',  ( -1.167146675921293397, -81.19530117510119283, 0.9583584161384303135 ) ) ;
#28613 = CARTESIAN_POINT ( 'NONE',  ( -3.564835704203999978, -77.29834088185198482, 8.912408990994999058 ) ) ;
#28614 = CARTESIAN_POINT ( 'NONE',  ( -1.250000000000000000, -79.50000000000000000, 0.000000000000000000 ) ) ;
#28615 = CARTESIAN_POINT ( 'NONE',  ( -1.500000000000000000, -79.50000000000000000, 0.000000000000000000 ) ) ;
#28616 = CARTESIAN_POINT ( 'NONE',  ( 1.712913800556999933, -3.546465114847999978, -3.088999176916999989 ) ) ;
#28617 = CARTESIAN_POINT ( 'NONE',  ( -1.845833107322000011, -77.89610176985598855, 11.90750485256000069 ) ) ;
#28618 = CARTESIAN_POINT ( 'NONE',  ( -9.212293474215000444, -77.23048492307799506, -2.808383990684999887 ) ) ;
#28620 = CARTESIAN_POINT ( 'NONE',  ( 1.179538764136264906, -77.83344348886518560, -11.01565543437853734 ) ) ;
#28619 = CARTESIAN_POINT ( 'NONE',  ( -8.304425937606323416, -76.13746526952284910, 8.312567492877647624 ) ) ;
#28621 = CARTESIAN_POINT ( 'NONE',  ( -1.232656909444999949, -82.61361845526398895, -0.5536498640889000455 ) ) ;
#28622 = CARTESIAN_POINT ( 'NONE',  ( -2.375816180258422339, -85.94828564506400426, 3.206979491545860039 ) ) ;
#28623 = EDGE_LOOP ( 'NONE', ( #19713, #21050, #35759, #40045 ) ) ;
#28624 = CARTESIAN_POINT ( 'NONE',  ( 12.71162862750088429, -24.23964265628594106, 1.720599174827327271 ) ) ;
#28625 = CARTESIAN_POINT ( 'NONE',  ( -11.77263653225999995, -79.73881804294899212, 3.029873667130000392 ) ) ;
#28626 = CARTESIAN_POINT ( 'NONE',  ( -8.414570695956999913, -55.64999999967000122, -8.414570695956999913 ) ) ;
#28627 = EDGE_CURVE ( 'NONE', #57022, #37791, #32738, .T. ) ;
#28628 = DIRECTION ( 'NONE',  ( 0.000000000000000000, -1.000000000000000000, 0.000000000000000000 ) ) ;
#28629 = CARTESIAN_POINT ( 'NONE',  ( 0.1291013223160000223, -79.36451833177198978, 10.97485077029999978 ) ) ;
#28630 = FACE_OUTER_BOUND ( 'NONE', #14355, .T. ) ;
#28631 = CARTESIAN_POINT ( 'NONE',  ( -0.09587540347749000380, -79.70338829707398531, -9.559386592703999597 ) ) ;
#28632 = CARTESIAN_POINT ( 'NONE',  ( 7.943801774166999508, -17.56598212471000053, -9.641153612788999183 ) ) ;
#28633 = CARTESIAN_POINT ( 'NONE',  ( -8.096452064242996016, -56.01421830980998351, -13.15643568217000769 ) ) ;
#28634 = VERTEX_POINT ( 'NONE', #43345 ) ;
#28635 = CARTESIAN_POINT ( 'NONE',  ( 5.768896245881999896, -78.60879439517700007, 9.672321370914000127 ) ) ;
#28636 = CARTESIAN_POINT ( 'NONE',  ( -7.695151247652856519, -76.28527187395242493, 8.115589632975689582 ) ) ;
#28637 = DIRECTION ( 'NONE',  ( -1.000000000000000000, 0.000000000000000000, 0.000000000000000000 ) ) ;
#28638 = CARTESIAN_POINT ( 'NONE',  ( 1.974456470848842127, -78.67390000031815589, 3.418760428718723432 ) ) ;
#28639 = CARTESIAN_POINT ( 'NONE',  ( -11.27280967271781797, -77.92393960097702177, 4.319288305624113811 ) ) ;
#28640 = CARTESIAN_POINT ( 'NONE',  ( -0.3912638815494142719, -81.50038330625253025, 1.190242956311802214 ) ) ;
#28641 = ADVANCED_FACE ( 'NONE', ( #2901 ), #26660, .F. ) ;
#28642 = CARTESIAN_POINT ( 'NONE',  ( 10.93175546140675003, -79.11789353073278619, 2.513629148400740032 ) ) ;
#28643 = CARTESIAN_POINT ( 'NONE',  ( -12.50745077485999879, -53.80005551680000053, 2.011910316382000212E-09 ) ) ;
#28644 = CARTESIAN_POINT ( 'NONE',  ( -9.298479816475497373, -17.11187382770906495, -8.385858173857444697 ) ) ;
#28645 = EDGE_CURVE ( 'NONE', #28865, #33521, #14454, .T. ) ;
#28646 = CARTESIAN_POINT ( 'NONE',  ( 1.075065877797000136, -78.28180136235999953, -0.7449938779133999933 ) ) ;
#28647 = CARTESIAN_POINT ( 'NONE',  ( 12.00000000000000000, -78.54999999999999716, 0.000000000000000000 ) ) ;
#28648 = CARTESIAN_POINT ( 'NONE',  ( 7.219097972577888100, -79.26798102650505484, 8.267553648188542326 ) ) ;
#28649 = AXIS2_PLACEMENT_3D ( 'NONE', #1008, #42601, #50881 ) ;
#28650 = CARTESIAN_POINT ( 'NONE',  ( -9.596002108778193929, -77.24791666666666856, 7.374560639698935383 ) ) ;
#28651 = VERTEX_POINT ( 'NONE', #44211 ) ;
#28652 = ORIENTED_EDGE ( 'NONE', *, *, #23912, .F. ) ;
#28653 = CARTESIAN_POINT ( 'NONE',  ( 2.951189771924322081, -77.75000000000000000, 9.074256859245707574 ) ) ;
#28654 = CARTESIAN_POINT ( 'NONE',  ( 7.210467705727123366, -78.78352963214712190, -7.974047016889574735 ) ) ;
#28655 = EDGE_LOOP ( 'NONE', ( #44140, #8321, #25688 ) ) ;
#28656 = CLOSED_SHELL ( 'NONE', ( #3963, #56165, #47598, #16034, #11345, #48640, #11754, #16727, #19934, #8294, #49705, #906, #46031, #41844, #15104, #12248, #49212, #25621, #33808, #48368, #50981, #858, #18126, #16155, #56348, #28019, #44155, #48889, #4788, #12486, #11782, #46635, #11377, #23841, #6249, #19369, #8176, #53206, #20973, #8665, #11907, #48032, #14875, #35397, #33668, #27818, #46428, #40592, #51176, #21446, #56823, #48414, #19382, #41269, #51972, #31674, #54591, #17789, #47077 ) ) ;
#28657 = CARTESIAN_POINT ( 'NONE',  ( 7.631896578932000352, -18.77877526479000281, 10.36221705164000184 ) ) ;
#28658 = ADVANCED_FACE ( 'NONE', ( #53067 ), #35492, .T. ) ;
#28659 = DIRECTION ( 'NONE',  ( 0.000000000000000000, -1.000000000000000000, 0.000000000000000000 ) ) ;
#28660 = CARTESIAN_POINT ( 'NONE',  ( 4.671825910118999836, -78.48810965511999882, -11.12032239270999945 ) ) ;
#28661 = CARTESIAN_POINT ( 'NONE',  ( 10.13402523426999835, -60.52303809408999768, 7.647751776506999555 ) ) ;
#28662 = CARTESIAN_POINT ( 'NONE',  ( 4.628805853411431137, -76.70534887877106200, -11.28743898164479553 ) ) ;
#28663 = CARTESIAN_POINT ( 'NONE',  ( -10.61611263540728700, -78.58824535677541689, -5.551409177842876019 ) ) ;
#28664 = CARTESIAN_POINT ( 'NONE',  ( -2.710423231297999891, -79.72831545226699745, 10.88447134676999895 ) ) ;
#28665 = EDGE_LOOP ( 'NONE', ( #35170, #28214, #53623, #12503 ) ) ;
#28666 = DIRECTION ( 'NONE',  ( 1.000000000000000000, 0.000000000000000000, 0.000000000000000000 ) ) ;
#28667 = ORIENTED_EDGE ( 'NONE', *, *, #39224, .T. ) ;
#28668 = CARTESIAN_POINT ( 'NONE',  ( 8.786704849164062026, -77.37533117377390113, 2.890659873118438306 ) ) ;
#28669 = CARTESIAN_POINT ( 'NONE',  ( 2.976905979876097952, -77.49628357046933047, -10.81478801228704079 ) ) ;
#28670 = CARTESIAN_POINT ( 'NONE',  ( 7.405962610586999340, -77.58454441596599338, -6.270759699041999369 ) ) ;
#28671 = CARTESIAN_POINT ( 'NONE',  ( -9.998734510784624163, -18.07263061081724942, -7.709128441133644927 ) ) ;
#28672 = CARTESIAN_POINT ( 'NONE',  ( 7.374560639698994002, -78.57708333333330586, -9.596002108778151296 ) ) ;
#28673 = CARTESIAN_POINT ( 'NONE',  ( -1.472167250137000005, -78.92387186976999658, -0.6938203229310999642 ) ) ;
#28674 = ADVANCED_FACE ( 'NONE', ( #40951 ), #39766, .F. ) ;
#28675 = CARTESIAN_POINT ( 'NONE',  ( 11.01715842067999951, -78.74909427755598301, 0.8367281403419999375 ) ) ;
#28676 = CARTESIAN_POINT ( 'NONE',  ( 12.71005379442530980, -61.09489531493035486, 1.687596142995509974 ) ) ;
#28677 = CIRCLE ( 'NONE', #55072, 1.000000000000000000 ) ;
#28678 = CARTESIAN_POINT ( 'NONE',  ( 12.69619287811999797, -58.55083378327000077, -1.799475295154000065 ) ) ;
#28679 = CARTESIAN_POINT ( 'NONE',  ( 3.544514315405999927, -85.39601319073598518, 0.03727608545351999980 ) ) ;
#28680 = EDGE_LOOP ( 'NONE', ( #41575, #24162, #39120, #11331 ) ) ;
#28681 = CARTESIAN_POINT ( 'NONE',  ( -10.19334857974716790, -77.19999999999998863, 4.001455984208257988 ) ) ;
#28682 = CARTESIAN_POINT ( 'NONE',  ( -11.59066951726000028, -76.28147497528598819, -0.7123197670545999838 ) ) ;
#28683 = CARTESIAN_POINT ( 'NONE',  ( 10.47042279852835200, -77.86824023481268853, 2.435997539233151876 ) ) ;
#28684 = CARTESIAN_POINT ( 'NONE',  ( 0.4844284812283000119, -77.50567552123600024, 11.97002061314999999 ) ) ;
#28685 = CARTESIAN_POINT ( 'NONE',  ( -9.621742410712839089, -54.17938299872298558, 8.060146970971464597 ) ) ;
#28686 = CIRCLE ( 'NONE', #53183, 12.05000000000000071 ) ;
#28687 = CARTESIAN_POINT ( 'NONE',  ( -0.3253823571070225129, -78.35445332720156841, -1.233148206733681862 ) ) ;
#28688 = CARTESIAN_POINT ( 'NONE',  ( 2.965694224434944903, -3.454766459150870439, -1.895013073882325205 ) ) ;
#28689 = DIRECTION ( 'NONE',  ( 0.000000000000000000, 0.000000000000000000, 1.000000000000000000 ) ) ;
#28690 = CARTESIAN_POINT ( 'NONE',  ( -6.563619111649000359, -77.64278619496199951, -6.747599474233999750 ) ) ;
#28691 = CARTESIAN_POINT ( 'NONE',  ( -3.451879464910993622, -85.80681307243298761, 1.536875756006014448 ) ) ;
#28692 = CARTESIAN_POINT ( 'NONE',  ( -8.585712843602999911, -77.90483863155199629, 6.927284413728999724 ) ) ;
#28693 = DIRECTION ( 'NONE',  ( -1.000000000000000000, 0.000000000000000000, 0.000000000000000000 ) ) ;
#28694 = CARTESIAN_POINT ( 'NONE',  ( 4.099300690538000502, -80.87094001750114103, 10.11134612214000050 ) ) ;
#28695 = ORIENTED_EDGE ( 'NONE', *, *, #22742, .T. ) ;
#28696 = CARTESIAN_POINT ( 'NONE',  ( -0.9200108141794000050, -81.78630577039299965, -0.9654823929056000065 ) ) ;
#28697 = CIRCLE ( 'NONE', #3251, 0.5000000000000004441 ) ;
#28698 = CARTESIAN_POINT ( 'NONE',  ( -11.75162232059617295, -78.71241119902158800, -1.843960194169528943 ) ) ;
#28699 = CARTESIAN_POINT ( 'NONE',  ( 9.662374122931806752, -80.38663027733564093, 4.763869651305610020 ) ) ;
#28700 = CARTESIAN_POINT ( 'NONE',  ( 2.976864594307000011, -77.41248104968700261, -10.81463766284999828 ) ) ;
#28701 = CARTESIAN_POINT ( 'NONE',  ( 9.632126701410999914, -79.09933249176198444, 5.261763182588000021 ) ) ;
#28702 = CARTESIAN_POINT ( 'NONE',  ( 7.633089125616000281, -23.39007426303999893, -10.18115018432999896 ) ) ;
#28703 = CARTESIAN_POINT ( 'NONE',  ( -0.04117230827835093726, -84.32708333387819266, 4.051288899054856785 ) ) ;
#28704 = CARTESIAN_POINT ( 'NONE',  ( 4.525754325328000149, -76.92122343098399995, 11.27843493294999888 ) ) ;
#28705 = DIRECTION ( 'NONE',  ( 0.000000000000000000, 1.000000000000000000, 0.000000000000000000 ) ) ;
#28706 = B_SPLINE_CURVE_WITH_KNOTS ( 'NONE', 3,
 ( #46104, #32480, #37213, #28936, #54653, #24227, #55226, #14772, #32771, #50818, #1811, #46396, #36922, #19806, #5060, #9779, #37800, #10361, #5344, #55821, #27768, #54934, #45810, #23353, #18930, #50523, #28347, #5922, #19509, #23927, #41946, #1517, #20382, #34510, #33653, #11815, #42822, #52541, #51693, #21239, #34224, #52258, #38956 ),
 .UNSPECIFIED., .F., .F.,
 ( 4, 2, 2, 2, 2, 1, 2, 2, 1, 2, 2, 1, 1, 1, 1, 2, 2, 1, 1, 1, 1, 2, 2, 1, 2, 2, 4 ),
 ( 0.000000000000000000, 0.06250000000000005551, 0.1250000000000001110, 0.1875000000000001665, 0.2500000000000002220, 0.3125000000000002776, 0.3437500000000001665, 0.3750000000000001110, 0.4375000000000001110, 0.4687500000000001665, 0.5000000000000002220, 0.5625000000000002220, 0.5937500000000003331, 0.6093750000000003331, 0.6171875000000003331, 0.6210937500000003331, 0.6250000000000003331, 0.6875000000000003331, 0.7187500000000004441, 0.7343750000000004441, 0.7421875000000004441, 0.7460937500000004441, 0.7500000000000004441, 0.8125000000000003331, 0.8437500000000003331, 0.8750000000000002220, 1.000000000000000000 ),
 .UNSPECIFIED. ) ;
#28707 = ORIENTED_EDGE ( 'NONE', *, *, #11589, .T. ) ;
#28708 = CARTESIAN_POINT ( 'NONE',  ( -0.6859742521509630819, -80.02179400559481337, 1.045181947014915069 ) ) ;
#28709 = CARTESIAN_POINT ( 'NONE',  ( 0.1963495408493571015, -80.36458333333331439, 1.500000000000000444 ) ) ;
#28710 = CARTESIAN_POINT ( 'NONE',  ( 7.956418361354000268, -54.27110680110000374, -9.787952249823998585 ) ) ;
#28711 = CARTESIAN_POINT ( 'NONE',  ( -3.257558841711999609, -76.87823906290799414, -10.78064358917000121 ) ) ;
#28712 = CARTESIAN_POINT ( 'NONE',  ( -1.603789611582999930, -80.35140824942999416, -0.4506860216877000558 ) ) ;
#28713 = CARTESIAN_POINT ( 'NONE',  ( 0.1259833764099000109, -78.82466101900999433, 1.429058429169000055 ) ) ;
#28714 = CARTESIAN_POINT ( 'NONE',  ( 7.374560639698954034, -77.62291666666666856, 9.596002108778181494 ) ) ;
#28715 = CARTESIAN_POINT ( 'NONE',  ( -1.338255681671218333, -81.71150629859762660, 0.7046537140460734649 ) ) ;
#28716 = CARTESIAN_POINT ( 'NONE',  ( -13.94241845804000057, -32.46002936525999871, -4.312607201059000272E-05 ) ) ;
#28717 = ORIENTED_EDGE ( 'NONE', *, *, #563, .F. ) ;
#28718 = CYLINDRICAL_SURFACE ( 'NONE', #7954, 4.100000000000000533 ) ;
#28719 = DIRECTION ( 'NONE',  ( 0.000000000000000000, -1.000000000000000000, 0.000000000000000000 ) ) ;
#28720 = ORIENTED_EDGE ( 'NONE', *, *, #54655, .T. ) ;
#28721 = CARTESIAN_POINT ( 'NONE',  ( -1.057559559974387886, -81.64527973143721340, -0.6673670114133440912 ) ) ;
#28722 =( LENGTH_UNIT ( ) NAMED_UNIT ( * ) SI_UNIT ( .MILLI., .METRE. ) );
#28723 = CARTESIAN_POINT ( 'NONE',  ( -8.243938165231000426, -80.01670276584620467, -7.330703780023000604 ) ) ;
#28724 = LINE ( 'NONE', #1312, #52548 ) ;
#28725 = ORIENTED_EDGE ( 'NONE', *, *, #46673, .T. ) ;
#28726 = ORIENTED_EDGE ( 'NONE', *, *, #39380, .F. ) ;
#28727 = CARTESIAN_POINT ( 'NONE',  ( 0.7077020876660000681, -81.71095816450198868, -1.340932479011999856 ) ) ;
#28728 = TOROIDAL_SURFACE ( 'NONE', #9909, 1.250000000000000000, 0.5000000000000000000 ) ;
#28729 = ORIENTED_EDGE ( 'NONE', *, *, #23694, .T. ) ;
#28730 = VERTEX_POINT ( 'NONE', #22048 ) ;
#28731 = CARTESIAN_POINT ( 'NONE',  ( 0.005119011380136999703, -17.06186137810999881, 12.43705489344000092 ) ) ;
#28732 = LINE ( 'NONE', #6600, #16910 ) ;
#28733 = PRODUCT_CONTEXT ( 'NONE', #40183, 'mechanical' ) ;
#28734 = ADVANCED_FACE ( 'NONE', ( #35322 ), #39391, .F. ) ;
#28735 = CARTESIAN_POINT ( 'NONE',  ( -0.8546198232617973067, -82.01458331760134968, -3.302194718003578888 ) ) ;
#28736 = VECTOR ( 'NONE', #22253, 1000.000000000000000 ) ;
#28737 = CARTESIAN_POINT ( 'NONE',  ( 7.138081588315396075, -78.29522891051385614, -5.883131579888745577 ) ) ;
#28738 = DIRECTION ( 'NONE',  ( 0.000000000000000000, -1.000000000000000000, 0.000000000000000000 ) ) ;
#28739 = ORIENTED_EDGE ( 'NONE', *, *, #372, .T. ) ;
#28740 = ORIENTED_EDGE ( 'NONE', *, *, #41511, .F. ) ;
#28741 = CARTESIAN_POINT ( 'NONE',  ( -9.136481091602316695, -77.58766093786633178, 1.444190332375185903 ) ) ;
#28742 = CARTESIAN_POINT ( 'NONE',  ( -0.6747260877994001316, -82.25000000000000000, -1.052256958371999840 ) ) ;
#28743 = CARTESIAN_POINT ( 'NONE',  ( 1.811016405462491541, -60.86173555339116348, -12.71771640067482601 ) ) ;
#28744 = CARTESIAN_POINT ( 'NONE',  ( -2.183112477083999803, -77.66290536852798709, 9.455407409464999802 ) ) ;
#28745 = CARTESIAN_POINT ( 'NONE',  ( 0.000000000000000000, -23.15000000000000213, 12.00000000000000000 ) ) ;
#28746 = CARTESIAN_POINT ( 'NONE',  ( -8.596418555780431348, -76.55208333333331439, -6.606377239730338857 ) ) ;
#28747 = DIRECTION ( 'NONE',  ( 0.000000000000000000, -1.000000000000000000, 0.000000000000000000 ) ) ;
#28748 = ADVANCED_FACE ( 'NONE', ( #44433, #3418, #26412, #31422, #17872, #4285 ), #9012, .T. ) ;
#28749 = CARTESIAN_POINT ( 'NONE',  ( -0.3234604031741999952, -79.66018296954999300, 1.671883997359000062 ) ) ;
#28750 = CARTESIAN_POINT ( 'NONE',  ( -7.305413871501877487, -77.60449693750338440, -5.989639219614036669 ) ) ;
#28751 = CARTESIAN_POINT ( 'NONE',  ( -8.064342063058008492, -76.63498362770486949, 8.546452962956790245 ) ) ;
#28752 = CARTESIAN_POINT ( 'NONE',  ( 4.046592612395000010, -82.41509632510098982, -0.2667223080253999790 ) ) ;
#28753 = CARTESIAN_POINT ( 'NONE',  ( -1.300212205372666130, -79.70741581913885909, 0.7726441571383775297 ) ) ;
#28754 = CARTESIAN_POINT ( 'NONE',  ( 6.533310722863999942, -79.19368667140099660, -6.649273783659000792 ) ) ;
#28755 = CARTESIAN_POINT ( 'NONE',  ( -7.374560639699019760, -77.32708333333330586, 9.596002108778129980 ) ) ;
#28756 = FACE_OUTER_BOUND ( 'NONE', #22562, .T. ) ;
#28758 = CARTESIAN_POINT ( 'NONE',  ( 0.5390150933986999071, -16.73739108348000215, -12.77520261005000002 ) ) ;
#28757 = CARTESIAN_POINT ( 'NONE',  ( -1.500000000000000444, -78.88958333333333428, 0.1963495408493560745 ) ) ;
#28759 = DIRECTION ( 'NONE',  ( 1.000000000000000000, 0.000000000000000000, 0.000000000000000000 ) ) ;
#28760 = FACE_OUTER_BOUND ( 'NONE', #15, .T. ) ;
#28761 = EDGE_CURVE ( 'NONE', #27335, #27676, #17569, .T. ) ;
#28762 = CARTESIAN_POINT ( 'NONE',  ( -11.18527010467000160, -78.31411136276199159, 1.312896411821999898 ) ) ;
#28763 = FACE_OUTER_BOUND ( 'NONE', #18511, .T. ) ;
#28764 = EDGE_LOOP ( 'NONE', ( #52886, #17261, #8247, #21744 ) ) ;
#28765 = CARTESIAN_POINT ( 'NONE',  ( 9.102117851719468078, -61.77186524099414555, 8.583692175706325145 ) ) ;
#28766 = EDGE_CURVE ( 'NONE', #36712, #3531, #33491, .T. ) ;
#28767 = DIRECTION ( 'NONE',  ( 0.000000000000000000, -1.000000000000000000, 0.000000000000000000 ) ) ;
#28768 = AXIS2_PLACEMENT_3D ( 'NONE', #58336, #791, #35288 ) ;
#28769 = CARTESIAN_POINT ( 'NONE',  ( 1.226351938740054770, -78.36563631113473605, 0.2418696441422709953 ) ) ;
#28770 = AXIS2_PLACEMENT_3D ( 'NONE', #16996, #39133, #4286 ) ;
#28771 = CARTESIAN_POINT ( 'NONE',  ( -7.722420941044000564, -79.94415467088899163, -5.774298730193000218 ) ) ;
#28772 = DIRECTION ( 'NONE',  ( 0.000000000000000000, -1.000000000000000000, 0.000000000000000000 ) ) ;
#28773 = DIRECTION ( 'NONE',  ( 0.000000000000000000, 1.000000000000000000, 0.000000000000000000 ) ) ;
#28774 = CARTESIAN_POINT ( 'NONE',  ( -0.0004935696944198294904, -79.47512061975739073, 10.74992982259620078 ) ) ;
#28775 = CIRCLE ( 'NONE', #18430, 4.000000000000000000 ) ;
#28776 = CARTESIAN_POINT ( 'NONE',  ( -6.207771380439999653, -79.37311332859900403, 7.503906557766999441 ) ) ;
#28777 = CARTESIAN_POINT ( 'NONE',  ( 0.000000000000000000, -76.00000000000000000, -11.70000000000000107 ) ) ;
#28778 = CARTESIAN_POINT ( 'NONE',  ( 10.96222314295999922, -77.91600195789497718, -1.826653240149999968 ) ) ;
#28779 = CARTESIAN_POINT ( 'NONE',  ( -1.489949360950307389, -76.31481021185051361, -11.66158060881517855 ) ) ;
#28780 = CARTESIAN_POINT ( 'NONE',  ( 1.060702322374999840, -81.59055028299499668, -1.203351566307999887 ) ) ;
#28781 = CARTESIAN_POINT ( 'NONE',  ( 8.219513559211000242, -78.94484514476064874, 5.194554602171000290 ) ) ;
#28782 = CARTESIAN_POINT ( 'NONE',  ( -1.000000000000000000, -81.99999999999998579, 7.000000000000000000 ) ) ;
#28784 = CARTESIAN_POINT ( 'NONE',  ( -11.75000000000000000, -76.30000000000001137, 1.487410190129999909E-14 ) ) ;
#28783 = CARTESIAN_POINT ( 'NONE',  ( -3.929695901009000458, -84.42629260435599292, -0.5133031271695001063 ) ) ;
#28785 = CARTESIAN_POINT ( 'NONE',  ( -2.364557222828000072, -79.58505584965399748, 9.257622954664000758 ) ) ;
#28786 = CARTESIAN_POINT ( 'NONE',  ( 0.1636246173744697330, -82.63541666666665719, -1.249999999999999778 ) ) ;
#28787 = CARTESIAN_POINT ( 'NONE',  ( 5.169396783903556170, -80.26528074669050739, -9.426735840945569933 ) ) ;
#28788 = CARTESIAN_POINT ( 'NONE',  ( -6.587136192994185180, -77.17264154318887392, -8.498578688690102467 ) ) ;
#28789 = CARTESIAN_POINT ( 'NONE',  ( 1.478685787649352434, -79.59375000137556810, -9.318529369750295999 ) ) ;
#28790 = ORIENTED_EDGE ( 'NONE', *, *, #58126, .F. ) ;
#28791 = ORIENTED_EDGE ( 'NONE', *, *, #44976, .F. ) ;
#28792 = CARTESIAN_POINT ( 'NONE',  ( 11.66950233118999947, -79.36437884805799570, -2.920592611544999606 ) ) ;
#28793 = CARTESIAN_POINT ( 'NONE',  ( -12.50745077494999968, -61.79994448255000350, -2.661703094427999907E-09 ) ) ;
#28794 = CARTESIAN_POINT ( 'NONE',  ( -10.07627163191000008, -60.04999999657000131, 7.601397897754999633 ) ) ;
#28795 = VERTEX_POINT ( 'NONE', #19035 ) ;
#28796 = CARTESIAN_POINT ( 'NONE',  ( 4.441925970415999458, -77.46806133255499560, 11.07721969470000190 ) ) ;
#28797 = ORIENTED_EDGE ( 'NONE', *, *, #8092, .T. ) ;
#28798 = ORIENTED_EDGE ( 'NONE', *, *, #12741, .T. ) ;
#28799 = CARTESIAN_POINT ( 'NONE',  ( 8.150146600852364642, -60.21532333328941178, 7.387512494710262168 ) ) ;
#28800 = ORIENTED_EDGE ( 'NONE', *, *, #12317, .T. ) ;
#28801 = CARTESIAN_POINT ( 'NONE',  ( 2.971188159787999883, -79.56916961237898533, 1.938195294252000211 ) ) ;
#28802 = CARTESIAN_POINT ( 'NONE',  ( 7.704680120202406890, -79.19943945225395510, 5.557390998954779171 ) ) ;
#28803 = EDGE_LOOP ( 'NONE', ( #33592, #29549, #24508, #54457 ) ) ;
#28804 = CARTESIAN_POINT ( 'NONE',  ( 0.000000000000000000, 0.000000000000000000, -8.800000000000000711 ) ) ;
#28805 = EDGE_LOOP ( 'NONE', ( #2437, #17677, #17036, #39618 ) ) ;
#28806 = CARTESIAN_POINT ( 'NONE',  ( -7.640030139739999449, -55.49283065365000311, 10.18491068058999893 ) ) ;
#28807 = ORIENTED_EDGE ( 'NONE', *, *, #19715, .F. ) ;
#28808 = CARTESIAN_POINT ( 'NONE',  ( 1.407171709420440342, -80.63541666666665719, -10.74999999999999822 ) ) ;
#28809 = CARTESIAN_POINT ( 'NONE',  ( -1.406533682220601156, -78.22053972881499817, 0.5448426528144166836 ) ) ;
#28810 = DIRECTION ( 'NONE',  ( 0.000000000000000000, 0.000000000000000000, -1.000000000000000000 ) ) ;
#28811 = CARTESIAN_POINT ( 'NONE',  ( -10.61509443659918084, -80.08771556321305241, 1.696495127445934559 ) ) ;
#28812 = DIRECTION ( 'NONE',  ( 0.000000000000000000, 1.000000000000000000, 0.000000000000000000 ) ) ;
#28813 = CARTESIAN_POINT ( 'NONE',  ( 7.890274420948999001, -78.95055344661277275, -5.649267206311999523 ) ) ;
#28814 = CARTESIAN_POINT ( 'NONE',  ( 11.01994305158000031, -76.50247340589800160, -1.906499110313000234 ) ) ;
#28815 = CYLINDRICAL_SURFACE ( 'NONE', #53173, 12.05000000000000071 ) ;
#28816 = ADVANCED_FACE ( 'NONE', ( #45328 ), #9747, .F. ) ;
#28817 = CARTESIAN_POINT ( 'NONE',  ( 4.923701317394000299, -76.48453125995000335, -10.09162495054999908 ) ) ;
#28818 = CARTESIAN_POINT ( 'NONE',  ( -3.201792520036055301, -78.69701081001878151, -8.678388619861092224 ) ) ;
#28819 = CARTESIAN_POINT ( 'NONE',  ( 8.318733234480337302, -76.51185634578514794, 8.297783748491672995 ) ) ;
#28820 = CARTESIAN_POINT ( 'NONE',  ( -1.248430190247999949, -79.21789842151099492, 0.06262635289305999720 ) ) ;
#28821 = DIRECTION ( 'NONE',  ( -1.000000000000000000, 0.000000000000000000, 0.000000000000000000 ) ) ;
#28822 = CARTESIAN_POINT ( 'NONE',  ( -2.531016240223846303, -3.046284654864954700, 2.042466395675148316 ) ) ;
#28823 = CARTESIAN_POINT ( 'NONE',  ( 2.236565090990000115, -78.92253455456848599, -3.018134580346000018 ) ) ;
#28824 = CARTESIAN_POINT ( 'NONE',  ( 8.035052034801999810, -79.89370463075219675, 9.025357223237000071 ) ) ;
#28825 = CARTESIAN_POINT ( 'NONE',  ( -9.232585280256000004, -78.05730742239006759, 5.508089239726199793 ) ) ;
#28826 = CARTESIAN_POINT ( 'NONE',  ( 0.01044744366229730971, -82.97494249513464126, 1.249636124618067834 ) ) ;
#28827 = DIRECTION ( 'NONE',  ( -0.7071067811864976127, 0.7071067811865975328, 1.047747575656995313E-09 ) ) ;
#28828 = CARTESIAN_POINT ( 'NONE',  ( -8.080493018338632538, -76.26413923100619741, -8.538429872746517546 ) ) ;
#28829 = CARTESIAN_POINT ( 'NONE',  ( 6.232755757386176043, -78.91383699956330133, 9.960036924250847079 ) ) ;
#28830 = CARTESIAN_POINT ( 'NONE',  ( -10.18114973714999927, -60.19009320380000361, -7.633087466122999487 ) ) ;
#28831 = CARTESIAN_POINT ( 'NONE',  ( -9.250175331044397709, -79.60562764437898409, -0.6054718526037866644 ) ) ;
#28832 = EDGE_CURVE ( 'NONE', #2323, #43690, #2773, .T. ) ;
#28833 = DIRECTION ( 'NONE',  ( 0.000000000000000000, 0.000000000000000000, -1.000000000000000000 ) ) ;
#28834 = CARTESIAN_POINT ( 'NONE',  ( 4.000000000000000000, -5.000000000000000000, 0.5999999999999999778 ) ) ;
#28835 = FACE_OUTER_BOUND ( 'NONE', #7469, .T. ) ;
#28836 = CARTESIAN_POINT ( 'NONE',  ( -7.635227771886311743, -23.76609606960563070, -10.36745004610104637 ) ) ;
#28837 = CARTESIAN_POINT ( 'NONE',  ( -10.74517267938467491, -77.94474881793972543, 0.7745379120455484490 ) ) ;
#28838 = CARTESIAN_POINT ( 'NONE',  ( 1.750000000001000089, -60.05000000958000328, 12.56594317859000043 ) ) ;
#28839 = CARTESIAN_POINT ( 'NONE',  ( 10.87588596538000019, -79.58926410129005546, -1.476184626237000863 ) ) ;
#28840 = CARTESIAN_POINT ( 'NONE',  ( 1.396436198717000199, -76.03442085042999565, 12.13192147124999920 ) ) ;
#28841 = ORIENTED_EDGE ( 'NONE', *, *, #26091, .T. ) ;
#28842 = CARTESIAN_POINT ( 'NONE',  ( -3.513940247509999892, -86.43863211209799147, 0.9924308411892999171 ) ) ;
#28843 = CARTESIAN_POINT ( 'NONE',  ( -7.401941616262999624, -80.64076758108089393, 8.523694671541999668 ) ) ;
#28844 = CARTESIAN_POINT ( 'NONE',  ( -7.850068285607218144, -17.68530314558974581, -9.837745660718102414 ) ) ;
#28845 = CARTESIAN_POINT ( 'NONE',  ( 2.273403379124000026E-14, -92.33215535459000023, 0.000000000000000000 ) ) ;
#28846 = CARTESIAN_POINT ( 'NONE',  ( 2.854969924326999919, -78.25620307428700073, 10.84745395576000071 ) ) ;
#28847 = CARTESIAN_POINT ( 'NONE',  ( -2.062673488738000049, -18.67547470641000018, -12.82904091339000097 ) ) ;
#28848 = CARTESIAN_POINT ( 'NONE',  ( -9.380647509327999956, -77.80751470757499533, 2.619761060131999830 ) ) ;
#28849 = CARTESIAN_POINT ( 'NONE',  ( -1.732827729967000074, -82.94607228207600258, 3.795241817643000282 ) ) ;
#28850 = CARTESIAN_POINT ( 'NONE',  ( 6.731009509123192736, -80.24817708364265911, -8.757207002688298658 ) ) ;
#28851 = CARTESIAN_POINT ( 'NONE',  ( 0.000000000000000000, -9.638971321655001034, 0.000000000000000000 ) ) ;
#28852 = EDGE_CURVE ( 'NONE', #15598, #42991, #48259, .T. ) ;
#28853 = ORIENTED_EDGE ( 'NONE', *, *, #26277, .F. ) ;
#28854 = AXIS2_PLACEMENT_3D ( 'NONE', #34358, #47692, #34647 ) ;
#28855 = LINE ( 'NONE', #1734, #4948 ) ;
#28856 = CARTESIAN_POINT ( 'NONE',  ( 2.366083363358619351, -78.97374669511339107, -2.683407710015649261 ) ) ;
#28857 = CONICAL_SURFACE ( 'NONE', #20397, 13.94999999959000014, 0.7853981633972997312 ) ;
#28858 = ORIENTED_EDGE ( 'NONE', *, *, #25049, .T. ) ;
#28859 = CIRCLE ( 'NONE', #2503, 1.749999999999999334 ) ;
#28860 = CARTESIAN_POINT ( 'NONE',  ( 0.2086861075963999945, -78.49683534933389240, 1.317203954600000060 ) ) ;
#28861 = CARTESIAN_POINT ( 'NONE',  ( 7.366954953549999630, -79.49001771131699456, -8.234431878459000487 ) ) ;
#28862 = CARTESIAN_POINT ( 'NONE',  ( 0.000000000000000000, -72.89999999999999147, 0.000000000000000000 ) ) ;
#28863 = CARTESIAN_POINT ( 'NONE',  ( -11.41214431921999939, -80.16675248214399119, 1.797791303879000102 ) ) ;
#28864 = AXIS2_PLACEMENT_3D ( 'NONE', #46879, #17813, #3928 ) ;
#28865 = VERTEX_POINT ( 'NONE', #11919 ) ;
#28866 = CARTESIAN_POINT ( 'NONE',  ( -4.148749056195000229, -78.66155876290798687, 11.43548913925000043 ) ) ;
#28867 = CARTESIAN_POINT ( 'NONE',  ( 3.831544248136000252, -77.96861728781497902, 10.77131813041000008 ) ) ;
#28868 = CARTESIAN_POINT ( 'NONE',  ( -4.763776579928164168, -77.51148305309406794, 9.662172649054632245 ) ) ;
#28869 = ORIENTED_EDGE ( 'NONE', *, *, #6959, .F. ) ;
#28870 = EDGE_CURVE ( 'NONE', #56311, #2750, #18590, .T. ) ;
#28871 = VERTEX_POINT ( 'NONE', #10768 ) ;
#28872 = CARTESIAN_POINT ( 'NONE',  ( -0.5074500732423817828, -80.50838598281532654, 1.142332835001032887 ) ) ;
#28873 = CARTESIAN_POINT ( 'NONE',  ( 7.374560639698954034, -79.62291666666662593, 9.596002108778181494 ) ) ;
#28874 = CARTESIAN_POINT ( 'NONE',  ( 8.193575559979001000, -79.42596350198101618, 5.316613930189999948 ) ) ;
#28875 = ORIENTED_EDGE ( 'NONE', *, *, #58265, .T. ) ;
#28876 = CARTESIAN_POINT ( 'NONE',  ( 12.54902617714999913, -53.79030198112999273, 0.4617931494615999943 ) ) ;
#28877 = CARTESIAN_POINT ( 'NONE',  ( -10.90697944550000109, -79.57677595101699808, -0.4616983494901999996 ) ) ;
#28878 = VERTEX_POINT ( 'NONE', #37903 ) ;
#28879 = CARTESIAN_POINT ( 'NONE',  ( -12.54981857173999948, -25.04836586201999893, 0.03768635776136999849 ) ) ;
#28880 = CARTESIAN_POINT ( 'NONE',  ( 1.529609450199000076, -76.87196915034600408, 9.371081266747001592 ) ) ;
#28881 = CARTESIAN_POINT ( 'NONE',  ( 3.872094496555182008, -82.58831665197764949, -0.8230422429851939059 ) ) ;
#28882 = CARTESIAN_POINT ( 'NONE',  ( 0.000000000000000000, -77.29999999999999716, -4.000000000000341949 ) ) ;
#28883 = CARTESIAN_POINT ( 'NONE',  ( -2.500000000000000000, -77.69999999999998863, 0.000000000000000000 ) ) ;
#28884 = B_SPLINE_CURVE_WITH_KNOTS ( 'NONE', 3,
 ( #14957, #6982, #56291, #51870, #51585, #56003, #47163, #1998, #20564, #33250, #16138, #41836, #2563, #34113, #19401, #11714, #42715, #29691 ),
 .UNSPECIFIED., .F., .F.,
 ( 4, 2, 2, 2, 2, 2, 2, 2, 4 ),
 ( 0.000000000000000000, 0.1250000000000000278, 0.2500000000000000555, 0.3750000000000001110, 0.5000000000000001110, 0.6250000000000001110, 0.7500000000000002220, 0.8750000000000001110, 1.000000000000000000 ),
 .UNSPECIFIED. ) ;
#28885 = EDGE_CURVE ( 'NONE', #35553, #38791, #4467, .T. ) ;
#28886 = CARTESIAN_POINT ( 'NONE',  ( 0.000000000000000000, -15.06282895647999887, 0.000000000000000000 ) ) ;
#28887 = CARTESIAN_POINT ( 'NONE',  ( 1.407449402687491524, -79.07027855378979098, -0.5447420947246425227 ) ) ;
#28888 = APPLICATION_CONTEXT ( 'automotive_design' ) ;
#28889 = CARTESIAN_POINT ( 'NONE',  ( 1.943390883608510533, -81.20520834021384360, 3.554109968293325483 ) ) ;
#28890 = EDGE_CURVE ( 'NONE', #36778, #800, #55985, .T. ) ;
#28891 = CARTESIAN_POINT ( 'NONE',  ( -7.685416442687999172, -76.55401027050999119, -9.616126112745998711 ) ) ;
#28892 = CARTESIAN_POINT ( 'NONE',  ( 2.813789756862274505, -77.64583333333332860, -10.47020627418438821 ) ) ;
#28893 = AXIS2_PLACEMENT_3D ( 'NONE', #7900, #29459, #30322 ) ;
#28894 = CARTESIAN_POINT ( 'NONE',  ( -5.684557159767995138, -77.92708333333334281, 7.396918292183145560 ) ) ;
#28895 = CARTESIAN_POINT ( 'NONE',  ( 9.641208724103000449, -61.23394297667999808, -7.943747389727000119 ) ) ;
#28896 = CARTESIAN_POINT ( 'NONE',  ( -1.307210027570999911, -79.09916823586999612, -12.19386267984000050 ) ) ;
#28897 = CARTESIAN_POINT ( 'NONE',  ( -0.6669403506045999963, -76.25457055981898691, -12.26286337364000012 ) ) ;
#28898 = CARTESIAN_POINT ( 'NONE',  ( -1.243547092045993674, -78.78541666666666288, 9.499999999999996447 ) ) ;
#28899 = AXIS2_PLACEMENT_3D ( 'NONE', #53965, #53663, #57502 ) ;
#28900 = DIRECTION ( 'NONE',  ( 0.000000000000000000, -1.000000000000000000, 0.000000000000000000 ) ) ;
#28901 = CARTESIAN_POINT ( 'NONE',  ( -3.099413287474135803, -78.15434610508248170, -11.66500092276903011 ) ) ;
#28902 = CARTESIAN_POINT ( 'NONE',  ( 5.694538069269999623E-14, -72.84999999994899156, 0.000000000000000000 ) ) ;
#28903 = EDGE_CURVE ( 'NONE', #56437, #12329, #37671, .T. ) ;
#28904 = ORIENTED_EDGE ( 'NONE', *, *, #40886, .F. ) ;
#28905 = CARTESIAN_POINT ( 'NONE',  ( -1.225487488653999923, -83.53778917074799892, -0.2866612609456000160 ) ) ;
#28906 = DIRECTION ( 'NONE',  ( 0.9859154929576978699, -0.1672442547472993701, 2.241733975738995337E-11 ) ) ;
#28907 = PLANE ( 'NONE',  #39844 ) ;
#28908 = VECTOR ( 'NONE', #54810, 1000.000000000000000 ) ;
#28909 = CARTESIAN_POINT ( 'NONE',  ( -0.7681833999686477066, -82.92708333333331439, 0.9995835529977223910 ) ) ;
#28910 = CARTESIAN_POINT ( 'NONE',  ( -1.791942608155000061, -1.881074315393999941, -3.430764814325999890 ) ) ;
#28911 = CARTESIAN_POINT ( 'NONE',  ( -3.566334030200000171, -77.40777409222799577, 11.50986677841000017 ) ) ;
#28912 = DIRECTION ( 'NONE',  ( 1.000000000000000000, 0.000000000000000000, 0.000000000000000000 ) ) ;
#28914 = CARTESIAN_POINT ( 'NONE',  ( 10.12290050253000118, -23.24999997822999731, -7.648026768374000639 ) ) ;
#28913 = CARTESIAN_POINT ( 'NONE',  ( -9.653806611548578331, -76.15120867658298209, 6.697802937877729512 ) ) ;
#28915 = CARTESIAN_POINT ( 'NONE',  ( 0.9322037676993999433, -79.15839416819699181, -10.87687281004000006 ) ) ;
#28916 = DIRECTION ( 'NONE',  ( 0.000000000000000000, -1.000000000000000000, 0.000000000000000000 ) ) ;
#28917 = VERTEX_POINT ( 'NONE', #21343 ) ;
#28918 = DIRECTION ( 'NONE',  ( 0.000000000000000000, 1.000000000000000000, 1.048986614577000002E-10 ) ) ;
#28919 = CARTESIAN_POINT ( 'NONE',  ( -9.250000000000000000, -78.09999999999999432, 0.000000000000000000 ) ) ;
#28920 = CARTESIAN_POINT ( 'NONE',  ( 0.000000000000000000, -75.67500000000001137, 0.000000000000000000 ) ) ;
#28921 = CARTESIAN_POINT ( 'NONE',  ( -9.479345976290870723, -76.20104166681831259, -5.464528704362162870 ) ) ;
#28922 = CARTESIAN_POINT ( 'NONE',  ( -0.5750802367077204602, -79.18702307077883518, -1.109883865317614848 ) ) ;
#28923 = DIRECTION ( 'NONE',  ( 0.000000000000000000, 1.000000000000000000, 0.000000000000000000 ) ) ;
#28924 = CARTESIAN_POINT ( 'NONE',  ( -6.708975540371000079, -79.20704916398798900, -6.964516712451000124 ) ) ;
#28925 = DIRECTION ( 'NONE',  ( 1.000000000000000000, 0.000000000000000000, 0.000000000000000000 ) ) ;
#28926 = CARTESIAN_POINT ( 'NONE',  ( 0.000000000000000000, -52.49705297114005020, -12.53545825868000207 ) ) ;
#28927 = EDGE_LOOP ( 'NONE', ( #48920, #44910, #44851 ) ) ;
#28928 = CARTESIAN_POINT ( 'NONE',  ( -11.10951737771999959, -79.28970297022300429, -1.847319190731999905 ) ) ;
#28929 = LINE ( 'NONE', #38082, #37093 ) ;
#28930 = CARTESIAN_POINT ( 'NONE',  ( 0.3533977571636973125, -79.17711132399134044, -11.83063463211526667 ) ) ;
#28931 = CARTESIAN_POINT ( 'NONE',  ( -2.038544192961597279, -78.70000000000000284, 3.380937561918479606 ) ) ;
#28932 = CARTESIAN_POINT ( 'NONE',  ( 2.320007599203503634, -77.81275085298281624, 11.90349632493328613 ) ) ;
#28934 = CARTESIAN_POINT ( 'NONE',  ( -0.0008345804459809217030, -81.47557856639851082, 1.249685689776924624 ) ) ;
#28933 = CARTESIAN_POINT ( 'NONE',  ( 0.9331017648476999105, -81.97053941010099720, 0.9326770562470999559 ) ) ;
#28935 = CARTESIAN_POINT ( 'NONE',  ( -0.3806779964142781858, -79.04933040305580505, 1.216001660871532275 ) ) ;
#28936 = CARTESIAN_POINT ( 'NONE',  ( -4.345263384820875707, -76.99999999999998579, -8.432632365033661870 ) ) ;
#28937 = CARTESIAN_POINT ( 'NONE',  ( -8.130811096542000627, -24.68523690389000080, -9.546858433121998999 ) ) ;
#28938 = EDGE_CURVE ( 'NONE', #308, #38673, #24229, .T. ) ;
#28939 = CARTESIAN_POINT ( 'NONE',  ( 0.000000000000000000, -2.949999999935999817, 0.000000000000000000 ) ) ;
#28940 = CARTESIAN_POINT ( 'NONE',  ( -12.49168433577000137, -55.50150862742999891, 1.667916687244999974 ) ) ;
#28941 = VECTOR ( 'NONE', #29413, 1000.000000000000227 ) ;
#28942 = CARTESIAN_POINT ( 'NONE',  ( 0.1291033597530705512, -79.32416573517009795, 10.97502397199794544 ) ) ;
#28943 = CARTESIAN_POINT ( 'NONE',  ( -3.140974612311405512, -77.19583333333332575, 11.68767212001977640 ) ) ;
#28944 = EDGE_LOOP ( 'NONE', ( #39239, #35026, #25476, #45209 ) ) ;
#28945 = CIRCLE ( 'NONE', #56316, 1.750000000000000000 ) ;
#28946 = ORIENTED_EDGE ( 'NONE', *, *, #19789, .F. ) ;
#28947 = CARTESIAN_POINT ( 'NONE',  ( 6.786979366286999493, -78.19513998579799363, 7.374582364394999701 ) ) ;
#28948 = CARTESIAN_POINT ( 'NONE',  ( 2.172204358709288297, -78.74132774247185296, -10.52819538874959981 ) ) ;
#28949 = AXIS2_PLACEMENT_3D ( 'NONE', #40186, #21883, #49056 ) ;
#28950 = ORIENTED_EDGE ( 'NONE', *, *, #28398, .F. ) ;
#28951 = CARTESIAN_POINT ( 'NONE',  ( 8.596775676242998543, -16.86467110163999905, 9.310147894694001280 ) ) ;
#28952 = CARTESIAN_POINT ( 'NONE',  ( -9.500094076791862463, -79.39994338716823563, -4.328536937075411965E-07 ) ) ;
#28953 = CARTESIAN_POINT ( 'NONE',  ( 10.85716400461000042, -78.54559109126999772, -5.254475923155999872 ) ) ;
#28954 = CARTESIAN_POINT ( 'NONE',  ( 14.00000000000000000, -32.88214388149999934, 0.000000000000000000 ) ) ;
#28955 = LINE ( 'NONE', #16262, #49437 ) ;
#28956 = CARTESIAN_POINT ( 'NONE',  ( 1.310679582531385279, -79.79166666666667140, 0.7554284705563519831 ) ) ;
#28957 = CARTESIAN_POINT ( 'NONE',  ( 8.822637088635000069, -80.20464915057038979, 6.926713255916000733 ) ) ;
#28958 = ORIENTED_EDGE ( 'NONE', *, *, #52626, .F. ) ;
#28959 = CARTESIAN_POINT ( 'NONE',  ( -10.69999999997999929, -81.80000000002199556, 2.760601855093000384E-10 ) ) ;
#28960 = VERTEX_POINT ( 'NONE', #57644 ) ;
#28961 = EDGE_CURVE ( 'NONE', #48419, #2165, #22208, .T. ) ;
#28962 = CARTESIAN_POINT ( 'NONE',  ( 8.506684281324854879, -77.38222109832315709, 3.641164479901510376 ) ) ;
#28963 = CARTESIAN_POINT ( 'NONE',  ( -1.500000000000000000, -83.34999999999999432, 0.000000000000000000 ) ) ;
#28964 = PLANE ( 'NONE',  #16822 ) ;
#28965 = UNCERTAINTY_MEASURE_WITH_UNIT (LENGTH_MEASURE( 1.000000000000000082E-05 ), #28722, 'distance_accuracy_value', 'NONE');
#28966 = DIRECTION ( 'NONE',  ( 0.7071067811864981678, 0.000000000000000000, 0.7071067811865970887 ) ) ;
#28967 = CARTESIAN_POINT ( 'NONE',  ( 7.374560639698994002, -77.57708333333330586, -9.596002108778151296 ) ) ;
#28968 = DIRECTION ( 'NONE',  ( 0.000000000000000000, 1.000000000000000000, 0.000000000000000000 ) ) ;
#28969 = CARTESIAN_POINT ( 'NONE',  ( -0.9156221410628999635, -78.31137460220000435, 1.345473579290000110 ) ) ;
#28970 = CARTESIAN_POINT ( 'NONE',  ( -9.569149049473001156, -79.45140313587198477, 5.523520626929999899 ) ) ;
#28971 = CARTESIAN_POINT ( 'NONE',  ( 1.500000000000000000, -80.75000000000000000, 0.000000000000000000 ) ) ;
#28972 = B_SPLINE_CURVE_WITH_KNOTS ( 'NONE', 3,
 ( #44167, #21717, #39722, #50355, #50649, #9902, #491, #41190, #1349, #6044, #24052, #50938, #27311, #36751, #18471, #19629, #36462, #32023, #31730, #28470, #32601, #54489, #54770, #9318, #42071, #27884, #1640, #41480, #4893, #779, #22890, #23759, #49774 ),
 .UNSPECIFIED., .F., .F.,
 ( 4, 2, 2, 1, 1, 1, 2, 2, 1, 1, 1, 2, 2, 1, 2, 2, 2, 2, 2, 4 ),
 ( 0.000000000000000000, 0.06250000000000030531, 0.1250000000000005829, 0.1875000000000008604, 0.2187500000000009992, 0.2343750000000010825, 0.2421875000000010825, 0.2500000000000010547, 0.3125000000000012212, 0.3437500000000012768, 0.3593750000000013323, 0.3671875000000013323, 0.3750000000000013878, 0.4375000000000009992, 0.4687500000000009437, 0.5000000000000008882, 0.6250000000000006661, 0.7500000000000004441, 0.8750000000000001110, 1.000000000000000000 ),
 .UNSPECIFIED. ) ;
#28973 = DIRECTION ( 'NONE',  ( 0.7071067811864976127, -0.7071067811865975328, -2.089956507868993372E-09 ) ) ;
#28974 = EDGE_CURVE ( 'NONE', #23500, #52926, #53510, .T. ) ;
#28975 = CARTESIAN_POINT ( 'NONE',  ( -2.856707873099999961, -84.79476111440199304, -2.098616509398999685 ) ) ;
#28976 = ORIENTED_EDGE ( 'NONE', *, *, #35611, .F. ) ;
#28977 = CARTESIAN_POINT ( 'NONE',  ( -10.16547580793340622, -77.20000000000000284, 4.069192989858231968 ) ) ;
#28978 = CARTESIAN_POINT ( 'NONE',  ( 1.676986109946000170, -79.59391447301999278, 0.2957349343760000138 ) ) ;
#28979 = CARTESIAN_POINT ( 'NONE',  ( 9.723174507645000020, -61.27697503925999456, 7.958760295356000825 ) ) ;
#28980 = EDGE_CURVE ( 'NONE', #23138, #42100, #45427, .T. ) ;
#28981 = CARTESIAN_POINT ( 'NONE',  ( 11.97742283006000186, -77.88548593716899404, 0.2395971301470999903 ) ) ;
#28982 = CARTESIAN_POINT ( 'NONE',  ( -8.950130560568000604, -16.79887407354000217, 8.958576480220999727 ) ) ;
#28983 = CIRCLE ( 'NONE', #6360, 2.600000000000000089 ) ;
#28984 = CARTESIAN_POINT ( 'NONE',  ( 10.74974228399219633, -78.85534952883524795, 0.7036061753646287720 ) ) ;
#28985 = CARTESIAN_POINT ( 'NONE',  ( -0.8622078521763266723, -3.355252669283040667, -3.415065585293687533 ) ) ;
#28986 = CARTESIAN_POINT ( 'NONE',  ( 10.38076106766223461, -80.87128293744233076, 2.794622580891152452 ) ) ;
#28987 = CARTESIAN_POINT ( 'NONE',  ( 1.442464609972999856, -77.21642875802798756, -9.302176701096998457 ) ) ;
#28988 = CARTESIAN_POINT ( 'NONE',  ( 1.798336774613000122, -55.60355501915000076, -12.61277771564000005 ) ) ;
#28989 = CARTESIAN_POINT ( 'NONE',  ( -8.584476293286000370, -76.90617272148499239, 6.698613553322000591 ) ) ;
#28990 = FACE_OUTER_BOUND ( 'NONE', #25929, .T. ) ;
#28991 = CARTESIAN_POINT ( 'NONE',  ( 3.140974612311377090, -78.44583333333332575, -11.68767212001978528 ) ) ;
#28992 = CARTESIAN_POINT ( 'NONE',  ( 0.2579617086353386823, -81.29143934431662899, -1.247668167079378110 ) ) ;
#28993 = ORIENTED_EDGE ( 'NONE', *, *, #2452, .F. ) ;
#28994 = CARTESIAN_POINT ( 'NONE',  ( 1.246077061130999919, -80.98666519049299950, -0.4752592857455000264 ) ) ;
#28995 = CARTESIAN_POINT ( 'NONE',  ( 0.8537148449456000154, -61.50498145875999256, -12.43377424877000159 ) ) ;
#28996 = CIRCLE ( 'NONE', #51650, 0.5000000000000004441 ) ;
#28997 = CARTESIAN_POINT ( 'NONE',  ( -7.710095619821999868, -21.75064714351000106, -10.18496935396999881 ) ) ;
#28998 = CARTESIAN_POINT ( 'NONE',  ( -9.457500717944000712, -78.37906892202299503, -6.031068363571000290 ) ) ;
#28999 = CARTESIAN_POINT ( 'NONE',  ( 6.718030245586000149, -78.98696307443100295, -8.679405866825000260 ) ) ;
#29000 = AXIS2_PLACEMENT_3D ( 'NONE', #48171, #51438, #34551 ) ;
#29001 = CYLINDRICAL_SURFACE ( 'NONE', #45095, 9.250000000000000000 ) ;
#29002 = CARTESIAN_POINT ( 'NONE',  ( 3.257100396869151204, -85.59895834756915178, 2.343891278707987968 ) ) ;
#29003 = CARTESIAN_POINT ( 'NONE',  ( -11.21087884115999955, -76.05337044997000362, 3.367372065805000148 ) ) ;
#29004 = CARTESIAN_POINT ( 'NONE',  ( 6.655614189731015706, -78.52578135515757651, 9.682981938576327607 ) ) ;
#29005 = DIRECTION ( 'NONE',  ( -0.7071067811865475727, 0.000000000000000000, -0.7071067811865475727 ) ) ;
#29006 = ORIENTED_EDGE ( 'NONE', *, *, #13370, .T. ) ;
#29007 = CARTESIAN_POINT ( 'NONE',  ( -0.1123201243897108126, -79.98247754429688428, 1.245149161110058689 ) ) ;
#29008 = EDGE_CURVE ( 'NONE', #57339, #26739, #17199, .T. ) ;
#29009 = AXIS2_PLACEMENT_3D ( 'NONE', #6679, #42699, #20264 ) ;
#29010 = CARTESIAN_POINT ( 'NONE',  ( -1.210822168571079605, -78.11458333333335702, -9.250000000000000000 ) ) ;
#29011 = CARTESIAN_POINT ( 'NONE',  ( 8.284626357322000700, -53.75139346809000074, -9.778502130833999217 ) ) ;
#29012 = CARTESIAN_POINT ( 'NONE',  ( 0.9331110433225999756, -78.54758795410299399, 11.22756599386000076 ) ) ;
#29013 = CYLINDRICAL_SURFACE ( 'NONE', #56630, 0.5000000000000004441 ) ;
#29014 = CARTESIAN_POINT ( 'NONE',  ( 11.68767212001977995, -77.57083333333333997, 3.140974612311385972 ) ) ;
#29015 = CARTESIAN_POINT ( 'NONE',  ( 0.9655056220227854480, -81.56980293136361126, 1.162965503173076121 ) ) ;
#29016 = CARTESIAN_POINT ( 'NONE',  ( -14.00000000000000000, -32.70420297070000260, 0.000000000000000000 ) ) ;
#29017 = CARTESIAN_POINT ( 'NONE',  ( 0.9433681713884025655, -79.79331829884100102, -0.8205418275783242787 ) ) ;
#29018 = EDGE_CURVE ( 'NONE', #22005, #6658, #31343, .T. ) ;
#29019 = CARTESIAN_POINT ( 'NONE',  ( 0.1963495408493637351, -78.03541666666667709, -1.499999999999999778 ) ) ;
#29020 = ORIENTED_EDGE ( 'NONE', *, *, #18338, .T. ) ;
#29021 = EDGE_CURVE ( 'NONE', #25888, #47851, #13723, .T. ) ;
#29022 = CARTESIAN_POINT ( 'NONE',  ( 0.0005350743312633779144, -81.72561961952891352, -1.249649688976135931 ) ) ;
#29023 = CARTESIAN_POINT ( 'NONE',  ( -8.833962032441000645, -79.90775739383900600, 6.607787011616999884 ) ) ;
#29024 = CARTESIAN_POINT ( 'NONE',  ( -1.072417187047447484, -81.45601597663524274, -0.9250971790290343222 ) ) ;
#29025 = VERTEX_POINT ( 'NONE', #25775 ) ;
#29026 = ORIENTED_EDGE ( 'NONE', *, *, #14268, .F. ) ;
#29027 = CARTESIAN_POINT ( 'NONE',  ( -1.275842582732999997, -80.62523951446499382, -0.3715998334726999808 ) ) ;
#29028 = ORIENTED_EDGE ( 'NONE', *, *, #30024, .F. ) ;
#29029 = ORIENTED_EDGE ( 'NONE', *, *, #43247, .T. ) ;
#29030 = CARTESIAN_POINT ( 'NONE',  ( -1.044910384896000188, -16.94473505805000002, 12.77260826199000121 ) ) ;
#29031 = CARTESIAN_POINT ( 'NONE',  ( -10.12290050255000118, -55.55000002206000431, -7.648026768392999664 ) ) ;
#29032 = CARTESIAN_POINT ( 'NONE',  ( 0.000000000000000000, 0.000000000000000000, 0.000000000000000000 ) ) ;
#29033 = CARTESIAN_POINT ( 'NONE',  ( -12.51072239526000196, -52.49705297114005020, 0.7871079366006996647 ) ) ;
#29034 = AXIS2_PLACEMENT_3D ( 'NONE', #53283, #31110, #57707 ) ;
#29035 = CARTESIAN_POINT ( 'NONE',  ( 8.472259919707001430, -79.11551001420200180, 5.354284829591000161 ) ) ;
#29036 = CARTESIAN_POINT ( 'NONE',  ( 3.540722753092142572, -78.25630082268401111, -8.545476915601279089 ) ) ;
#29037 = CARTESIAN_POINT ( 'NONE',  ( -6.206245474241999460, -79.61997468871599892, 9.343480492029000217 ) ) ;
#29038 = VERTEX_POINT ( 'NONE', #16925 ) ;
#29039 = ORIENTED_EDGE ( 'NONE', *, *, #46918, .T. ) ;
#29040 = CARTESIAN_POINT ( 'NONE',  ( -9.238076119067644143, -77.59563551126068148, 0.5262792932712636595 ) ) ;
#29041 = DIRECTION ( 'NONE',  ( 0.7071067811865474617, 0.7071067811865474617, 6.606111637375445165E-09 ) ) ;
#29042 = CARTESIAN_POINT ( 'NONE',  ( -12.68703394093999925, -60.55066116444000102, -1.889962945498999902 ) ) ;
#29043 = CARTESIAN_POINT ( 'NONE',  ( -7.203390125892000562, -78.82828236281598322, -6.502451851937000704 ) ) ;
#29044 = AXIS2_PLACEMENT_3D ( 'NONE', #55572, #10128, #28693 ) ;
#29045 = LINE ( 'NONE', #30188, #50202 ) ;
#29046 = CARTESIAN_POINT ( 'NONE',  ( 0.3271848554490964789, -79.85416666666667140, 1.217465845835395521 ) ) ;
#29047 = B_SPLINE_CURVE_WITH_KNOTS ( 'NONE', 3,
 ( #57458, #35002, #57166, #43602, #34715, #7581, #12583, #25580, #56599, #38870, #44179, #3727, #39735, #17301, #25006, #34428, #16159, #11447, #34136, #7292, #29426, #47478, #43027, #56890, #29996, #20586, #38583, #3163, #43312, #2869, #20867, #16446, #21153, #4906, #30864 ),
 .UNSPECIFIED., .F., .F.,
 ( 4, 1, 1, 1, 1, 1, 1, 1, 1, 1, 1, 1, 1, 1, 1, 1, 1, 1, 1, 1, 1, 1, 1, 1, 1, 1, 1, 1, 1, 1, 1, 1, 4 ),
 ( 0.000000000000000000, 0.01250080552085842261, 0.04500075182226595527, 0.07750069812385441959, 0.1100006444252618482, 0.1425005907268503125, 0.1750005370282577410, 0.2075004833298462192, 0.2400004296312538421, 0.2725003759328423203, 0.3050003222342497766, 0.3375002685358381993, 0.3700002148372456556, 0.4025001611388341338, 0.4350001074402415346, 0.4675000537418300128, 0.5000000000432374136, 0.5324999463446450365, 0.5649998926462335147, 0.5974998389476411376, 0.6299997852492296158, 0.6624997315506371276, 0.6949996778522256058, 0.7274996241536330066, 0.7599995704552214848, 0.7924995167566288856, 0.8249994630582173638, 0.8574994093596247646, 0.8899993556612132428, 0.9224993019626208657, 0.9549992482642093439, 0.9874991945656167447, 1.000000000000000000 ),
 .UNSPECIFIED. ) ;
#29048 = CARTESIAN_POINT ( 'NONE',  ( -0.9686576707075671422, -79.75000000000000000, -9.250000010076565360 ) ) ;
#29049 = CARTESIAN_POINT ( 'NONE',  ( 0.4542139134408000323, -80.35477686209999604, -1.519238769708999959 ) ) ;
#29050 = CARTESIAN_POINT ( 'NONE',  ( -3.808723190200999920, -78.60716621652929348, 1.220149157440000076 ) ) ;
#29051 = CARTESIAN_POINT ( 'NONE',  ( -1.238772947848447270, -79.79851084093215263, -0.8634107199282021750 ) ) ;
#29052 = CARTESIAN_POINT ( 'NONE',  ( 7.103190263045000563, -77.81460333806700191, 6.271635551916999951 ) ) ;
#29053 = CARTESIAN_POINT ( 'NONE',  ( -12.00000000000000888, -77.38958333333334849, 1.570796326794847264 ) ) ;
#29054 = LINE ( 'NONE', #47093, #32504 ) ;
#29056 = CARTESIAN_POINT ( 'NONE',  ( -0.9612450871864000046, -78.82660789559399461, -0.9244371432244999909 ) ) ;
#29055 = DIRECTION ( 'NONE',  ( 0.000000000000000000, 0.000000000000000000, -1.000000000000000000 ) ) ;
#29057 = CARTESIAN_POINT ( 'NONE',  ( -8.081851865186232331, -79.55868232694022879, 4.658047483831220248 ) ) ;
#29058 = CARTESIAN_POINT ( 'NONE',  ( 11.02435598615611489, -79.24999999999998579, 4.903336801626744901 ) ) ;
#29059 = DIRECTION ( 'NONE',  ( -1.000000000000000000, 0.000000000000000000, 0.000000000000000000 ) ) ;
#29060 = CARTESIAN_POINT ( 'NONE',  ( 1.500000000000000000, -78.14999999999999147, 0.000000000000000000 ) ) ;
#29061 = CARTESIAN_POINT ( 'NONE',  ( -2.033046685338129933, -1.172096679664639707, 2.984826379946394326 ) ) ;
#29062 = VERTEX_POINT ( 'NONE', #12484 ) ;
#29063 = CARTESIAN_POINT ( 'NONE',  ( 0.5584036861551523456, -3.500000000000000444, -3.445874424517756829 ) ) ;
#29064 = DIRECTION ( 'NONE',  ( -1.000000000000000000, 0.000000000000000000, -2.044813970925001362E-13 ) ) ;
#29065 = CARTESIAN_POINT ( 'NONE',  ( 0.2047640445682097077, -78.46198029154169262, 1.235340249920343858 ) ) ;
#29066 = CARTESIAN_POINT ( 'NONE',  ( -3.906545279024999928, -79.30125618921398711, 8.815735697348999977 ) ) ;
#29067 = CARTESIAN_POINT ( 'NONE',  ( -10.59876350475000173, -77.39874337786000069, 7.550195564144000393 ) ) ;
#29068 = CARTESIAN_POINT ( 'NONE',  ( 7.422208247548548243, -79.41434947898993357, 7.776989760925737905 ) ) ;
#29070 = ADVANCED_FACE ( 'NONE', ( #44658 ), #9264, .F. ) ;
#29069 = AXIS2_PLACEMENT_3D ( 'NONE', #21724, #3437, #48607 ) ;
#29071 = CARTESIAN_POINT ( 'NONE',  ( -8.817171295982999979, -79.40821332859900394, 4.135520484479999759 ) ) ;
#29072 = CARTESIAN_POINT ( 'NONE',  ( 10.07627163191000008, -23.24999999758999536, 7.601397897754999633 ) ) ;
#29073 = EDGE_CURVE ( 'NONE', #10595, #16041, #20485, .T. ) ;
#29074 = CARTESIAN_POINT ( 'NONE',  ( -11.04409640815999971, -77.31072091705098615, -0.5254229673086000529 ) ) ;
#29075 = CARTESIAN_POINT ( 'NONE',  ( 1.144839767925999841, -81.15898056936499927, 0.9788987191686998601 ) ) ;
#29076 = CARTESIAN_POINT ( 'NONE',  ( 3.441164836547143668, -77.99567685992036559, 8.842878308218095285 ) ) ;
#29077 = CARTESIAN_POINT ( 'NONE',  ( -7.608915353569000395, -77.97071810079599175, 5.542165790529000269 ) ) ;
#29079 = CARTESIAN_POINT ( 'NONE',  ( 7.634645345446648079, -55.32415927443057058, 10.10912681045544126 ) ) ;
#29078 = CARTESIAN_POINT ( 'NONE',  ( 2.877624606631000059, -83.46428928222098875, -2.724934237387000024 ) ) ;
#29080 = CARTESIAN_POINT ( 'NONE',  ( -6.090475762158000350, -79.56005194988499341, 7.362120511650999788 ) ) ;
#29081 = CARTESIAN_POINT ( 'NONE',  ( 5.173492352009886552, -77.16091037829299637, -10.64243289338730314 ) ) ;
#29082 = CARTESIAN_POINT ( 'NONE',  ( 4.328681851349221787, -80.25812132654044717, -9.840240413715774181 ) ) ;
#29083 = CARTESIAN_POINT ( 'NONE',  ( -6.194671355491903952, -77.17629026837472850, -8.785600045674199166 ) ) ;
#29084 = CARTESIAN_POINT ( 'NONE',  ( 7.483407197968000801, -79.75000000000000000, -5.437013583705000208 ) ) ;
#29085 = CIRCLE ( 'NONE', #10255, 1.499999999999999556 ) ;
#29086 = ORIENTED_EDGE ( 'NONE', *, *, #8716, .T. ) ;
#29087 = EDGE_CURVE ( 'NONE', #23838, #58165, #47847, .T. ) ;
#29088 = CARTESIAN_POINT ( 'NONE',  ( -5.246265831776000255, -79.65519386495199683, -10.82514862071000117 ) ) ;
#29089 = CARTESIAN_POINT ( 'NONE',  ( 0.5999999999999999778, -5.200000000000000178, 0.5999999999999999778 ) ) ;
#29090 = CARTESIAN_POINT ( 'NONE',  ( 4.000000000000000000, -5.000000000000000000, -0.5999999999999999778 ) ) ;
#29091 = EDGE_LOOP ( 'NONE', ( #41315, #3126, #18096, #48495, #10, #21409 ) ) ;
#29092 = CARTESIAN_POINT ( 'NONE',  ( -11.65000000000000036, -76.00000000000000000, 0.000000000000000000 ) ) ;
#29093 = ORIENTED_EDGE ( 'NONE', *, *, #48434, .T. ) ;
#29094 = EDGE_LOOP ( 'NONE', ( #50962, #52055 ) ) ;
#29095 = EDGE_LOOP ( 'NONE', ( #11976, #36210, #34890, #28266 ) ) ;
#29096 = CARTESIAN_POINT ( 'NONE',  ( 2.784687482942999726, -80.77167385719099002, -2.197743332419999973 ) ) ;
#29097 = CARTESIAN_POINT ( 'NONE',  ( 6.164680649823143455, -79.21867059585197524, 7.228082388273737280 ) ) ;
#29098 = EDGE_CURVE ( 'NONE', #50613, #38246, #17639, .T. ) ;
#29099 = EDGE_LOOP ( 'NONE', ( #57541, #3837 ) ) ;
#29100 = DIRECTION ( 'NONE',  ( 0.000000000000000000, 0.000000000000000000, -1.000000000000000000 ) ) ;
#29101 = ORIENTED_EDGE ( 'NONE', *, *, #22944, .T. ) ;
#29102 = CARTESIAN_POINT ( 'NONE',  ( -2.887306206174000245, -3.099943126209999900, -1.798010284767999956 ) ) ;
#29103 = ORIENTED_EDGE ( 'NONE', *, *, #45453, .F. ) ;
#29104 = DIRECTION ( 'NONE',  ( -6.735242868878000753E-11, -1.000000000000000000, 0.000000000000000000 ) ) ;
#29105 = CARTESIAN_POINT ( 'NONE',  ( -0.3822735262362919051, -79.14481419606127588, 1.483096551402029339 ) ) ;
#29106 = CARTESIAN_POINT ( 'NONE',  ( -4.907978555306589108, -79.79999999999999716, -10.78460461868905185 ) ) ;
#29107 = LINE ( 'NONE', #47152, #34039 ) ;
#29108 = AXIS2_PLACEMENT_3D ( 'NONE', #19839, #51437, #20135 ) ;
#29109 = CARTESIAN_POINT ( 'NONE',  ( -0.5548610165507998904, -77.87044793971165291, -9.688283574444998436 ) ) ;
#29110 = CARTESIAN_POINT ( 'NONE',  ( -10.07624512687999996, -76.43739497653800186, -4.852130239470000106 ) ) ;
#29111 = CARTESIAN_POINT ( 'NONE',  ( -7.781451050798130709, -79.90091309342098214, -5.818437412919247542 ) ) ;
#29112 = CARTESIAN_POINT ( 'NONE',  ( 0.01010140970966217668, -81.22383189636278189, 1.534624794271530313 ) ) ;
#29113 = CARTESIAN_POINT ( 'NONE',  ( -1.930828380988000248, -76.56982150479699101, -10.82837744324000084 ) ) ;
#29114 = CARTESIAN_POINT ( 'NONE',  ( -6.936452160827999869, -78.65757999610664797, -6.128159196645447615 ) ) ;
#29115 = CARTESIAN_POINT ( 'NONE',  ( -0.9565643533716999825, -80.11676424817299846, 0.9292797142584000580 ) ) ;
#29116 = CARTESIAN_POINT ( 'NONE',  ( 2.166634614239063377E-07, -77.01246206852036380, -9.437473063691797392 ) ) ;
#29117 = CARTESIAN_POINT ( 'NONE',  ( -3.003502455080446776, -3.070129738312371348, 1.239521229451738371 ) ) ;
#29118 = CARTESIAN_POINT ( 'NONE',  ( -3.368240389584999939, -80.00478455456800475, -1.663225410646000046 ) ) ;
#29119 = CARTESIAN_POINT ( 'NONE',  ( -3.735625875409999797, -79.47660106058199858, 11.49193229459999799 ) ) ;
#29120 = CARTESIAN_POINT ( 'NONE',  ( -8.973499209047250957, -78.05374552803205290, 5.919245077633647156 ) ) ;
#29121 = CIRCLE ( 'NONE', #38566, 12.50000000000000000 ) ;
#29122 = CARTESIAN_POINT ( 'NONE',  ( 0.3322227578772471435, -82.95365193092793277, 1.205740489271630356 ) ) ;
#29123 = PLANE ( 'NONE',  #45348 ) ;
#29124 = CARTESIAN_POINT ( 'NONE',  ( -0.9995835529977281642, -80.44791666666664298, 0.7681833999686391579 ) ) ;
#29125 = CARTESIAN_POINT ( 'NONE',  ( 10.35845608625999859, -18.70221245812999911, 7.627487525417000036 ) ) ;
#29126 = DIRECTION ( 'NONE',  ( -0.7071067811865470176, -0.7071067811865470176, -3.680441518142245308E-08 ) ) ;
#29127 = CARTESIAN_POINT ( 'NONE',  ( 0.7554284705563509839, -77.66666666666667140, -1.310679582531385945 ) ) ;
#29128 = CARTESIAN_POINT ( 'NONE',  ( 1.500000000000000000, -79.25000000000000000, 0.000000000000000000 ) ) ;
#29129 = CARTESIAN_POINT ( 'NONE',  ( 12.43359700617999941, -24.70705514168999883, 0.8500729763772000291 ) ) ;
#29130 = PRODUCT_DEFINITION_SHAPE ( 'NONE', 'NONE',  #58409 ) ;
#29131 = CARTESIAN_POINT ( 'NONE',  ( 7.744117733784010582, -77.63885439857841675, -7.580542634272604552 ) ) ;
#29132 = CARTESIAN_POINT ( 'NONE',  ( 1.535733471446528275, -78.33339274391919105, -11.74722481345108704 ) ) ;
#29133 = CARTESIAN_POINT ( 'NONE',  ( -9.813193589766999736, -78.88695524297345685, -4.915816122623000162 ) ) ;
#29134 = CARTESIAN_POINT ( 'NONE',  ( 11.31564005662000127, -75.97748313630999917, -4.176683572666000543 ) ) ;
#29135 = ORIENTED_EDGE ( 'NONE', *, *, #57426, .T. ) ;
#29136 = CARTESIAN_POINT ( 'NONE',  ( 2.168873741030000080, -82.99146544543100390, 3.316912045576999812 ) ) ;
#29137 = B_SPLINE_CURVE_WITH_KNOTS ( 'NONE', 3,
 ( #40786, #20322, #6740, #24751, #36644, #28873, #18360, #6157, #56338, #2326, #381, #2043, #55462, #49954, #33003, #29447, #24165, #672 ),
 .UNSPECIFIED., .F., .F.,
 ( 4, 2, 2, 2, 2, 2, 2, 2, 4 ),
 ( 0.000000000000000000, 0.1249999999999999722, 0.2499999999999999445, 0.3749999999999998890, 0.4999999999999998890, 0.6249999999999998890, 0.7499999999999997780, 0.8749999999999998890, 1.000000000000000000 ),
 .UNSPECIFIED. ) ;
#29138 = DIRECTION ( 'NONE',  ( -1.000000000000000000, 0.000000000000000000, 0.000000000000000000 ) ) ;
#29140 = CARTESIAN_POINT ( 'NONE',  ( -4.743262841170142963, -76.29154122859117138, -10.75029064995872652 ) ) ;
#29139 = CARTESIAN_POINT ( 'NONE',  ( -7.634645345497448332, -18.52415927528491579, -10.10912681051243567 ) ) ;
#29141 = CARTESIAN_POINT ( 'NONE',  ( -0.9218200799623716968, -81.57291666666667140, -1.199500263597270910 ) ) ;
#29142 = CARTESIAN_POINT ( 'NONE',  ( -0.9512330062464999791, -78.28343941728898869, 11.17646036812999988 ) ) ;
#29143 = CARTESIAN_POINT ( 'NONE',  ( 12.68702648024000190, -55.04922088160000015, -1.889939500033999797 ) ) ;
#29144 = CARTESIAN_POINT ( 'NONE',  ( -0.1544424224854999972, -78.20544831538099118, 9.738369639964998825 ) ) ;
#29145 = CARTESIAN_POINT ( 'NONE',  ( -0.6811744818814000624, -82.48030346844899441, -1.520282978132999840 ) ) ;
#29146 = CYLINDRICAL_SURFACE ( 'NONE', #9528, 0.5999999999999999778 ) ;
#29147 = CARTESIAN_POINT ( 'NONE',  ( 1.610212697858000030, -79.23601699803499798, -0.1201205297940999978 ) ) ;
#29148 = VERTEX_POINT ( 'NONE', #25697 ) ;
#29149 = DIRECTION ( 'NONE',  ( 0.000000000000000000, 0.000000000000000000, -1.000000000000000000 ) ) ;
#29150 = AXIS2_PLACEMENT_3D ( 'NONE', #58006, #21410, #48296 ) ;
#29151 = CARTESIAN_POINT ( 'NONE',  ( -2.960776533348827844, -78.76333549854666671, -1.715155014509248899 ) ) ;
#29152 = ORIENTED_EDGE ( 'NONE', *, *, #39362, .T. ) ;
#29153 = EDGE_CURVE ( 'NONE', #5025, #9279, #20843, .T. ) ;
#29154 = CARTESIAN_POINT ( 'NONE',  ( 1.302799686710000016, -77.94525788633960417, 0.2851120931344000020 ) ) ;
#29155 = CARTESIAN_POINT ( 'NONE',  ( -0.4458096168708076679, -80.69702831834133860, -1.185855554560490965 ) ) ;
#29156 = VERTEX_POINT ( 'NONE', #45404 ) ;
#29157 = CARTESIAN_POINT ( 'NONE',  ( 0.9776138843420000279, -78.39026560866999205, -12.12546088519999898 ) ) ;
#29158 = CARTESIAN_POINT ( 'NONE',  ( -4.551883652666999680, -77.52840078382998001, 10.48724849044000074 ) ) ;
#29159 = AXIS2_PLACEMENT_3D ( 'NONE', #38516, #25226, #25805 ) ;
#29160 = ORIENTED_EDGE ( 'NONE', *, *, #18038, .T. ) ;
#29161 = ORIENTED_EDGE ( 'NONE', *, *, #25046, .F. ) ;
#29162 = CIRCLE ( 'NONE', #36711, 9.750000000000000000 ) ;
#29163 = CARTESIAN_POINT ( 'NONE',  ( 0.1941027164032131103, -80.46307531212140418, 1.234895603396590991 ) ) ;
#29164 = CARTESIAN_POINT ( 'NONE',  ( 1.835192269501999984, -76.98893998579799813, 9.364437132986999757 ) ) ;
#29165 = CARTESIAN_POINT ( 'NONE',  ( 1.841371367509999857, -80.27025261668801193, -9.592189096167999196 ) ) ;
#29166 = EDGE_CURVE ( 'NONE', #31439, #32566, #55358, .T. ) ;
#29167 = ORIENTED_EDGE ( 'NONE', *, *, #15907, .T. ) ;
#29168 = CARTESIAN_POINT ( 'NONE',  ( -1.995546491236848352, -2.528183067936913275, 2.597540663301302732 ) ) ;
#29169 = CARTESIAN_POINT ( 'NONE',  ( -9.475123589965999571, -79.03204909097999575, 5.421936826000999687 ) ) ;
#29170 = ORIENTED_EDGE ( 'NONE', *, *, #48808, .T. ) ;
#29171 = CARTESIAN_POINT ( 'NONE',  ( -12.49997170191999984, -23.19201514549000009, -1.666513530428999967 ) ) ;
#29172 = CYLINDRICAL_SURFACE ( 'NONE', #10503, 9.500000000000000000 ) ;
#29173 = PLANE ( 'NONE',  #45156 ) ;
#29174 = LINE ( 'NONE', #34172, #27975 ) ;
#29175 = DIRECTION ( 'NONE',  ( 1.000000000000000000, 0.000000000000000000, 0.000000000000000000 ) ) ;
#29176 = LINE ( 'NONE', #42776, #37239 ) ;
#29177 = CARTESIAN_POINT ( 'NONE',  ( 7.033509982383000292, -77.03085009973318620, 6.880083864244000758 ) ) ;
#29178 = CARTESIAN_POINT ( 'NONE',  ( 1.467401882609930430, -78.62410577527140276, 0.4599864963736973733 ) ) ;
#29179 = CARTESIAN_POINT ( 'NONE',  ( -1.439896632895311335, -79.71458333333333712, -11.00000000000000178 ) ) ;
#29180 = CARTESIAN_POINT ( 'NONE',  ( -7.636246406686000299, -23.76323123101999713, 10.30460653225000023 ) ) ;
#29181 = CARTESIAN_POINT ( 'NONE',  ( 8.596418555780450887, -77.69791666666668561, -6.606377239730321982 ) ) ;
#29182 = EDGE_CURVE ( 'NONE', #52771, #1911, #39314, .T. ) ;
#29183 = CARTESIAN_POINT ( 'NONE',  ( 4.888750975951074551, -77.12187499993380868, -7.978256397349015927 ) ) ;
#29184 = CARTESIAN_POINT ( 'NONE',  ( 7.601397897754999633, -18.75000000240999753, 10.07627163191000008 ) ) ;
#29185 = CARTESIAN_POINT ( 'NONE',  ( 12.21456857099000004, -78.69087223421999511, -1.096995930408000142 ) ) ;
#29186 = CARTESIAN_POINT ( 'NONE',  ( -9.801255020792000394, -76.58243246625799827, 7.399866681860999940 ) ) ;
#29187 = DIRECTION ( 'NONE',  ( 0.000000000000000000, 1.000000000000000000, 0.000000000000000000 ) ) ;
#29188 = CARTESIAN_POINT ( 'NONE',  ( 0.2837406302606167996, -77.92307676773893377, 12.06313962186550270 ) ) ;
#29189 = CARTESIAN_POINT ( 'NONE',  ( -10.75729140709000120, -78.77285858373909377, -3.177859684494000359 ) ) ;
#29190 = ORIENTED_EDGE ( 'NONE', *, *, #37559, .T. ) ;
#29191 = CARTESIAN_POINT ( 'NONE',  ( -1.545693644023152125, -80.25398594989877665, -0.08651074858955706826 ) ) ;
#29192 = CARTESIAN_POINT ( 'NONE',  ( -17.50000000000000000, -51.86282895648000135, -3.979077900507000222E-10 ) ) ;
#29193 = CARTESIAN_POINT ( 'NONE',  ( 1.929975092517999924, -23.20107256264000029, 12.72537404210999945 ) ) ;
#29194 = AXIS2_PLACEMENT_3D ( 'NONE', #1365, #5481, #56252 ) ;
#29195 = CARTESIAN_POINT ( 'NONE',  ( 0.000000000000000000, -77.50000000000000000, 0.000000000000000000 ) ) ;
#29196 = CARTESIAN_POINT ( 'NONE',  ( -3.597461531748000318, -3.264312248862000221, 1.427805196757999884 ) ) ;
#29197 = AXIS2_PLACEMENT_3D ( 'NONE', #53401, #58129, #48699 ) ;
#29198 = CARTESIAN_POINT ( 'NONE',  ( -10.93129665128000028, -77.54342066934700028, -5.069765792968000007 ) ) ;
#29199 = CARTESIAN_POINT ( 'NONE',  ( 9.725848778082999857, -78.51658531640698868, -0.5172632330995999839 ) ) ;
#29201 = CARTESIAN_POINT ( 'NONE',  ( -0.1577822530794797395, -77.82391181108907574, -11.07750337872512780 ) ) ;
#29200 = CARTESIAN_POINT ( 'NONE',  ( -11.41855217635170838, -76.18078835300777030, 2.773217851598793526 ) ) ;
#29202 = CARTESIAN_POINT ( 'NONE',  ( 0.4274279416557000277, -82.92941453081499503, 1.281884980902999960 ) ) ;
#29203 = DIRECTION ( 'NONE',  ( -1.000000000000000000, 0.000000000000000000, 0.000000000000000000 ) ) ;
#29204 = ORIENTED_EDGE ( 'NONE', *, *, #49913, .F. ) ;
#29205 = CARTESIAN_POINT ( 'NONE',  ( 12.72966770606015530, -23.76881200365913571, 1.931346186345839211 ) ) ;
#29206 = CARTESIAN_POINT ( 'NONE',  ( 2.421389049398865900, -77.95433015483983752, 9.009788787264410459 ) ) ;
#29207 = CARTESIAN_POINT ( 'NONE',  ( -1.636761686205434607, -2.416666666666666963, 2.839805762151332402 ) ) ;
#29208 = CARTESIAN_POINT ( 'NONE',  ( -8.292771711479000274, -61.85529938492000213, 9.770424367394999976 ) ) ;
#29209 = CARTESIAN_POINT ( 'NONE',  ( -9.672666136464620479, -80.06087742290506526, 5.252905469540832151 ) ) ;
#29210 = CARTESIAN_POINT ( 'NONE',  ( 9.385821630279000516, -78.84439215714098736, 1.815438171114999832 ) ) ;
#29211 = CARTESIAN_POINT ( 'NONE',  ( 0.000000000000000000, -80.49999999999998579, 0.000000000000000000 ) ) ;
#29212 = LINE ( 'NONE', #48120, #12311 ) ;
#29213 = VERTEX_POINT ( 'NONE', #18530 ) ;
#29214 = CARTESIAN_POINT ( 'NONE',  ( 10.02591968313939752, -76.63641906179947227, 4.955712094219922648 ) ) ;
#29215 = DIRECTION ( 'NONE',  ( 1.000000000000000000, 0.000000000000000000, 0.000000000000000000 ) ) ;
#29216 = CARTESIAN_POINT ( 'NONE',  ( -8.130811096204000776, -61.48523690322999613, -9.546858433459998849 ) ) ;
#29217 = EDGE_CURVE ( 'NONE', #25686, #233, #54254, .T. ) ;
#29218 = CARTESIAN_POINT ( 'NONE',  ( 0.1243710621956479329, -81.46772713155802137, 1.245975140190170194 ) ) ;
#29219 = AXIS2_PLACEMENT_3D ( 'NONE', #41545, #22955, #19115 ) ;
#29220 = EDGE_CURVE ( 'NONE', #5962, #52316, #37453, .T. ) ;
#29221 = CARTESIAN_POINT ( 'NONE',  ( 0.000000000000000000, -77.49999999999998579, 0.000000000000000000 ) ) ;
#29222 = CARTESIAN_POINT ( 'NONE',  ( -0.8338927956455162160, -53.99946422210319952, -12.50366901599826797 ) ) ;
#29223 = CARTESIAN_POINT ( 'NONE',  ( 1.931087888049999979, -55.48415522678000400, -12.71658889739000031 ) ) ;
#29224 = CARTESIAN_POINT ( 'NONE',  ( -0.9051267565814000715, -79.01584333927000614, 0.9442094098902999999 ) ) ;
#29225 = CARTESIAN_POINT ( 'NONE',  ( 10.85425666711977755, -76.19571949791584586, 1.138855506895539493 ) ) ;
#29226 = DIRECTION ( 'NONE',  ( 0.000000000000000000, -1.000000000000000000, 0.000000000000000000 ) ) ;
#29227 = CARTESIAN_POINT ( 'NONE',  ( 12.71758670595498053, -54.73493368741875997, -1.809547514116605971 ) ) ;
#29228 = ORIENTED_EDGE ( 'NONE', *, *, #12558, .F. ) ;
#29229 = EDGE_CURVE ( 'NONE', #52985, #49658, #33655, .T. ) ;
#29230 = VERTEX_POINT ( 'NONE', #20986 ) ;
#29231 = CARTESIAN_POINT ( 'NONE',  ( -5.007587013623000516, -76.73414604793399008, 11.54976330113999872 ) ) ;
#29232 = CARTESIAN_POINT ( 'NONE',  ( 2.099707639723427555, -78.74077357293465695, -10.54285705307466969 ) ) ;
#29233 = ORIENTED_EDGE ( 'NONE', *, *, #34661, .F. ) ;
#29234 = CARTESIAN_POINT ( 'NONE',  ( 10.47840693002000023, -18.21310507181999938, 7.622759963130000038 ) ) ;
#29235 = AXIS2_PLACEMENT_3D ( 'NONE', #32193, #50235, #5064 ) ;
#29236 = AXIS2_PLACEMENT_3D ( 'NONE', #9580, #5149, #26979 ) ;
#29237 = AXIS2_PLACEMENT_3D ( 'NONE', #41438, #157, #54444 ) ;
#29238 = CARTESIAN_POINT ( 'NONE',  ( -1.575772165460815666, -54.33845457181071481, 12.70597445614748544 ) ) ;
#29239 = CARTESIAN_POINT ( 'NONE',  ( 8.299965097802999736, -78.51685037320000049, -8.752034438815000428 ) ) ;
#29240 = FACE_OUTER_BOUND ( 'NONE', #6007, .T. ) ;
#29241 = CYLINDRICAL_SURFACE ( 'NONE', #6992, 0.5000000000000006661 ) ;
#29242 = CARTESIAN_POINT ( 'NONE',  ( -1.500000000000000888, -79.98958333333334281, 0.1963495408493559080 ) ) ;
#29243 = CARTESIAN_POINT ( 'NONE',  ( -0.4146318973825999787, -79.45595202224899367, -11.20920117498000046 ) ) ;
#29244 = ORIENTED_EDGE ( 'NONE', *, *, #47114, .T. ) ;
#29245 = DIRECTION ( 'NONE',  ( 0.000000000000000000, -1.000000000000000000, 0.000000000000000000 ) ) ;
#29246 = EDGE_LOOP ( 'NONE', ( #30888, #3604, #49458 ) ) ;
#29247 = CARTESIAN_POINT ( 'NONE',  ( 4.200728562467627825, -77.26253573339837999, -8.241112584695276411 ) ) ;
#29248 = CARTESIAN_POINT ( 'NONE',  ( 10.74764839381999870, -78.23878986046499051, -0.2248421733643000131 ) ) ;
#29249 = DIRECTION ( 'NONE',  ( 0.000000000000000000, 1.000000000000000000, 0.000000000000000000 ) ) ;
#29250 = CARTESIAN_POINT ( 'NONE',  ( 8.061017305527000687, -59.94999999967000548, -8.909545442949999838 ) ) ;
#29251 = CARTESIAN_POINT ( 'NONE',  ( 0.6064284284549000814, -78.76285795985199911, -1.281524057860000010 ) ) ;
#29252 = DIRECTION ( 'NONE',  ( -1.000000000000000000, 0.000000000000000000, 0.000000000000000000 ) ) ;
#29253 = FACE_OUTER_BOUND ( 'NONE', #40801, .T. ) ;
#29254 = CARTESIAN_POINT ( 'NONE',  ( 0.3877229342594999961, -78.03296675330000198, -1.580612325761999948 ) ) ;
#29255 = CARTESIAN_POINT ( 'NONE',  ( -7.678667886068000215, -20.24263462181000151, 10.59548767699999949 ) ) ;
#29256 = CARTESIAN_POINT ( 'NONE',  ( -3.571993175857000491, -79.59186490753599230, -10.45556112308999985 ) ) ;
#29257 = CARTESIAN_POINT ( 'NONE',  ( -2.112861425255000203, -79.26094992126056127, -11.84242215301999934 ) ) ;
#29258 = DIRECTION ( 'NONE',  ( 0.000000000000000000, -1.000000000000000000, 0.000000000000000000 ) ) ;
#29259 = CARTESIAN_POINT ( 'NONE',  ( -2.858594134272999909, -84.86381343186599224, -2.100002208958999805 ) ) ;
#29260 = ORIENTED_EDGE ( 'NONE', *, *, #8219, .T. ) ;
#29261 = CARTESIAN_POINT ( 'NONE',  ( -0.4591954515747000420, -81.72675258327998904, 1.639803156192000122 ) ) ;
#29262 = CARTESIAN_POINT ( 'NONE',  ( -1.666294527194000175, -79.84655133345999900, -0.3511123450079000063 ) ) ;
#29263 = CARTESIAN_POINT ( 'NONE',  ( 0.000000000000000000, -75.15999999999999659, 0.000000000000000000 ) ) ;
#29264 = CARTESIAN_POINT ( 'NONE',  ( -7.167604382869000368, -77.55993415208399711, 9.599037027053000770 ) ) ;
#29265 = CARTESIAN_POINT ( 'NONE',  ( -10.07615509326000058, -17.27367739700000016, 7.986954869189998973 ) ) ;
#29266 = EDGE_CURVE ( 'NONE', #22214, #55898, #38990, .T. ) ;
#29267 = CARTESIAN_POINT ( 'NONE',  ( -1.160984792064531756, -78.78379718552881172, -0.5251923553234724151 ) ) ;
#29268 = CARTESIAN_POINT ( 'NONE',  ( -0.3956897636865157608, -2.133947066360573519, 3.499075337960325882 ) ) ;
#29269 = CARTESIAN_POINT ( 'NONE',  ( 9.779639049769572878, -80.88431169961586420, 4.483730783971120459 ) ) ;
#29270 = CARTESIAN_POINT ( 'NONE',  ( -2.523869816676000077, -78.24671468919598283, -9.181528052588999955 ) ) ;
#29271 = CARTESIAN_POINT ( 'NONE',  ( 1.669849926076999891, -55.42771399551000400, -12.48404299551000030 ) ) ;
#29272 = CARTESIAN_POINT ( 'NONE',  ( -2.149738495732000043, -78.06825668956298614, -10.82036777477999934 ) ) ;
#29273 = CARTESIAN_POINT ( 'NONE',  ( -7.674614791514000167, -19.24899163938999891, 10.14948852566999804 ) ) ;
#29274 = CARTESIAN_POINT ( 'NONE',  ( -5.230597743581999914, -80.44137704144308998, 9.575199762653999969 ) ) ;
#29275 = CARTESIAN_POINT ( 'NONE',  ( -0.2413114649954342938, -81.25963638061078598, -1.251987394859889413 ) ) ;
#29276 = ORIENTED_EDGE ( 'NONE', *, *, #38157, .F. ) ;
#29277 = CARTESIAN_POINT ( 'NONE',  ( -11.75000000000000000, -78.70000000000000284, -1.701764645356999850E-14 ) ) ;
#29278 = CARTESIAN_POINT ( 'NONE',  ( -0.9113424693929998988, -61.62535793526999583, -12.54674099561999867 ) ) ;
#29279 = DIRECTION ( 'NONE',  ( 0.000000000000000000, 1.000000000000000000, 0.000000000000000000 ) ) ;
#29280 = CIRCLE ( 'NONE', #1169, 11.00000000000000000 ) ;
#29281 = CARTESIAN_POINT ( 'NONE',  ( 1.508420534579999917, -77.63037179370199681, 11.11497989572000122 ) ) ;
#29282 = CARTESIAN_POINT ( 'NONE',  ( -8.058638732054999920, -78.42923420478300045, -7.451332657186999775 ) ) ;
#29283 = CARTESIAN_POINT ( 'NONE',  ( 6.586108526242999694, -80.07391735373440156, 8.810401493720998900 ) ) ;
#29284 = CARTESIAN_POINT ( 'NONE',  ( -2.947487654899788367, -84.51979166928597920, 2.780664221283836390 ) ) ;
#29285 = CARTESIAN_POINT ( 'NONE',  ( 5.913823124159999445, -76.24203414149499736, -10.61660120017000075 ) ) ;
#29286 = CARTESIAN_POINT ( 'NONE',  ( 9.965884746006045347, -78.49300387697907411, 6.229937699784958482 ) ) ;
#29287 = CARTESIAN_POINT ( 'NONE',  ( -7.861032689964853049, -61.26660299196984738, 10.10708926016829778 ) ) ;
#29288 = ORIENTED_EDGE ( 'NONE', *, *, #23290, .F. ) ;
#29289 = AXIS2_PLACEMENT_3D ( 'NONE', #17427, #25990, #12988 ) ;
#29290 = CARTESIAN_POINT ( 'NONE',  ( -0.9022118396650773420, -80.03964887368034908, 0.8648181855745056268 ) ) ;
#29291 = LINE ( 'NONE', #57041, #20745 ) ;
#29292 = CARTESIAN_POINT ( 'NONE',  ( -7.103610810849999346, -79.24989681241999051, -8.744578195291998313 ) ) ;
#29293 = EDGE_CURVE ( 'NONE', #46323, #51903, #45954, .T. ) ;
#29294 = CARTESIAN_POINT ( 'NONE',  ( 10.48543666025110710, -77.00833333333332575, -6.043427764450776785 ) ) ;
#29295 = CARTESIAN_POINT ( 'NONE',  ( 12.00000000000000000, -79.54999999999999716, 0.000000000000000000 ) ) ;
#29296 = CARTESIAN_POINT ( 'NONE',  ( 8.838834764832000701, -55.54999999966999980, 8.838834764832000701 ) ) ;
#29297 = CARTESIAN_POINT ( 'NONE',  ( -0.7635483339353790200, -81.93231960672001435, -1.306464905284852263 ) ) ;
#29298 = CARTESIAN_POINT ( 'NONE',  ( 0.7731065358596024284, -79.77859623460356886, -0.9850382754349712444 ) ) ;
#29299 = CARTESIAN_POINT ( 'NONE',  ( -8.610991514451539430, -53.62512235746365263, 9.355860133842407222 ) ) ;
#29300 = ORIENTED_EDGE ( 'NONE', *, *, #27695, .T. ) ;
#29301 = CARTESIAN_POINT ( 'NONE',  ( 1.931086388455000025, -23.29778595484999926, 12.71798280855999863 ) ) ;
#29302 = CARTESIAN_POINT ( 'NONE',  ( -12.82202361517000000, -23.42627773034000427, 2.066043355638000012 ) ) ;
#29303 = ORIENTED_EDGE ( 'NONE', *, *, #12027, .T. ) ;
#29304 = ADVANCED_FACE ( 'NONE', ( #5518 ), #5809, .F. ) ;
#29305 = ORIENTED_EDGE ( 'NONE', *, *, #31790, .F. ) ;
#29306 = TOROIDAL_SURFACE ( 'NONE', #44392, 1.250000000000000000, 0.5000000000000000000 ) ;
#29307 = CARTESIAN_POINT ( 'NONE',  ( -12.61112375829999976, -55.58433928934000079, -1.798929377343999825 ) ) ;
#29308 = ORIENTED_EDGE ( 'NONE', *, *, #14549, .T. ) ;
#29309 = ORIENTED_EDGE ( 'NONE', *, *, #45850, .T. ) ;
#29310 = CARTESIAN_POINT ( 'NONE',  ( 8.485281374238999419, -18.75000000000000000, -8.485281374238999419 ) ) ;
#29311 = CARTESIAN_POINT ( 'NONE',  ( -10.84231296956000001, -78.06411136276199159, 1.272641041331999956 ) ) ;
#29312 = DIRECTION ( 'NONE',  ( 1.000000000000000000, 0.000000000000000000, 0.000000000000000000 ) ) ;
#29313 = CARTESIAN_POINT ( 'NONE',  ( 7.601397897754999633, -23.25000000000000000, 9.369164850722000892 ) ) ;
#29314 = CARTESIAN_POINT ( 'NONE',  ( 4.399173910654000430, -79.09528667140098435, 8.880751478442000746 ) ) ;
#29315 = CARTESIAN_POINT ( 'NONE',  ( -1.803312564769471660, -78.20945996376244125, -9.072471366556113637 ) ) ;
#29316 = CARTESIAN_POINT ( 'NONE',  ( -8.090227444665263334, -79.45847354739515822, 4.644024077103019899 ) ) ;
#29317 = ORIENTED_EDGE ( 'NONE', *, *, #28605, .F. ) ;
#29318 = VERTEX_POINT ( 'NONE', #19400 ) ;
#29319 = CYLINDRICAL_SURFACE ( 'NONE', #32944, 11.70000000000000107 ) ;
#29320 = CIRCLE ( 'NONE', #36865, 11.59999999999999964 ) ;
#29321 = CARTESIAN_POINT ( 'NONE',  ( -1.392423410630999929E-14, -75.80000000000001137, 0.000000000000000000 ) ) ;
#29322 = B_SPLINE_CURVE_WITH_KNOTS ( 'NONE', 3,
 ( #13208, #3494, #8209, #39503, #12639, #40077 ),
 .UNSPECIFIED., .F., .F.,
 ( 4, 1, 1, 4 ),
 ( 0.000000000000000000, 0.3333333333333000081, 0.6666666666667000474, 1.000000000000000000 ),
 .UNSPECIFIED. ) ;
#29323 = CARTESIAN_POINT ( 'NONE',  ( -12.43652404748999984, -61.72065244505999715, -0.1284256373645000227 ) ) ;
#29324 = CIRCLE ( 'NONE', #50126, 5.500000000000000000 ) ;
#29325 = CARTESIAN_POINT ( 'NONE',  ( 2.260091721765999928, -78.97385677587398334, -9.437303113984999214 ) ) ;
#29326 = CARTESIAN_POINT ( 'NONE',  ( 7.668949790020999302, -19.22870851082999977, 10.21381326473999884 ) ) ;
#29327 = CARTESIAN_POINT ( 'NONE',  ( 0.000000000000000000, -32.70420297070000260, 0.000000000000000000 ) ) ;
#29328 = CARTESIAN_POINT ( 'NONE',  ( 6.606377239730347739, -76.67708333333331439, -8.596418555780422466 ) ) ;
#29329 = CARTESIAN_POINT ( 'NONE',  ( -7.374560639699019760, -76.82708333333329165, 9.596002108778129980 ) ) ;
#29330 = CARTESIAN_POINT ( 'NONE',  ( -0.6472661464068000248, -81.17600413218998767, 1.575051776950999960 ) ) ;
#29331 = DIRECTION ( 'NONE',  ( 0.000000000000000000, 0.000000000000000000, 1.000000000000000000 ) ) ;
#29332 = CARTESIAN_POINT ( 'NONE',  ( 0.000000000000000000, -75.67500000000001137, 0.000000000000000000 ) ) ;
#29333 = CARTESIAN_POINT ( 'NONE',  ( 1.362698812343641652, -79.46449576102331491, -0.6541207564315330014 ) ) ;
#29334 = CARTESIAN_POINT ( 'NONE',  ( -9.832476300866000329, -78.43311332859899210, 1.242130619674999936 ) ) ;
#29335 = CARTESIAN_POINT ( 'NONE',  ( -1.750000000000000000, -21.74977139337000054, -12.65375411739000100 ) ) ;
#29336 = CARTESIAN_POINT ( 'NONE',  ( 2.062673488738000049, -23.32452529362999982, -12.82904091339000097 ) ) ;
#29337 = EDGE_CURVE ( 'NONE', #40915, #56632, #1618, .T. ) ;
#29339 = CARTESIAN_POINT ( 'NONE',  ( 13.86363636363000218, -32.36102867817999851, 1.277888278705000044E-05 ) ) ;
#29338 = DIRECTION ( 'NONE',  ( 0.000000000000000000, 0.7071067811866525998, -0.7071067811864425456 ) ) ;
#29340 = CARTESIAN_POINT ( 'NONE',  ( -2.486604901413152824, -78.90416666666666856, -9.252740428349003565 ) ) ;
#29341 = CARTESIAN_POINT ( 'NONE',  ( -10.65969359034999897, -80.46865055360498786, 3.376454609634999660 ) ) ;
#29342 = CARTESIAN_POINT ( 'NONE',  ( 12.50000000000000000, -18.75000000000000000, -1.250000000000000000 ) ) ;
#29343 = CARTESIAN_POINT ( 'NONE',  ( 0.000000000000000000, -74.70999999999999375, 0.000000000000000000 ) ) ;
#29344 = DIRECTION ( 'NONE',  ( 1.000000000000000000, 0.000000000000000000, 0.000000000000000000 ) ) ;
#29345 = EDGE_CURVE ( 'NONE', #10810, #47434, #35445, .T. ) ;
#29346 = EDGE_LOOP ( 'NONE', ( #14700, #8925, #2083, #4996 ) ) ;
#29347 = CARTESIAN_POINT ( 'NONE',  ( 12.50240681834000078, -24.68234730741999883, -1.005418943851999813 ) ) ;
#29348 = CARTESIAN_POINT ( 'NONE',  ( -1.930628539546999978, -55.57875555881000196, 12.72375828102000028 ) ) ;
#29349 = CARTESIAN_POINT ( 'NONE',  ( 1.017054994240753851, -78.39947633289455098, 0.7277666091791081815 ) ) ;
#29350 = VECTOR ( 'NONE', #34950, 1000.000000000000000 ) ;
#29351 = CARTESIAN_POINT ( 'NONE',  ( -9.175873485632997983, -79.97880775341398873, -2.587226946429999952 ) ) ;
#29352 = CARTESIAN_POINT ( 'NONE',  ( -12.54673671095000209, -53.97796527404000244, 0.9173654211234000266 ) ) ;
#29353 = CARTESIAN_POINT ( 'NONE',  ( -0.4846980698234193974, -79.22879212854250852, 9.704134706623241513 ) ) ;
#29354 = CARTESIAN_POINT ( 'NONE',  ( 1.667260628937999867, -60.00942012442000362, 12.49858003896999925 ) ) ;
#29355 = CARTESIAN_POINT ( 'NONE',  ( 1.500000000000000000, -78.75000000000000000, 0.000000000000000000 ) ) ;
#29356 = CARTESIAN_POINT ( 'NONE',  ( 11.00000000000000000, -77.44999999999998863, 0.000000000000000000 ) ) ;
#29357 = CARTESIAN_POINT ( 'NONE',  ( -1.250000000000000000, -79.59999999999999432, 0.000000000000000000 ) ) ;
#29358 = CARTESIAN_POINT ( 'NONE',  ( -7.206703837310000083, -77.80299228781500176, 8.241246436175000412 ) ) ;
#29359 = CARTESIAN_POINT ( 'NONE',  ( 9.766266492730634852, -76.40258437943595027, -6.532607198706168461 ) ) ;
#29360 = CARTESIAN_POINT ( 'NONE',  ( -10.94146508061000134, -77.15133007910999652, -1.409282183016999923 ) ) ;
#29361 = CARTESIAN_POINT ( 'NONE',  ( -1.017084552132891728, -82.05124430433711780, 0.7286258421704788768 ) ) ;
#29362 = VECTOR ( 'NONE', #40366, 1000.000000000000000 ) ;
#29363 = CARTESIAN_POINT ( 'NONE',  ( 1.750000000000000000, -57.05022860762000647, -12.65375411742999923 ) ) ;
#29364 = CARTESIAN_POINT ( 'NONE',  ( 7.559982449049000408, -76.96625235366248319, -6.032732969207000195 ) ) ;
#29365 = CARTESIAN_POINT ( 'NONE',  ( 6.479078291783999966, -79.19414415034599131, -7.022474634662000170 ) ) ;
#29366 = CARTESIAN_POINT ( 'NONE',  ( 11.00000000000000000, -77.34999999999999432, 0.000000000000000000 ) ) ;
#29367 = CARTESIAN_POINT ( 'NONE',  ( 0.9218200799623694763, -81.32291666666668561, 1.199500263597272465 ) ) ;
#29368 = CARTESIAN_POINT ( 'NONE',  ( -1.250000000000000000, -76.75499999999999545, 0.000000000000000000 ) ) ;
#29369 = DIRECTION ( 'NONE',  ( -4.277603912091000087E-12, 1.000000000000000000, 1.682670357362999898E-10 ) ) ;
#29370 = CIRCLE ( 'NONE', #14321, 1.750000000000001332 ) ;
#29371 = CARTESIAN_POINT ( 'NONE',  ( -8.734850699938000673, -79.50577571071400484, 8.271005326623001253 ) ) ;
#29372 = CARTESIAN_POINT ( 'NONE',  ( 12.00000000000000000, -18.84999999999999787, 0.5999999999999999778 ) ) ;
#29373 = CARTESIAN_POINT ( 'NONE',  ( 0.000000000000000000, -23.15000000000000213, -12.00000000000000000 ) ) ;
#29374 = VERTEX_POINT ( 'NONE', #2280 ) ;
#29375 = EDGE_CURVE ( 'NONE', #8523, #32213, #20276, .T. ) ;
#29376 = CARTESIAN_POINT ( 'NONE',  ( 1.718598679964348896, -24.24962933043864766, 12.71111582768155124 ) ) ;
#29377 = EDGE_CURVE ( 'NONE', #18726, #49572, #34982, .T. ) ;
#29378 = VERTEX_POINT ( 'NONE', #11998 ) ;
#29379 = VERTEX_POINT ( 'NONE', #42714 ) ;
#29380 = CARTESIAN_POINT ( 'NONE',  ( 8.107762507645077221, -60.31691643837567796, 7.434020715871779039 ) ) ;
#29381 = CARTESIAN_POINT ( 'NONE',  ( 1.538071403320016461, -77.43541666666664014, -11.74999999999999822 ) ) ;
#29382 = CARTESIAN_POINT ( 'NONE',  ( -3.585749735645000325, -80.37756669824999278, 0.1616911715135000149 ) ) ;
#29383 = CARTESIAN_POINT ( 'NONE',  ( 6.261610633530541037, -79.21755913019184447, 7.144501166461902919 ) ) ;
#29384 = VERTEX_POINT ( 'NONE', #57150 ) ;
#29385 = CARTESIAN_POINT ( 'NONE',  ( 0.07626174556372275481, -82.73051772784693014, -1.247420650239736251 ) ) ;
#29386 = ORIENTED_EDGE ( 'NONE', *, *, #39474, .T. ) ;
#29387 = CARTESIAN_POINT ( 'NONE',  ( -10.75000000000000355, -76.99058402040098770, 1.271990410372850544 ) ) ;
#29388 = B_SPLINE_CURVE_WITH_KNOTS ( 'NONE', 3,
 ( #28914, #24496, #38355, #33632, #51954, #55799 ),
 .UNSPECIFIED., .F., .F.,
 ( 4, 1, 1, 4 ),
 ( 0.000000000000000000, 0.3333333333333000081, 0.6666666666667000474, 1.000000000000000000 ),
 .UNSPECIFIED. ) ;
#29389 = ORIENTED_EDGE ( 'NONE', *, *, #17914, .F. ) ;
#29390 = CARTESIAN_POINT ( 'NONE',  ( 7.483407197968000801, -79.75000000000000000, -5.437013583705000208 ) ) ;
#29391 = CARTESIAN_POINT ( 'NONE',  ( 1.341660107401375646, -78.53983454477609882, 0.7399033773893253230 ) ) ;
#29392 = CARTESIAN_POINT ( 'NONE',  ( -5.019662172184764515, -79.80000000000001137, -10.73459069481442185 ) ) ;
#29393 = CARTESIAN_POINT ( 'NONE',  ( -6.472707105664965432, -80.02684928995590496, 8.585610045933069756 ) ) ;
#29394 = ADVANCED_FACE ( 'NONE', ( #3143 ), #57441, .T. ) ;
#29395 = CARTESIAN_POINT ( 'NONE',  ( 2.347484846439459094, -86.31452042059399332, -3.296887854808300045 ) ) ;
#29396 = CARTESIAN_POINT ( 'NONE',  ( 9.886069181790999139, -76.54518001718498965, -5.228720670581999741 ) ) ;
#29397 = CARTESIAN_POINT ( 'NONE',  ( -11.75000000000000000, -77.29999999999999716, 0.000000000000000000 ) ) ;
#29398 = CARTESIAN_POINT ( 'NONE',  ( 2.309309650359952393, -76.99409235924242978, -9.392413018435071592 ) ) ;
#29399 = CARTESIAN_POINT ( 'NONE',  ( 8.104133543071000645, -76.20111113651499579, 7.605434776855999779 ) ) ;
#29400 = CARTESIAN_POINT ( 'NONE',  ( -4.876868007374968172, -78.68090168310180843, -7.860757581031139196 ) ) ;
#29401 = CARTESIAN_POINT ( 'NONE',  ( -0.6056189234361001317, -80.26560211831599645, -1.188192690176999911 ) ) ;
#29402 = CONICAL_SURFACE ( 'NONE', #36949, 10.93038838648999977, 1.373400766944759877 ) ;
#29403 = CARTESIAN_POINT ( 'NONE',  ( 12.00000000000000000, -23.15000000002000036, 0.7999999999999001243 ) ) ;
#29404 = CARTESIAN_POINT ( 'NONE',  ( -1.247385803317999864, -61.27722255996999934, -12.50301438880000049 ) ) ;
#29405 = CARTESIAN_POINT ( 'NONE',  ( -2.751252219471000071, -78.67817549782625974, -2.305321983890999959 ) ) ;
#29406 = CARTESIAN_POINT ( 'NONE',  ( -8.325889437744001143, -79.44363262701600092, 8.917886277098999059 ) ) ;
#29407 = VECTOR ( 'NONE', #8757, 1000.000000000000000 ) ;
#29408 = CARTESIAN_POINT ( 'NONE',  ( -8.943304019696144636, -78.05334570480560785, 5.964714355002641355 ) ) ;
#29409 = CARTESIAN_POINT ( 'NONE',  ( -0.01036771288394258174, -82.97628653625926631, 1.249625640293676732 ) ) ;
#29410 = CARTESIAN_POINT ( 'NONE',  ( -3.321932689530000093, -81.00000000000000000, 10.22385755016999909 ) ) ;
#29411 = CARTESIAN_POINT ( 'NONE',  ( 1.095375403649999857, -84.30649735065199479, 3.371218846835000171 ) ) ;
#29412 = CARTESIAN_POINT ( 'NONE',  ( -0.3271848554491046945, -80.39583333333331439, 1.217465845835393301 ) ) ;
#29413 = DIRECTION ( 'NONE',  ( -0.7071067811705339379, 1.925103501360094241E-07, -0.7071067812025347843 ) ) ;
#29414 = ADVANCED_FACE ( 'NONE', ( #6981 ), #22356, .T. ) ;
#29415 = CARTESIAN_POINT ( 'NONE',  ( -7.645391636782999711, -60.01530450324999322, -10.18949673577000148 ) ) ;
#29416 = DIRECTION ( 'NONE',  ( 0.000000000000000000, -1.000000000000000000, 0.000000000000000000 ) ) ;
#29417 = CARTESIAN_POINT ( 'NONE',  ( -1.310679582531386611, -77.54166666666667140, -0.7554284705563495406 ) ) ;
#29418 = CARTESIAN_POINT ( 'NONE',  ( -12.72394144137000005, -18.77839271500000251, -1.930881231431999856 ) ) ;
#29419 = CARTESIAN_POINT ( 'NONE',  ( -9.339950055924999717, -78.11329442843999971, -9.061158367717998985 ) ) ;
#29420 = CARTESIAN_POINT ( 'NONE',  ( -3.788397905917849862, -77.54708607277024157, -10.15569713685381537 ) ) ;
#29422 = CARTESIAN_POINT ( 'NONE',  ( 7.169497772410326597, -78.37458968298378181, -9.346273223251115425 ) ) ;
#29421 = CIRCLE ( 'NONE', #21090, 10.50000000000000000 ) ;
#29423 = CARTESIAN_POINT ( 'NONE',  ( 1.618935784642556275, -23.92751168673077800, -12.52134385800271410 ) ) ;
#29424 = CARTESIAN_POINT ( 'NONE',  ( -6.371817981013998988, -76.16336784646999547, -10.59357524699000130 ) ) ;
#29425 = ORIENTED_EDGE ( 'NONE', *, *, #42508, .F. ) ;
#29426 = CARTESIAN_POINT ( 'NONE',  ( 8.828526701892000617, -80.44666485374948195, -6.997593314318000246 ) ) ;
#29427 = CYLINDRICAL_SURFACE ( 'NONE', #9754, 11.75000000000000000 ) ;
#29428 = CARTESIAN_POINT ( 'NONE',  ( 1.165893053700000070, -80.95418768743299154, -0.5987630157190000357 ) ) ;
#29429 = CARTESIAN_POINT ( 'NONE',  ( -3.689662007795999621, -78.48144319244001110, 11.36357164112000007 ) ) ;
#29430 = CARTESIAN_POINT ( 'NONE',  ( 12.66008925480999814, -54.17289997881999852, -1.387046028394999908 ) ) ;
#29431 = CARTESIAN_POINT ( 'NONE',  ( -9.596198845516999754, -77.89981427748799092, -0.8161970854479000392 ) ) ;
#29432 = CARTESIAN_POINT ( 'NONE',  ( 1.531359430757999851, -82.60662189866998517, -0.6558942768039000004 ) ) ;
#29433 = FACE_OUTER_BOUND ( 'NONE', #34569, .T. ) ;
#29434 = CARTESIAN_POINT ( 'NONE',  ( -12.50000000000000000, -63.73717104351998586, -1.871520963622999753E-13 ) ) ;
#29435 = ORIENTED_EDGE ( 'NONE', *, *, #31389, .F. ) ;
#29436 = CARTESIAN_POINT ( 'NONE',  ( 0.7347525963730557885, -78.91284375429691522, -3.410767982593458925 ) ) ;
#29437 = ORIENTED_EDGE ( 'NONE', *, *, #31744, .T. ) ;
#29438 = CARTESIAN_POINT ( 'NONE',  ( -7.998217534801063344, -77.54306880728415763, -4.799733181834938023 ) ) ;
#29439 = CARTESIAN_POINT ( 'NONE',  ( -1.250000000000000000, -76.29999999999999716, -0.6999999999999999556 ) ) ;
#29440 = VERTEX_POINT ( 'NONE', #34409 ) ;
#29441 = CARTESIAN_POINT ( 'NONE',  ( 3.299676814977999584, -78.90572260172200458, -11.70874303878999889 ) ) ;
#29442 = CARTESIAN_POINT ( 'NONE',  ( -7.443442755000000410, -78.12484979902399118, -8.531552098207999535 ) ) ;
#29443 = ORIENTED_EDGE ( 'NONE', *, *, #51767, .T. ) ;
#29444 = VERTEX_POINT ( 'NONE', #29116 ) ;
#29445 = CARTESIAN_POINT ( 'NONE',  ( -0.4867589087424958327, -80.50691733354545931, 1.151273400566878324 ) ) ;
#29446 = AXIS2_PLACEMENT_3D ( 'NONE', #33684, #42853, #29252 ) ;
#29447 = CARTESIAN_POINT ( 'NONE',  ( -11.68767212001979594, -79.77916666666664014, 3.140974612311315806 ) ) ;
#29448 = CARTESIAN_POINT ( 'NONE',  ( 1.739862777674999972, -79.37105597504650234, 9.611119481339999382 ) ) ;
#29449 = VERTEX_POINT ( 'NONE', #34112 ) ;
#29450 = CARTESIAN_POINT ( 'NONE',  ( 12.54983130235000033, -53.74901607425999828, 0.1356732392833999989 ) ) ;
#29451 = CARTESIAN_POINT ( 'NONE',  ( 2.368087569675000115, -79.99857547445330397, 10.55620284977000090 ) ) ;
#29452 = ORIENTED_EDGE ( 'NONE', *, *, #26831, .F. ) ;
#29453 = CARTESIAN_POINT ( 'NONE',  ( 7.919595949288999570, -59.94999999446000771, -8.768124086549999419 ) ) ;
#29454 = CARTESIAN_POINT ( 'NONE',  ( 2.459440699436000077, -77.15569415034599388, -9.171074077620000153 ) ) ;
#29455 = AXIS2_PLACEMENT_3D ( 'NONE', #8238, #35372, #35975 ) ;
#29456 = CARTESIAN_POINT ( 'NONE',  ( 9.108265402946999600, -53.92189187171000242, 8.478706101031999509 ) ) ;
#29457 = ADVANCED_FACE ( 'NONE', ( #6694 ), #15843, .T. ) ;
#29458 = CARTESIAN_POINT ( 'NONE',  ( 7.635226873550689852, -18.23391307131834438, -10.36745167322480121 ) ) ;
#29459 = DIRECTION ( 'NONE',  ( 0.000000000000000000, -1.000000000000000000, 0.000000000000000000 ) ) ;
#29460 = CARTESIAN_POINT ( 'NONE',  ( -10.26032959198470884, -77.24059631258572267, -5.914278839158486178 ) ) ;
#29461 = AXIS2_PLACEMENT_3D ( 'NONE', #53842, #5126, #27536 ) ;
#29462 = CARTESIAN_POINT ( 'NONE',  ( 9.620021812515000548, -76.95241263186049707, -2.063756841170000023 ) ) ;
#29463 = CARTESIAN_POINT ( 'NONE',  ( 7.103405556168159940, -78.97354755707108609, 9.415197073630089619 ) ) ;
#29464 = CARTESIAN_POINT ( 'NONE',  ( -2.698602497352579732, -81.89895834794788243, -2.969860844161505753 ) ) ;
#29465 = CARTESIAN_POINT ( 'NONE',  ( -8.652376385601000308, -25.26264602966000083, 9.414489258817999584 ) ) ;
#29466 = CARTESIAN_POINT ( 'NONE',  ( -2.384669060246999983, -80.44857046129098421, -3.423433742407000047 ) ) ;
#29467 = FACE_OUTER_BOUND ( 'NONE', #41807, .T. ) ;
#29468 = LINE ( 'NONE', #24185, #15343 ) ;
#29469 = CARTESIAN_POINT ( 'NONE',  ( -5.950798862880000151, -78.89798320933999776, 10.72320280238000123 ) ) ;
#29470 = CARTESIAN_POINT ( 'NONE',  ( -10.51110168222999874, -76.02285105332299509, 6.351495789100000344 ) ) ;
#29471 = FACE_OUTER_BOUND ( 'NONE', #38504, .T. ) ;
#29472 = EDGE_CURVE ( 'NONE', #35168, #7317, #11060, .T. ) ;
#29473 = CARTESIAN_POINT ( 'NONE',  ( 3.945923481703957680, -77.70070240490868230, -11.63927170873302863 ) ) ;
#29474 = CARTESIAN_POINT ( 'NONE',  ( -0.7681833999686432657, -78.57291666666668561, -0.9995835529977258327 ) ) ;
#29475 = VERTEX_POINT ( 'NONE', #20563 ) ;
#29476 = CARTESIAN_POINT ( 'NONE',  ( -1.319810957934479445, -80.70946105886535804, 0.7378495871194835631 ) ) ;
#29477 = CARTESIAN_POINT ( 'NONE',  ( 12.72554383682000001, -60.00159311597000311, -1.930239506950999884 ) ) ;
#29478 = CARTESIAN_POINT ( 'NONE',  ( 0.000000000000000000, -81.90000000002299885, 0.000000000000000000 ) ) ;
#29479 = VECTOR ( 'NONE', #7709, 1000.000000000000000 ) ;
#29480 = CARTESIAN_POINT ( 'NONE',  ( 1.750000000001000089, -23.25000000990999993, 12.56594317857000043 ) ) ;
#29481 = CARTESIAN_POINT ( 'NONE',  ( 0.6912376084024000056, -2.021356624101999788, -3.649169745438999968 ) ) ;
#29482 = CARTESIAN_POINT ( 'NONE',  ( 5.622631719431000263, -78.77790074527499087, 10.78740717875000144 ) ) ;
#29483 = CARTESIAN_POINT ( 'NONE',  ( -4.832441116568999995, -78.68712829118099705, 8.456193503077001239 ) ) ;
#29484 = B_SPLINE_CURVE_WITH_KNOTS ( 'NONE', 3,
 ( #23061, #18062, #49947, #54076, #14776, #4482 ),
 .UNSPECIFIED., .F., .F.,
 ( 4, 2, 4 ),
 ( 0.000000000000000000, 0.5000000000000000000, 1.000000000000000000 ),
 .UNSPECIFIED. ) ;
#29485 = EDGE_CURVE ( 'NONE', #3332, #16171, #46885, .T. ) ;
#29487 = DIRECTION ( 'NONE',  ( 0.000000000000000000, 0.000000000000000000, -1.000000000000000000 ) ) ;
#29486 = CARTESIAN_POINT ( 'NONE',  ( -0.3046678973520325906, -76.07670231100695446, 11.75299617503634764 ) ) ;
#29488 = CARTESIAN_POINT ( 'NONE',  ( 10.07627163191000008, -23.24999999758999536, 7.601397897754999633 ) ) ;
#29489 = FACE_OUTER_BOUND ( 'NONE', #34212, .T. ) ;
#29490 = ORIENTED_EDGE ( 'NONE', *, *, #18460, .F. ) ;
#29491 = LINE ( 'NONE', #38649, #40807 ) ;
#29492 = AXIS2_PLACEMENT_3D ( 'NONE', #52288, #11847, #30690 ) ;
#29493 = ADVANCED_FACE ( 'NONE', ( #12278 ), #38561, .F. ) ;
#29494 = CARTESIAN_POINT ( 'NONE',  ( 2.853743189566999534E-14, -82.05000000008600125, -10.29999999990999981 ) ) ;
#29495 = CARTESIAN_POINT ( 'NONE',  ( 3.250000000000000000, -2.250000000000000000, 0.000000000000000000 ) ) ;
#29496 = CARTESIAN_POINT ( 'NONE',  ( -7.758897894450000443, -61.10081253415999925, 10.31443085085999911 ) ) ;
#29497 = CARTESIAN_POINT ( 'NONE',  ( -11.00000000000000000, -77.69999999999998863, 0.000000000000000000 ) ) ;
#29498 = CARTESIAN_POINT ( 'NONE',  ( -1.288745046912000092, -80.02869764566298727, 9.583962847433999954 ) ) ;
#29499 = CARTESIAN_POINT ( 'NONE',  ( 7.633478597825000378, -18.79901960220000134, -10.36292351978000070 ) ) ;
#29500 = CARTESIAN_POINT ( 'NONE',  ( 1.439896632895333539, -78.73541666666665151, -10.99999999999999822 ) ) ;
#29501 = EDGE_LOOP ( 'NONE', ( #53487, #32197, #44723 ) ) ;
#29503 = AXIS2_PLACEMENT_3D ( 'NONE', #52603, #3014, #8585 ) ;
#29502 = CARTESIAN_POINT ( 'NONE',  ( 5.888733633253000477, -78.44537633716700498, -9.599841314972998418 ) ) ;
#29504 = CARTESIAN_POINT ( 'NONE',  ( 1.849768683728251428, -76.71166488776647441, 11.02980055127182624 ) ) ;
#29505 = CARTESIAN_POINT ( 'NONE',  ( -11.79296105283189533, -79.04295787391396289, 0.9841517631264623533 ) ) ;
#29506 = DIRECTION ( 'NONE',  ( 1.000000000000000000, 0.000000000000000000, 0.000000000000000000 ) ) ;
#29507 = AXIS2_PLACEMENT_3D ( 'NONE', #11800, #2660, #20654 ) ;
#29508 = CARTESIAN_POINT ( 'NONE',  ( 0.2887706833722973876, -81.45697567580890563, 1.216636297542402767 ) ) ;
#29509 = DIRECTION ( 'NONE',  ( 0.000000000000000000, -1.000000000000000000, 0.000000000000000000 ) ) ;
#29510 = CARTESIAN_POINT ( 'NONE',  ( 1.103931346181417528, -54.17916251664232163, -12.50298439256130578 ) ) ;
#29511 = CARTESIAN_POINT ( 'NONE',  ( 1.667936688463999895, -59.56486430393999854, -12.53239398061000109 ) ) ;
#29512 = ADVANCED_FACE ( 'NONE', ( #30268 ), #22592, .F. ) ;
#29513 = DIRECTION ( 'NONE',  ( 0.000000000000000000, -1.000000000000000000, 0.000000000000000000 ) ) ;
#29514 = CARTESIAN_POINT ( 'NONE',  ( -10.75000000000000000, -78.60000000000000853, 0.000000000000000000 ) ) ;
#29515 = FACE_OUTER_BOUND ( 'NONE', #31912, .T. ) ;
#29516 = ORIENTED_EDGE ( 'NONE', *, *, #37483, .F. ) ;
#29517 = ORIENTED_EDGE ( 'NONE', *, *, #53542, .F. ) ;
#29518 = CARTESIAN_POINT ( 'NONE',  ( -6.786191657256999576, -76.40628414149500713, -10.60285507971000030 ) ) ;
#29519 = CARTESIAN_POINT ( 'NONE',  ( 4.486458642797829910, -78.75926223335113718, -9.769447897824372617 ) ) ;
#29520 = CONICAL_SURFACE ( 'NONE', #4065, 12.84999999995999964, 0.7853981633972997312 ) ;
#29521 = EDGE_LOOP ( 'NONE', ( #26545, #5069, #54000, #16400, #26695, #47945, #27803, #9611, #1977, #22973, #13415, #39268, #7168 ) ) ;
#29522 = CARTESIAN_POINT ( 'NONE',  ( 8.485548443539000729, -17.11931586736000455, 9.101490738460999097 ) ) ;
#29523 = CARTESIAN_POINT ( 'NONE',  ( -4.814939325413682525, -78.76622030423393994, 8.425567463547647407 ) ) ;
#29524 = CARTESIAN_POINT ( 'NONE',  ( 8.768124086549999419, -59.94999999446000771, 7.919595949288999570 ) ) ;
#29525 = CARTESIAN_POINT ( 'NONE',  ( 5.554616340558999887, -78.00781628945000534, 11.53062854294000061 ) ) ;
#29526 = FACE_OUTER_BOUND ( 'NONE', #41620, .T. ) ;
#29527 = CARTESIAN_POINT ( 'NONE',  ( 4.100000000000000533, -75.19999999999998863, 0.000000000000000000 ) ) ;
#29528 = CARTESIAN_POINT ( 'NONE',  ( 0.000000000000000000, -79.50000000000000000, 0.000000000000000000 ) ) ;
#29529 = CONICAL_SURFACE ( 'NONE', #15390, 13.94999999937999924, 0.7853981633972997312 ) ;
#29530 = CARTESIAN_POINT ( 'NONE',  ( 5.745747329289000227, -78.66609807519598974, 9.633509135241000720 ) ) ;
#29531 = ORIENTED_EDGE ( 'NONE', *, *, #49961, .F. ) ;
#29532 = CARTESIAN_POINT ( 'NONE',  ( 11.61663471297537242, -78.06380585108666992, 2.038423278490623325 ) ) ;
#29533 = ORIENTED_EDGE ( 'NONE', *, *, #23115, .F. ) ;
#29534 = CARTESIAN_POINT ( 'NONE',  ( 5.439234600025764088, -77.27515920132572091, -7.481681149270881903 ) ) ;
#29535 = FACE_OUTER_BOUND ( 'NONE', #50961, .T. ) ;
#29536 = CARTESIAN_POINT ( 'NONE',  ( -0.2201363562291999698, -79.46327907014000402, -1.483758735329000045 ) ) ;
#29537 = CARTESIAN_POINT ( 'NONE',  ( -10.54506146704257752, -77.87759237249433397, -3.824040745093859162 ) ) ;
#29538 = CARTESIAN_POINT ( 'NONE',  ( 0.7786926255480000059, -77.71523380450280172, -1.300993539011999989 ) ) ;
#29539 = AXIS2_PLACEMENT_3D ( 'NONE', #33711, #29279, #51167 ) ;
#29540 = DIRECTION ( 'NONE',  ( 0.000000000000000000, -1.000000000000000000, 0.000000000000000000 ) ) ;
#29541 = CYLINDRICAL_SURFACE ( 'NONE', #13429, 1.750000000000001332 ) ;
#29542 = CARTESIAN_POINT ( 'NONE',  ( -1.481905647302000029, -78.42273774175998824, -0.6727694308694001091 ) ) ;
#29543 = CARTESIAN_POINT ( 'NONE',  ( -7.668936932643000581, -19.22847221992000044, 10.21380041495000057 ) ) ;
#29544 = CARTESIAN_POINT ( 'NONE',  ( -8.689005542484000699, -78.44007837989597931, 6.824886543446999632 ) ) ;
#29545 = EDGE_CURVE ( 'NONE', #41153, #19814, #201, .T. ) ;
#29546 = CARTESIAN_POINT ( 'NONE',  ( -11.22206352832999876, -79.67932075312558027, -4.332716936452000844 ) ) ;
#29547 = FILL_AREA_STYLE_COLOUR ( '', #46097 ) ;
#29548 = CARTESIAN_POINT ( 'NONE',  ( 1.924478147487999946, -85.15551236020199610, -2.976802803591999780 ) ) ;
#29549 = ORIENTED_EDGE ( 'NONE', *, *, #26512, .T. ) ;
#29550 = ADVANCED_FACE ( 'NONE', ( #4885 ), #55005, .F. ) ;
#29551 = CARTESIAN_POINT ( 'NONE',  ( 2.457916154627046712, -77.19999999999998863, 10.51642625215182036 ) ) ;
#29552 = CARTESIAN_POINT ( 'NONE',  ( 1.447659443890000119, -81.10989310931999796, -0.6470525719642999940 ) ) ;
#29553 = CARTESIAN_POINT ( 'NONE',  ( 10.06692847421147086, -60.50343452142983125, 7.655995225842833207 ) ) ;
#29554 = CARTESIAN_POINT ( 'NONE',  ( 2.697636866285999968, -77.70918012219799209, -11.67213861177999945 ) ) ;
#29555 = CARTESIAN_POINT ( 'NONE',  ( -9.101506735347999921, -17.11932813898000205, 8.485532457246998561 ) ) ;
#29556 = CARTESIAN_POINT ( 'NONE',  ( 0.5253929667144483506, -77.90920784449171776, -1.161211157036742048 ) ) ;
#29557 = CARTESIAN_POINT ( 'NONE',  ( -2.870721577664869351, -1.799218864078162117, -2.038938680912825596 ) ) ;
#29558 = CARTESIAN_POINT ( 'NONE',  ( 7.920136950582000068, -77.98335584965398937, 4.778486233528999705 ) ) ;
#29559 = CARTESIAN_POINT ( 'NONE',  ( 6.123453098898000491, -77.96247639790598782, 7.292029784470999587 ) ) ;
#29560 = CARTESIAN_POINT ( 'NONE',  ( -10.47083672843175783, -76.58144398812963516, 2.512152686489665054 ) ) ;
#29561 = CARTESIAN_POINT ( 'NONE',  ( -9.367668485852000515, -77.41458445751899831, 5.826535979523000286 ) ) ;
#29562 = CARTESIAN_POINT ( 'NONE',  ( 9.393203674808285442, -79.20833333333332860, -5.413904038987152667 ) ) ;
#29563 = CARTESIAN_POINT ( 'NONE',  ( 1.233875498716631158, -81.87979417287398576, -0.3168210084591759346 ) ) ;
#29564 = ORIENTED_EDGE ( 'NONE', *, *, #24164, .T. ) ;
#29565 = CYLINDRICAL_SURFACE ( 'NONE', #25537, 1.250000000000000000 ) ;
#29566 = CARTESIAN_POINT ( 'NONE',  ( -0.9816856958575284064, -80.76975118242557983, -0.7730884388065356605 ) ) ;
#29567 = CARTESIAN_POINT ( 'NONE',  ( -1.194090705995999979, -61.24031658870000427, -12.43436538493000043 ) ) ;
#29568 = EDGE_CURVE ( 'NONE', #52988, #36311, #11540, .T. ) ;
#29569 = CARTESIAN_POINT ( 'NONE',  ( -9.998780405325002008, -77.30353567768000289, -5.083552005986999411 ) ) ;
#29570 = CARTESIAN_POINT ( 'NONE',  ( -6.920341278396000106, -79.44055896075899170, -8.518972542050999408 ) ) ;
#29571 = CARTESIAN_POINT ( 'NONE',  ( 10.31986335554000078, -24.28918510737999981, -7.753844818030001029 ) ) ;
#29572 = CARTESIAN_POINT ( 'NONE',  ( -3.361724651403247499, -84.55833333636749671, 2.260551657038760709 ) ) ;
#29573 = CARTESIAN_POINT ( 'NONE',  ( -11.10423584941000108, -77.10988712250798471, -4.937773032316999711 ) ) ;
#29574 = CARTESIAN_POINT ( 'NONE',  ( -1.250000000000000000, -55.54999999966999980, -12.50000000000000000 ) ) ;
#29575 = DIRECTION ( 'NONE',  ( -0.7071067811865475727, 0.000000000000000000, 0.7071067811865475727 ) ) ;
#29576 = ORIENTED_EDGE ( 'NONE', *, *, #15348, .T. ) ;
#29577 = CARTESIAN_POINT ( 'NONE',  ( -0.05067031697304230642, -79.97863705871390039, 1.248890127844249243 ) ) ;
#29578 = CARTESIAN_POINT ( 'NONE',  ( 10.71369944335147117, -77.97083333333331723, 2.879226727952105769 ) ) ;
#29579 = CARTESIAN_POINT ( 'NONE',  ( 7.511900341590999730, -79.36226622975098621, -8.396444939682998765 ) ) ;
#29580 = CARTESIAN_POINT ( 'NONE',  ( 1.568318300085000120E-14, -0.05000000003700048185, 0.000000000000000000 ) ) ;
#29581 = CARTESIAN_POINT ( 'NONE',  ( 1.538071403319964281, -77.66458333333333997, 11.75000000000000711 ) ) ;
#29582 = CARTESIAN_POINT ( 'NONE',  ( -12.76303204298000082, -60.06485150663000638, 1.980584515756000030 ) ) ;
#29583 = CARTESIAN_POINT ( 'NONE',  ( -1.431540077043731873, -82.82304749526281284, 0.4904972203789410012 ) ) ;
#29584 = ADVANCED_FACE ( 'NONE', ( #18464 ), #31128, .F. ) ;
#29585 = CARTESIAN_POINT ( 'NONE',  ( -0.07293566597372513893, -79.72091539213137423, -1.249663842961500571 ) ) ;
#29586 = ORIENTED_EDGE ( 'NONE', *, *, #19172, .F. ) ;
#29587 = DIRECTION ( 'NONE',  ( -0.7071067811865475727, 0.000000000000000000, 0.7071067811865475727 ) ) ;
#29588 = FILL_AREA_STYLE_COLOUR ( '', #46362 ) ;
#29589 = CARTESIAN_POINT ( 'NONE',  ( 0.000000000000000000, -87.70000000000000284, 0.000000000000000000 ) ) ;
#29590 = ORIENTED_EDGE ( 'NONE', *, *, #14177, .F. ) ;
#29591 = ORIENTED_EDGE ( 'NONE', *, *, #48653, .T. ) ;
#29592 = CARTESIAN_POINT ( 'NONE',  ( -12.68625206992999921, -55.03580249152999926, -1.886949102778999965 ) ) ;
#29593 = ORIENTED_EDGE ( 'NONE', *, *, #54091, .T. ) ;
#29595 = ADVANCED_FACE ( 'NONE', ( #8719 ), #26710, .F. ) ;
#29594 = ORIENTED_EDGE ( 'NONE', *, *, #1218, .F. ) ;
#29596 = CARTESIAN_POINT ( 'NONE',  ( 10.35398566681999988, -23.40788276239999988, 7.619388279076999559 ) ) ;
#29597 = CARTESIAN_POINT ( 'NONE',  ( -0.9257816722924000485, -77.95516599075499187, 10.87742130684000053 ) ) ;
#29598 = APPLICATION_PROTOCOL_DEFINITION ( 'draft international standard', 'automotive_design', 1998, #8898 ) ;
#29599 = B_SPLINE_CURVE_WITH_KNOTS ( 'NONE', 3,
 ( #38968, #17399, #52841, #7674, #48423, #26833 ),
 .UNSPECIFIED., .F., .F.,
 ( 4, 2, 4 ),
 ( 0.000000000000000000, 0.5000000000000000000, 1.000000000000000000 ),
 .UNSPECIFIED. ) ;
#29600 = CARTESIAN_POINT ( 'NONE',  ( 0.000000000000000000, -39.30476017083000073, 0.000000000000000000 ) ) ;
#29601 = CARTESIAN_POINT ( 'NONE',  ( 6.635658238781000584, -78.50891332859899308, 7.210160158573999389 ) ) ;
#29602 = CARTESIAN_POINT ( 'NONE',  ( -1.734462217213118773, -78.21007448308577636, -9.085917012415309912 ) ) ;
#29603 = CARTESIAN_POINT ( 'NONE',  ( -2.047671225339077468E-06, -76.25353340279926329, -10.79679441329301959 ) ) ;
#29604 = VECTOR ( 'NONE', #56985, 1000.000000000000114 ) ;
#29605 = ORIENTED_EDGE ( 'NONE', *, *, #27793, .T. ) ;
#29606 = VERTEX_POINT ( 'NONE', #4292 ) ;
#29607 = CARTESIAN_POINT ( 'NONE',  ( -7.440986743656934799, -77.54937432391301400, 5.495388714296327137 ) ) ;
#29608 = DIRECTION ( 'NONE',  ( -0.3090169943748909409, 0.000000000000000000, -0.9510565162951719609 ) ) ;
#29609 = B_SPLINE_CURVE_WITH_KNOTS ( 'NONE', 3,
 ( #40728, #4117, #41019, #53722, #30959, #44863, #54016, #49293, #9143, #8844, #57845, #40127, #319, #5004, #23008, #49891, #26835, #27128, #12682, #4416, #35386, #13557, #45461, #22715, #9435, #17402, #35694, #8257, #611, #22418, #18592, #40430, #21827, #58140, #39832, #36291, #48711, #13260, #53133, #13853, #45166, #48997, #54313, #22118, #31251, #26256, #4716, #21, #18001, #31849, #44270, #53415, #12962, #8544, #26536, #44563, #24175, #6165, #19458, #23586, #37454, #1469, #18876, #10314, #37750, #55772, #42191, #1760, #33013, #14431, #46637, #5575, #19754, #37164, #14141, #894, #36870, #50180, #36582, #28293, #10024, #54604, #55473, #55177, #46345, #32426, #28592, #15319, #32141, #28002, #46051, #9726, #15019, #1180, #33313, #50472, #27714 ),
 .UNSPECIFIED., .F., .F.,
 ( 4, 2, 2, 2, 1, 1, 1, 2, 2, 2, 2, 2, 1, 1, 1, 2, 2, 2, 2, 2, 1, 1, 1, 2, 2, 2, 2, 2, 1, 1, 1, 2, 2, 2, 2, 2, 1, 1, 1, 2, 2, 2, 2, 2, 1, 1, 1, 2, 2, 2, 2, 2, 1, 1, 1, 2, 2, 2, 4 ),
 ( 0.000000000000000000, 0.06249999999989072630, 0.09374999999983574250, 0.1093749999998082506, 0.1171874999997942757, 0.1210937499997875449, 0.1230468749997841726, 0.1240234374997827155, 0.1249999999997812583, 0.1874999999996865008, 0.2187499999996390665, 0.2343749999996153355, 0.2421874999996037059, 0.2460937499995978495, 0.2480468749995949074, 0.2490234374995934641, 0.2499999999995919930, 0.3124999999994510502, 0.3437499999993806066, 0.3593749999993457456, 0.3671874999993280375, 0.3710937499993191557, 0.3730468749993147703, 0.3740234374993125499, 0.3749999999993103295, 0.4374999999993330890, 0.4687499999993448574, 0.4843749999993509636, 0.4921874999993540167, 0.4960937499993555710, 0.4980468749993561817, 0.4990234374993564592, 0.4999999999993567368, 0.5624999999993588462, 0.5937499999993598454, 0.6093749999993606226, 0.6171874999993607336, 0.6210937499993607336, 0.6230468749993607336, 0.6240234374993610666, 0.6249999999993612887, 0.6874999999994607647, 0.7187499999995101696, 0.7343749999995347055, 0.7421874999995472511, 0.7460937499995535793, 0.7480468749995566879, 0.7490234374995581312, 0.7499999999995596855, 0.8124999999996873612, 0.8437499999997515321, 0.8593749999997836175, 0.8671874999997996047, 0.8710937499998074873, 0.8730468749998111511, 0.8740234374998130384, 0.8749999999998148148, 0.9374999999999074074, 1.000000000000000000 ),
 .UNSPECIFIED. ) ;
#29610 = DIRECTION ( 'NONE',  ( 0.000000000000000000, 1.000000000000000000, 0.000000000000000000 ) ) ;
#29611 = CARTESIAN_POINT ( 'NONE',  ( 0.8618009059429999619, -78.46222785155198665, -9.665816497589000633 ) ) ;
#29612 = CARTESIAN_POINT ( 'NONE',  ( 7.668936932623999780, -22.77152778045000048, 10.21380041493000057 ) ) ;
#29613 = CARTESIAN_POINT ( 'NONE',  ( 12.50000000000000000, -51.86282895648000135, 0.000000000000000000 ) ) ;
#29614 = CARTESIAN_POINT ( 'NONE',  ( 0.000000000000000000, -76.39999999999899671, -3.399999999997999733 ) ) ;
#29615 = DIRECTION ( 'NONE',  ( 0.7071067811865475727, 0.000000000000000000, -0.7071067811865475727 ) ) ;
#29616 = CARTESIAN_POINT ( 'NONE',  ( 1.349451115848000038, -79.91266235632998871, -0.8326934693224998796 ) ) ;
#29617 = EDGE_CURVE ( 'NONE', #42760, #28272, #17168, .T. ) ;
#29618 = CIRCLE ( 'NONE', #46640, 3.799999999999999822 ) ;
#29619 = CARTESIAN_POINT ( 'NONE',  ( -0.3673871636652999983, -82.25905252924800948, -1.180734503437000038 ) ) ;
#29620 = EDGE_CURVE ( 'NONE', #24195, #10296, #1343, .T. ) ;
#29621 = CARTESIAN_POINT ( 'NONE',  ( -0.6605212418366763760, -79.83899751728472438, -1.359602850557828591 ) ) ;
#29622 = CARTESIAN_POINT ( 'NONE',  ( -9.816946295765999864, -77.95406332859900544, -1.359421753724999959 ) ) ;
#29623 = CARTESIAN_POINT ( 'NONE',  ( 9.450487096927000508, -77.89901585959799490, -7.362360902974999455 ) ) ;
#29624 = CARTESIAN_POINT ( 'NONE',  ( 2.062597299672999540, -22.78485473281999774, -12.87022657272000004 ) ) ;
#29626 = CARTESIAN_POINT ( 'NONE',  ( 13.98934701301999972, -32.57813015402999923, 1.420884290714999950E-05 ) ) ;
#29625 = FACE_OUTER_BOUND ( 'NONE', #41508, .T. ) ;
#29627 = CARTESIAN_POINT ( 'NONE',  ( 6.112256811392500211, -79.41782375574760522, 6.968603012018727227 ) ) ;
#29628 = CARTESIAN_POINT ( 'NONE',  ( -8.481311802608001216, -79.93973307352598567, 6.721462691642999587 ) ) ;
#29629 = CARTESIAN_POINT ( 'NONE',  ( -12.00000000000000000, -79.29999999999999716, 0.000000000000000000 ) ) ;
#29630 = LINE ( 'NONE', #55644, #53479 ) ;
#29631 = CARTESIAN_POINT ( 'NONE',  ( 2.859635500329999580, -0.9504959227639564467, -2.056314849297946612 ) ) ;
#29632 = ORIENTED_EDGE ( 'NONE', *, *, #57353, .F. ) ;
#29633 = CARTESIAN_POINT ( 'NONE',  ( -10.05000000000000071, -87.20000000000000284, 0.000000000000000000 ) ) ;
#29634 = DIRECTION ( 'NONE',  ( -2.493024943570999650E-13, -1.000000000000000000, 2.029372555462999773E-12 ) ) ;
#29635 = CARTESIAN_POINT ( 'NONE',  ( 10.06692933833339687, -18.29657287078697792, -7.655995045172042879 ) ) ;
#29636 = CARTESIAN_POINT ( 'NONE',  ( 0.5914329913499263291, -78.43615203708624506, 1.104891015251897368 ) ) ;
#29637 = CARTESIAN_POINT ( 'NONE',  ( -9.167409920518998945, -79.41814682224598698, -2.989462504633000339 ) ) ;
#29638 = CARTESIAN_POINT ( 'NONE',  ( 2.814035350851149087, -76.95432989093133358, 10.47073005108091692 ) ) ;
#29639 = CARTESIAN_POINT ( 'NONE',  ( 0.000000000000000000, 4.040000000000000036, 0.000000000000000000 ) ) ;
#29640 = CARTESIAN_POINT ( 'NONE',  ( 0.4254240051736215000, -3.135416666666666075, -3.250000000000000000 ) ) ;
#29641 = DIRECTION ( 'NONE',  ( 0.7071067811865475727, 0.000000000000000000, 0.7071067811865475727 ) ) ;
#29642 = CARTESIAN_POINT ( 'NONE',  ( -3.992195115638344838, -78.62148118236265759, -0.07526023106989525313 ) ) ;
#29643 = CARTESIAN_POINT ( 'NONE',  ( 7.906400319760000350, -78.06002966580298619, -7.572567058774000159 ) ) ;
#29644 = AXIS2_PLACEMENT_3D ( 'NONE', #43822, #31072, #49110 ) ;
#29645 = CARTESIAN_POINT ( 'NONE',  ( 0.5211352025712173708, -76.32812523379961078, -11.74973435454385040 ) ) ;
#29646 = CARTESIAN_POINT ( 'NONE',  ( -8.675294248905000671, -77.65483863155199629, 6.999562148146999618 ) ) ;
#29647 = B_SPLINE_CURVE_WITH_KNOTS ( 'NONE', 3,
 ( #41819, #12961, #19389, #14941, #30958, #48996, #8543, #26535, #44562, #42118, #43280, #34396, #24399, #16123, #29105, #38256, #52427, #20831, #38548, #15242, #55693, #11411, #24689, #42700, #20552, #37675, #33532, #33234, #51279, #2265, #7260, #20265, #34101, #56853, #6680, #56279, #46856, #11986, #16412, #15829, #33817, #52141, #51856, #29391, #47438, #6968, #42993, #24972, #10833, #51569, #11127, #46566, #2549, #19978, #56562, #11700, #6090, #29676, #28809, #42413, #24099, #47726, #25261, #1685, #2834, #38838, #1983, #6385, #19675, #37964, #55990, #15537, #47149, #25836, #26697, #44429, #48581, #16702, #53287, #43864, #35556, #12833, #58306 ),
 .UNSPECIFIED., .F., .F.,
 ( 4, 2, 1, 2, 2, 2, 2, 2, 2, 2, 2, 2, 2, 2, 2, 2, 2, 1, 2, 2, 2, 2, 2, 2, 2, 2, 2, 2, 2, 1, 2, 2, 2, 2, 2, 2, 2, 2, 2, 2, 2, 2, 4 ),
 ( 0.000000000000000000, 0.01562499999999997918, 0.03124999999999995837, 0.04687499999999994449, 0.06249999999999993061, 0.07812499999999991673, 0.09374999999999991673, 0.1249999999999998890, 0.1562499999999998612, 0.1874999999999998612, 0.2187499999999998335, 0.2499999999999998335, 0.2812499999999998335, 0.3124999999999998335, 0.3281249999999998335, 0.3437499999999998335, 0.3593749999999997780, 0.3749999999999998335, 0.3906249999999998890, 0.4062499999999998890, 0.4374999999999998335, 0.4687499999999998335, 0.4999999999999997780, 0.5312499999999997780, 0.5624999999999996669, 0.5937499999999996669, 0.6249999999999995559, 0.6562499999999995559, 0.6718749999999995559, 0.6874999999999995559, 0.7031249999999995559, 0.7187499999999994449, 0.7343749999999994449, 0.7499999999999994449, 0.7812499999999995559, 0.8124999999999995559, 0.8437499999999996669, 0.8749999999999996669, 0.9062499999999997780, 0.9374999999999998890, 0.9687499999999998890, 0.9843749999999998890, 1.000000000000000000 ),
 .UNSPECIFIED. ) ;
#29648 = CARTESIAN_POINT ( 'NONE',  ( -0.9121818130210588293, -82.04075852875078567, 0.8543134884758614156 ) ) ;
#29649 = CARTESIAN_POINT ( 'NONE',  ( -3.027333896924861101, -1.068427606005047048, 1.360419436555698969 ) ) ;
#29650 = CARTESIAN_POINT ( 'NONE',  ( -9.467475792354999697, -77.31375831598298021, 1.978357023055999919 ) ) ;
#29651 = CARTESIAN_POINT ( 'NONE',  ( 8.857115352654000517, -79.22924415034600543, -3.584237475251999872 ) ) ;
#29652 = CARTESIAN_POINT ( 'NONE',  ( -8.796335266380006956, -77.54791666666667993, 6.760013919724027431 ) ) ;
#29653 = CARTESIAN_POINT ( 'NONE',  ( 1.500000000000000000, -81.25000000000000000, 0.000000000000000000 ) ) ;
#29654 = CARTESIAN_POINT ( 'NONE',  ( -1.384806900013862530, -80.93538967717266530, -0.6660020126448532585 ) ) ;
#29655 = CARTESIAN_POINT ( 'NONE',  ( 8.554245750310725427, -80.04392919279416674, -7.255790090871102826 ) ) ;
#29656 = CARTESIAN_POINT ( 'NONE',  ( -2.112861425255000203, -79.10926721811499363, -11.84242215301999934 ) ) ;
#29657 = AXIS2_PLACEMENT_3D ( 'NONE', #16397, #3679, #30242 ) ;
#29658 = CARTESIAN_POINT ( 'NONE',  ( -0.7676956659902818281, -78.17301476101459912, -0.9990819215154366217 ) ) ;
#29659 =( BOUNDED_SURFACE ( )  B_SPLINE_SURFACE ( 3, 3, ( 
 ( #29033, #55914, #15466, #51496 ),
 ( #6601, #24612, #42627, #11624 ),
 ( #14477, #28633, #27757, #1222 ),
 ( #28926, #46683, #45801, #6203 ),
 ( #23919, #937, #28335, #46969 ),
 ( #41937, #32468, #42235, #46386 ),
 ( #10946, #33356, #5910, #650 ) ),
 .UNSPECIFIED., .F., .F., .F. ) 
 B_SPLINE_SURFACE_WITH_KNOTS ( ( 4, 3, 4 ),
 ( 4, 4 ),
 ( 0.000000000000000000, 1.000000000000000000, 2.000000000000000000 ),
 ( 0.000000000000000000, 1.000000000000000000 ),
 .UNSPECIFIED. ) 
 GEOMETRIC_REPRESENTATION_ITEM ( )  RATIONAL_B_SPLINE_SURFACE ( (
 ( 1.196373642248999891, 1.184225762575999985, 1.184225762575999985, 1.196373642248999891),
 ( 0.9447739570234999773, 0.9351807998836999536, 0.9351807998836999536, 0.9447739570234999773),
 ( 0.9447739570234999773, 0.9351807998836999536, 0.9351807998836999536, 0.9447739570234999773),
 ( 1.196373642248999891, 1.184225762575999985, 1.184225762575999985, 1.196373642248999891),
 ( 0.9447739570234999773, 0.9351807998836999536, 0.9351807998836999536, 0.9447739570234999773),
 ( 0.9447739570234999773, 0.9351807998836999536, 0.9351807998836999536, 0.9447739570234999773),
 ( 1.196373642248999891, 1.184225762575999985, 1.184225762575999985, 1.196373642248999891) ) ) 
 REPRESENTATION_ITEM ( '' )  SURFACE ( )  );
#29660 = CARTESIAN_POINT ( 'NONE',  ( -7.330610599118999815, -79.25481274797898834, 8.549626471514999437 ) ) ;
#29661 = VERTEX_POINT ( 'NONE', #50057 ) ;
#29662 = CARTESIAN_POINT ( 'NONE',  ( 1.495357591751715010, -24.55876337363582707, 12.70444646759489693 ) ) ;
#29663 = EDGE_LOOP ( 'NONE', ( #38098, #28357, #13551, #50677 ) ) ;
#29665 = ADVANCED_FACE ( 'NONE', ( #50642 ), #46071, .F. ) ;
#29664 = ORIENTED_EDGE ( 'NONE', *, *, #5634, .F. ) ;
#29666 = CARTESIAN_POINT ( 'NONE',  ( 3.415507079190750250, -3.499999999999999556, -0.9241186193027908224 ) ) ;
#29667 = ORIENTED_EDGE ( 'NONE', *, *, #16117, .T. ) ;
#29668 = CARTESIAN_POINT ( 'NONE',  ( -3.453006609811000160, -78.85439465482099308, 0.4995584808644000230 ) ) ;
#29669 = CARTESIAN_POINT ( 'NONE',  ( 4.302121030171025318, -79.23722901812243435, 8.469798634234269485 ) ) ;
#29670 = ORIENTED_EDGE ( 'NONE', *, *, #32095, .F. ) ;
#29671 = CARTESIAN_POINT ( 'NONE',  ( -1.250000000000000000, -82.59999999999999432, 0.000000000000000000 ) ) ;
#29672 = ORIENTED_EDGE ( 'NONE', *, *, #8769, .T. ) ;
#29673 = DIRECTION ( 'NONE',  ( 0.000000000000000000, -1.000000000000000000, 0.000000000000000000 ) ) ;
#29674 = ORIENTED_EDGE ( 'NONE', *, *, #19298, .T. ) ;
#29675 = CARTESIAN_POINT ( 'NONE',  ( 0.2851276402532497700, -79.45731520756731925, 1.217241021790539390 ) ) ;
#29676 = CARTESIAN_POINT ( 'NONE',  ( -1.489116662163645133, -78.23734471912871413, 0.2394897313045940002 ) ) ;
#29677 = CARTESIAN_POINT ( 'NONE',  ( 9.290912487798001607, -79.80000000000001137, 7.341183704965414947 ) ) ;
#29678 = CARTESIAN_POINT ( 'NONE',  ( -9.805087678983213095, -80.06653000188077840, 4.415917898387408336 ) ) ;
#29679 = PLANE ( 'NONE',  #39051 ) ;
#29680 = CARTESIAN_POINT ( 'NONE',  ( 2.491951192718460106, -86.40321104920799655, -3.499781323192636684 ) ) ;
#29681 = CARTESIAN_POINT ( 'NONE',  ( -1.660522255173999984, -76.72075361110900360, 11.05968181062000077 ) ) ;
#29682 = CARTESIAN_POINT ( 'NONE',  ( -11.44417895085272008, -77.27916666666668277, 3.075537641221497420 ) ) ;
#29683 = CARTESIAN_POINT ( 'NONE',  ( 9.670688080733903291, -77.09852982711514358, -0.1674119159864788653 ) ) ;
#29684 = CONICAL_SURFACE ( 'NONE', #35356, 0.6999999997695030007, 0.7853981633972997312 ) ;
#29685 = CARTESIAN_POINT ( 'NONE',  ( -3.304785372409708710, -78.69605523039359696, -8.639930098831065663 ) ) ;
#29686 = B_SPLINE_CURVE_WITH_KNOTS ( 'NONE', 3,
 ( #56398, #51979, #7093, #43115, #20669, #49278 ),
 .UNSPECIFIED., .F., .F.,
 ( 4, 2, 4 ),
 ( 0.000000000000000000, 0.5000000000000000000, 1.000000000000000000 ),
 .UNSPECIFIED. ) ;
#29687 = EDGE_CURVE ( 'NONE', #36499, #10154, #43221, .T. ) ;
#29688 = CARTESIAN_POINT ( 'NONE',  ( -0.1698911186725000078, -80.56327785860300139, 1.322768475116000042 ) ) ;
#29689 = CIRCLE ( 'NONE', #23083, 1.750000000000001998 ) ;
#29690 = DIRECTION ( 'NONE',  ( 0.000000000000000000, -1.000000000000000000, 0.000000000000000000 ) ) ;
#29691 = CARTESIAN_POINT ( 'NONE',  ( -9.500000000000000000, -77.29999999999999716, 0.000000000000000000 ) ) ;
#29692 = CARTESIAN_POINT ( 'NONE',  ( -0.3926621439294999960, -80.24528455456798781, -3.735930744721999819 ) ) ;
#29693 = CARTESIAN_POINT ( 'NONE',  ( -8.948369457197285826, -78.05341261098192263, 5.957113593040013200 ) ) ;
#29694 = DIRECTION ( 'NONE',  ( -1.000000000000000000, 0.000000000000000000, 0.000000000000000000 ) ) ;
#29695 = CARTESIAN_POINT ( 'NONE',  ( 3.435184454807999721, -84.06599735065199752, 0.8743406370706999775 ) ) ;
#29696 = CARTESIAN_POINT ( 'NONE',  ( -12.50000000000000000, -49.87071422276000021, 0.000000000000000000 ) ) ;
#29697 = CARTESIAN_POINT ( 'NONE',  ( 1.980584515752000119, -60.06485146591000301, -12.76303204605000197 ) ) ;
#29698 = CARTESIAN_POINT ( 'NONE',  ( -7.633403016722000167, -60.18650073818000124, -10.18126993295000027 ) ) ;
#29699 = CIRCLE ( 'NONE', #4259, 11.70000000000000107 ) ;
#29700 = FACE_OUTER_BOUND ( 'NONE', #17919, .T. ) ;
#29701 = B_SPLINE_CURVE_WITH_KNOTS ( 'NONE', 3,
 ( #7718, #7432, #22155, #8290, #8582, #25434, #57591, #26570, #43449, #3863, #21005, #35425, #21291, #53168, #48461, #44603, #34567, #57020, #16581, #53455, #30136, #57883, #26294, #25721, #39870, #57309, #12999, #30429, #52599, #12151, #48186, #43746, #3298, #48747, #12717, #21863, #52883, #21581, #8004, #30997, #12436, #26001, #44026, #3577, #44307, #8877, #50207, #36322, #41342, #9175, #26871, #10054, #58, #28036, #23615, #36899, #350, #46081, #49331, #32455, #40466, #27453, #13587, #14464, #9757, #5605, #44898, #4451, #5034, #13294, #36613, #18329, #9468, #22452, #50500, #49627, #54346, #54912, #27742, #18033, #41628, #36026, #54052, #45491, #13885, #40756, #31880, #31287, #49923, #45789, #23036, #54635, #31582, #14171, #1208, #27159, #926, #41052, #45198, #32168, #5325, #19200, #23332, #37191, #4745, #639, #22746, #18622, #18906, #29486, #42800, #46664, #42509, #47543, #51088, #51953, #11221, #15349, #41923, #20077, #10637, #2362, #6191, #43092, #55798, #33041, #23905, #20359, #37777, #28619, #7067, #47245, #33914, #1787, #15049, #24785, #38354, #24204, #56376, #15927, #38069, #37478, #25069, #33342, #11509, #28913, #2650, #20644, #55205, #14748, #51673, #42221, #6777, #19783, #32748, #51375, #50796, #19485, #55501, #10341, #28320, #46372, #10932, #5896, #56089, #46957, #6484, #24495, #1495, #2079, #15635, #33631, #29200, #34196, #17074, #3222, #8214, #34487, #52234, #35349, #25352, #12074, #29765 ),
 .UNSPECIFIED., .F., .F.,
 ( 4, 2, 1, 1, 1, 1, 2, 2, 2, 2, 1, 1, 1, 1, 1, 1, 2, 2, 2, 2, 2, 1, 1, 1, 1, 1, 2, 2, 2, 1, 1, 1, 1, 2, 2, 2, 2, 1, 1, 1, 1, 2, 2, 2, 2, 2, 2, 2, 1, 1, 1, 1, 2, 2, 2, 2, 2, 1, 1, 1, 1, 2, 2, 2, 2, 1, 1, 1, 1, 1, 1, 2, 2, 2, 2, 2, 2, 2, 2, 2, 1, 1, 1, 1, 1, 2, 2, 2, 2, 1, 1, 2, 2, 2, 2, 1, 1, 1, 2, 2, 2, 2, 2, 1, 1, 1, 1, 1, 2, 2, 2, 2, 2, 1, 1, 1, 2, 2, 4 ),
 ( 0.000000000000000000, 0.03125000000005081352, 0.04687500000007623763, 0.05468750000008895662, 0.05859375000009531265, 0.06054687500009849760, 0.06152343750010012130, 0.06250000000010175194, 0.09375000000015386303, 0.1093750000001798978, 0.1171875000001929429, 0.1210937500001994238, 0.1230468750002026851, 0.1240234375002043643, 0.1245117187502051553, 0.1247558593752055855, 0.1248779296877058076, 0.1250000000002060296, 0.1562500000002606804, 0.1718750000002879919, 0.1796875000003016198, 0.1835937500003083644, 0.1855468750003117229, 0.1865234375003133049, 0.1870117187503139711, 0.1872558593753144152, 0.1873779296878145262, 0.1875000000003146650, 0.2031250000003272105, 0.2109375000003335388, 0.2148437500003366751, 0.2167968750003382850, 0.2177734375003390621, 0.2182617187503395062, 0.2187500000003399225, 0.2343750000003542444, 0.2421875000003613498, 0.2460937500003649026, 0.2480468750003666512, 0.2490234375003675393, 0.2495117187503679834, 0.2497558593753683165, 0.2500000000003685940, 0.2812500000004109491, 0.3125000000004533041, 0.3437500000004956036, 0.3593750000005168088, 0.3671875000005274114, 0.3710937500005328515, 0.3730468750005358491, 0.3740234375005368483, 0.3745117187505374035, 0.3747558593755371814, 0.3750000000005369594, 0.4062500000005068168, 0.4218750000004917178, 0.4296875000004841127, 0.4335937500004803935, 0.4355468750004785061, 0.4365234375004776179, 0.4370117187504771183, 0.4372558593754768963, 0.4375000000004766743, 0.4687500000004548029, 0.4843750000004438117, 0.4921875000004383716, 0.4960937500004356515, 0.4980468750004342637, 0.4990234375004335421, 0.4995117187504332645, 0.4997558593754330980, 0.4998779296879329870, 0.5000000000004328760, 0.5625000000003597123, 0.6250000000002866596, 0.6562500000002500222, 0.6875000000002134959, 0.7187500000001769696, 0.7343750000001587619, 0.7421875000001495470, 0.7460937500001449951, 0.7480468750001427747, 0.7490234375001416645, 0.7495117187501411093, 0.7497558593751408873, 0.7498779296876407763, 0.7500000000001405542, 0.7656250000001202372, 0.7734375000001100231, 0.7773437500001049161, 0.7792968750001023626, 0.7802734375001010303, 0.7812500000000996980, 0.7968750000000796030, 0.8046875000000695000, 0.8085937500000645040, 0.8105468750000618394, 0.8115234375000606182, 0.8120117187500600631, 0.8125000000000595080, 0.8437500000000257572, 0.8593750000000086597, 0.8671875000000003331, 0.8710937499999961142, 0.8730468749999940048, 0.8740234374999928946, 0.8745117187499923395, 0.8747558593749921174, 0.8748779296874918954, 0.8749999999999917843, 0.9062499999999941158, 0.9218749999999952260, 0.9296874999999957812, 0.9335937499999960032, 0.9355468749999962252, 0.9365234374999962252, 0.9370117187499962252, 0.9374999999999963363, 1.000000000000000000 ),
 .UNSPECIFIED. ) ;
#29702 = ADVANCED_FACE ( 'NONE', ( #1525 ), #42146, .F. ) ;
#29703 = CARTESIAN_POINT ( 'NONE',  ( -12.50745077490000057, -17.00005551713000074, 2.011909873286000185E-09 ) ) ;
#29705 = ADVANCED_FACE ( 'NONE', ( #33076 ), #37081, .F. ) ;
#29704 = CARTESIAN_POINT ( 'NONE',  ( -1.460959015002473826, -80.42083333333334849, -0.3926218265389207485 ) ) ;
#29706 = DIRECTION ( 'NONE',  ( -0.7071067811865969777, 0.7071067811864980568, -6.623700168368979662E-09 ) ) ;
#29707 = CARTESIAN_POINT ( 'NONE',  ( 9.684822944874866835, -78.30969691107382857, -5.379607873393639217 ) ) ;
#29708 = CARTESIAN_POINT ( 'NONE',  ( 1.501534314719157326, -24.55152951663309224, -12.70455943739907845 ) ) ;
#29709 = CARTESIAN_POINT ( 'NONE',  ( 10.65858277789999953, -75.78824986905000571, 6.553927674015000093 ) ) ;
#29710 = ORIENTED_EDGE ( 'NONE', *, *, #40776, .F. ) ;
#29711 = CARTESIAN_POINT ( 'NONE',  ( 3.620209227050000145, -85.94828561723799965, -1.611820994701000043 ) ) ;
#29712 = CARTESIAN_POINT ( 'NONE',  ( 12.72397319118000070, -60.02144180272999563, 1.930910316632999946 ) ) ;
#29713 = CARTESIAN_POINT ( 'NONE',  ( -12.63427402858000015, -78.67048691447000408, -0.3091878550698000105 ) ) ;
#29714 = CARTESIAN_POINT ( 'NONE',  ( 12.59682398755999877, -55.41262488626999527, -1.801644812721000077 ) ) ;
#29715 = CARTESIAN_POINT ( 'NONE',  ( 1.251117773441000169, -77.75769513184299342, 9.549236319306000809 ) ) ;
#29716 = CARTESIAN_POINT ( 'NONE',  ( 0.3142805516909999430, -82.81955637232998413, 4.160687065221000402 ) ) ;
#29717 = CARTESIAN_POINT ( 'NONE',  ( 3.211701487445925984, -79.95131508034484114, 10.27501478995334949 ) ) ;
#29718 = CARTESIAN_POINT ( 'NONE',  ( 1.237149555198000073, -79.18640437465400339, -1.037631781681999987 ) ) ;
#29719 = ORIENTED_EDGE ( 'NONE', *, *, #26817, .T. ) ;
#29720 = DIRECTION ( 'NONE',  ( -0.7071067811865475727, 0.000000000000000000, -0.7071067811865475727 ) ) ;
#29721 = ADVANCED_FACE ( 'NONE', ( #19748 ), #14134, .F. ) ;
#29722 = CARTESIAN_POINT ( 'NONE',  ( 2.420934736278871569, -78.97605044823936282, -2.640979877710285972 ) ) ;
#29723 = EDGE_LOOP ( 'NONE', ( #4393, #43486, #6434, #14349 ) ) ;
#29724 = B_SPLINE_CURVE_WITH_KNOTS ( 'NONE', 3,
 ( #27623, #58347, #49799, #1090 ),
 .UNSPECIFIED., .F., .F.,
 ( 4, 4 ),
 ( 0.000000000000000000, 1.000000000000000000 ),
 .UNSPECIFIED. ) ;
#29725 = CARTESIAN_POINT ( 'NONE',  ( 5.312973029106999867, -78.20546044413198672, 9.563478878364000124 ) ) ;
#29726 = CARTESIAN_POINT ( 'NONE',  ( -7.401770473315045784, -55.34844303569003898, -8.137215171343788356 ) ) ;
#29727 = CARTESIAN_POINT ( 'NONE',  ( -9.428734693618999074, -79.82940494353799465, 5.424968178012999687 ) ) ;
#29728 = ORIENTED_EDGE ( 'NONE', *, *, #40709, .F. ) ;
#29729 = ORIENTED_EDGE ( 'NONE', *, *, #42988, .T. ) ;
#29731 = EDGE_CURVE ( 'NONE', #8867, #19870, #53140, .T. ) ;
#29730 = EDGE_LOOP ( 'NONE', ( #53941, #51632, #57053 ) ) ;
#29732 = CARTESIAN_POINT ( 'NONE',  ( -0.8376080881386354093, -80.53392362615774402, 0.9306764106483600418 ) ) ;
#29733 = EDGE_CURVE ( 'NONE', #46351, #31027, #21396, .T. ) ;
#29734 = CARTESIAN_POINT ( 'NONE',  ( -3.654181822837000215, -86.12610001214198974, 1.626946589673999854 ) ) ;
#29735 = CARTESIAN_POINT ( 'NONE',  ( -8.396223008680999911, -80.17283464191400810, -4.990405176070999538 ) ) ;
#29736 = ORIENTED_EDGE ( 'NONE', *, *, #1245, .T. ) ;
#29737 = ORIENTED_EDGE ( 'NONE', *, *, #16724, .F. ) ;
#29738 = CARTESIAN_POINT ( 'NONE',  ( 0.7032092222470416321, -79.47867041308421676, 1.062278989215700742 ) ) ;
#29739 = CARTESIAN_POINT ( 'NONE',  ( 8.813891479047955002, -25.01010130368346296, 8.872963530592734571 ) ) ;
#29740 = CARTESIAN_POINT ( 'NONE',  ( 8.541162059860999634, -53.79199348416999982, 9.205819316548000231 ) ) ;
#29741 = CARTESIAN_POINT ( 'NONE',  ( 1.310679582531385501, -80.69166666666669130, 0.7554284705563518720 ) ) ;
#29742 = DIRECTION ( 'NONE',  ( 1.000000000000000000, 0.000000000000000000, 0.000000000000000000 ) ) ;
#29743 = CARTESIAN_POINT ( 'NONE',  ( 0.000000000000000000, -5.899999999999999467, 0.000000000000000000 ) ) ;
#29744 = CARTESIAN_POINT ( 'NONE',  ( 6.205001111027785399, -80.17721126027063860, 9.095289649731126858 ) ) ;
#29745 = CARTESIAN_POINT ( 'NONE',  ( 11.95248949435000085, -78.90537670790513403, 0.8087524912306001124 ) ) ;
#29746 = CARTESIAN_POINT ( 'NONE',  ( 3.457929002525866213, -82.32291668600672097, -2.035687669133669164 ) ) ;
#29747 = CARTESIAN_POINT ( 'NONE',  ( -7.633501923154999425, -23.20104675770999947, 10.36289748052999826 ) ) ;
#29748 = CARTESIAN_POINT ( 'NONE',  ( -1.507378969381000022, -79.00557046129088690, -3.890280846631000156 ) ) ;
#29749 = CARTESIAN_POINT ( 'NONE',  ( 9.252740428349001789, -78.12916666666666288, -2.486604901413144830 ) ) ;
#29750 = CARTESIAN_POINT ( 'NONE',  ( 9.778543098509999254, -61.84857981670000271, -8.284584910426000093 ) ) ;
#29751 = CARTESIAN_POINT ( 'NONE',  ( -1.500000000000000000, -81.50000000000000000, 0.000000000000000000 ) ) ;
#29752 = DIRECTION ( 'NONE',  ( 0.9999999999999992228, 4.158392524217991108E-08, 7.906211575362985062E-12 ) ) ;
#29753 = DIRECTION ( 'NONE',  ( 0.9859154929577472748, 0.1672442547470080754, 0.000000000000000000 ) ) ;
#29754 = CARTESIAN_POINT ( 'NONE',  ( -3.140974612311351777, -77.90416666666665435, -11.68767212001978884 ) ) ;
#29755 = AXIS2_PLACEMENT_3D ( 'NONE', #23543, #5827, #50728 ) ;
#29756 = CARTESIAN_POINT ( 'NONE',  ( -1.403374235224089883, -80.78031274248239413, -0.5631813226398475480 ) ) ;
#29757 = CARTESIAN_POINT ( 'NONE',  ( 12.83836863002999884, -60.00626272179999887, -2.062146390631000248 ) ) ;
#29758 = CARTESIAN_POINT ( 'NONE',  ( 0.9995835529977233902, -79.30208333333332860, 0.7681833999686461523 ) ) ;
#29759 = CARTESIAN_POINT ( 'NONE',  ( 1.199500263597271799, -78.69791666666667140, -0.9218200799623701425 ) ) ;
#29760 = ADVANCED_FACE ( 'NONE', ( #10308 ), #23294, .F. ) ;
#29761 = CARTESIAN_POINT ( 'NONE',  ( -3.098209881784000252, -2.427646227706999671, 1.748874889861999904 ) ) ;
#29762 = CONICAL_SURFACE ( 'NONE', #51604, 10.93038838648999977, 1.373400766944759877 ) ;
#29763 = CARTESIAN_POINT ( 'NONE',  ( -3.132815200277000223, -78.04540922883299459, -11.75448848339000030 ) ) ;
#29764 = CARTESIAN_POINT ( 'NONE',  ( 9.618404959434000645, -78.03338022121498341, 1.531659799953999812 ) ) ;
#29766 = CARTESIAN_POINT ( 'NONE',  ( 0.9728932632037999850, -79.05095245453999553, 0.8910916192982000217 ) ) ;
#29765 = CARTESIAN_POINT ( 'NONE',  ( -11.75000000000000000, -76.20000000000000284, -1.391479524197000231E-14 ) ) ;
#29767 = CARTESIAN_POINT ( 'NONE',  ( 1.358765745638999878, -82.42429828359199462, 0.5569594143531000352 ) ) ;
#29768 = CARTESIAN_POINT ( 'NONE',  ( -7.686918321221999584, -20.24439829127999957, 10.48771805383000100 ) ) ;
#29769 = VECTOR ( 'NONE', #49277, 1000.000000000000000 ) ;
#29770 = VERTEX_POINT ( 'NONE', #37157 ) ;
#29771 = CARTESIAN_POINT ( 'NONE',  ( -10.55910102244999926, -19.21514526754999963, -7.642147947538999730 ) ) ;
#29772 = CARTESIAN_POINT ( 'NONE',  ( 2.198909403236999793, -79.76316569920798827, -11.72178803194999830 ) ) ;
#29773 = CARTESIAN_POINT ( 'NONE',  ( 9.081835416235971792, -79.47540137645063396, -2.898796417172264217 ) ) ;
#29774 = CARTESIAN_POINT ( 'NONE',  ( -0.7301085713275398126, -79.99999999999998579, -9.448919309928943022 ) ) ;
#29775 = CARTESIAN_POINT ( 'NONE',  ( -7.760939450761999758, -61.03085356300000086, 10.15321588361999972 ) ) ;
#29776 = DIRECTION ( 'NONE',  ( 0.000000000000000000, -1.000000000000000000, 0.000000000000000000 ) ) ;
#29777 = CARTESIAN_POINT ( 'NONE',  ( 9.743790892929999004, -80.00705849419799165, -1.701210078859999975 ) ) ;
#29778 = CARTESIAN_POINT ( 'NONE',  ( 8.485281374238999419, -59.94999999967000548, -8.485281374238999419 ) ) ;
#29779 = CARTESIAN_POINT ( 'NONE',  ( 7.396918292183175758, -79.19791666666665719, -5.684557159767951617 ) ) ;
#29780 = VERTEX_POINT ( 'NONE', #10601 ) ;
#29781 = CARTESIAN_POINT ( 'NONE',  ( 9.699999999837999098, -87.69999999983798489, 3.624870943809000214E-09 ) ) ;
#29782 = CARTESIAN_POINT ( 'NONE',  ( 9.458574655020427713, -79.24897924367529356, -7.006660078105245937 ) ) ;
#29783 = CARTESIAN_POINT ( 'NONE',  ( -8.855994692495000820, -79.78646001420200662, 4.059079031676999350 ) ) ;
#29784 = ADVANCED_FACE ( 'NONE', ( #14426 ), #31869, .F. ) ;
#29785 = CARTESIAN_POINT ( 'NONE',  ( 0.2454699089725678463, -81.45983395354696199, 1.225829166526236191 ) ) ;
#29786 = EDGE_CURVE ( 'NONE', #51185, #15436, #12968, .T. ) ;
#29787 = CARTESIAN_POINT ( 'NONE',  ( 1.520902128651999918, -81.10537593950999735, -0.6797894616744000196 ) ) ;
#29788 = ORIENTED_EDGE ( 'NONE', *, *, #38802, .F. ) ;
#29789 = CARTESIAN_POINT ( 'NONE',  ( -1.184185271002474060, -78.61999039302729386, 0.4726615109851249885 ) ) ;
#29790 = PLANE ( 'NONE',  #38306 ) ;
#29791 = CARTESIAN_POINT ( 'NONE',  ( 1.799501877760999902, -55.51082434643999619, -12.60552522433000000 ) ) ;
#29792 = CARTESIAN_POINT ( 'NONE',  ( -12.82904109066000053, -60.12452273675999947, 2.062673488410000200 ) ) ;
#29793 = CARTESIAN_POINT ( 'NONE',  ( -9.254388464354001087, -79.90752053325199711, 5.469807505829999528 ) ) ;
#29794 = EDGE_CURVE ( 'NONE', #456, #47003, #47533, .T. ) ;
#29795 = CARTESIAN_POINT ( 'NONE',  ( -2.116314338179000387, -79.81716549451699905, -9.535298106756000536 ) ) ;
#29796 = ORIENTED_EDGE ( 'NONE', *, *, #19177, .F. ) ;
#29797 = ORIENTED_EDGE ( 'NONE', *, *, #4570, .T. ) ;
#29798 = CARTESIAN_POINT ( 'NONE',  ( 0.03331989244325999494, -76.20137044996999975, 12.04427157219000044 ) ) ;
#29799 = CARTESIAN_POINT ( 'NONE',  ( -7.103738426970670261, -78.66783617555775265, -8.098733187644580056 ) ) ;
#29800 = CARTESIAN_POINT ( 'NONE',  ( -1.414324776981999987, -78.13539177200999575, 0.1417646478728999959 ) ) ;
#29801 = ORIENTED_EDGE ( 'NONE', *, *, #1146, .F. ) ;
#29802 = CARTESIAN_POINT ( 'NONE',  ( 7.765024210423000284, -17.90905971384000139, 9.830784063418001040 ) ) ;
#29803 = AXIS2_PLACEMENT_3D ( 'NONE', #17151, #47901, #17439 ) ;
#29804 = CARTESIAN_POINT ( 'NONE',  ( -1.565148314788150197, -78.73779647510495749, 9.577271978113845563 ) ) ;
#29805 = CARTESIAN_POINT ( 'NONE',  ( 14.00000000000000000, -6.100000000000000533, 0.000000000000000000 ) ) ;
#29806 = ADVANCED_FACE ( 'NONE', ( #43055 ), #43921, .T. ) ;
#29807 = CONICAL_SURFACE ( 'NONE', #37370, 11.54999999996000071, 0.7853981633972997312 ) ;
#29808 = CARTESIAN_POINT ( 'NONE',  ( -9.186177604835998878, -78.22983485330000519, -8.911975928459002105 ) ) ;
#29809 = VECTOR ( 'NONE', #32177, 1000.000000000000000 ) ;
#29810 = CARTESIAN_POINT ( 'NONE',  ( -11.19999999999999929, -74.80000000000001137, 0.000000000000000000 ) ) ;
#29811 = CARTESIAN_POINT ( 'NONE',  ( -7.000000000000000000, -80.99999999999998579, 0.000000000000000000 ) ) ;
#29812 = CARTESIAN_POINT ( 'NONE',  ( -0.3926218265389255779, -79.89583333333337123, 1.460959015002472494 ) ) ;
#29813 = CARTESIAN_POINT ( 'NONE',  ( 2.407803015296000382, -80.25912183657409571, 10.73324203768999929 ) ) ;
#29814 = EDGE_CURVE ( 'NONE', #26014, #18217, #49517, .T. ) ;
#29815 = CARTESIAN_POINT ( 'NONE',  ( 3.539309974270077319, -79.94384682290294108, 8.546032899262883120 ) ) ;
#29816 = CIRCLE ( 'NONE', #32641, 5.000000000000000888 ) ;
#29817 = VERTEX_POINT ( 'NONE', #21474 ) ;
#29818 = DIRECTION ( 'NONE',  ( 1.000000000000000000, 0.000000000000000000, 0.000000000000000000 ) ) ;
#29819 = ORIENTED_EDGE ( 'NONE', *, *, #25276, .T. ) ;
#29820 = CARTESIAN_POINT ( 'NONE',  ( 4.145744906942999464, -79.77580109776799588, -10.47576887544000002 ) ) ;
#29821 = CARTESIAN_POINT ( 'NONE',  ( 9.153609394656651688, -77.33741943966701626, -1.470339571718344285 ) ) ;
#29822 = CARTESIAN_POINT ( 'NONE',  ( -1.063776463958000074, -79.73983917928698872, 0.9372507776557998938 ) ) ;
#29823 = CARTESIAN_POINT ( 'NONE',  ( -0.6295237254636235624, -83.08333333333332860, -1.092232985442822990 ) ) ;
#29824 = CARTESIAN_POINT ( 'NONE',  ( 5.151396044562439158, -77.68693797148132774, 9.964172206255058839 ) ) ;
#29825 = CARTESIAN_POINT ( 'NONE',  ( 0.9976655664682999580, -78.41556959618471012, 1.007334501387000092 ) ) ;
#29826 = LINE ( 'NONE', #47301, #32269 ) ;
#29827 = FACE_OUTER_BOUND ( 'NONE', #16303, .T. ) ;
#29828 = CARTESIAN_POINT ( 'NONE',  ( -0.9347040216968000026, -78.75329240633999461, 1.332288049216000081 ) ) ;
#29829 = CARTESIAN_POINT ( 'NONE',  ( -12.58338334675000070, -20.25199022618999933, -1.667961445601999992 ) ) ;
#29830 = CARTESIAN_POINT ( 'NONE',  ( -5.866053559275163032, -78.43233687970867152, 10.46067059907391439 ) ) ;
#29831 = CARTESIAN_POINT ( 'NONE',  ( 10.38514225167999960, -78.21533954523499688, -3.771779243421000238 ) ) ;
#29832 = CARTESIAN_POINT ( 'NONE',  ( -9.931052045577779097, -24.12278631289421682, -7.764003813950841604 ) ) ;
#29833 = DIRECTION ( 'NONE',  ( 0.000000000000000000, 0.000000000000000000, -1.000000000000000000 ) ) ;
#29834 = CARTESIAN_POINT ( 'NONE',  ( -12.52134121561647895, -60.72745484868465127, -1.618935178750646742 ) ) ;
#29835 = EDGE_LOOP ( 'NONE', ( #29039, #29728, #40878 ) ) ;
#29836 = CARTESIAN_POINT ( 'NONE',  ( -8.985908341961819090, -77.20000000000000284, 6.204576319714215416 ) ) ;
#29837 = CARTESIAN_POINT ( 'NONE',  ( -0.8049692409160000839, -81.53111201704999189, -1.105758127848999850 ) ) ;
#29838 = CARTESIAN_POINT ( 'NONE',  ( 17.50000000000000000, -49.87071424677999687, 2.026612384852999926E-13 ) ) ;
#29839 = CARTESIAN_POINT ( 'NONE',  ( 10.42503750987000011, -77.27511107541700142, -5.902083371034000159 ) ) ;
#29840 = CARTESIAN_POINT ( 'NONE',  ( -12.70556836347999941, -16.77227722772000007, 1.774192816106000118E-09 ) ) ;
#29841 = CARTESIAN_POINT ( 'NONE',  ( -0.6572886123566999972, -82.61845057239298740, 1.530761476772000140 ) ) ;
#29842 = CARTESIAN_POINT ( 'NONE',  ( 2.685641878552820661, -1.943966194794985336, -2.278905777910877006 ) ) ;
#29843 = CARTESIAN_POINT ( 'NONE',  ( 9.345760913908002010, -78.46240584965400444, 2.683384691900000174 ) ) ;
#29844 = CARTESIAN_POINT ( 'NONE',  ( -9.171168281578999881, -77.62139044835899426, 2.561259179188999813 ) ) ;
#29845 = CARTESIAN_POINT ( 'NONE',  ( 12.00000000000000000, -23.15000000000000213, 0.8000000000000000444 ) ) ;
#29846 = CARTESIAN_POINT ( 'NONE',  ( 1.468061006981000061, -77.89085666695899590, 10.81758581523999929 ) ) ;
#29847 = CARTESIAN_POINT ( 'NONE',  ( 1.500000000000000000, -81.25000000000000000, 0.000000000000000000 ) ) ;
#29848 = LINE ( 'NONE', #4156, #43037 ) ;
#29849 = CARTESIAN_POINT ( 'NONE',  ( -0.1075386183112145844, -81.76848379990374838, -1.270412146854431379 ) ) ;
#29850 = ORIENTED_EDGE ( 'NONE', *, *, #52146, .T. ) ;
#29851 = CARTESIAN_POINT ( 'NONE',  ( -4.658475568430852753, -78.91666666666665719, 8.082524092276868188 ) ) ;
#29852 = CARTESIAN_POINT ( 'NONE',  ( -1.824767972787999959, -79.93971326159969237, -12.13485939589000040 ) ) ;
#29853 = CARTESIAN_POINT ( 'NONE',  ( -4.036611966185642331, -78.62148118236265759, -2.280826645528176488 ) ) ;
#29854 = CARTESIAN_POINT ( 'NONE',  ( -8.729704736439998669, -77.77986937598299733, 7.043462628994999974 ) ) ;
#29855 = CARTESIAN_POINT ( 'NONE',  ( 10.74341457190999982, -79.10345070876699936, -2.245675826504000216 ) ) ;
#29856 = CARTESIAN_POINT ( 'NONE',  ( -1.508277812474833501, -79.34690567646997295, 0.05089315114023049147 ) ) ;
#29857 = CARTESIAN_POINT ( 'NONE',  ( 1.318114156663148018, -17.26427522804863912, 12.70261578162694427 ) ) ;
#29858 = CARTESIAN_POINT ( 'NONE',  ( -1.250000000000000000, -80.49999999999998579, 0.000000000000000000 ) ) ;
#29859 = CARTESIAN_POINT ( 'NONE',  ( 11.24215158465786324, -78.47224147109442072, 3.414609402431842522 ) ) ;
#29860 = CARTESIAN_POINT ( 'NONE',  ( -7.610436523699135591, -60.32540704675938059, 10.41144397134750221 ) ) ;
#29861 = EDGE_LOOP ( 'NONE', ( #34521, #26572, #31870, #44040 ) ) ;
#29862 = VECTOR ( 'NONE', #42809, 1000.000000000000000 ) ;
#29863 = CARTESIAN_POINT ( 'NONE',  ( -8.917244775899000331, -78.69123101036599621, -6.494958043606000153 ) ) ;
#29864 = CARTESIAN_POINT ( 'NONE',  ( -1.050857806474344569, -80.05454060933334404, 0.6785706715357363583 ) ) ;
#29865 = CARTESIAN_POINT ( 'NONE',  ( -2.879226727952121312, -78.09583333333330302, 10.71369944335146052 ) ) ;
#29866 = CIRCLE ( 'NONE', #28899, 10.25000000000000000 ) ;
#29867 = CARTESIAN_POINT ( 'NONE',  ( 6.184832724006000149, -78.41481721455799914, -9.286519468188998871 ) ) ;
#29868 = CARTESIAN_POINT ( 'NONE',  ( 11.68767212001979594, -77.02916666666669698, -3.140974612311341563 ) ) ;
#29869 = DIRECTION ( 'NONE',  ( 1.000000000000000000, 0.000000000000000000, 0.000000000000000000 ) ) ;
#29870 = DIRECTION ( 'NONE',  ( 1.000000000000000000, -3.446666965303000135E-11, 0.000000000000000000 ) ) ;
#29871 = AXIS2_PLACEMENT_3D ( 'NONE', #28192, #10508, #14627 ) ;
#29872 = CARTESIAN_POINT ( 'NONE',  ( 0.01078207265347602868, -82.97487611262788221, -1.511023810634444020 ) ) ;
#29873 = CARTESIAN_POINT ( 'NONE',  ( -1.079840341978513862, -79.64263545050475557, -0.6301668656408577762 ) ) ;
#29874 = CARTESIAN_POINT ( 'NONE',  ( 1.799501877760999902, -23.28917565320000094, 12.60552522436000089 ) ) ;
#29875 = EDGE_CURVE ( 'NONE', #38477, #5068, #43940, .T. ) ;
#29876 = DIRECTION ( 'NONE',  ( 1.044282320439000087E-09, -1.000000000000000000, -6.141137129051000072E-09 ) ) ;
#29877 = VERTEX_POINT ( 'NONE', #12611 ) ;
#29878 = ORIENTED_EDGE ( 'NONE', *, *, #48767, .F. ) ;
#29879 = CARTESIAN_POINT ( 'NONE',  ( -12.44180763921999855, -54.70743932605000026, -1.459474665415000150 ) ) ;
#29880 = ORIENTED_EDGE ( 'NONE', *, *, #36593, .F. ) ;
#29881 = ORIENTED_EDGE ( 'NONE', *, *, #26750, .T. ) ;
#29882 = CARTESIAN_POINT ( 'NONE',  ( 10.18948929998999908, -23.21532694344000092, 7.645397820736000050 ) ) ;
#29883 = CARTESIAN_POINT ( 'NONE',  ( -0.7284109703836757488, -77.80208333347505345, -1.265496004316788214 ) ) ;
#29884 = CARTESIAN_POINT ( 'NONE',  ( -1.460959015002473382, -78.02083333333337123, -0.3926218265389205819 ) ) ;
#29885 = CARTESIAN_POINT ( 'NONE',  ( 7.184181682494999777, -78.06460333806700191, 6.343145485738000744 ) ) ;
#29886 = CARTESIAN_POINT ( 'NONE',  ( 1.694996965211734263, -76.26093750039238728, -10.68870303814569311 ) ) ;
#29887 = EDGE_CURVE ( 'NONE', #16917, #38582, #6619, .T. ) ;
#29888 = ORIENTED_EDGE ( 'NONE', *, *, #190, .T. ) ;
#29889 = ORIENTED_EDGE ( 'NONE', *, *, #45937, .T. ) ;
#29890 = CARTESIAN_POINT ( 'NONE',  ( -2.988019896091281158, -77.50128957587054401, 8.754269285533984757 ) ) ;
#29891 = CARTESIAN_POINT ( 'NONE',  ( 10.65102452230999930, -77.58073545347198774, 2.905137941168000282 ) ) ;
#29892 = VECTOR ( 'NONE', #24626, 1000.000000000000000 ) ;
#29893 = CARTESIAN_POINT ( 'NONE',  ( -12.77651047021000075, -62.10895689102999739, 0.04321256188116000263 ) ) ;
#29894 = CARTESIAN_POINT ( 'NONE',  ( 7.256139241522999939, -77.63793680681199305, 6.443535727668999513 ) ) ;
#29895 = CARTESIAN_POINT ( 'NONE',  ( 7.612971540274999782, -18.67547726287999765, 10.53003236233000095 ) ) ;
#29896 = CARTESIAN_POINT ( 'NONE',  ( 9.433548213746519195, -61.92797454583810435, 8.532643227366113692 ) ) ;
#29897 = CARTESIAN_POINT ( 'NONE',  ( -10.04116292118000153, -19.23537109840999904, 7.682344222590000271 ) ) ;
#29898 = CARTESIAN_POINT ( 'NONE',  ( 11.10498291493000167, -80.04654471278098526, -1.830582403018000015 ) ) ;
#29899 = DIRECTION ( 'NONE',  ( -1.000000000000000000, 0.000000000000000000, 0.000000000000000000 ) ) ;
#29900 = CARTESIAN_POINT ( 'NONE',  ( -0.3827951509036000011, -82.22793592742999635, -1.230253768017000038 ) ) ;
#29901 = AXIS2_PLACEMENT_3D ( 'NONE', #22561, #53863, #41149 ) ;
#29902 = AXIS2_PLACEMENT_3D ( 'NONE', #9198, #13908, #48484 ) ;
#29903 = FACE_OUTER_BOUND ( 'NONE', #33461, .T. ) ;
#29904 = CARTESIAN_POINT ( 'NONE',  ( -7.662730551410999347, -78.45333667140100431, 6.107448752912000067 ) ) ;
#29905 = CARTESIAN_POINT ( 'NONE',  ( 8.272973658470998970, -78.38734353722499293, -8.664523719228998999 ) ) ;
#29906 = EDGE_CURVE ( 'NONE', #16765, #10750, #12261, .T. ) ;
#29907 = CARTESIAN_POINT ( 'NONE',  ( -12.70228545259607955, -61.62820680317611277, 1.205254117661766600 ) ) ;
#29909 = CARTESIAN_POINT ( 'NONE',  ( -1.798368564625000054, -18.80363242954000214, -12.61278090841000044 ) ) ;
#29908 = CARTESIAN_POINT ( 'NONE',  ( 9.249548791923931645, -78.36046089431209793, 1.210758159010477009 ) ) ;
#29910 = VECTOR ( 'NONE', #51025, 1000.000000000000000 ) ;
#29911 = CARTESIAN_POINT ( 'NONE',  ( 9.500000000000000000, -79.04999999999999716, 0.000000000000000000 ) ) ;
#29912 = CARTESIAN_POINT ( 'NONE',  ( 0.7294602504688000311, -80.36286705758899984, 11.15791328003000160 ) ) ;
#29913 = CARTESIAN_POINT ( 'NONE',  ( 12.80088938722999892, -22.76256651757000071, 1.980532758767000301 ) ) ;
#29914 = CARTESIAN_POINT ( 'NONE',  ( 7.110505486850000167, -78.57249282818800395, -8.302835368086999068 ) ) ;
#29915 = CARTESIAN_POINT ( 'NONE',  ( 2.050740132903084323, -3.500000000000000444, 2.700322267406692234 ) ) ;
#29916 = CARTESIAN_POINT ( 'NONE',  ( -2.270853409273421608, -1.678612695437378122, 2.807048657911480394 ) ) ;
#29917 = ORIENTED_EDGE ( 'NONE', *, *, #35484, .F. ) ;
#29918 = CARTESIAN_POINT ( 'NONE',  ( -11.75000000000000000, -75.80000000000001137, -9.948686767780999254E-14 ) ) ;
#29919 = CYLINDRICAL_SURFACE ( 'NONE', #26671, 10.20000000000000107 ) ;
#29920 = CARTESIAN_POINT ( 'NONE',  ( -12.50000000000000000, -91.29999999999999716, -2.556024836231000547E-12 ) ) ;
#29921 = CARTESIAN_POINT ( 'NONE',  ( 0.8677903656447200076, -78.41400833188230024, 0.8997504066187256289 ) ) ;
#29922 = CARTESIAN_POINT ( 'NONE',  ( -0.9150818714851000069, -2.526649131856000263, 3.529087875733000423 ) ) ;
#29923 = CARTESIAN_POINT ( 'NONE',  ( 1.995261538442000049, -79.66278893684399520, -9.211143000868998953 ) ) ;
#29924 = CARTESIAN_POINT ( 'NONE',  ( -10.74976571963693317, -77.09494490966720548, 0.7036152397608054221 ) ) ;
#29925 = DIRECTION ( 'NONE',  ( 0.000000000000000000, 0.000000000000000000, -1.000000000000000000 ) ) ;
#29926 = CARTESIAN_POINT ( 'NONE',  ( 9.950000000000001066, -86.20000000000000284, 0.000000000000000000 ) ) ;
#29927 = CARTESIAN_POINT ( 'NONE',  ( 0.000000000000000000, -76.29999999995945359, 0.000000000000000000 ) ) ;
#29928 = CARTESIAN_POINT ( 'NONE',  ( -9.611650271896834852, -77.24166666666666003, -5.539808784079895965 ) ) ;
#29929 = CARTESIAN_POINT ( 'NONE',  ( 0.000000000000000000, 0.000000000000000000, 0.000000000000000000 ) ) ;
#29930 = CARTESIAN_POINT ( 'NONE',  ( -10.77935564133999868, -77.82479567302799239, -2.460411616693999992 ) ) ;
#29931 = CARTESIAN_POINT ( 'NONE',  ( 8.229676248979066244, -76.38669349085955673, -8.386630946024894229 ) ) ;
#29932 = CARTESIAN_POINT ( 'NONE',  ( 0.2638252682412000061, -78.33574720659700574, -11.14383981435000059 ) ) ;
#29933 = CARTESIAN_POINT ( 'NONE',  ( 1.208156862686758704, -81.87077954161354398, 0.3220240808263279964 ) ) ;
#29934 = CARTESIAN_POINT ( 'NONE',  ( 7.674627477122999863, -19.24922971947000150, 10.14950121128000049 ) ) ;
#29935 = CARTESIAN_POINT ( 'NONE',  ( -8.324924863653999196, -77.16704309767348491, 4.923709561474999497 ) ) ;
#29936 = CARTESIAN_POINT ( 'NONE',  ( 1.199500263597268246, -78.80208333333334281, 0.9218200799623752495 ) ) ;
#29937 = CARTESIAN_POINT ( 'NONE',  ( 2.661813197064093472, -3.400464207879271950, 1.930198727209918363 ) ) ;
#29938 = CARTESIAN_POINT ( 'NONE',  ( 7.235888310811381174, -80.28381975494082212, -7.950577990028921960 ) ) ;
#29939 = CARTESIAN_POINT ( 'NONE',  ( 13.94827586207000003, -45.69638659094999866, 8.082388075971999052E-06 ) ) ;
#29940 = CARTESIAN_POINT ( 'NONE',  ( -5.394504329618741600, -79.93498382078693965, -9.834680065944747085 ) ) ;
#29941 = CARTESIAN_POINT ( 'NONE',  ( -11.95950202284999975, -79.05752124800099523, 1.295167635372999948 ) ) ;
#29942 = EDGE_CURVE ( 'NONE', #39794, #18938, #44073, .T. ) ;
#29943 = CARTESIAN_POINT ( 'NONE',  ( -9.500000000000000000, -78.79999999999999716, 0.000000000000000000 ) ) ;
#29944 = CARTESIAN_POINT ( 'NONE',  ( 11.20174477810000013, -79.58164886400000171, 1.163992476170999879 ) ) ;
#29945 = AXIS2_PLACEMENT_3D ( 'NONE', #667, #51118, #23645 ) ;
#29946 = CARTESIAN_POINT ( 'NONE',  ( 1.407258332515630483, -77.46462077040253291, 10.74994165454338635 ) ) ;
#29947 = ORIENTED_EDGE ( 'NONE', *, *, #40763, .F. ) ;
#29948 = ADVANCED_FACE ( 'NONE', ( #4931 ), #42113, .T. ) ;
#29949 = CARTESIAN_POINT ( 'NONE',  ( 0.5999999999999999778, -18.84999999999000053, 11.79999999999999893 ) ) ;
#29950 = ORIENTED_EDGE ( 'NONE', *, *, #6764, .T. ) ;
#29951 = ORIENTED_EDGE ( 'NONE', *, *, #22959, .T. ) ;
#29952 = VECTOR ( 'NONE', #28568, 1000.000000000000114 ) ;
#29953 = PRESENTATION_STYLE_ASSIGNMENT (( #52703 ) ) ;
#29954 = ORIENTED_EDGE ( 'NONE', *, *, #37347, .T. ) ;
#29955 = CARTESIAN_POINT ( 'NONE',  ( 2.968874816653999993, -79.64448742432209372, 1.936686231029999927 ) ) ;
#29956 = CARTESIAN_POINT ( 'NONE',  ( 4.335582242278486653, -79.23692256116504495, 8.452722948151309978 ) ) ;
#29957 = ORIENTED_EDGE ( 'NONE', *, *, #46553, .T. ) ;
#29959 = EDGE_CURVE ( 'NONE', #50093, #53581, #32354, .T. ) ;
#29958 = CARTESIAN_POINT ( 'NONE',  ( 7.648026768024999811, -18.75000001589999954, -10.12290050218000026 ) ) ;
#29960 = EDGE_LOOP ( 'NONE', ( #4158, #4778, #25146, #44590 ) ) ;
#29961 = CARTESIAN_POINT ( 'NONE',  ( 10.36289662403999756, -60.00106470408999826, 7.633500902345000227 ) ) ;
#29962 = ORIENTED_EDGE ( 'NONE', *, *, #7171, .F. ) ;
#29963 = CARTESIAN_POINT ( 'NONE',  ( 0.7373373228469349838, -79.42494015767908877, 1.010443065347468750 ) ) ;
#29964 = FACE_OUTER_BOUND ( 'NONE', #12821, .T. ) ;
#29965 = CARTESIAN_POINT ( 'NONE',  ( -10.98384528668754712, -18.77109020607789347, 0.5959859912294981354 ) ) ;
#29966 = PRODUCT_DEFINITION_SHAPE ( 'NONE', 'NONE',  #55670 ) ;
#29967 = CARTESIAN_POINT ( 'NONE',  ( -6.634760531095161618, -80.02836359101850405, 8.459757256220747479 ) ) ;
#29968 = DIRECTION ( 'NONE',  ( -0.7071067811865475727, 0.000000000000000000, -0.7071067811865475727 ) ) ;
#29969 = CARTESIAN_POINT ( 'NONE',  ( -3.213800095599238293, -86.36264282632896538, 1.504086442990089534 ) ) ;
#29970 = CARTESIAN_POINT ( 'NONE',  ( -5.007180289739999068, -76.74583555309799010, 10.00009952528999868 ) ) ;
#29971 = CARTESIAN_POINT ( 'NONE',  ( 12.64769468388000107, -77.23434608859999173, -3.464320626314000062 ) ) ;
#29972 = CARTESIAN_POINT ( 'NONE',  ( 7.764384370167843663, -77.15074856105154311, 5.767544481182754090 ) ) ;
#29973 = CARTESIAN_POINT ( 'NONE',  ( 11.02958081164000070, -76.15094725253700858, 1.366722674935999970 ) ) ;
#29974 = CARTESIAN_POINT ( 'NONE',  ( -8.997583233551933901, -78.61904547633861284, -2.178759007882292931 ) ) ;
#29975 = CARTESIAN_POINT ( 'NONE',  ( 1.021809889922000059, -79.41634891503500171, -0.8570204080543000202 ) ) ;
#29976 = CARTESIAN_POINT ( 'NONE',  ( -10.89601512763299240, -80.11112176916604710, -1.508143038157861993 ) ) ;
#29977 = CARTESIAN_POINT ( 'NONE',  ( 1.238562849883346084, -2.945020736201496181, 3.003986674293444015 ) ) ;
#29978 = CARTESIAN_POINT ( 'NONE',  ( 0.4796867442264000081, -78.91867549782628544, -3.557196995368999914 ) ) ;
#29979 = CARTESIAN_POINT ( 'NONE',  ( -2.672184218513227627, -77.99512583853751835, 10.41389279075909791 ) ) ;
#29980 = VECTOR ( 'NONE', #21842, 1000.000000000000000 ) ;
#29981 = DIRECTION ( 'NONE',  ( 0.000000000000000000, 0.000000000000000000, -1.000000000000000000 ) ) ;
#29982 = CARTESIAN_POINT ( 'NONE',  ( -3.517187213417000358, -84.71844503318800434, -0.4592999679426000292 ) ) ;
#29983 = CARTESIAN_POINT ( 'NONE',  ( -8.333327861477410892, -76.26168058832676877, -8.283105682464439568 ) ) ;
#29984 = CARTESIAN_POINT ( 'NONE',  ( 10.18589226631999978, -18.71082276572999703, 7.641012305223999768 ) ) ;
#29985 = CARTESIAN_POINT ( 'NONE',  ( -9.770427757074999775, -61.85529868422999300, -8.292768371773000524 ) ) ;
#29986 = CARTESIAN_POINT ( 'NONE',  ( -0.7446082967701639355, -79.17994009691294366, 12.02413132939186724 ) ) ;
#29987 = CARTESIAN_POINT ( 'NONE',  ( -1.127489577578000057, -80.67343018535999022, -0.5989559841152000130 ) ) ;
#29988 = DIRECTION ( 'NONE',  ( 1.000000000000000000, 0.000000000000000000, 0.000000000000000000 ) ) ;
#29989 = CARTESIAN_POINT ( 'NONE',  ( -10.55511172854000002, -78.00228514651000467, 7.611100925114999249 ) ) ;
#29990 = EDGE_CURVE ( 'NONE', #16041, #55326, #15078, .T. ) ;
#29991 = CARTESIAN_POINT ( 'NONE',  ( 10.28103400416999946, -78.08800773578599319, 3.842432268884000024 ) ) ;
#29992 = CONICAL_SURFACE ( 'NONE', #43261, 1.203124999988000043, 0.7853981633972997312 ) ;
#29993 = CARTESIAN_POINT ( 'NONE',  ( 1.003693376009385796, -24.96223992107688971, -12.70247752664816510 ) ) ;
#29994 = CARTESIAN_POINT ( 'NONE',  ( -10.48773066565999912, -76.04028235578000761, -6.823991308961000257 ) ) ;
#29995 = ORIENTED_EDGE ( 'NONE', *, *, #38712, .F. ) ;
#29996 = CARTESIAN_POINT ( 'NONE',  ( -6.474781754604000739, -80.32627410973498172, -9.218806710208998112 ) ) ;
#29997 = DIRECTION ( 'NONE',  ( 0.000000000000000000, -1.000000000000000000, 0.000000000000000000 ) ) ;
#29998 = APPLICATION_CONTEXT ( 'automotive_design' ) ;
#29999 = CARTESIAN_POINT ( 'NONE',  ( 12.43359700621999941, -61.50705514136999597, 0.8500729763766999847 ) ) ;
#30000 = CARTESIAN_POINT ( 'NONE',  ( -11.27056218971000057, -79.04223899011000753, 6.053064779036000154 ) ) ;
#30001 = DIRECTION ( 'NONE',  ( -0.0001230612157847738313, 0.000000000000000000, 0.9999999924279686647 ) ) ;
#30002 = CARTESIAN_POINT ( 'NONE',  ( 4.996366032364999654, -78.78798106301098869, 8.105967104710000370 ) ) ;
#30003 = CARTESIAN_POINT ( 'NONE',  ( 3.807751191731999718, -82.30958586555499323, -1.403162806651999883 ) ) ;
#30004 = CARTESIAN_POINT ( 'NONE',  ( 0.9032081954762855025, -79.96855000297721006, 10.71863955025375148 ) ) ;
#30005 = CARTESIAN_POINT ( 'NONE',  ( 0.7680438806649999561, -80.32749471241899641, 1.420324776730000238 ) ) ;
#30006 = ORIENTED_EDGE ( 'NONE', *, *, #40270, .F. ) ;
#30007 = CARTESIAN_POINT ( 'NONE',  ( 10.66187250086873561, -77.33868385048562288, -1.541903100460451537 ) ) ;
#30008 = CARTESIAN_POINT ( 'NONE',  ( 1.205681127563965394, -82.11979166666397134, 0.6958864542683118604 ) ) ;
#30009 = CARTESIAN_POINT ( 'NONE',  ( 1.034427849767293406, -78.91950550033550371, -3.765568750399868492 ) ) ;
#30010 = ORIENTED_EDGE ( 'NONE', *, *, #31266, .F. ) ;
#30011 = CARTESIAN_POINT ( 'NONE',  ( -3.661365483191000081, -79.27296990877398741, 10.30932680317000028 ) ) ;
#30012 = CARTESIAN_POINT ( 'NONE',  ( 12.71798280852999952, -55.50221404479999876, 1.931086388455000025 ) ) ;
#30013 = CARTESIAN_POINT ( 'NONE',  ( 11.06914806276000185, -80.10781271246199253, -1.824675266527999939 ) ) ;
#30014 = ORIENTED_EDGE ( 'NONE', *, *, #23673, .F. ) ;
#30015 = EDGE_CURVE ( 'NONE', #28471, #14201, #10528, .T. ) ;
#30016 = CARTESIAN_POINT ( 'NONE',  ( 10.63100742340999894, -77.54925683053299679, 5.913054471243999188 ) ) ;
#30017 = EDGE_LOOP ( 'NONE', ( #45802, #4334, #3396, #11898 ) ) ;
#30018 = ORIENTED_EDGE ( 'NONE', *, *, #5513, .F. ) ;
#30019 = CIRCLE ( 'NONE', #19679, 12.50000000000000000 ) ;
#30020 = CARTESIAN_POINT ( 'NONE',  ( 0.4217350494414291440, -80.44779469249306203, 1.176759651058753242 ) ) ;
#30021 = CARTESIAN_POINT ( 'NONE',  ( 1.750000000001000089, -60.05000000958000328, 12.56594317859000043 ) ) ;
#30022 = CARTESIAN_POINT ( 'NONE',  ( 9.534323188421000239, -79.37184240488002729, -1.008198710029000189 ) ) ;
#30023 = VERTEX_POINT ( 'NONE', #36795 ) ;
#30024 = EDGE_CURVE ( 'NONE', #30255, #41507, #14354, .T. ) ;
#30025 = EDGE_LOOP ( 'NONE', ( #58052, #2617, #18228 ) ) ;
#30026 = CARTESIAN_POINT ( 'NONE',  ( 0.2017117102288683017, -79.28785263084954238, -1.258247021708098545 ) ) ;
#30027 = EDGE_CURVE ( 'NONE', #24330, #56968, #50711, .T. ) ;
#30028 = CARTESIAN_POINT ( 'NONE',  ( 1.978576907476573332, -78.77851879815550262, -3.425895241845610339 ) ) ;
#30029 = CARTESIAN_POINT ( 'NONE',  ( 9.835237363953000411, -54.71864156536999957, 7.760968332694998750 ) ) ;
#30030 = DIRECTION ( 'NONE',  ( -1.776356839400000238E-14, 1.000000000000000000, -4.909721057536999944E-14 ) ) ;
#30031 = DIRECTION ( 'NONE',  ( -0.7071067811865969777, -0.7071067811864980568, -3.873916144559985708E-09 ) ) ;
#30032 = FACE_OUTER_BOUND ( 'NONE', #52186, .T. ) ;
#30033 = CARTESIAN_POINT ( 'NONE',  ( -10.30095950721840481, -80.88213540149526182, -4.424346738711788518 ) ) ;
#30034 = CARTESIAN_POINT ( 'NONE',  ( -0.6235925192133262573, -77.75853058493544268, 1.374630246012743529 ) ) ;
#30035 = CARTESIAN_POINT ( 'NONE',  ( 9.369164850722000892, -60.04999999966999980, -7.601397897754999633 ) ) ;
#30036 = CARTESIAN_POINT ( 'NONE',  ( -10.62397638184999948, -75.99013970749000180, -6.218250916117999516 ) ) ;
#30037 = LINE ( 'NONE', #51936, #1662 ) ;
#30038 = CARTESIAN_POINT ( 'NONE',  ( -1.081559480311999888, -0.7500000000000000000, 3.328697807033000000 ) ) ;
#30039 = EDGE_CURVE ( 'NONE', #36505, #15394, #28983, .T. ) ;
#30040 = CARTESIAN_POINT ( 'NONE',  ( -12.54238283046690405, -23.52853599825456499, 1.749799162367805305 ) ) ;
#30041 = CARTESIAN_POINT ( 'NONE',  ( 2.624826629463999694, -78.80583510652000712, 11.97953966613999910 ) ) ;
#30042 = CARTESIAN_POINT ( 'NONE',  ( -8.598496321198998871, -77.06159643427999129, -8.768570137950998600 ) ) ;
#30043 = CARTESIAN_POINT ( 'NONE',  ( 9.252740428348992907, -78.67083333333332007, 2.486604901413179025 ) ) ;
#30044 = CARTESIAN_POINT ( 'NONE',  ( -4.697272406144668011, -78.45677523852745594, 11.11871297001820302 ) ) ;
#30045 = CARTESIAN_POINT ( 'NONE',  ( 1.217465845835394855, -78.72916666666665719, -0.3271848554490981997 ) ) ;
#30046 = PRODUCT_DEFINITION_FORMATION_WITH_SPECIFIED_SOURCE ( 'ANY', '', #49847, .NOT_KNOWN. ) ;
#30047 = CARTESIAN_POINT ( 'NONE',  ( -1.510136601423560432, -80.74994773521794400, -0.0005225141870202556918 ) ) ;
#30048 = CARTESIAN_POINT ( 'NONE',  ( 8.929983232555001038, -77.17945105385759064, -3.213320707285999500 ) ) ;
#30049 = FACE_OUTER_BOUND ( 'NONE', #33212, .T. ) ;
#30050 = CARTESIAN_POINT ( 'NONE',  ( -0.2809113064957999839, -2.587250604645999985, -3.546626096927000038 ) ) ;
#30051 = EDGE_CURVE ( 'NONE', #5620, #34281, #7343, .T. ) ;
#30052 = CARTESIAN_POINT ( 'NONE',  ( 11.38106369370999893, -77.71985744374799765, 4.295802577524999499 ) ) ;
#30053 = CARTESIAN_POINT ( 'NONE',  ( -9.380647509327999956, -77.74914192992498840, 2.619761060131999830 ) ) ;
#30054 = AXIS2_PLACEMENT_3D ( 'NONE', #38792, #3366, #16369 ) ;
#30056 = CARTESIAN_POINT ( 'NONE',  ( -1.232249204661999942, -77.76678331097849650, 0.4974159524616000305 ) ) ;
#30055 = CARTESIAN_POINT ( 'NONE',  ( -11.35771826322349476, -75.79999999999999716, 3.694658569866112074 ) ) ;
#30057 = CARTESIAN_POINT ( 'NONE',  ( -1.446479059201000172, -82.74025183280099327, -0.6496884318727998986 ) ) ;
#30058 = DIRECTION ( 'NONE',  ( 1.000000000000000000, 0.000000000000000000, 3.332461511940999929E-11 ) ) ;
#30059 = EDGE_LOOP ( 'NONE', ( #51553, #17689, #37371, #56989 ) ) ;
#30060 = EDGE_CURVE ( 'NONE', #525, #38648, #38291, .T. ) ;
#30061 = CARTESIAN_POINT ( 'NONE',  ( -10.21380041495000057, -19.22847221992000044, -7.668936932643000581 ) ) ;
#30062 = CARTESIAN_POINT ( 'NONE',  ( 10.38331776012999974, -79.55238262701600149, 6.321536042210999184 ) ) ;
#30063 = CARTESIAN_POINT ( 'NONE',  ( -3.879127410312085633, -79.34166267545728601, -8.706117637024775036 ) ) ;
#30064 = CARTESIAN_POINT ( 'NONE',  ( 11.44842197274081030, -79.67499999999999716, 3.717781425818833529 ) ) ;
#30065 = CARTESIAN_POINT ( 'NONE',  ( -8.669743459559573040, -76.20755208352487386, -6.663793442645963516 ) ) ;
#30066 = CARTESIAN_POINT ( 'NONE',  ( -2.599785613040999976, -0.9850476590665998566, 2.400557175927000131 ) ) ;
#30067 = CARTESIAN_POINT ( 'NONE',  ( -9.399803042841998746, -79.74562488639199387, 3.078846114291999836 ) ) ;
#30068 = LINE ( 'NONE', #52529, #22975 ) ;
#30069 = CARTESIAN_POINT ( 'NONE',  ( -9.009247259181922374, -79.02083333333334281, -2.421167930323344653 ) ) ;
#30070 = VERTEX_POINT ( 'NONE', #29958 ) ;
#30071 = DIRECTION ( 'NONE',  ( 0.000000000000000000, 1.000000000000000000, 0.000000000000000000 ) ) ;
#30072 = AXIS2_PLACEMENT_3D ( 'NONE', #35542, #31992, #13109 ) ;
#30073 = CARTESIAN_POINT ( 'NONE',  ( 6.233047529871999615, -78.88050366622999832, 9.960502923565000444 ) ) ;
#30074 = CARTESIAN_POINT ( 'NONE',  ( -8.757268953861998995, -79.72268667140099296, 4.013828826648000003 ) ) ;
#30075 = CARTESIAN_POINT ( 'NONE',  ( -10.01332844635999919, -55.51943307300000185, -7.654537085013999764 ) ) ;
#30076 = CARTESIAN_POINT ( 'NONE',  ( -0.8906226101088000613, -79.34480369890998475, -1.206976125017999779 ) ) ;
#30077 = B_SPLINE_CURVE_WITH_KNOTS ( 'NONE', 3,
 ( #6946, #7235, #25240, #43259, #38816, #56833, #16389, #52407, #49729, #18428 ),
 .UNSPECIFIED., .F., .F.,
 ( 4, 2, 2, 2, 4 ),
 ( 0.000000000000000000, 0.2500000000000000000, 0.5000000000000000000, 0.7500000000000000000, 1.000000000000000000 ),
 .UNSPECIFIED. ) ;
#30078 = VERTEX_POINT ( 'NONE', #28804 ) ;
#30079 = DIRECTION ( 'NONE',  ( 0.000000000000000000, 1.000000000000000000, 0.000000000000000000 ) ) ;
#30080 = CARTESIAN_POINT ( 'NONE',  ( -0.3279074862126110657, -82.20481765143225061, -1.218086081608457771 ) ) ;
#30081 = CYLINDRICAL_SURFACE ( 'NONE', #10133, 5.000000000000000000 ) ;
#30082 = CARTESIAN_POINT ( 'NONE',  ( -11.19999999861000006, -74.79999999860999083, -9.230037863942000436E-09 ) ) ;
#30083 = CARTESIAN_POINT ( 'NONE',  ( -9.387315177295000979, -79.68727486148499395, 2.697965643110000311 ) ) ;
#30084 = ORIENTED_EDGE ( 'NONE', *, *, #56073, .T. ) ;
#30085 = ORIENTED_EDGE ( 'NONE', *, *, #51838, .T. ) ;
#30087 = ADVANCED_FACE ( 'NONE', ( #6963 ), #20529, .T. ) ;
#30086 = CARTESIAN_POINT ( 'NONE',  ( 2.612329186234000122, -77.18495616928899494, 12.31457248274999827 ) ) ;
#30088 = CARTESIAN_POINT ( 'NONE',  ( 5.336354586632489294, -78.76643638245003842, -9.332050835440680814 ) ) ;
#30089 = PRODUCT_DEFINITION_FORMATION_WITH_SPECIFIED_SOURCE ( 'ANY', '', #25743, .NOT_KNOWN. ) ;
#30090 = CARTESIAN_POINT ( 'NONE',  ( -1.205073015186999941, -78.18782334179000770, -0.7537975966218000146 ) ) ;
#30091 = EDGE_CURVE ( 'NONE', #15955, #43107, #25257, .T. ) ;
#30092 = ORIENTED_EDGE ( 'NONE', *, *, #21561, .T. ) ;
#30093 = CARTESIAN_POINT ( 'NONE',  ( 8.979348251287998295, -77.90640194988499445, 3.086914251890999772 ) ) ;
#30094 = DIRECTION ( 'NONE',  ( -1.000000000000000000, 0.000000000000000000, 0.000000000000000000 ) ) ;
#30095 = VECTOR ( 'NONE', #8958, 1000.000000000000000 ) ;
#30096 = CARTESIAN_POINT ( 'NONE',  ( 1.980610890454014283, -55.27926110484507660, 12.74374574604364341 ) ) ;
#30097 = CARTESIAN_POINT ( 'NONE',  ( -1.184344363998000027, -77.19917510722000031, -12.90193715879000003 ) ) ;
#30098 = CARTESIAN_POINT ( 'NONE',  ( 5.413930304708984842, -79.76668259678613992, -9.393115503636845887 ) ) ;
#30099 = CARTESIAN_POINT ( 'NONE',  ( -5.747123378374999980, -78.21567021303999923, 10.24856442990000005 ) ) ;
#30100 = CARTESIAN_POINT ( 'NONE',  ( 0.000000000000000000, -0.1000000007601000024, 0.000000000000000000 ) ) ;
#30101 = CARTESIAN_POINT ( 'NONE',  ( 10.58946819037999987, -78.62494125646499299, -3.698823201301000285 ) ) ;
#30102 = CARTESIAN_POINT ( 'NONE',  ( 5.335925835648241744, -79.92656333706742089, 7.555489928919846498 ) ) ;
#30103 = ORIENTED_EDGE ( 'NONE', *, *, #57529, .F. ) ;
#30104 = CARTESIAN_POINT ( 'NONE',  ( -4.227801413918860145E-27, -6.000000000000000000, -13.89999999999999680 ) ) ;
#30105 = ORIENTED_EDGE ( 'NONE', *, *, #27194, .T. ) ;
#30106 = CARTESIAN_POINT ( 'NONE',  ( -0.5331530516160000177, -79.24204636544699554, -11.25365194899999999 ) ) ;
#30107 = CARTESIAN_POINT ( 'NONE',  ( 6.587734798705522365, -77.28814994202326716, -6.493410667348151755 ) ) ;
#30108 = CARTESIAN_POINT ( 'NONE',  ( 1.157603047269999852, -80.03175585522699009, 0.6328671228825999417 ) ) ;
#30109 = CARTESIAN_POINT ( 'NONE',  ( -1.250000000000000000, -82.99999999999998579, 0.000000000000000000 ) ) ;
#30110 = VECTOR ( 'NONE', #6868, 1000.000000000000227 ) ;
#30111 = CARTESIAN_POINT ( 'NONE',  ( 9.090775133877240677, -76.50427104666793809, 7.448072922064946866 ) ) ;
#30112 = CARTESIAN_POINT ( 'NONE',  ( 1.495190308928000089, -78.31058528507570315, 0.2516904690231000497 ) ) ;
#30113 = CARTESIAN_POINT ( 'NONE',  ( -1.249999992656000147, -76.50000000027618796, 0.4999999997238000482 ) ) ;
#30114 = VECTOR ( 'NONE', #35555, 1000.000000000000227 ) ;
#30115 = EDGE_CURVE ( 'NONE', #10285, #15955, #47720, .T. ) ;
#30116 = CARTESIAN_POINT ( 'NONE',  ( -5.413904038987206846, -80.91666666666667140, 9.393203674808249914 ) ) ;
#30117 = CARTESIAN_POINT ( 'NONE',  ( 10.99999999999999645, -78.36041666666666572, 1.439896632895345974 ) ) ;
#30118 = DIRECTION ( 'NONE',  ( -1.000000000000000000, 0.000000000000000000, 0.000000000000000000 ) ) ;
#30119 = CARTESIAN_POINT ( 'NONE',  ( 11.12554012740000076, -78.81297001833898719, 0.8449594846185999319 ) ) ;
#30120 = ADVANCED_FACE ( 'NONE', ( #56558 ), #28121, .F. ) ;
#30121 = CARTESIAN_POINT ( 'NONE',  ( 10.59548767697000038, -21.75736537952000305, -7.678667886032999768 ) ) ;
#30122 = DIRECTION ( 'NONE',  ( 0.000000000000000000, -1.000000000000000000, 0.000000000000000000 ) ) ;
#30123 = DIRECTION ( 'NONE',  ( 0.000000000000000000, -1.000000000000000000, 0.000000000000000000 ) ) ;
#30124 = CARTESIAN_POINT ( 'NONE',  ( 0.000000000000000000, -92.13603921945998820, 0.000000000000000000 ) ) ;
#30125 = ORIENTED_EDGE ( 'NONE', *, *, #21885, .T. ) ;
#30126 = CARTESIAN_POINT ( 'NONE',  ( -0.6718767921597000869, -82.73730002504399295, 1.564735933714000105 ) ) ;
#30127 = CARTESIAN_POINT ( 'NONE',  ( 1.340661125304000167, -81.17320979808999937, -0.5992281077721001159 ) ) ;
#30128 = DIRECTION ( 'NONE',  ( 0.000000000000000000, -1.000000000000000000, 0.000000000000000000 ) ) ;
#30129 = CARTESIAN_POINT ( 'NONE',  ( 0.4844284812283000119, -77.43788696795999726, 11.97002061314999999 ) ) ;
#30130 = CARTESIAN_POINT ( 'NONE',  ( -12.71536175402382973, -17.87444297184845254, 1.781227265987796571 ) ) ;
#30131 = CARTESIAN_POINT ( 'NONE',  ( -0.8762103189736000219, -81.29210705507999535, -1.416501064863000092 ) ) ;
#30132 = CARTESIAN_POINT ( 'NONE',  ( -3.708203932498999933, -76.29999999999999716, 11.41267819554000162 ) ) ;
#30133 = CARTESIAN_POINT ( 'NONE',  ( 4.316051676898999823, -78.96845194988499372, 8.712949996777000550 ) ) ;
#30134 = CARTESIAN_POINT ( 'NONE',  ( -8.420145992286000691, -77.04588578325369497, 3.744741888101000171 ) ) ;
#30135 = CARTESIAN_POINT ( 'NONE',  ( -10.30489194730139602, -76.57673360226559112, 3.128758578913356292 ) ) ;
#30136 = CARTESIAN_POINT ( 'NONE',  ( 10.86177173228253956, -75.98064620389800439, 4.480746983072430467 ) ) ;
#30137 = CARTESIAN_POINT ( 'NONE',  ( 0.4184574958520561605, -81.49815860840411119, 1.203822021099241857 ) ) ;
#30138 = ORIENTED_EDGE ( 'NONE', *, *, #45220, .F. ) ;
#30139 = EDGE_CURVE ( 'NONE', #4324, #20196, #36930, .T. ) ;
#30140 = CARTESIAN_POINT ( 'NONE',  ( 4.658475568430798575, -78.83333333333330017, 8.082524092276898386 ) ) ;
#30141 = CARTESIAN_POINT ( 'NONE',  ( 1.635689433014386296, -2.268028125413032559, -2.840897925314485928 ) ) ;
#30142 = CARTESIAN_POINT ( 'NONE',  ( 1.876038030996965977, -78.83715597219580218, -11.74176995800102574 ) ) ;
#30143 = DIRECTION ( 'NONE',  ( 0.000000000000000000, -1.000000000000000000, 0.000000000000000000 ) ) ;
#30144 = CARTESIAN_POINT ( 'NONE',  ( -0.4492251327744000156, -81.72633577836998597, 1.604198796042999753 ) ) ;
#30145 = CARTESIAN_POINT ( 'NONE',  ( 8.212410987726999068, -78.12433652412899221, -6.936771999183999782 ) ) ;
#30146 = CARTESIAN_POINT ( 'NONE',  ( 10.36222489919000012, -23.22120223852000009, -7.631889817950999522 ) ) ;
#30147 = CARTESIAN_POINT ( 'NONE',  ( 9.506651817130499893, -80.31979166666521053, 5.480266767440791220 ) ) ;
#30148 = CARTESIAN_POINT ( 'NONE',  ( 8.243508989658998587, -76.32523803030200327, 9.088020496884999133 ) ) ;
#30149 = CARTESIAN_POINT ( 'NONE',  ( -9.967566199302938301, -79.66460044437665999, 4.754512900091780736 ) ) ;
#30150 = CARTESIAN_POINT ( 'NONE',  ( -3.799999999999999822, -77.50000000000000000, 0.000000000000000000 ) ) ;
#30151 = ORIENTED_EDGE ( 'NONE', *, *, #28974, .F. ) ;
#30152 = CARTESIAN_POINT ( 'NONE',  ( 1.092964466808999946, -79.57604836483399424, 11.09324250366999998 ) ) ;
#30153 = CARTESIAN_POINT ( 'NONE',  ( 7.507395534388972891, -77.29994500668442470, 5.452647970045330972 ) ) ;
#30154 = CARTESIAN_POINT ( 'NONE',  ( 9.611650271896829523, -77.99166666666667425, 5.539808784079915505 ) ) ;
#30155 = EDGE_CURVE ( 'NONE', #21348, #27676, #49742, .T. ) ;
#30156 = CARTESIAN_POINT ( 'NONE',  ( -4.515747639259999779, -79.58700506441199707, 10.32167056182999865 ) ) ;
#30157 = CARTESIAN_POINT ( 'NONE',  ( -7.326354731301396583, -79.17057289994376390, -9.531881770301540158 ) ) ;
#30158 = CARTESIAN_POINT ( 'NONE',  ( -1.538071403320043551, -77.68541666666666856, 11.74999999999999467 ) ) ;
#30159 = DIRECTION ( 'NONE',  ( -1.000000000000000000, 0.000000000000000000, 0.000000000000000000 ) ) ;
#30160 = AXIS2_PLACEMENT_3D ( 'NONE', #47344, #6871, #29869 ) ;
#30161 = CARTESIAN_POINT ( 'NONE',  ( -0.1453150226336093476, -82.73195032484389344, 1.504369831130939472 ) ) ;
#30162 = CARTESIAN_POINT ( 'NONE',  ( -0.3119967359391886408, -79.70551649949634054, -1.210739184258169399 ) ) ;
#30163 = AXIS2_PLACEMENT_3D ( 'NONE', #9200, #30739, #4185 ) ;
#30164 = ORIENTED_EDGE ( 'NONE', *, *, #58029, .T. ) ;
#30165 = CARTESIAN_POINT ( 'NONE',  ( -1.232226824161543277, -61.32290911199032735, 12.50408896753025445 ) ) ;
#30166 = CARTESIAN_POINT ( 'NONE',  ( -10.42531125072000009, -55.53514854654000032, -7.624341767124000135 ) ) ;
#30167 = CARTESIAN_POINT ( 'NONE',  ( -12.57354097141999993, -23.72384125742000194, 1.757953070309000054 ) ) ;
#30168 = ORIENTED_EDGE ( 'NONE', *, *, #47250, .F. ) ;
#30169 = EDGE_LOOP ( 'NONE', ( #30879, #39178, #16331, #12262 ) ) ;
#30170 = CARTESIAN_POINT ( 'NONE',  ( -12.54983130235000033, -53.74901607425999828, -0.1356732392833999989 ) ) ;
#30171 = EDGE_LOOP ( 'NONE', ( #48070, #31630, #51163, #36654 ) ) ;
#30172 = CARTESIAN_POINT ( 'NONE',  ( 0.4482635754052999855, -78.67990936191000628, -12.25553529036999834 ) ) ;
#30173 = ORIENTED_EDGE ( 'NONE', *, *, #57590, .F. ) ;
#30174 = CARTESIAN_POINT ( 'NONE',  ( 1.711430185772882417, -81.00000000000000000, -10.87976356598724159 ) ) ;
#30175 = CARTESIAN_POINT ( 'NONE',  ( -0.3747936025892038003, -77.81510416683644848, -1.397875464054185501 ) ) ;
#30176 = CARTESIAN_POINT ( 'NONE',  ( 9.909302118288000116, -79.00818667140099194, 0.1618955519762999840 ) ) ;
#30177 = CARTESIAN_POINT ( 'NONE',  ( -12.50000000000000000, -60.04999999966999980, 1.250000000000000000 ) ) ;
#30178 = ORIENTED_EDGE ( 'NONE', *, *, #27932, .F. ) ;
#30179 = CONICAL_SURFACE ( 'NONE', #19843, 13.89999999994999946, 0.7853981633972997312 ) ;
#30180 = ORIENTED_EDGE ( 'NONE', *, *, #14756, .F. ) ;
#30181 = CARTESIAN_POINT ( 'NONE',  ( -5.722401730670302555, -77.52815347229775966, 7.267916609703462427 ) ) ;
#30182 = CARTESIAN_POINT ( 'NONE',  ( -10.79754810892000094, -77.38656070981998880, -2.301543980133000211 ) ) ;
#30183 = DIRECTION ( 'NONE',  ( 0.000000000000000000, -1.000000000000000000, 0.000000000000000000 ) ) ;
#30184 = CARTESIAN_POINT ( 'NONE',  ( -12.82230166705999963, -60.22260937973999972, -2.065916748305000272 ) ) ;
#30185 = CARTESIAN_POINT ( 'NONE',  ( 1.487026788147999934, -77.40709090636698875, -9.589549613196998834 ) ) ;
#30186 = CARTESIAN_POINT ( 'NONE',  ( 7.682344222590000271, -19.23537109840999904, 10.04116292118000153 ) ) ;
#30187 = ADVANCED_FACE ( 'NONE', ( #34044 ), #57255, .T. ) ;
#30188 = CARTESIAN_POINT ( 'NONE',  ( -12.70556836352000118, -62.02772277195000328, -2.424224025342999716E-09 ) ) ;
#30189 = CARTESIAN_POINT ( 'NONE',  ( 0.000000000000000000, -80.70000000003399521, -9.099999999966000175 ) ) ;
#30190 = CARTESIAN_POINT ( 'NONE',  ( -11.09141466634999951, -79.97688649776199554, 1.909950515085000022 ) ) ;
#30191 = CARTESIAN_POINT ( 'NONE',  ( 12.77301916226999978, -16.94808379552999966, -1.052060437765000023 ) ) ;
#30192 = CARTESIAN_POINT ( 'NONE',  ( 1.980532758766000212, -56.03743349309000621, 12.80088938803999810 ) ) ;
#30193 = CARTESIAN_POINT ( 'NONE',  ( -10.52337198490644710, -76.66276897022568448, 5.229864349995584583 ) ) ;
#30194 = B_SPLINE_CURVE_WITH_KNOTS ( 'NONE', 3,
 ( #5915, #1804, #46098, #5054, #45508, #50518 ),
 .UNSPECIFIED., .F., .F.,
 ( 4, 2, 4 ),
 ( 0.000000000000000000, 0.5000000000000000000, 1.000000000000000000 ),
 .UNSPECIFIED. ) ;
#30195 = EDGE_LOOP ( 'NONE', ( #54638, #55975, #19772, #56710 ) ) ;
#30196 = CARTESIAN_POINT ( 'NONE',  ( -7.633403241802001027, -55.41350283619000550, 10.18127013546999926 ) ) ;
#30197 = CARTESIAN_POINT ( 'NONE',  ( -11.48784787867999846, -78.22456764468299184, -3.397854551190000016 ) ) ;
#30198 = CARTESIAN_POINT ( 'NONE',  ( -8.958657468039000094, -16.79887336309000290, -8.950049500644999156 ) ) ;
#30199 = VECTOR ( 'NONE', #6511, 1000.000000000000000 ) ;
#30201 = CARTESIAN_POINT ( 'NONE',  ( -10.75000000000000000, -80.44999999999998863, 5.225043809877999334E-10 ) ) ;
#30200 = DIRECTION ( 'NONE',  ( 0.000000000000000000, 1.433665241479999788E-08, -0.9999999999999998890 ) ) ;
#30202 = AXIS2_PLACEMENT_3D ( 'NONE', #39522, #48973, #13232 ) ;
#30203 = CARTESIAN_POINT ( 'NONE',  ( 3.162950201720829746, -1.330633240748065660, -0.8520949969437336957 ) ) ;
#30204 = CARTESIAN_POINT ( 'NONE',  ( -10.93859554520000010, -80.49215799716398578, 0.1126871859218999961 ) ) ;
#30205 = PLANE ( 'NONE',  #14442 ) ;
#30206 = CARTESIAN_POINT ( 'NONE',  ( 3.988644160859999399, -78.54525648518600178, -10.40888963995999994 ) ) ;
#30207 = CARTESIAN_POINT ( 'NONE',  ( 12.52785920744742398, -23.79405666946011166, 1.668536824485531200 ) ) ;
#30208 = CARTESIAN_POINT ( 'NONE',  ( 5.539808784079868431, -80.03333333334234112, 9.611650271896850839 ) ) ;
#30209 = ORIENTED_EDGE ( 'NONE', *, *, #18299, .T. ) ;
#30210 = DIRECTION ( 'NONE',  ( 0.000000000000000000, 1.000000000000000000, 0.000000000000000000 ) ) ;
#30211 = EDGE_CURVE ( 'NONE', #2137, #25757, #15806, .T. ) ;
#30212 = CARTESIAN_POINT ( 'NONE',  ( -12.50728630770449001, -24.99975539312151795, 0.1757873578728431363 ) ) ;
#30213 = CARTESIAN_POINT ( 'NONE',  ( -12.49306764015999960, -23.28056535155999995, 1.667917367065999912 ) ) ;
#30214 = CARTESIAN_POINT ( 'NONE',  ( 3.801730483759000023, -3.472300407297999936, 0.1797210791774999927 ) ) ;
#30215 = CARTESIAN_POINT ( 'NONE',  ( 5.959432220885000575, -79.34133969600698322, 7.301460587826000825 ) ) ;
#30216 = CARTESIAN_POINT ( 'NONE',  ( -10.20081059776443944, -77.07411305503957522, 3.463749923433618871 ) ) ;
#30217 = CARTESIAN_POINT ( 'NONE',  ( 0.8674776458591695327, -77.23125000000000284, -10.99972142223460736 ) ) ;
#30218 = CARTESIAN_POINT ( 'NONE',  ( -1.460959015002473382, -80.02083333333335702, -0.3926218265389205819 ) ) ;
#30219 = DIRECTION ( 'NONE',  ( 0.7071067811865475727, 0.000000000000000000, 0.7071067811865475727 ) ) ;
#30220 = CARTESIAN_POINT ( 'NONE',  ( 3.835454611662000080, -84.19396544543099026, -0.9976315582358001866 ) ) ;
#30221 = DIRECTION ( 'NONE',  ( 1.000000000000000000, 0.000000000000000000, 0.000000000000000000 ) ) ;
#30222 = B_SPLINE_CURVE_WITH_KNOTS ( 'NONE', 3,
 ( #44871, #30682, #8264, #25972, #43999, #49301, #39556, #17716, #35106, #48720, #53141, #53729, #26264, #3836, #57854, #17411, #53426, #12969, #26544, #22125, #10319, #5874, #54319, #13859 ),
 .UNSPECIFIED., .F., .F.,
 ( 4, 2, 2, 2, 2, 2, 2, 2, 2, 2, 2, 4 ),
 ( 0.000000000000000000, 0.1250000000000002498, 0.2500000000000004996, 0.3750000000000007772, 0.4375000000000011657, 0.5000000000000015543, 0.6250000000000028866, 0.7500000000000043299, 0.8125000000000045519, 0.8437500000000038858, 0.8750000000000033307, 1.000000000000000000 ),
 .UNSPECIFIED. ) ;
#30223 = EDGE_CURVE ( 'NONE', #3255, #4702, #51642, .T. ) ;
#30224 = CARTESIAN_POINT ( 'NONE',  ( 5.463250847760000362, -77.20323840584198649, 9.217959235020000364 ) ) ;
#30225 = EDGE_CURVE ( 'NONE', #49519, #54390, #10185, .T. ) ;
#30226 = AXIS2_PLACEMENT_3D ( 'NONE', #15270, #2293, #10864 ) ;
#30227 = CARTESIAN_POINT ( 'NONE',  ( 10.81612714324542779, -76.41779430387406080, -4.590319906461707511 ) ) ;
#30228 = CARTESIAN_POINT ( 'NONE',  ( -10.77981876821000107, -77.12409373610799435, 2.344619735928000104 ) ) ;
#30229 = CARTESIAN_POINT ( 'NONE',  ( 0.7437748020536760762, -81.92464731248038845, 1.006161971671994060 ) ) ;
#30230 = CARTESIAN_POINT ( 'NONE',  ( 1.655661065614000060, -79.08779862992999199, 0.1622525715179000128 ) ) ;
#30231 = CARTESIAN_POINT ( 'NONE',  ( -9.429275737370000243, -77.21926183160998391, -1.157047565421999824 ) ) ;
#30232 = CARTESIAN_POINT ( 'NONE',  ( 9.009247259181925926, -78.27083333333331439, 2.421167930323317119 ) ) ;
#30233 = CARTESIAN_POINT ( 'NONE',  ( 8.796335266379966100, -77.40208333333333712, 6.760013919724084275 ) ) ;
#30234 = CARTESIAN_POINT ( 'NONE',  ( -4.104898415690168889, -80.19419946738641158, -9.935154032304627236 ) ) ;
#30235 = DIRECTION ( 'NONE',  ( 0.000000000000000000, 1.000000000000000000, 0.000000000000000000 ) ) ;
#30236 = CARTESIAN_POINT ( 'NONE',  ( -8.982242211535060861, -79.79880210577779565, 6.718700307134141347 ) ) ;
#30237 = CARTESIAN_POINT ( 'NONE',  ( -5.246265831776000255, -79.58740531167599386, -10.82514862071000117 ) ) ;
#30238 = CARTESIAN_POINT ( 'NONE',  ( -5.838193839761721016, -78.72708333333332575, 7.596835002782687418 ) ) ;
#30239 = CARTESIAN_POINT ( 'NONE',  ( -11.08513710546999853, -79.30928543398199793, 1.988391287278999942 ) ) ;
#30240 = CARTESIAN_POINT ( 'NONE',  ( -10.47050256948984526, -77.57917301698132917, 2.813946892465741367 ) ) ;
#30241 = ORIENTED_EDGE ( 'NONE', *, *, #209, .F. ) ;
#30242 = DIRECTION ( 'NONE',  ( 0.000000000000000000, -1.000000000000000000, 0.000000000000000000 ) ) ;
#30243 = AXIS2_PLACEMENT_3D ( 'NONE', #23341, #23047, #8889 ) ;
#30244 = EDGE_LOOP ( 'NONE', ( #36202, #37589, #39482 ) ) ;
#30245 = ORIENTED_EDGE ( 'NONE', *, *, #18720, .F. ) ;
#30246 = AXIS2_PLACEMENT_3D ( 'NONE', #34570, #51747, #11297 ) ;
#30247 = CARTESIAN_POINT ( 'NONE',  ( 0.000000000000000000, -5.000000000000000000, 0.000000000000000000 ) ) ;
#30248 = EDGE_LOOP ( 'NONE', ( #15339, #28077, #13555 ) ) ;
#30249 = CARTESIAN_POINT ( 'NONE',  ( -0.05248490571276999417, -80.01681542480598353, 3.589009686742000493 ) ) ;
#30250 = CARTESIAN_POINT ( 'NONE',  ( 1.480533219823060742, -79.26251219753629584, 9.383902645560738165 ) ) ;
#30251 = ORIENTED_EDGE ( 'NONE', *, *, #48146, .F. ) ;
#30252 = CARTESIAN_POINT ( 'NONE',  ( -11.47456978792000015, -79.03590068956999914, -4.589774320666000662 ) ) ;
#30253 = ORIENTED_EDGE ( 'NONE', *, *, #16713, .T. ) ;
#30254 = CARTESIAN_POINT ( 'NONE',  ( 2.421167930323352646, -79.64583333333334281, -9.009247259181915268 ) ) ;
#30255 = VERTEX_POINT ( 'NONE', #11066 ) ;
#30256 = DIRECTION ( 'NONE',  ( 0.000000000000000000, -1.000000000000000000, 0.000000000000000000 ) ) ;
#30257 = DIRECTION ( 'NONE',  ( 0.000000000000000000, -1.000000000000000000, 0.000000000000000000 ) ) ;
#30258 = CARTESIAN_POINT ( 'NONE',  ( -9.166035821854576326, -80.05650656212442584, 5.627461772928610273 ) ) ;
#30259 = LINE ( 'NONE', #16706, #41884 ) ;
#30260 = CARTESIAN_POINT ( 'NONE',  ( 2.314946975858551248, -86.25171435493599859, -3.251190558613353598 ) ) ;
#30261 = CARTESIAN_POINT ( 'NONE',  ( 5.380788203752000065, -76.16895088734899844, 9.804131929786001010 ) ) ;
#30262 = CARTESIAN_POINT ( 'NONE',  ( 12.62753648294000008, -77.73388785726000094, -3.537092078510000182 ) ) ;
#30263 = CARTESIAN_POINT ( 'NONE',  ( -0.5065304950087446967, -77.22907666195568765, 9.658864201383851267 ) ) ;
#30264 = CARTESIAN_POINT ( 'NONE',  ( 4.823055945868000016, -76.61998538877500664, -9.885342059496000644 ) ) ;
#30265 = CARTESIAN_POINT ( 'NONE',  ( -8.627689810547352067, -78.62938668033045531, -3.338956675450427181 ) ) ;
#30266 = AXIS2_PLACEMENT_3D ( 'NONE', #24081, #46840, #51840 ) ;
#30267 = CARTESIAN_POINT ( 'NONE',  ( -3.553512937130000271, -80.61420806598900413, -1.754575727644000160 ) ) ;
#30268 = FACE_OUTER_BOUND ( 'NONE', #11824, .T. ) ;
#30269 = CARTESIAN_POINT ( 'NONE',  ( 1.233621921305137370, -2.945159437469935693, 3.006013160803045814 ) ) ;
#30270 = CARTESIAN_POINT ( 'NONE',  ( 0.5655101697426998530, -82.05675264934798463, -3.499301708937000210 ) ) ;
#30271 = B_SPLINE_CURVE_WITH_KNOTS ( 'NONE', 3,
 ( #27659, #50128, #45996, #18823, #9381, #1125 ),
 .UNSPECIFIED., .F., .F.,
 ( 4, 1, 1, 4 ),
 ( 0.000000000000000000, 0.3333333333333000081, 0.6666666666667000474, 1.000000000000000000 ),
 .UNSPECIFIED. ) ;
#30272 = DIRECTION ( 'NONE',  ( 0.000000000000000000, -1.000000000000000000, 0.000000000000000000 ) ) ;
#30273 = CARTESIAN_POINT ( 'NONE',  ( 2.588229337315999690, -84.11719503318798274, 2.425413624993999928 ) ) ;
#30274 = CARTESIAN_POINT ( 'NONE',  ( -1.209804193477999945, -2.347258720801999932, -3.608664049297999998 ) ) ;
#30275 = CARTESIAN_POINT ( 'NONE',  ( -1.203848874799230195, -80.72378167735320176, 0.4182774650447538822 ) ) ;
#30276 = CARTESIAN_POINT ( 'NONE',  ( -7.601397897754999633, -55.55000000209000177, -10.07627163191000008 ) ) ;
#30277 = EDGE_CURVE ( 'NONE', #12545, #15664, #44683, .T. ) ;
#30278 = DIRECTION ( 'NONE',  ( -1.000000000000000000, 0.000000000000000000, 0.000000000000000000 ) ) ;
#30279 = CARTESIAN_POINT ( 'NONE',  ( 1.289124607492999841, -80.99250379629599195, 0.3416633729347999804 ) ) ;
#30280 = ADVANCED_FACE ( 'NONE', ( #46798 ), #30415, .F. ) ;
#30281 = CIRCLE ( 'NONE', #15210, 12.05000000000000071 ) ;
#30282 = CARTESIAN_POINT ( 'NONE',  ( -1.390809606518046193, -79.01333333333329279, -9.431280820568582968 ) ) ;
#30283 = CARTESIAN_POINT ( 'NONE',  ( 12.55073801092999908, -77.28072481401001426, -3.437763296274999991 ) ) ;
#30284 = AXIS2_PLACEMENT_3D ( 'NONE', #12524, #24947, #20806 ) ;
#30285 = CARTESIAN_POINT ( 'NONE',  ( 10.49999999996000000, -76.19999999995870610, 1.566655805052999811E-09 ) ) ;
#30286 = CARTESIAN_POINT ( 'NONE',  ( 1.722320549971293024, -24.23663688827699403, -12.71171904436489797 ) ) ;
#30287 = CARTESIAN_POINT ( 'NONE',  ( 4.917835995879999977, -76.82652295158999323, -11.17807926867999946 ) ) ;
#30288 = ORIENTED_EDGE ( 'NONE', *, *, #3957, .F. ) ;
#30289 = CARTESIAN_POINT ( 'NONE',  ( -9.497876546326999403, -77.25168256874098915, -0.2008509664869000122 ) ) ;
#30290 = CARTESIAN_POINT ( 'NONE',  ( -1.000000000000000000, -75.20000000000000284, 7.200000000000000178 ) ) ;
#30291 = EDGE_CURVE ( 'NONE', #3967, #13029, #48792, .T. ) ;
#30292 = CARTESIAN_POINT ( 'NONE',  ( 12.83838776462000020, -60.00596988455000513, 2.062170466182000172 ) ) ;
#30293 = CARTESIAN_POINT ( 'NONE',  ( 7.682331425195999763, -19.23513569609999863, -10.04115011120000034 ) ) ;
#30294 = CARTESIAN_POINT ( 'NONE',  ( -9.070848764158998989, -77.36923613374699471, 2.805586010018000120 ) ) ;
#30295 = CARTESIAN_POINT ( 'NONE',  ( -1.831741169393000135, -85.95233266374599168, 3.748532606556000069 ) ) ;
#30296 = CARTESIAN_POINT ( 'NONE',  ( 4.190783791506424549, -79.94328038420290738, 9.899395638210270576 ) ) ;
#30297 = CARTESIAN_POINT ( 'NONE',  ( 1.364204221418999774, -80.33325377676599999, 0.6617315995101000770 ) ) ;
#30298 = ORIENTED_EDGE ( 'NONE', *, *, #40266, .T. ) ;
#30299 = CARTESIAN_POINT ( 'NONE',  ( 0.3502547437541005948, -82.15885416666446872, 1.306565524318783700 ) ) ;
#30300 = CARTESIAN_POINT ( 'NONE',  ( -2.309105416988717074, -78.81515588160679897, -3.255121060972665514 ) ) ;
#30301 = ORIENTED_EDGE ( 'NONE', *, *, #21672, .F. ) ;
#30302 = CARTESIAN_POINT ( 'NONE',  ( 9.949629901056999515, -78.65493811345498898, 4.548920879513999260 ) ) ;
#30303 = CARTESIAN_POINT ( 'NONE',  ( 12.80896991324999945, -58.55453807205000061, 1.930989179114000143 ) ) ;
#30304 = CARTESIAN_POINT ( 'NONE',  ( -11.08184087837999954, -80.35837970449398426, 1.745757554832999991 ) ) ;
#30305 = VERTEX_POINT ( 'NONE', #54103 ) ;
#30306 =( GEOMETRIC_REPRESENTATION_CONTEXT ( 3 ) GLOBAL_UNCERTAINTY_ASSIGNED_CONTEXT ( ( #15978 ) ) GLOBAL_UNIT_ASSIGNED_CONTEXT ( ( #33736, #20468, #47644 ) ) REPRESENTATION_CONTEXT ( 'NONE', 'WORKASPACE' ) );
#30307 = CARTESIAN_POINT ( 'NONE',  ( 8.042137835475001495, -77.57638614595698812, 9.127242153301999394 ) ) ;
#30308 = ORIENTED_EDGE ( 'NONE', *, *, #14364, .T. ) ;
#30309 = EDGE_LOOP ( 'NONE', ( #18372, #55171, #48782, #12326, #57334 ) ) ;
#30310 = CARTESIAN_POINT ( 'NONE',  ( 1.222648819026868727, -80.36782262874812943, 0.2742722701991916479 ) ) ;
#30311 = CYLINDRICAL_SURFACE ( 'NONE', #28571, 1.750000000000000000 ) ;
#30312 = CARTESIAN_POINT ( 'NONE',  ( 3.985185646092895606, -1.087326648717707789, -0.5301898958182351684 ) ) ;
#30313 = ORIENTED_EDGE ( 'NONE', *, *, #17520, .F. ) ;
#30314 = CARTESIAN_POINT ( 'NONE',  ( -12.71005379439038663, -24.29489531516004064, -1.687596143068920140 ) ) ;
#30315 = ORIENTED_EDGE ( 'NONE', *, *, #54871, .F. ) ;
#30316 = CARTESIAN_POINT ( 'NONE',  ( 2.624826629463999694, -78.90783571398633001, 11.97953966613999910 ) ) ;
#30317 = CARTESIAN_POINT ( 'NONE',  ( -3.484880015263546404, -78.91452042059380290, 0.06569681124688563079 ) ) ;
#30318 = EDGE_CURVE ( 'NONE', #30070, #16697, #46801, .T. ) ;
#30319 = VECTOR ( 'NONE', #24673, 1000.000000000000000 ) ;
#30320 = CARTESIAN_POINT ( 'NONE',  ( 9.778561352688999619, -53.75143577336000078, 8.284566532368000225 ) ) ;
#30321 = B_SPLINE_CURVE_WITH_KNOTS ( 'NONE', 3,
 ( #35018, #9641, #26748, #22632, #27041, #4921, #40346, #5491, #31762, #40937, #4631, #41512, #45377, #45080, #31464, #27628, #22922, #524 ),
 .UNSPECIFIED., .F., .F.,
 ( 4, 2, 2, 2, 2, 2, 2, 2, 4 ),
 ( 0.000000000000000000, 0.1249999999999999445, 0.2499999999999998890, 0.3749999999999998335, 0.4999999999999998890, 0.6249999999999998890, 0.7500000000000000000, 0.8750000000000000000, 1.000000000000000000 ),
 .UNSPECIFIED. ) ;
#30322 = DIRECTION ( 'NONE',  ( -1.000000000000000000, 0.000000000000000000, 0.000000000000000000 ) ) ;
#30323 = CARTESIAN_POINT ( 'NONE',  ( 9.468750000004000356, -79.53124999999600675, -6.681056941828999630E-10 ) ) ;
#30324 = CARTESIAN_POINT ( 'NONE',  ( 12.71106812367828454, -61.05135172934481602, -1.717582538848928309 ) ) ;
#30325 = CARTESIAN_POINT ( 'NONE',  ( 3.925078296951999501, -78.49843697654912944, 11.31856107452000337 ) ) ;
#30326 = CARTESIAN_POINT ( 'NONE',  ( 8.555152029244165846, -78.81910539201572874, -3.517135500673375326 ) ) ;
#30327 = CARTESIAN_POINT ( 'NONE',  ( -7.961052042448998556, -24.53567435024999810, 9.783216378915000178 ) ) ;
#30328 = CARTESIAN_POINT ( 'NONE',  ( 4.049271016118000333, -82.37741931601499346, -0.2669009547921000203 ) ) ;
#30329 = CARTESIAN_POINT ( 'NONE',  ( 9.872661273383000591, -77.07106001420200414, 0.04965331886949000267 ) ) ;
#30330 = CARTESIAN_POINT ( 'NONE',  ( -12.50686498856104478, -24.30484291404696151, 1.423095204833915384 ) ) ;
#30331 = CARTESIAN_POINT ( 'NONE',  ( 7.999999997059999757, -81.20000000293998710, 1.734976716005999945E-08 ) ) ;
#30332 = CARTESIAN_POINT ( 'NONE',  ( -7.601397897754999633, -23.25000000000000000, -9.369164850722000892 ) ) ;
#30333 = CARTESIAN_POINT ( 'NONE',  ( 0.000000000000000000, -13.07071424677999971, 0.000000000000000000 ) ) ;
#30334 = DIRECTION ( 'NONE',  ( 0.000000000000000000, 1.000000000000000000, 0.000000000000000000 ) ) ;
#30335 = CARTESIAN_POINT ( 'NONE',  ( -1.250000000000000000, -78.50000000000000000, 0.000000000000000000 ) ) ;
#30337 = ADVANCED_FACE ( 'NONE', ( #27798, #41102 ), #35782, .F. ) ;
#30336 = CARTESIAN_POINT ( 'NONE',  ( -0.1549237127504899669, -80.13252592084100456, 1.540935225050198198 ) ) ;
#30338 = CARTESIAN_POINT ( 'NONE',  ( 8.932658457838000388, -77.29554552857699434, 2.869163408763999890 ) ) ;
#30339 = CARTESIAN_POINT ( 'NONE',  ( 1.136236858042999787, -78.72094128391299250, 1.147248764840999913 ) ) ;
#30340 = CARTESIAN_POINT ( 'NONE',  ( 3.113245456484129203, -78.43116804080246141, -10.55002948983070610 ) ) ;
#30341 = CARTESIAN_POINT ( 'NONE',  ( -2.042632565901000063, -3.544876866276999827, -2.913050207213999876 ) ) ;
#30342 = CARTESIAN_POINT ( 'NONE',  ( 9.596418076563999477, -77.63846949747699000, -7.476047798475000228 ) ) ;
#30343 = DIRECTION ( 'NONE',  ( -1.000000000000000000, 0.000000000000000000, 0.000000000000000000 ) ) ;
#30344 = CARTESIAN_POINT ( 'NONE',  ( 5.413904038987179312, -79.16666666666662877, -9.393203674808262349 ) ) ;
#30346 = CARTESIAN_POINT ( 'NONE',  ( -1.281518013001000211, -77.76102424663160662, -0.3132342491214999969 ) ) ;
#30345 = CARTESIAN_POINT ( 'NONE',  ( -5.376030604968692117, -75.79999999999999716, 10.62656574052478753 ) ) ;
#30347 = CARTESIAN_POINT ( 'NONE',  ( -1.368292558779000023, -82.61377592892299049, 0.5331262435804999811 ) ) ;
#30348 = CARTESIAN_POINT ( 'NONE',  ( -4.868526683403212374, -79.51253823190735659, 9.584316550000758994 ) ) ;
#30349 = ORIENTED_EDGE ( 'NONE', *, *, #46328, .T. ) ;
#30350 = CARTESIAN_POINT ( 'NONE',  ( -0.6295237254636235624, -82.08333333333332860, -1.092232985442822990 ) ) ;
#30351 = CARTESIAN_POINT ( 'NONE',  ( 4.729501432732000410, -79.84864851751980552, -10.91094243975000033 ) ) ;
#30352 = CARTESIAN_POINT ( 'NONE',  ( -9.498944747049275605, -79.25084052136060109, -0.1003342093385300032 ) ) ;
#30353 = EDGE_CURVE ( 'NONE', #15969, #16250, #46928, .T. ) ;
#30354 = CYLINDRICAL_SURFACE ( 'NONE', #38893, 11.00000000000000000 ) ;
#30355 = CYLINDRICAL_SURFACE ( 'NONE', #311, 9.199999999999999289 ) ;
#30356 = VECTOR ( 'NONE', #46502, 1000.000000000000114 ) ;
#30357 = CARTESIAN_POINT ( 'NONE',  ( -2.373463140952000394, -1.290903522605000076, -3.049005324064999911 ) ) ;
#30358 = CARTESIAN_POINT ( 'NONE',  ( 1.514375715454999938, -79.63358191161798061, 9.774571951410999660 ) ) ;
#30359 = CARTESIAN_POINT ( 'NONE',  ( 12.46083365854999769, -23.68341615479999973, -1.628972628240999976 ) ) ;
#30360 = DIRECTION ( 'NONE',  ( 1.000000000000000000, 0.000000000000000000, 0.000000000000000000 ) ) ;
#30361 = VERTEX_POINT ( 'NONE', #31933 ) ;
#30362 = CARTESIAN_POINT ( 'NONE',  ( -14.00000000000000000, -91.29999999999999716, 0.000000000000000000 ) ) ;
#30363 = CARTESIAN_POINT ( 'NONE',  ( -12.60354432324999863, -56.04899162853999428, 1.750000000000000000 ) ) ;
#30364 = PLANE ( 'NONE',  #6375 ) ;
#30365 = CARTESIAN_POINT ( 'NONE',  ( 3.621447497675000182, -78.40681307385639798, 0.000000000000000000 ) ) ;
#30366 = CARTESIAN_POINT ( 'NONE',  ( -0.5432945554243000519, -81.42511490629999571, -1.398152719143000100 ) ) ;
#30367 = CIRCLE ( 'NONE', #4939, 0.5000000000000004441 ) ;
#30368 = ORIENTED_EDGE ( 'NONE', *, *, #52639, .F. ) ;
#30369 = CARTESIAN_POINT ( 'NONE',  ( 3.535831105395000229, -77.07998060082339009, -10.52352073039000047 ) ) ;
#30370 = DIRECTION ( 'NONE',  ( 0.000000000000000000, -1.000000000000000000, 0.000000000000000000 ) ) ;
#30371 = CARTESIAN_POINT ( 'NONE',  ( -10.07979664880000037, -76.57175206120300004, 3.736335038366999761 ) ) ;
#30372 = AXIS2_PLACEMENT_3D ( 'NONE', #12665, #8525, #26518 ) ;
#30373 = PRODUCT_RELATED_PRODUCT_CATEGORY ( 'part', '', ( #40385 ) ) ;
#30374 = B_SPLINE_CURVE_WITH_KNOTS ( 'NONE', 3,
 ( #48901, #44459, #22015, #40023, #17597, #28184 ),
 .UNSPECIFIED., .F., .F.,
 ( 4, 2, 4 ),
 ( 0.000000000000000000, 0.5000000000000000000, 1.000000000000000000 ),
 .UNSPECIFIED. ) ;
#30375 = CARTESIAN_POINT ( 'NONE',  ( -12.69616050746999925, -57.04828923575999511, 1.799475304559999822 ) ) ;
#30376 = CARTESIAN_POINT ( 'NONE',  ( -8.652389292562999046, -53.53734871844999788, -9.414476472778000371 ) ) ;
#30377 = CONICAL_SURFACE ( 'NONE', #25669, 10.59999999995999964, 0.7853981633972997312 ) ;
#30378 = CARTESIAN_POINT ( 'NONE',  ( 8.249323304235000265, -79.91458346929098866, -5.229696851825000437 ) ) ;
#30379 = EDGE_LOOP ( 'NONE', ( #37823, #12196, #10527, #53326, #36075, #34457 ) ) ;
#30380 = ORIENTED_EDGE ( 'NONE', *, *, #25590, .T. ) ;
#30381 = CARTESIAN_POINT ( 'NONE',  ( -8.731271169595000714, -77.32214279640000143, -8.903971204279999441 ) ) ;
#30382 = CARTESIAN_POINT ( 'NONE',  ( -9.574728980326261407, -78.63772619795470575, -4.887204237426289843 ) ) ;
#30383 = CARTESIAN_POINT ( 'NONE',  ( 0.0005244906250799999826, -77.76837078354999733, -1.421402001996999953 ) ) ;
#30384 = ORIENTED_EDGE ( 'NONE', *, *, #1306, .T. ) ;
#30385 = DIRECTION ( 'NONE',  ( 0.9999433559010179051, 0.000000000000000000, 0.01064354214585019887 ) ) ;
#30386 = ADVANCED_FACE ( 'NONE', ( #13645 ), #31640, .F. ) ;
#30387 = CARTESIAN_POINT ( 'NONE',  ( 9.508279846913755051, -79.09345843291232825, -0.7695542747135521999 ) ) ;
#30388 = CARTESIAN_POINT ( 'NONE',  ( 11.75000000000000000, -76.05000000000001137, 0.000000000000000000 ) ) ;
#30389 = CARTESIAN_POINT ( 'NONE',  ( 12.15305909882999913, -78.48342962590999150, -3.479748152880000056 ) ) ;
#30390 = EDGE_CURVE ( 'NONE', #7685, #7374, #747, .T. ) ;
#30391 = DIRECTION ( 'NONE',  ( 0.000000000000000000, -1.000000000000000000, 0.000000000000000000 ) ) ;
#30392 = CARTESIAN_POINT ( 'NONE',  ( 13.63885489310999510, -19.21421830981000056, 7.254376133916000668 ) ) ;
#30393 = CARTESIAN_POINT ( 'NONE',  ( 3.380118192975835711, -86.40321104920799655, -1.504925579246371159 ) ) ;
#30394 = CARTESIAN_POINT ( 'NONE',  ( -0.2291600886666000092, -78.52507466545799275, -11.06898422383999936 ) ) ;
#30395 = CARTESIAN_POINT ( 'NONE',  ( 1.436206387574776588, -79.96308954466168473, 9.137514757049482128 ) ) ;
#30396 = CARTESIAN_POINT ( 'NONE',  ( 1.980584515756000030, -55.53514849873000259, -12.76303204337999908 ) ) ;
#30397 = ORIENTED_EDGE ( 'NONE', *, *, #33002, .T. ) ;
#30398 = CARTESIAN_POINT ( 'NONE',  ( -4.515747639259999779, -80.02863228676199014, 10.32167056182999865 ) ) ;
#30399 = CARTESIAN_POINT ( 'NONE',  ( 9.249995191645682624, -77.35005069067575789, 0.005711754169352296386 ) ) ;
#30400 = CARTESIAN_POINT ( 'NONE',  ( -0.8999941789210000875, -80.86439197592500250, -1.015940422307999969 ) ) ;
#30401 = FACE_OUTER_BOUND ( 'NONE', #7099, .T. ) ;
#30402 = AXIS2_PLACEMENT_3D ( 'NONE', #55850, #34544, #2706 ) ;
#30403 = CARTESIAN_POINT ( 'NONE',  ( 11.22546153480763564, -77.12033577748668733, -4.386301564758396054 ) ) ;
#30404 = CARTESIAN_POINT ( 'NONE',  ( 0.2372582530112999910, -78.40981053183779181, 1.497548220759000071 ) ) ;
#30405 = DIRECTION ( 'NONE',  ( 0.000000000000000000, -1.000000000000000000, 0.000000000000000000 ) ) ;
#30406 = CARTESIAN_POINT ( 'NONE',  ( -0.9820397338569999413, -80.70308451575900222, -0.7733679338621000099 ) ) ;
#30407 = CARTESIAN_POINT ( 'NONE',  ( -6.760013919724099374, -78.52708333333332291, 8.796335266379958995 ) ) ;
#30408 = CARTESIAN_POINT ( 'NONE',  ( -1.335477334469999862E-14, -72.70000000000000284, 0.000000000000000000 ) ) ;
#30409 = CARTESIAN_POINT ( 'NONE',  ( -4.392572548605500060, -80.45000000000000284, -9.875985572387369515 ) ) ;
#30410 = CARTESIAN_POINT ( 'NONE',  ( -3.734118835908999845, -79.45909416798998848, 10.51417881607000027 ) ) ;
#30411 = CARTESIAN_POINT ( 'NONE',  ( 10.98362417419999915, -18.84999999999999787, 0.5999999999999999778 ) ) ;
#30412 = CARTESIAN_POINT ( 'NONE',  ( -1.158404848901380957, -83.06944763503472018, 0.4695662491237505565 ) ) ;
#30413 = CARTESIAN_POINT ( 'NONE',  ( -1.151331214113000101, -81.37292597959698526, 4.010111216070000317 ) ) ;
#30414 = CONICAL_SURFACE ( 'NONE', #45534, 13.94999999994999840, 0.7853981633972997312 ) ;
#30415 = B_SPLINE_SURFACE_WITH_KNOTS ( 'NONE', 3, 3, ( 
 ( #55628, #25484, #57645, #3912, #47670, #43504, #43802, #11920, #29898, #2774, #7196, #8058, #57364, #21632, #25198, #39356, #48238, #53220, #44358 ),
 ( #26053, #21914, #3628, #47956, #20774, #13052, #16926, #35480, #48511, #57937, #52937, #57075, #21060, #38775, #44078, #34333, #7487, #34906, #21344 ),
 ( #3064, #12485, #25776, #3348, #39637, #56793, #34621, #16353, #52367, #30485, #8344, #39061, #53511, #17200, #16637, #7774, #52650, #43218, #17493 ),
 ( #35188, #12204, #30190, #12768, #30764, #48797, #26340, #39923, #5377, #8637, #50265, #58231, #40221, #45252, #31344, #32223, #27507, #45843, #26623 ) ),
 .UNSPECIFIED., .F., .F., .F.,
 ( 4, 4 ),
 ( 4, 1, 1, 1, 1, 1, 1, 1, 1, 1, 1, 1, 1, 1, 1, 1, 4 ),
 ( -0.4045438850611000059, 1.404543885061000141 ),
 ( -0.007432834721512999662, 0.01672387812341000202, 0.04088059096832000194, 0.06503730381324000775, 0.08919401665815999969, 0.1133507295031000034, 0.1375074423479999974, 0.1616641551929000054, 0.1858208680378000133, 0.2099775808827999968, 0.2341342937277000047, 0.2582910065726000126, 0.2824477194174999650, 0.3066044322623999729, 0.3307611451072999809, 0.3549178579523000199, 0.3790745707971999723 ),
 .UNSPECIFIED. ) ;
#30416 = B_SPLINE_CURVE_WITH_KNOTS ( 'NONE', 3,
 ( #54924, #10067, #28047, #46093 ),
 .UNSPECIFIED., .F., .F.,
 ( 4, 4 ),
 ( 0.000000000000000000, 1.000000000000000000 ),
 .UNSPECIFIED. ) ;
#30417 = EDGE_LOOP ( 'NONE', ( #24895, #35606, #54872, #46072 ) ) ;
#30419 = EDGE_CURVE ( 'NONE', #233, #37512, #33698, .T. ) ;
#30418 = CARTESIAN_POINT ( 'NONE',  ( 0.7473949548134999343, -82.16886708904999637, 1.530103832088000049 ) ) ;
#30420 = CARTESIAN_POINT ( 'NONE',  ( -0.7081060581029999801, -80.54161764699000514, -1.286481228505000018 ) ) ;
#30421 = CARTESIAN_POINT ( 'NONE',  ( -1.250000000000000000, -78.00000000000000000, 2.658254822585999717E-14 ) ) ;
#30422 = CARTESIAN_POINT ( 'NONE',  ( -7.615853692923001184, -78.42814171621100172, 9.247423260715999405 ) ) ;
#30423 = CARTESIAN_POINT ( 'NONE',  ( -12.70249541838816576, -17.03496187199482392, 0.9988462570818790187 ) ) ;
#30424 = CIRCLE ( 'NONE', #34213, 1.250000000000000444 ) ;
#30425 = CARTESIAN_POINT ( 'NONE',  ( 1.484562552624000054, -81.92369920617998957, -0.7558657512595999828 ) ) ;
#30426 = CARTESIAN_POINT ( 'NONE',  ( -2.513431698483562293, -2.188227315379490445, 2.466895036164149957 ) ) ;
#30427 = CARTESIAN_POINT ( 'NONE',  ( 2.210712544800999879, -79.21319805011499682, -9.468498208576999531 ) ) ;
#30428 = CARTESIAN_POINT ( 'NONE',  ( -0.005119011380322999356, -53.86186137778000216, -12.43705489340000092 ) ) ;
#30429 = CARTESIAN_POINT ( 'NONE',  ( 10.06040271365206529, -75.99314077920472243, 6.073823502367483584 ) ) ;
#30430 = VERTEX_POINT ( 'NONE', #40811 ) ;
#30431 = AXIS2_PLACEMENT_3D ( 'NONE', #15273, #50003, #36112 ) ;
#30432 = CARTESIAN_POINT ( 'NONE',  ( -7.488678058322025599, -78.62828703116568363, 9.109634963579681610 ) ) ;
#30433 = CARTESIAN_POINT ( 'NONE',  ( -0.4259899833590489737, -2.215981609665019558, -3.248268024827842826 ) ) ;
#30434 = CARTESIAN_POINT ( 'NONE',  ( 10.50046875551768366, -78.91200283610369581, -5.354272345414459622 ) ) ;
#30435 = CYLINDRICAL_SURFACE ( 'NONE', #48403, 10.75000000000000000 ) ;
#30436 = ADVANCED_FACE ( 'NONE', ( #8934 ), #58226, .F. ) ;
#30437 = CARTESIAN_POINT ( 'NONE',  ( -0.5790013745696001024, -82.92636086546200147, -1.562055304842999925 ) ) ;
#30438 = CARTESIAN_POINT ( 'NONE',  ( 9.233664981878000333, -79.66529779542098311, 5.933249305785000871 ) ) ;
#30439 = EDGE_CURVE ( 'NONE', #21876, #8361, #18676, .T. ) ;
#30440 = CARTESIAN_POINT ( 'NONE',  ( 1.103931348481366204, -17.37916251880048080, -12.50298439258972039 ) ) ;
#30441 = CARTESIAN_POINT ( 'NONE',  ( 0.4218791420769999467, -76.06884727436400340, -12.37978857546999834 ) ) ;
#30442 = FACE_OUTER_BOUND ( 'NONE', #31163, .T. ) ;
#30443 = DIRECTION ( 'NONE',  ( 1.000000000000000000, 0.000000000000000000, 0.000000000000000000 ) ) ;
#30444 = CARTESIAN_POINT ( 'NONE',  ( 9.317996701405999005, -79.41263030682299018, -6.117968457212000111 ) ) ;
#30445 = CARTESIAN_POINT ( 'NONE',  ( 1.146533421241619388, -79.88288899934906340, 0.4975437065520775248 ) ) ;
#30446 = CARTESIAN_POINT ( 'NONE',  ( -2.879226727952072018, -77.70416666666665151, -10.71369944335147295 ) ) ;
#30447 = CARTESIAN_POINT ( 'NONE',  ( 8.267239500339000458, -78.00112293168498923, -6.983083964283999912 ) ) ;
#30448 = CARTESIAN_POINT ( 'NONE',  ( -11.44417895085272008, -77.77916666666666856, 3.075537641221497420 ) ) ;
#30449 = CARTESIAN_POINT ( 'NONE',  ( 11.00000000000000000, -79.94999999999998863, 0.000000000000000000 ) ) ;
#30450 = AXIS2_PLACEMENT_3D ( 'NONE', #25633, #56940, #42503 ) ;
#30451 = CARTESIAN_POINT ( 'NONE',  ( 0.3513416744041613637, -81.99305105366586588, -1.471649999805617393 ) ) ;
#30452 = PRODUCT ( 'Push Button Case', 'Push Button Case', '', ( #28733 ) ) ;
#30453 = CARTESIAN_POINT ( 'NONE',  ( 10.03503830778000072, -79.02770829698199861, -7.077696433220999950 ) ) ;
#30454 = ORIENTED_EDGE ( 'NONE', *, *, #19768, .T. ) ;
#30455 = EDGE_CURVE ( 'NONE', #36484, #19156, #9520, .T. ) ;
#30456 = CARTESIAN_POINT ( 'NONE',  ( -1.749899258079942843, -60.18716848725600954, 12.55433901293707599 ) ) ;
#30457 = CARTESIAN_POINT ( 'NONE',  ( 2.062502994258999856, -21.75648180056000314, 12.92181194095000052 ) ) ;
#30458 = B_SPLINE_CURVE_WITH_KNOTS ( 'NONE', 3,
 ( #46906, #26447, #8170, #26172, #44470, #44191, #25593, #3737, #56901, #7877, #17609, #30592, #40034, #35012, #39169, #3174, #20878, #48623, #16458, #48062, #39464, #43613, #53045, #43323 ),
 .UNSPECIFIED., .F., .F.,
 ( 4, 2, 1, 2, 2, 2, 2, 2, 2, 2, 1, 2, 4 ),
 ( 0.000000000000000000, 0.06250000000000001388, 0.1250000000000000278, 0.1875000000000000555, 0.2500000000000000555, 0.3750000000000000000, 0.5000000000000000000, 0.6250000000000000000, 0.7500000000000000000, 0.8125000000000001110, 0.8750000000000001110, 0.9375000000000001110, 1.000000000000000000 ),
 .UNSPECIFIED. ) ;
#30459 = CIRCLE ( 'NONE', #1294, 13.94827586206999825 ) ;
#30460 = CARTESIAN_POINT ( 'NONE',  ( 7.220923959705223716, -76.12291666666662593, 9.396085398178630754 ) ) ;
#30461 = VERTEX_POINT ( 'NONE', #5093 ) ;
#30462 = ORIENTED_EDGE ( 'NONE', *, *, #26955, .F. ) ;
#30463 = FACE_OUTER_BOUND ( 'NONE', #28927, .T. ) ;
#30464 = VERTEX_POINT ( 'NONE', #4213 ) ;
#30465 = CARTESIAN_POINT ( 'NONE',  ( -8.224854987054504463, -79.70792932115747931, 4.804646458694507238 ) ) ;
#30466 = ORIENTED_EDGE ( 'NONE', *, *, #9903, .T. ) ;
#30467 = CARTESIAN_POINT ( 'NONE',  ( -1.539492778512501880, -81.00000000000001421, -10.83296861242082443 ) ) ;
#30468 = EDGE_CURVE ( 'NONE', #10884, #22005, #34717, .T. ) ;
#30469 = AXIS2_PLACEMENT_3D ( 'NONE', #39736, #49188, #22906 ) ;
#30470 = CARTESIAN_POINT ( 'NONE',  ( 6.160618408503998999, -77.90069330475100173, 9.012333039518999556 ) ) ;
#30471 = APPLICATION_PROTOCOL_DEFINITION ( 'draft international standard', 'automotive_design', 1998, #11925 ) ;
#30472 = EDGE_CURVE ( 'NONE', #27909, #33815, #30037, .T. ) ;
#30473 = CIRCLE ( 'NONE', #31438, 0.8000000000000000444 ) ;
#30474 = CARTESIAN_POINT ( 'NONE',  ( 8.072669757012000957, -78.05008667140099021, 4.870514429535999668 ) ) ;
#30475 = CARTESIAN_POINT ( 'NONE',  ( 5.622824352109999424, -79.93289032900889879, -9.705769245306999693 ) ) ;
#30476 = VERTEX_POINT ( 'NONE', #20909 ) ;
#30477 = EDGE_LOOP ( 'NONE', ( #56621, #4023, #50318, #55034 ) ) ;
#30478 = CARTESIAN_POINT ( 'NONE',  ( -7.485639807788073696, -77.55002885482164743, 5.433928319481235114 ) ) ;
#30479 = CARTESIAN_POINT ( 'NONE',  ( 10.90987126150000108, -77.13208304049749131, 1.690571823134000118 ) ) ;
#30480 = DIRECTION ( 'NONE',  ( 0.000000000000000000, 0.000000000000000000, -1.000000000000000000 ) ) ;
#30481 = CARTESIAN_POINT ( 'NONE',  ( 4.186942200393000135, -78.49065168068099752, -8.754440266352000677 ) ) ;
#30482 = CARTESIAN_POINT ( 'NONE',  ( 7.705119999407000542, -21.75171076523999858, 10.24996238026999862 ) ) ;
#30483 = CARTESIAN_POINT ( 'NONE',  ( -5.033129434213242881, -79.48027501432439124, -8.057022635265637334 ) ) ;
#30484 = CARTESIAN_POINT ( 'NONE',  ( 0.08338359222296000406, -79.34015964247998909, -1.538001148114999994 ) ) ;
#30485 = CARTESIAN_POINT ( 'NONE',  ( 10.52776997023000050, -80.20891172946198822, 3.979665013433000720 ) ) ;
#30486 = CARTESIAN_POINT ( 'NONE',  ( -7.919595949288999570, -59.94999999446000771, 8.768124086549999419 ) ) ;
#30487 = DIRECTION ( 'NONE',  ( -1.000000000000000000, 0.000000000000000000, 0.000000000000000000 ) ) ;
#30488 = CARTESIAN_POINT ( 'NONE',  ( -11.52087155025212972, -76.68407063598148454, 2.308491139881042375 ) ) ;
#30489 = EDGE_LOOP ( 'NONE', ( #12539, #30683, #28739, #14860, #5438, #32724 ) ) ;
#30490 = CARTESIAN_POINT ( 'NONE',  ( 8.112534416287001449, -79.82597756633930430, 9.112389163837999462 ) ) ;
#30491 = CARTESIAN_POINT ( 'NONE',  ( -7.658894278873999539, -55.59060682883999505, 10.01676917980999981 ) ) ;
#30492 = CARTESIAN_POINT ( 'NONE',  ( 9.789819849890999848, -78.90280053027699125, -6.904744247936999813 ) ) ;
#30493 = CARTESIAN_POINT ( 'NONE',  ( -10.00844281758000065, -18.63109810616999695, -7.647097920691000361 ) ) ;
#30495 = CARTESIAN_POINT ( 'NONE',  ( -1.056237665594999875, -16.95133986302000295, -12.77256098197999989 ) ) ;
#30494 = CARTESIAN_POINT ( 'NONE',  ( -12.76303204298000082, -60.06485150663000638, 1.980584515756000030 ) ) ;
#30496 = DIRECTION ( 'NONE',  ( -1.000000000000000000, 0.000000000000000000, 0.000000000000000000 ) ) ;
#30497 = CARTESIAN_POINT ( 'NONE',  ( -8.343537481004000611, -80.56114086983298250, 7.770819240183000076 ) ) ;
#30498 = CARTESIAN_POINT ( 'NONE',  ( -10.87500000000999911, -76.17499999999400018, 1.221063213659000093E-09 ) ) ;
#30499 = CARTESIAN_POINT ( 'NONE',  ( 11.06080859785000037, -77.08847592767999402, 2.119546583493000291 ) ) ;
#30500 = CARTESIAN_POINT ( 'NONE',  ( 3.500000000000000000, -3.500000000000000000, 1.049058100190999900E-13 ) ) ;
#30501 = CARTESIAN_POINT ( 'NONE',  ( -11.23644965357999936, -80.31873890621510270, 0.6602389571347000441 ) ) ;
#30502 = ORIENTED_EDGE ( 'NONE', *, *, #12858, .F. ) ;
#30503 = DIRECTION ( 'NONE',  ( 0.000000000000000000, -1.000000000000000000, 0.000000000000000000 ) ) ;
#30504 = AXIS2_PLACEMENT_3D ( 'NONE', #37864, #37274, #14838 ) ;
#30505 = CARTESIAN_POINT ( 'NONE',  ( -0.5045596072235000173, -53.66471086928999767, 12.66210649705999991 ) ) ;
#30506 = CARTESIAN_POINT ( 'NONE',  ( -12.92181194095000052, -21.75648180056000314, 2.062502994258999856 ) ) ;
#30507 = CARTESIAN_POINT ( 'NONE',  ( -0.5150151199216000952, -3.104341653420000124, 3.771016058666000426 ) ) ;
#30508 = CARTESIAN_POINT ( 'NONE',  ( 10.02153394804916786, -77.66944384051467409, -4.123993692972488745 ) ) ;
#30509 = CARTESIAN_POINT ( 'NONE',  ( 0.000000000000000000, -91.89999999999999147, 0.000000000000000000 ) ) ;
#30510 = CARTESIAN_POINT ( 'NONE',  ( 3.411343139177948736, -77.25000000000000000, -10.49328960906044728 ) ) ;
#30511 = DIRECTION ( 'NONE',  ( 0.7071067811865475727, 0.000000000000000000, 0.7071067811865475727 ) ) ;
#30512 = CARTESIAN_POINT ( 'NONE',  ( -8.485281374238999419, -60.04999999966999980, -8.485281374238999419 ) ) ;
#30513 = AXIS2_PLACEMENT_3D ( 'NONE', #14459, #42504, #46367 ) ;
#30514 = CARTESIAN_POINT ( 'NONE',  ( -3.905292900344000007, -86.19041401731898588, 1.102959312106999823 ) ) ;
#30515 = CARTESIAN_POINT ( 'NONE',  ( 5.539808784079907511, -77.36666666666666003, -9.611650271896827746 ) ) ;
#30516 = CARTESIAN_POINT ( 'NONE',  ( -4.229409687621918934, -76.85652762026346352, 11.31572571056822341 ) ) ;
#30517 = CARTESIAN_POINT ( 'NONE',  ( 10.77656672099982949, -76.41708097615209283, -4.682833356338025332 ) ) ;
#30518 = CARTESIAN_POINT ( 'NONE',  ( -9.992683672509999226, -78.17232914858600168, 4.939724043997999914 ) ) ;
#30519 = CARTESIAN_POINT ( 'NONE',  ( 1.096288133368404472, -81.89016418702514954, 0.6007765553674837555 ) ) ;
#30520 = CARTESIAN_POINT ( 'NONE',  ( -2.188064519153326781, -1.035140800317944532, 2.430261573971487010 ) ) ;
#30521 = CARTESIAN_POINT ( 'NONE',  ( -9.429275737370000243, -77.27956475728099406, -1.157047565421999824 ) ) ;
#30522 = CARTESIAN_POINT ( 'NONE',  ( 4.067416459488999436, -79.17074415034599610, -8.418325902196000854 ) ) ;
#30523 = DIRECTION ( 'NONE',  ( 0.000000000000000000, 0.000000000000000000, -1.000000000000000000 ) ) ;
#30524 = CARTESIAN_POINT ( 'NONE',  ( 2.099527108784107199, -80.24101286911570696, -10.54274609721885092 ) ) ;
#30525 = DIRECTION ( 'NONE',  ( 0.000000000000000000, 1.000000000000000000, 0.000000000000000000 ) ) ;
#30526 = CARTESIAN_POINT ( 'NONE',  ( -7.635939924820385194, -18.22474192285963923, -10.36595855977485137 ) ) ;
#30527 = EDGE_CURVE ( 'NONE', #57635, #42021, #16490, .T. ) ;
#30528 = CARTESIAN_POINT ( 'NONE',  ( -11.15966350340000091, -79.46787078828600670, 4.490997254915999548 ) ) ;
#30529 = CARTESIAN_POINT ( 'NONE',  ( -7.999999997059999757, -81.20000000293998710, -1.734976707327999832E-08 ) ) ;
#30530 = CARTESIAN_POINT ( 'NONE',  ( -12.50000000000000000, -23.24999999758999536, 1.750000000000000000 ) ) ;
#30531 = DIRECTION ( 'NONE',  ( 0.6562721000521710701, 0.7545243075561669510, -7.880219195195659585E-10 ) ) ;
#30532 = ORIENTED_EDGE ( 'NONE', *, *, #25893, .T. ) ;
#30533 = ORIENTED_EDGE ( 'NONE', *, *, #15522, .F. ) ;
#30534 = CARTESIAN_POINT ( 'NONE',  ( 12.50728617052612357, -17.00024476466254342, 0.1757991157707580188 ) ) ;
#30535 = ORIENTED_EDGE ( 'NONE', *, *, #41461, .F. ) ;
#30536 = FACE_OUTER_BOUND ( 'NONE', #28805, .T. ) ;
#30537 = ORIENTED_EDGE ( 'NONE', *, *, #6888, .T. ) ;
#30538 = CARTESIAN_POINT ( 'NONE',  ( -0.9409828818170595799, -79.00833332933186171, -3.278629126855026499 ) ) ;
#30539 = EDGE_CURVE ( 'NONE', #25733, #3055, #1264, .T. ) ;
#30540 = CARTESIAN_POINT ( 'NONE',  ( 6.585359383873000461, -79.24993983499498995, -8.706802385234000852 ) ) ;
#30541 = AXIS2_PLACEMENT_3D ( 'NONE', #14135, #37448, #55466 ) ;
#30542 = CARTESIAN_POINT ( 'NONE',  ( -0.3752914285551999796, -80.73831797169299307, -3.569720093411000050 ) ) ;
#30543 = CARTESIAN_POINT ( 'NONE',  ( -6.268809852910352198, -79.33229580225618349, 7.139848268590238689 ) ) ;
#30544 = ORIENTED_EDGE ( 'NONE', *, *, #2671, .F. ) ;
#30545 = CARTESIAN_POINT ( 'NONE',  ( 8.899186938125001944, -76.04999999999999716, 6.465637775217000005 ) ) ;
#30546 = CARTESIAN_POINT ( 'NONE',  ( -12.11584633110999931, -78.48982704611999850, 2.436790123298999688 ) ) ;
#30547 = ORIENTED_EDGE ( 'NONE', *, *, #50242, .F. ) ;
#30548 = VERTEX_POINT ( 'NONE', #46138 ) ;
#30549 = DIRECTION ( 'NONE',  ( 0.7071067812087692417, 2.829528277810876343E-07, -0.7071067811642691714 ) ) ;
#30550 = LINE ( 'NONE', #48582, #2008 ) ;
#30551 = CARTESIAN_POINT ( 'NONE',  ( -10.41537882044915264, -80.08004720311535607, 2.677681550047262604 ) ) ;
#30552 = FACE_OUTER_BOUND ( 'NONE', #54803, .T. ) ;
#30553 = CARTESIAN_POINT ( 'NONE',  ( -1.447626959621158838, -86.31452042059397911, -3.170659391604351285 ) ) ;
#30555 = ADVANCED_FACE ( 'NONE', ( #21195 ), #5024, .T. ) ;
#30554 = CARTESIAN_POINT ( 'NONE',  ( 2.115553404172148433, -85.88479124992733205, 2.777125045544115434 ) ) ;
#30556 = CARTESIAN_POINT ( 'NONE',  ( 12.66594527011999816, -76.73480431993999673, -3.392478259704000187 ) ) ;
#30557 = CARTESIAN_POINT ( 'NONE',  ( 6.694424008027000106, -76.41805712980000465, -9.543441777632999390 ) ) ;
#30558 = EDGE_CURVE ( 'NONE', #48463, #21680, #34616, .T. ) ;
#30559 = CARTESIAN_POINT ( 'NONE',  ( -9.806643590720000248, -76.56230274324299501, -4.722305910095999870 ) ) ;
#30560 = CARTESIAN_POINT ( 'NONE',  ( -8.768304182600733299, -78.62583989957664699, -2.946665245982536430 ) ) ;
#30561 = CARTESIAN_POINT ( 'NONE',  ( -4.052938665471999435, -78.93456160447509262, -0.7948260755284000112 ) ) ;
#30562 = CARTESIAN_POINT ( 'NONE',  ( 6.043427764450761686, -76.63333333333329733, 10.48543666025110888 ) ) ;
#30563 = CARTESIAN_POINT ( 'NONE',  ( -1.273994397749967256, -3.008312834910695788, 2.989085386252882781 ) ) ;
#30564 = CARTESIAN_POINT ( 'NONE',  ( -3.459341176421000252, -81.69600264934798872, -0.7732545034468999434 ) ) ;
#30565 = CARTESIAN_POINT ( 'NONE',  ( 1.249611939558153084, -82.85111090171837134, 0.007260609876616985064 ) ) ;
#30566 = CARTESIAN_POINT ( 'NONE',  ( 0.2670125575351000036, -82.86349735065198274, 3.534640024372999623 ) ) ;
#30567 = CARTESIAN_POINT ( 'NONE',  ( -0.4587696627765999735, -3.432718315767000039, -3.778272981138000031 ) ) ;
#30568 = CARTESIAN_POINT ( 'NONE',  ( 1.245667655356138326, -79.48345497551839856, -0.2692737754160527408 ) ) ;
#30569 = VERTEX_POINT ( 'NONE', #50348 ) ;
#30570 = CARTESIAN_POINT ( 'NONE',  ( -1.407171709420443895, -80.11458333333332860, -10.74999999999999645 ) ) ;
#30571 = PLANE ( 'NONE',  #44922 ) ;
#30572 = AXIS2_PLACEMENT_3D ( 'NONE', #24825, #25110, #43135 ) ;
#30573 = CARTESIAN_POINT ( 'NONE',  ( 1.246077061130999919, -80.94289117291501157, -0.4752592857455000264 ) ) ;
#30574 = CARTESIAN_POINT ( 'NONE',  ( -12.77297374713000089, -17.27184670111999765, -1.476174539902000094 ) ) ;
#30575 = CARTESIAN_POINT ( 'NONE',  ( -10.64207148833999916, -77.00320160920000490, 7.489034475093999887 ) ) ;
#30576 = B_SPLINE_CURVE_WITH_KNOTS ( 'NONE', 3,
 ( #57823, #48977, #3803, #4093, #21806, #12376, #53112, #26812 ),
 .UNSPECIFIED., .F., .F.,
 ( 4, 2, 2, 4 ),
 ( 0.000000000000000000, 0.5000000000000026645, 0.7500000000000013323, 1.000000000000000000 ),
 .UNSPECIFIED. ) ;
#30577 = CARTESIAN_POINT ( 'NONE',  ( 0.5951337072741887946, -79.55689260744961189, -1.420922764992056386 ) ) ;
#30578 = DIRECTION ( 'NONE',  ( -0.7071067811864980568, 1.531837635818995070E-11, 0.7071067811865969777 ) ) ;
#30579 = CARTESIAN_POINT ( 'NONE',  ( 9.424223717388999333, -76.77544674281999448, -8.000359493957999391 ) ) ;
#30580 = VERTEX_POINT ( 'NONE', #40606 ) ;
#30581 = CIRCLE ( 'NONE', #19316, 0.5000000000000004441 ) ;
#30582 = DIRECTION ( 'NONE',  ( -1.000000000000000000, 0.000000000000000000, 0.000000000000000000 ) ) ;
#30583 = DIRECTION ( 'NONE',  ( 1.894056204930980603E-11, 1.538483568841980365E-07, -0.9999999999999882316 ) ) ;
#30584 = CARTESIAN_POINT ( 'NONE',  ( -10.98675469975087182, -18.58582062461403339, -0.5398555193318074208 ) ) ;
#30585 = CARTESIAN_POINT ( 'NONE',  ( -1.667961430005999945, -20.25111654322000021, -12.58335110166999904 ) ) ;
#30586 = CARTESIAN_POINT ( 'NONE',  ( -9.212293474215000444, -77.41660918229499089, -2.808383990684999887 ) ) ;
#30587 = CARTESIAN_POINT ( 'NONE',  ( 3.685509519663000333, -82.57905554179599505, 1.956350997232000122 ) ) ;
#30588 = CARTESIAN_POINT ( 'NONE',  ( 5.777098977877974662, -79.93015161712408201, 9.071507582019696869 ) ) ;
#30589 = CARTESIAN_POINT ( 'NONE',  ( 0.3499829075702999837, -79.24753512672899092, -1.373881155581999858 ) ) ;
#30590 = ORIENTED_EDGE ( 'NONE', *, *, #22230, .F. ) ;
#30591 = CARTESIAN_POINT ( 'NONE',  ( 9.599999999916001059, -90.40000000008399184, -6.531555804621000072E-10 ) ) ;
#30592 = CARTESIAN_POINT ( 'NONE',  ( -1.255428910056382685, -78.98621335419240097, 9.244592359588491348 ) ) ;
#30593 = CARTESIAN_POINT ( 'NONE',  ( 3.485499217011999828, -78.91452042059380290, -4.268505459544351420E-16 ) ) ;
#30594 = EDGE_LOOP ( 'NONE', ( #16210, #8326, #38034, #16767, #26045 ) ) ;
#30595 = ORIENTED_EDGE ( 'NONE', *, *, #10366, .F. ) ;
#30596 = CARTESIAN_POINT ( 'NONE',  ( -9.062201444876000878, -78.82349223945099936, 6.128973919716999674 ) ) ;
#30597 = CARTESIAN_POINT ( 'NONE',  ( 12.87024489158000051, -56.01538333533000014, 2.062597265787999845 ) ) ;
#30598 = CARTESIAN_POINT ( 'NONE',  ( -4.083745399801999909, -80.14710589224999637, 10.68783448605000075 ) ) ;
#30599 = ORIENTED_EDGE ( 'NONE', *, *, #41362, .F. ) ;
#30600 = VERTEX_POINT ( 'NONE', #13728 ) ;
#30601 = ORIENTED_EDGE ( 'NONE', *, *, #10495, .F. ) ;
#30602 = EDGE_CURVE ( 'NONE', #17785, #38899, #53037, .T. ) ;
#30603 = DIRECTION ( 'NONE',  ( -1.000000000000000000, 0.000000000000000000, 0.000000000000000000 ) ) ;
#30604 = CARTESIAN_POINT ( 'NONE',  ( -9.358268528169000788, -79.77312495323751307, -2.797054701638000296 ) ) ;
#30605 = AXIS2_PLACEMENT_3D ( 'NONE', #22216, #44665, #26059 ) ;
#30606 = VERTEX_POINT ( 'NONE', #55937 ) ;
#30607 = CARTESIAN_POINT ( 'NONE',  ( 0.3926156672727783015, -81.75433307437405972, 1.500698096577291363 ) ) ;
#30608 = ORIENTED_EDGE ( 'NONE', *, *, #22891, .F. ) ;
#30609 = CARTESIAN_POINT ( 'NONE',  ( -10.61911868076999887, -78.59168781514685520, -6.134606423928000041 ) ) ;
#30610 = VECTOR ( 'NONE', #6382, 1000.000000000000000 ) ;
#30611 = CARTESIAN_POINT ( 'NONE',  ( -3.957350048490399175, -78.91452044229970397, -2.236040895654427985 ) ) ;
#30612 = CARTESIAN_POINT ( 'NONE',  ( 7.647736468613000049, -55.07704514418999509, 10.13404651203999940 ) ) ;
#30613 = CARTESIAN_POINT ( 'NONE',  ( -7.612971540274999782, -18.67547726287999765, -10.53003236233000095 ) ) ;
#30614 = DIRECTION ( 'NONE',  ( 0.7071067811865475727, 0.000000000000000000, -0.7071067811865475727 ) ) ;
#30615 = AXIS2_PLACEMENT_3D ( 'NONE', #55640, #47384, #24923 ) ;
#30616 = CARTESIAN_POINT ( 'NONE',  ( 12.70556836326691119, -62.02772277412548618, -0.2597962961632950818 ) ) ;
#30617 = ADVANCED_FACE ( 'NONE', ( #28756 ), #39857, .F. ) ;
#30618 = CARTESIAN_POINT ( 'NONE',  ( -0.03709510739890169162, -77.97269351862679798, -1.508447481417284575 ) ) ;
#30619 = DIRECTION ( 'NONE',  ( 1.000000000000000000, 0.000000000000000000, 0.000000000000000000 ) ) ;
#30620 = CARTESIAN_POINT ( 'NONE',  ( -8.541150802303999257, -25.00800189280999675, 9.205830468593999782 ) ) ;
#30621 = CARTESIAN_POINT ( 'NONE',  ( 2.571168007570000302, -82.24605496681199668, -3.286240184565999645 ) ) ;
#30622 = CARTESIAN_POINT ( 'NONE',  ( 8.835761575230000275, -77.10746001420200457, 4.404575387497999372 ) ) ;
#30623 = CARTESIAN_POINT ( 'NONE',  ( 1.249999999999999778, -83.26041666666665719, 0.1636246173744711763 ) ) ;
#30624 = CARTESIAN_POINT ( 'NONE',  ( 8.796335266379966100, -77.90208333333333712, 6.760013919724084275 ) ) ;
#30625 = DIRECTION ( 'NONE',  ( 0.000000000000000000, 1.000000000000000000, 0.000000000000000000 ) ) ;
#30626 = CARTESIAN_POINT ( 'NONE',  ( 1.178809752479577311, -80.96240752144423425, -0.6053965928639025718 ) ) ;
#30627 = DIRECTION ( 'NONE',  ( 0.000000000000000000, -1.000000000000000000, -1.480297366168000156E-13 ) ) ;
#30628 = CARTESIAN_POINT ( 'NONE',  ( -0.3271848554491046945, -80.89583333333328596, 1.217465845835393301 ) ) ;
#30629 = CARTESIAN_POINT ( 'NONE',  ( 0.4629760832825556838, -79.99908104961433253, -1.440305437130205313 ) ) ;
#30630 = CARTESIAN_POINT ( 'NONE',  ( 8.485281374238999419, -23.25000000000000000, 8.485281374238999419 ) ) ;
#30631 = CARTESIAN_POINT ( 'NONE',  ( -1.521132372192000037, -77.89406422756130155, 0.2748539626865999508 ) ) ;
#30632 = CARTESIAN_POINT ( 'NONE',  ( 0.000000000000000000, -26.30294702885999669, -12.53545825868000207 ) ) ;
#30633 = EDGE_CURVE ( 'NONE', #1462, #39052, #33180, .T. ) ;
#30634 = CARTESIAN_POINT ( 'NONE',  ( -8.689305806348999184, -77.50282292035799969, -8.513430283325000403 ) ) ;
#30635 = CARTESIAN_POINT ( 'NONE',  ( -1.980464483675000054, -58.55560170709000545, 12.85140862643000048 ) ) ;
#30637 = DIRECTION ( 'NONE',  ( 1.000000000000000000, 0.000000000000000000, 0.000000000000000000 ) ) ;
#30636 = CARTESIAN_POINT ( 'NONE',  ( 0.000000000000000000, -3.000000000000000000, 0.000000000000000000 ) ) ;
#30638 = CARTESIAN_POINT ( 'NONE',  ( -1.289397738844999974, -81.16111398138998823, -0.2928510814055000355 ) ) ;
#30639 = CARTESIAN_POINT ( 'NONE',  ( -4.456894928553262858, -79.50918558175608553, 9.783918442212431898 ) ) ;
#30640 = ORIENTED_EDGE ( 'NONE', *, *, #19222, .F. ) ;
#30641 = CARTESIAN_POINT ( 'NONE',  ( -1.333333333333333259, -83.14999999999999147, 0.000000000000000000 ) ) ;
#30642 = CARTESIAN_POINT ( 'NONE',  ( -12.00003092673000005, -79.69772460938399661, -0.9957469300414000246 ) ) ;
#30643 = CARTESIAN_POINT ( 'NONE',  ( -9.497892349503649356, -79.25146880129915417, -0.1753275914303987493 ) ) ;
#30644 = CARTESIAN_POINT ( 'NONE',  ( 11.11995425589478081, -79.68125000000000568, 4.608132131667403542 ) ) ;
#30645 = CARTESIAN_POINT ( 'NONE',  ( 8.796335266379966100, -78.90208333333333712, 6.760013919724084275 ) ) ;
#30646 = VECTOR ( 'NONE', #13270, 1000.000000000000114 ) ;
#30647 = DIRECTION ( 'NONE',  ( 0.000000000000000000, 1.000000000000000000, 0.000000000000000000 ) ) ;
#30648 = CARTESIAN_POINT ( 'NONE',  ( -0.2763518505204999864, -79.08418661348099477, 9.776846056101000215 ) ) ;
#30649 = CARTESIAN_POINT ( 'NONE',  ( 12.61271904360000029, -23.19692351046000311, -1.798332623270999964 ) ) ;
#30650 = CARTESIAN_POINT ( 'NONE',  ( 2.600000000000000089, -78.49999999999998579, 0.000000000000000000 ) ) ;
#30651 = ORIENTED_EDGE ( 'NONE', *, *, #40072, .F. ) ;
#30652 = LINE ( 'NONE', #57821, #34261 ) ;
#30653 = CARTESIAN_POINT ( 'NONE',  ( 3.082700750924999955, -79.47186001420199375, -9.022326502593001507 ) ) ;
#30654 = CARTESIAN_POINT ( 'NONE',  ( 9.722718241315000398, -18.75000000000000000, 7.954951288349001004 ) ) ;
#30655 = CARTESIAN_POINT ( 'NONE',  ( -0.7554284705563483193, -78.48333333333333428, -1.310679582531387721 ) ) ;
#30656 = CARTESIAN_POINT ( 'NONE',  ( 1.617840321509000034, -80.15798771285999180, 0.3973055507782000118 ) ) ;
#30657 = ORIENTED_EDGE ( 'NONE', *, *, #44288, .T. ) ;
#30658 = DIRECTION ( 'NONE',  ( 0.000000000000000000, 1.000000000000000000, 0.000000000000000000 ) ) ;
#30659 = CARTESIAN_POINT ( 'NONE',  ( -5.915435705384207488, -77.78186773030601842, -10.26011948101617755 ) ) ;
#30660 = DIRECTION ( 'NONE',  ( -0.7071067811865473507, -1.433670265776094594E-08, 0.7071067811865473507 ) ) ;
#30661 = ORIENTED_EDGE ( 'NONE', *, *, #22519, .F. ) ;
#30662 = CARTESIAN_POINT ( 'NONE',  ( -7.659225706216000518, -55.11732795990999989, -9.963487823480999594 ) ) ;
#30663 = EDGE_CURVE ( 'NONE', #14347, #3055, #29054, .T. ) ;
#30664 = CARTESIAN_POINT ( 'NONE',  ( 6.728605944993000243, -79.45532386283399262, -7.080011783993000130 ) ) ;
#30665 = ORIENTED_EDGE ( 'NONE', *, *, #18523, .F. ) ;
#30666 = ORIENTED_EDGE ( 'NONE', *, *, #4331, .F. ) ;
#30667 = CARTESIAN_POINT ( 'NONE',  ( -10.91969632658999956, -76.22984727436399055, -5.774793620716000220 ) ) ;
#30668 = CARTESIAN_POINT ( 'NONE',  ( 8.485281374238999419, -59.94999999967000548, 8.485281374238999419 ) ) ;
#30669 = EDGE_CURVE ( 'NONE', #40915, #20424, #42647, .T. ) ;
#30670 = CARTESIAN_POINT ( 'NONE',  ( 1.076318381221999854, -78.44998119068999642, 0.9284129100290999803 ) ) ;
#30671 = EDGE_LOOP ( 'NONE', ( #25315, #44236, #33045, #15931 ) ) ;
#30672 = CARTESIAN_POINT ( 'NONE',  ( 5.102724688570000389, -78.01904751632000057, 7.811319209985999379 ) ) ;
#30673 = CARTESIAN_POINT ( 'NONE',  ( -7.203509393524943683, -78.90833944987893744, -6.502559514027580256 ) ) ;
#30674 = CARTESIAN_POINT ( 'NONE',  ( 11.89999999977000122, -23.15000000000000213, 0.000000000000000000 ) ) ;
#30675 = CARTESIAN_POINT ( 'NONE',  ( -9.194628130165000357, -77.14367046626000501, -9.128060447331000304 ) ) ;
#30676 = FACE_OUTER_BOUND ( 'NONE', #50980, .T. ) ;
#30677 = CARTESIAN_POINT ( 'NONE',  ( 1.387607402548411528, -86.31452042059399332, 3.197381817703935702 ) ) ;
#30678 = CARTESIAN_POINT ( 'NONE',  ( -7.624341764926000131, -23.26485149464000202, 10.42531124853000080 ) ) ;
#30679 = VECTOR ( 'NONE', #16217, 1000.000000000000114 ) ;
#30680 = CARTESIAN_POINT ( 'NONE',  ( 3.538814480809993945, -79.94385127736886432, 8.546238217284953365 ) ) ;
#30681 = EDGE_CURVE ( 'NONE', #26523, #30955, #2214, .T. ) ;
#30682 = CARTESIAN_POINT ( 'NONE',  ( 7.610436392416016105, -18.47459049295285993, 10.41144384038989656 ) ) ;
#30683 = ORIENTED_EDGE ( 'NONE', *, *, #52060, .T. ) ;
#30684 = CARTESIAN_POINT ( 'NONE',  ( 0.2682802194768000303, -79.74770874343499827, -11.26307951182000089 ) ) ;
#30685 = FACE_OUTER_BOUND ( 'NONE', #7538, .T. ) ;
#30686 = CARTESIAN_POINT ( 'NONE',  ( -1.410851365044999861, -79.78945180266799753, 0.1398492253880000147 ) ) ;
#30687 = CARTESIAN_POINT ( 'NONE',  ( -12.65375411752000012, -20.25022861081000158, -1.750000000000000000 ) ) ;
#30688 = CIRCLE ( 'NONE', #36489, 0.8000000000000011546 ) ;
#30689 = CARTESIAN_POINT ( 'NONE',  ( 1.733997378035627035, -60.32383216727249930, -12.54437956615601202 ) ) ;
#30690 = DIRECTION ( 'NONE',  ( 1.000000000000000000, 0.000000000000000000, 0.000000000000000000 ) ) ;
#30691 = CARTESIAN_POINT ( 'NONE',  ( 12.80896991324000034, -21.75453807238000081, 1.930989179114000143 ) ) ;
#30692 = CARTESIAN_POINT ( 'NONE',  ( -5.917523019358107206, -76.71666666666662593, 10.26699006316250795 ) ) ;
#30693 = FACE_OUTER_BOUND ( 'NONE', #459, .T. ) ;
#30694 = DIRECTION ( 'NONE',  ( -1.000000000000000000, 0.000000000000000000, 0.000000000000000000 ) ) ;
#30695 = CARTESIAN_POINT ( 'NONE',  ( 0.9241086513771999966, -78.92533943566898813, 11.11924560648999893 ) ) ;
#30696 = AXIS2_PLACEMENT_3D ( 'NONE', #50621, #28738, #41749 ) ;
#30697 = CARTESIAN_POINT ( 'NONE',  ( 10.38645071867999903, -22.77819125662999866, -7.655542440070999710 ) ) ;
#30698 = CARTESIAN_POINT ( 'NONE',  ( -1.168994172860275071, -83.07126995735822561, 0.4429671410178434576 ) ) ;
#30699 = CARTESIAN_POINT ( 'NONE',  ( -7.342331066867000544, -55.64999999967000122, -8.190859204290999784 ) ) ;
#30700 = ORIENTED_EDGE ( 'NONE', *, *, #22178, .F. ) ;
#30701 = CARTESIAN_POINT ( 'NONE',  ( -0.8340143124269999708, -81.47427319649999333, -1.348286063383000055 ) ) ;
#30702 = CARTESIAN_POINT ( 'NONE',  ( 0.5128916439544000117, -81.11005058297999426, -1.376005298375999830 ) ) ;
#30703 = CARTESIAN_POINT ( 'NONE',  ( -13.99999999996999911, -5.900000000026950353, 3.874891027003000340E-10 ) ) ;
#30704 = CARTESIAN_POINT ( 'NONE',  ( 10.99419336675999936, -78.78082281672000420, 4.758540471090999979 ) ) ;
#30705 = CARTESIAN_POINT ( 'NONE',  ( 4.470112180701956817, -77.00000000000000000, 8.126903283748925233 ) ) ;
#30706 = CARTESIAN_POINT ( 'NONE',  ( -1.588687380433000174, -83.24609983225398935, 0.5002921117598999601 ) ) ;
#30707 = CARTESIAN_POINT ( 'NONE',  ( 0.000000000000000000, -79.50000000000000000, 0.000000000000000000 ) ) ;
#30708 = CARTESIAN_POINT ( 'NONE',  ( 7.048436826466999428, -77.99787251632000107, 6.223291978577000449 ) ) ;
#30709 = CARTESIAN_POINT ( 'NONE',  ( -0.005928781627726999008, -53.59886949703999903, -12.66336824414000084 ) ) ;
#30710 = CARTESIAN_POINT ( 'NONE',  ( 10.48543666025110710, -78.50833333333332575, -6.043427764450776785 ) ) ;
#30711 = DIRECTION ( 'NONE',  ( 0.000000000000000000, 1.000000000000000000, 0.000000000000000000 ) ) ;
#30712 = ORIENTED_EDGE ( 'NONE', *, *, #19022, .T. ) ;
#30713 = CARTESIAN_POINT ( 'NONE',  ( -0.1834469635243000107, -79.61327907013999550, -1.236465612773999911 ) ) ;
#30714 = CARTESIAN_POINT ( 'NONE',  ( 2.599382155498818570, -2.299256034861846043, -1.997070427629134448 ) ) ;
#30715 = CARTESIAN_POINT ( 'NONE',  ( -0.01679078366784302057, -78.82468149487773701, -11.88860714937941054 ) ) ;
#30716 = CARTESIAN_POINT ( 'NONE',  ( -3.913805347717917105, -78.48547955770028750, 0.07378289354579982418 ) ) ;
#30717 = CARTESIAN_POINT ( 'NONE',  ( -1.462746796095000024, -81.28816416383999410, -0.3322225316158000097 ) ) ;
#30718 = CARTESIAN_POINT ( 'NONE',  ( -10.58728162385000005, -77.80710571898499950, 3.705074683290000337 ) ) ;
#30719 = CARTESIAN_POINT ( 'NONE',  ( -4.985523414424999800, -78.51762948478699400, -9.777963635945001286 ) ) ;
#30720 = CARTESIAN_POINT ( 'NONE',  ( 1.811016405462505530, -17.93826444626764172, 12.71771640064008579 ) ) ;
#30721 = CARTESIAN_POINT ( 'NONE',  ( 6.695644564036999924, -77.11278636746699533, -10.05404869174999938 ) ) ;
#30722 = CARTESIAN_POINT ( 'NONE',  ( -3.845786535788662253, -78.59967399330191995, 11.15268554086950559 ) ) ;
#30723 = CARTESIAN_POINT ( 'NONE',  ( 10.07627163191000008, -60.04999999657000131, -7.601397897754999633 ) ) ;
#30724 = ORIENTED_EDGE ( 'NONE', *, *, #55841, .T. ) ;
#30725 = ADVANCED_FACE ( 'NONE', ( #38782 ), #30891, .F. ) ;
#30726 = CARTESIAN_POINT ( 'NONE',  ( 8.503062319121001522, -78.44610392334999460, 7.028489548493999983 ) ) ;
#30727 = CARTESIAN_POINT ( 'NONE',  ( 0.4578503181340247696, -79.94544045178886904, 1.162965988986303767 ) ) ;
#30728 = CARTESIAN_POINT ( 'NONE',  ( 3.679515170149685765, -75.79999999999999716, -11.28544018175951358 ) ) ;
#30729 = B_SPLINE_CURVE_WITH_KNOTS ( 'NONE', 3,
 ( #12532, #20533, #16683, #34379, #48562, #38531, #52124, #24955, #25530, #34665, #7531, #44126, #30238, #8106, #16392, #12814, #52410, #29943 ),
 .UNSPECIFIED., .F., .F.,
 ( 4, 2, 2, 2, 2, 2, 2, 2, 4 ),
 ( 0.000000000000000000, 0.1250000000000000278, 0.2500000000000000555, 0.3750000000000001110, 0.5000000000000001110, 0.6250000000000001110, 0.7500000000000002220, 0.8750000000000001110, 1.000000000000000000 ),
 .UNSPECIFIED. ) ;
#30730 = CARTESIAN_POINT ( 'NONE',  ( -9.595360835209000072, -79.28568019887099183, -5.693913425678999829 ) ) ;
#30731 = B_SPLINE_CURVE_WITH_KNOTS ( 'NONE', 3,
 ( #29603, #47659, #29886, #20192, #43206, #2765, #20763, #38186, #16343, #47944 ),
 .UNSPECIFIED., .F., .F.,
 ( 4, 2, 2, 2, 4 ),
 ( 0.6250000037914531514, 0.7187500028435899191, 0.8125000018957265757, 0.9062500009478633434, 1.000000000000000000 ),
 .UNSPECIFIED. ) ;
#30732 = CARTESIAN_POINT ( 'NONE',  ( 5.407950800604435670, -76.33333333333332860, 9.358624512123000727 ) ) ;
#30733 = CARTESIAN_POINT ( 'NONE',  ( 0.9661584243600921384, -81.66915000328793894, 1.163803266013009097 ) ) ;
#30734 = CARTESIAN_POINT ( 'NONE',  ( 12.25187917533000004, -79.08196692782999548, 0.8290103756198000662 ) ) ;
#30735 = AXIS2_PLACEMENT_3D ( 'NONE', #49035, #3010, #35729 ) ;
#30736 = EDGE_LOOP ( 'NONE', ( #44523, #14054, #12891 ) ) ;
#30737 = CARTESIAN_POINT ( 'NONE',  ( 9.102137320399311449, -17.02814024880371591, -8.583672455337429952 ) ) ;
#30738 = TOROIDAL_SURFACE ( 'NONE', #46814, 1.250000000000000000, 0.5000000000000000000 ) ;
#30739 = DIRECTION ( 'NONE',  ( 0.000000000000000000, 1.000000000000000000, 0.000000000000000000 ) ) ;
#30740 = DIRECTION ( 'NONE',  ( 0.000000000000000000, -1.000000000000000000, 0.000000000000000000 ) ) ;
#30741 = ORIENTED_EDGE ( 'NONE', *, *, #53680, .T. ) ;
#30742 = AXIS2_PLACEMENT_3D ( 'NONE', #52296, #30122, #29833 ) ;
#30743 = ORIENTED_EDGE ( 'NONE', *, *, #171, .F. ) ;
#30744 = DIRECTION ( 'NONE',  ( 0.000000000000000000, -1.000000000000000000, 0.000000000000000000 ) ) ;
#30745 = EDGE_CURVE ( 'NONE', #51037, #56909, #9335, .T. ) ;
#30746 = ORIENTED_EDGE ( 'NONE', *, *, #5812, .F. ) ;
#30747 = CYLINDRICAL_SURFACE ( 'NONE', #5667, 12.50000000000000000 ) ;
#30748 = ORIENTED_EDGE ( 'NONE', *, *, #35119, .F. ) ;
#30749 = CARTESIAN_POINT ( 'NONE',  ( 10.01749676170999948, -23.19181054693000021, 7.660430254659999605 ) ) ;
#30750 = CARTESIAN_POINT ( 'NONE',  ( 10.17013595917000046, -77.85947499715699394, -4.274350120612000481 ) ) ;
#30751 = CARTESIAN_POINT ( 'NONE',  ( -0.6447613848864999220, -78.00963998579798897, 9.665783406873000416 ) ) ;
#30752 = CARTESIAN_POINT ( 'NONE',  ( -6.180994592422803358, -78.16689241883609895, -6.883246697956296067 ) ) ;
#30753 = CARTESIAN_POINT ( 'NONE',  ( -6.324515969367999979, -78.77564805565999961, -9.263833350438000380 ) ) ;
#30754 = EDGE_CURVE ( 'NONE', #36961, #26860, #10119, .T. ) ;
#30755 = EDGE_LOOP ( 'NONE', ( #12610, #17849, #244 ) ) ;
#30756 = EDGE_LOOP ( 'NONE', ( #51441, #38836, #48138, #39980 ) ) ;
#30757 = CARTESIAN_POINT ( 'NONE',  ( -6.466212988017749019, -77.53676806074847150, 6.615100391815839309 ) ) ;
#30758 = CARTESIAN_POINT ( 'NONE',  ( -10.79754810892000094, -77.32625778414998763, -2.301543980133000211 ) ) ;
#30759 = EDGE_CURVE ( 'NONE', #8704, #7685, #49483, .T. ) ;
#30760 = CARTESIAN_POINT ( 'NONE',  ( -9.500000000000000000, -78.89999999999999147, 0.000000000000000000 ) ) ;
#30761 = CARTESIAN_POINT ( 'NONE',  ( 6.037385872459999803, -75.75138372272999732, 10.30991454870999924 ) ) ;
#30762 = CARTESIAN_POINT ( 'NONE',  ( -2.935661446561999899, -79.50000000000000000, -9.035036904803998681 ) ) ;
#30763 = CARTESIAN_POINT ( 'NONE',  ( -0.6794254437148999903, -78.80190446794000536, -1.478865823597000029 ) ) ;
#30764 = CARTESIAN_POINT ( 'NONE',  ( -7.179058446792000225, -80.06040882843898032, -8.667882172381000672 ) ) ;
#30765 = FACE_OUTER_BOUND ( 'NONE', #53883, .T. ) ;
#30766 = CARTESIAN_POINT ( 'NONE',  ( -0.7681833999686432657, -78.07291666666668561, -0.9995835529977258327 ) ) ;
#30767 = CARTESIAN_POINT ( 'NONE',  ( -11.51760730114658848, -76.68396387802945924, 2.324764085046806983 ) ) ;
#30768 = ORIENTED_EDGE ( 'NONE', *, *, #43060, .T. ) ;
#30769 = B_SPLINE_CURVE_WITH_KNOTS ( 'NONE', 3,
 ( #23475, #1073, #33193, #50656, #51239, #10202, #46821, #37926 ),
 .UNSPECIFIED., .F., .F.,
 ( 4, 2, 2, 4 ),
 ( 0.000000000000000000, 0.5000000000000026645, 0.7500000000000013323, 1.000000000000000000 ),
 .UNSPECIFIED. ) ;
#30770 = CARTESIAN_POINT ( 'NONE',  ( -6.443880121360000324, -79.99798052329479958, 9.772379853565000829 ) ) ;
#30771 = DIRECTION ( 'NONE',  ( 0.000000000000000000, -1.000000000000000000, 0.000000000000000000 ) ) ;
#30772 = CARTESIAN_POINT ( 'NONE',  ( -4.743879332790999825, -78.79428326858199227, -11.00053059214000051 ) ) ;
#30773 = CARTESIAN_POINT ( 'NONE',  ( -10.01752115541999899, -18.80828330197000042, -7.660412752602000275 ) ) ;
#30774 = AXIS2_PLACEMENT_3D ( 'NONE', #37751, #55773, #33314 ) ;
#30776 = CARTESIAN_POINT ( 'NONE',  ( 0.000000000000000000, -75.20000000000000284, -7.200000000000000178 ) ) ;
#30775 = CARTESIAN_POINT ( 'NONE',  ( 7.641012386020999969, -55.51082434643999619, 10.18589234707000202 ) ) ;
#30777 = ADVANCED_FACE ( 'NONE', ( #705 ), #18393, .F. ) ;
#30778 = CARTESIAN_POINT ( 'NONE',  ( 5.939680743703000668E-14, -6.000000000000000000, 0.000000000000000000 ) ) ;
#30779 = CARTESIAN_POINT ( 'NONE',  ( 10.01332844639000008, -60.08056692637000396, -7.654537085048000122 ) ) ;
#30780 = LINE ( 'NONE', #48814, #16936 ) ;
#30781 = CARTESIAN_POINT ( 'NONE',  ( 11.13061814830999907, -77.06123958467900081, -1.715606072514000102 ) ) ;
#30782 = DIRECTION ( 'NONE',  ( 0.7071067811705838979, 1.925102962605954398E-07, 0.7071067812024849353 ) ) ;
#30783 = CARTESIAN_POINT ( 'NONE',  ( 2.063852278220999814, -80.96308337030230007, -11.06498607923999877 ) ) ;
#30784 = VECTOR ( 'NONE', #14667, 1000.000000000000227 ) ;
#30785 = ORIENTED_EDGE ( 'NONE', *, *, #3191, .F. ) ;
#30786 = CARTESIAN_POINT ( 'NONE',  ( -1.995597954366113980, -1.528831350911639575, 2.597155843134357323 ) ) ;
#30787 = CYLINDRICAL_SURFACE ( 'NONE', #10807, 0.5999999999999999778 ) ;
#30788 = FACE_OUTER_BOUND ( 'NONE', #39467, .T. ) ;
#30789 = VECTOR ( 'NONE', #10177, 1000.000000000000114 ) ;
#30790 = CARTESIAN_POINT ( 'NONE',  ( 2.492987828166000064, -3.446546016549000058, 2.660538423215999870 ) ) ;
#30791 = FACE_OUTER_BOUND ( 'NONE', #15885, .T. ) ;
#30792 = CONICAL_SURFACE ( 'NONE', #9114, 13.94999999993999928, 0.7853981633972997312 ) ;
#30793 = FACE_OUTER_BOUND ( 'NONE', #45458, .T. ) ;
#30794 = DIRECTION ( 'NONE',  ( 0.7592504785507936393, 0.04890181649399957808, 0.6489586451877946693 ) ) ;
#30795 = CARTESIAN_POINT ( 'NONE',  ( -1.667269374592999842, -60.00939883451999890, 12.49858097732999873 ) ) ;
#30796 = CARTESIAN_POINT ( 'NONE',  ( 12.43569863939999998, -17.11799904157000185, 0.4278707626186000201 ) ) ;
#30797 = CARTESIAN_POINT ( 'NONE',  ( -3.349785279347999634, -83.03494503318799502, 2.487770294745999866 ) ) ;
#30798 = CARTESIAN_POINT ( 'NONE',  ( 0.000000000000000000, -75.00000000000000000, -7.200000000000000178 ) ) ;
#30799 = EDGE_CURVE ( 'NONE', #44267, #33739, #4812, .T. ) ;
#30800 = CARTESIAN_POINT ( 'NONE',  ( 11.73832436745839836, -77.18564631431473799, -2.604929631990708483 ) ) ;
#30801 = CARTESIAN_POINT ( 'NONE',  ( -10.79885705035999877, -76.72880296949000467, -2.763914921897999921 ) ) ;
#30802 = CARTESIAN_POINT ( 'NONE',  ( 0.5036000104604843042, -81.94200777690970483, 1.144331684476223909 ) ) ;
#30803 = CARTESIAN_POINT ( 'NONE',  ( -1.419508297042999967, -77.92612078354999028, -0.6202052238666999617 ) ) ;
#30804 = CARTESIAN_POINT ( 'NONE',  ( 9.100722152916000951, -77.11296757197209217, -3.274758550341999808 ) ) ;
#30805 = CARTESIAN_POINT ( 'NONE',  ( -0.1451771616029145784, -82.63257818562124157, 1.503302264768924257 ) ) ;
#30806 = CARTESIAN_POINT ( 'NONE',  ( -12.77306367233000017, -61.85881314422999822, 1.040970605966999862 ) ) ;
#30807 = CARTESIAN_POINT ( 'NONE',  ( 0.1721334691643799375, -80.22656007235991638, -10.74864075682200593 ) ) ;
#30808 = DIRECTION ( 'NONE',  ( 0.000000000000000000, -1.000000000000000000, 0.000000000000000000 ) ) ;
#30809 = CARTESIAN_POINT ( 'NONE',  ( 11.80573474569990644, -75.80000000000001137, 2.494142706669169041 ) ) ;
#30810 = ORIENTED_EDGE ( 'NONE', *, *, #42658, .T. ) ;
#30811 = CARTESIAN_POINT ( 'NONE',  ( 0.5288604877964585560, -81.75996230616158300, -1.132634026371601044 ) ) ;
#30812 = CARTESIAN_POINT ( 'NONE',  ( 1.247385803315000041, -61.27722255996999934, 12.50301438880000049 ) ) ;
#30813 = CYLINDRICAL_SURFACE ( 'NONE', #33065, 9.500000000000000000 ) ;
#30814 = CARTESIAN_POINT ( 'NONE',  ( 10.75000000000000355, -78.74148622562242394, -1.150112874675813579 ) ) ;
#30815 = ORIENTED_EDGE ( 'NONE', *, *, #20837, .T. ) ;
#30816 = ORIENTED_EDGE ( 'NONE', *, *, #6666, .F. ) ;
#30817 = CARTESIAN_POINT ( 'NONE',  ( 0.2607165876585000319, -81.85403697029799730, 1.593499524613000151 ) ) ;
#30818 = ORIENTED_EDGE ( 'NONE', *, *, #49807, .F. ) ;
#30819 = CARTESIAN_POINT ( 'NONE',  ( 10.06692933812901636, -55.09657286943566845, -7.655995045250127085 ) ) ;
#30820 = AXIS2_PLACEMENT_3D ( 'NONE', #20416, #17939, #21270 ) ;
#30821 = ORIENTED_EDGE ( 'NONE', *, *, #6959, .T. ) ;
#30822 = FACE_OUTER_BOUND ( 'NONE', #25989, .T. ) ;
#30823 = CARTESIAN_POINT ( 'NONE',  ( -1.454554856007286512, -78.96979166281558093, -3.085434141896665317 ) ) ;
#30824 = CARTESIAN_POINT ( 'NONE',  ( -3.912255148455999976, -78.97757640497698617, 10.19164489391000217 ) ) ;
#30825 = CARTESIAN_POINT ( 'NONE',  ( 1.698401934077000019, -24.22014045903999957, -12.66748707612999958 ) ) ;
#30826 = CARTESIAN_POINT ( 'NONE',  ( -2.147210328137000079, -80.73445849046999001, -3.082346235878000051 ) ) ;
#30827 = CARTESIAN_POINT ( 'NONE',  ( -3.634880433973583180, -79.30591575590990772, 8.776894603130271477 ) ) ;
#30828 = VERTEX_POINT ( 'NONE', #8946 ) ;
#30829 = CARTESIAN_POINT ( 'NONE',  ( 3.792698199283999649, -78.00290701960965123, -10.36819406884000117 ) ) ;
#30830 = CARTESIAN_POINT ( 'NONE',  ( 4.786724983033999514, -78.66227135457999964, -11.39381604551999772 ) ) ;
#30831 = AXIS2_PLACEMENT_3D ( 'NONE', #50704, #28225, #42709 ) ;
#30832 = VERTEX_POINT ( 'NONE', #32521 ) ;
#30833 = DIRECTION ( 'NONE',  ( 0.000000000000000000, 0.000000000000000000, -1.000000000000000000 ) ) ;
#30834 = AXIS2_PLACEMENT_3D ( 'NONE', #28548, #37706, #54562 ) ;
#30835 = ADVANCED_FACE ( 'NONE', ( #13656 ), #22812, .F. ) ;
#30836 = CARTESIAN_POINT ( 'NONE',  ( -0.2340539085346999837, -80.15469965994898871, 1.312933706406000267 ) ) ;
#30837 = CARTESIAN_POINT ( 'NONE',  ( -9.311105030178968178, -77.13820107031234841, -0.1312602372466275813 ) ) ;
#30838 = CARTESIAN_POINT ( 'NONE',  ( 0.4861418710280006605, -86.09999999999979536, -4.619149248742774994 ) ) ;
#30839 = CARTESIAN_POINT ( 'NONE',  ( 8.332845033087998843, -76.09460843601999613, -7.273191856730000460 ) ) ;
#30840 = CARTESIAN_POINT ( 'NONE',  ( -13.07887593023000150, -78.01141106207001030, -0.9532572298037998992 ) ) ;
#30841 = CARTESIAN_POINT ( 'NONE',  ( 12.15305909882999913, -77.97218707672999471, -3.479748152880000056 ) ) ;
#30842 = FACE_OUTER_BOUND ( 'NONE', #36762, .T. ) ;
#30843 = CARTESIAN_POINT ( 'NONE',  ( -9.056035971749563984, -78.61657572224720525, -1.894306744419020250 ) ) ;
#30844 = DIRECTION ( 'NONE',  ( 0.000000000000000000, -1.000000000000000000, 0.000000000000000000 ) ) ;
#30845 = CARTESIAN_POINT ( 'NONE',  ( 0.2546300289211099743, -2.969716266808483773, 3.249428101292205717 ) ) ;
#30846 = CARTESIAN_POINT ( 'NONE',  ( 3.342627291359000274, -80.97450264934799691, 1.179748523689000184 ) ) ;
#30847 = EDGE_CURVE ( 'NONE', #52194, #51486, #43849, .T. ) ;
#30848 = CYLINDRICAL_SURFACE ( 'NONE', #58105, 1.750000000000000000 ) ;
#30849 = CARTESIAN_POINT ( 'NONE',  ( -6.711381441964999972, -80.25968072146179111, 9.048015653393999713 ) ) ;
#30850 = CARTESIAN_POINT ( 'NONE',  ( 0.07399134906894000441, -2.156119551551000324, 3.805339572302000040 ) ) ;
#30851 = CARTESIAN_POINT ( 'NONE',  ( -0.3056428120159084827, -80.64427355544083298, 1.237341845012493557 ) ) ;
#30852 = ORIENTED_EDGE ( 'NONE', *, *, #9852, .F. ) ;
#30853 = CYLINDRICAL_SURFACE ( 'NONE', #48063, 9.250000000000000000 ) ;
#30854 = ADVANCED_FACE ( 'NONE', ( #9533 ), #54530, .F. ) ;
#30855 = CARTESIAN_POINT ( 'NONE',  ( 1.439896632895334649, -79.33541666666666003, -10.99999999999999822 ) ) ;
#30856 = CARTESIAN_POINT ( 'NONE',  ( 1.304222966381000104, -81.48863003010599471, 0.2785293583740000023 ) ) ;
#30857 = PLANE ( 'NONE',  #19890 ) ;
#30858 = CARTESIAN_POINT ( 'NONE',  ( -3.274010471232999819, -77.37790540356000690, 12.59444704299999884 ) ) ;
#30859 = AXIS2_PLACEMENT_3D ( 'NONE', #13347, #694, #44659 ) ;
#30860 = CARTESIAN_POINT ( 'NONE',  ( -8.114920487416192429, -61.62884529303471481, -9.847900218127630723 ) ) ;
#30861 = CARTESIAN_POINT ( 'NONE',  ( 12.53239398062000198, -19.23513569609999863, -1.667936688463999895 ) ) ;
#30862 = VERTEX_POINT ( 'NONE', #14817 ) ;
#30863 = ADVANCED_FACE ( 'NONE', ( #24562 ), #46438, .T. ) ;
#30864 = CARTESIAN_POINT ( 'NONE',  ( 6.586108526242999694, -80.07391735373440156, 8.810401493720998900 ) ) ;
#30865 = CARTESIAN_POINT ( 'NONE',  ( 8.385806979662810079, -53.91189752975327565, -9.298530586697486555 ) ) ;
#30866 = CONICAL_SURFACE ( 'NONE', #41261, 9.649999999948999374, 0.7853981633972997312 ) ;
#30867 = CARTESIAN_POINT ( 'NONE',  ( 0.7893528373467999515, -81.56550947952499087, 1.046299686877999902 ) ) ;
#30868 = CARTESIAN_POINT ( 'NONE',  ( -6.043427764450784778, -78.98333333333332007, -10.48543666025109822 ) ) ;
#30869 = CARTESIAN_POINT ( 'NONE',  ( 4.939304878001000709, -78.85185680379399287, 8.013392654152999839 ) ) ;
#30870 = TOROIDAL_SURFACE ( 'NONE', #41136, 17.50000000000000000, 5.000000000000000000 ) ;
#30871 = CARTESIAN_POINT ( 'NONE',  ( -3.362339023590000142, -84.87007892634498774, -2.470067118709999843 ) ) ;
#30872 = CARTESIAN_POINT ( 'NONE',  ( 1.612132099153596565, -79.96332688086813789, 10.62905773014771071 ) ) ;
#30873 = CARTESIAN_POINT ( 'NONE',  ( 0.2827145210274000231, -79.74366136053998844, -1.389291862697999980 ) ) ;
#30874 = ORIENTED_EDGE ( 'NONE', *, *, #47629, .T. ) ;
#30875 = CARTESIAN_POINT ( 'NONE',  ( -2.397279086078224708, -77.20726813167010505, -10.47917899088556126 ) ) ;
#30876 = CARTESIAN_POINT ( 'NONE',  ( -0.7967926909478446618, -82.20442708333173698, 1.035424098837760098 ) ) ;
#30877 = VECTOR ( 'NONE', #29104, 1000.000000000000000 ) ;
#30878 = CARTESIAN_POINT ( 'NONE',  ( -0.7377377962817491808, -78.86606320632056111, -3.889143611529064515 ) ) ;
#30879 = ORIENTED_EDGE ( 'NONE', *, *, #31426, .T. ) ;
#30880 = ORIENTED_EDGE ( 'NONE', *, *, #4441, .T. ) ;
#30881 = EDGE_CURVE ( 'NONE', #23208, #8867, #13610, .T. ) ;
#30882 = CARTESIAN_POINT ( 'NONE',  ( 12.83044039271999992, -55.49360374314999689, 2.062670899148999926 ) ) ;
#30883 = CARTESIAN_POINT ( 'NONE',  ( -9.522411774477998136, -79.76552920275499048, 5.478866733777000952 ) ) ;
#30884 = ORIENTED_EDGE ( 'NONE', *, *, #6448, .F. ) ;
#30885 = B_SPLINE_CURVE_WITH_KNOTS ( 'NONE', 3,
 ( #23731, #41742, #1319, #19313, #14863, #16622, #29883, #30175, #47939, #38471 ),
 .UNSPECIFIED., .F., .F.,
 ( 4, 2, 2, 2, 4 ),
 ( 0.000000000000000000, 0.1250000001980599851, 0.2500000003961199702, 0.3750000005941799275, 0.5000000007922399403 ),
 .UNSPECIFIED. ) ;
#30886 = CARTESIAN_POINT ( 'NONE',  ( 11.99621472858000004, -77.52212751510998601, 2.018255885614000267 ) ) ;
#30887 = VERTEX_POINT ( 'NONE', #34846 ) ;
#30888 = ORIENTED_EDGE ( 'NONE', *, *, #11689, .F. ) ;
#30889 = CARTESIAN_POINT ( 'NONE',  ( -3.112536536121000008, -86.17851878748298589, 1.385790882648999967 ) ) ;
#30890 = CARTESIAN_POINT ( 'NONE',  ( 6.653382217586999658, -80.06537887755254701, 7.150748904218000135 ) ) ;
#30891 = B_SPLINE_SURFACE_WITH_KNOTS ( 'NONE', 3, 3, ( 
 ( #50931, #10479, #11358, #56224 ),
 ( #28464, #15774, #46513, #33766 ),
 ( #37620, #6037, #51804, #42940 ),
 ( #24046, #42063, #51226, #34630 ),
 ( #21923, #25783, #57081, #26634 ),
 ( #25491, #34340, #39932, #16645 ),
 ( #44668, #8648, #3638, #21351 ),
 ( #57948, #57653, #12211, #17209 ),
 ( #43809, #30198, #17502, #34913 ),
 ( #35197, #16933, #48522, #52657 ),
 ( #26350, #16359, #48246, #3354 ),
 ( #40230, #26061, #4221, #53229 ),
 ( #21641, #39366, #7783, #7494 ),
 ( #3073, #57373, #44088, #8066 ),
 ( #52945, #39647, #12495, #30493 ),
 ( #43512, #12778, #21067, #39072 ),
 ( #35491, #47961, #22219, #30773 ) ),
 .UNSPECIFIED., .F., .F., .F.,
 ( 4, 1, 1, 1, 1, 1, 1, 1, 1, 1, 1, 1, 1, 1, 4 ),
 ( 4, 4 ),
 ( -0.01011837001263999995, 0.000000000000000000, 0.08333333333333001192, 0.1666666666667000196, 0.2500000000000000000, 0.3333333333333000081, 0.4166666666666999919, 0.5000000000000000000, 0.5833333333333000637, 0.6666666666667000474, 0.7500000000000000000, 0.8333333333333000637, 0.9166666666667000474, 1.000000000000000000, 1.010372850415000023 ),
 ( -0.3559705548695000221, 1.357613361108999994 ),
 .UNSPECIFIED. ) ;
#30892 = ORIENTED_EDGE ( 'NONE', *, *, #56411, .F. ) ;
#30893 = CARTESIAN_POINT ( 'NONE',  ( 1.382657135218546385, -82.08072916571396149, -0.3707038244580741493 ) ) ;
#30894 = ORIENTED_EDGE ( 'NONE', *, *, #13958, .F. ) ;
#30895 = CARTESIAN_POINT ( 'NONE',  ( -0.5175321235027776634, -80.24194154202476170, -1.165191863362585512 ) ) ;
#30896 = CARTESIAN_POINT ( 'NONE',  ( 1.996052055574059514, -78.85171435493610659, -3.456153366506571789 ) ) ;
#30897 = CARTESIAN_POINT ( 'NONE',  ( -12.00000000000000000, -77.89999999999999147, -2.795183092923000262E-14 ) ) ;
#30898 = CARTESIAN_POINT ( 'NONE',  ( -0.4515105396358876089, -18.45278097531891959, 10.99076531923741840 ) ) ;
#30899 = FACE_OUTER_BOUND ( 'NONE', #26832, .T. ) ;
#30900 = CARTESIAN_POINT ( 'NONE',  ( 11.75000000000000000, -78.54999999999999716, 0.000000000000000000 ) ) ;
#30901 = CARTESIAN_POINT ( 'NONE',  ( 7.682344222584999827, -59.56462890159999546, -10.04116292117000064 ) ) ;
#30902 = CARTESIAN_POINT ( 'NONE',  ( 9.075776011423059231, -78.83460089325743070, -1.786594630451423971 ) ) ;
#30903 = CARTESIAN_POINT ( 'NONE',  ( -10.15831671671000080, -24.21991983044000207, 7.756223511073000232 ) ) ;
#30904 = CARTESIAN_POINT ( 'NONE',  ( 3.840130277397999947, -82.29725264934799611, -1.637844927514000126 ) ) ;
#30905 = CARTESIAN_POINT ( 'NONE',  ( -1.296582552281000167, -77.37128667140099481, -9.676207389328999042 ) ) ;
#30906 = LINE ( 'NONE', #17345, #41724 ) ;
#30907 = VECTOR ( 'NONE', #11583, 1000.000000000000114 ) ;
#30908 = CARTESIAN_POINT ( 'NONE',  ( 10.48771805366000009, -21.75560171527000008, -7.686918321049000191 ) ) ;
#30909 = CARTESIAN_POINT ( 'NONE',  ( -1.669724228656999987, -23.36897676534000112, 12.48434610067999984 ) ) ;
#30910 = CARTESIAN_POINT ( 'NONE',  ( 0.1738177897059751675, -81.38563030058524816, -1.313728265332345657 ) ) ;
#30911 = CARTESIAN_POINT ( 'NONE',  ( 1.199999999999999956, -75.00000000000000000, -7.200000000000000178 ) ) ;
#30912 = FACE_OUTER_BOUND ( 'NONE', #24097, .T. ) ;
#30913 = CARTESIAN_POINT ( 'NONE',  ( 1.480842118789938100, -80.57602979559986522, -0.4564364147450694631 ) ) ;
#30914 = CARTESIAN_POINT ( 'NONE',  ( 12.44180635032999938, -60.89260544892000127, -1.459447571596000026 ) ) ;
#30915 = CARTESIAN_POINT ( 'NONE',  ( 1.449215700157000075, -78.62171603714999435, -0.7120307440141999678 ) ) ;
#30916 = CARTESIAN_POINT ( 'NONE',  ( -9.549999999999998934, -79.99999999999998579, 0.000000000000000000 ) ) ;
#30917 = CARTESIAN_POINT ( 'NONE',  ( -8.496131438301000927, -77.97256569596500242, 6.855006679309999740 ) ) ;
#30918 = CARTESIAN_POINT ( 'NONE',  ( -11.03570087982000025, -77.47569360493399415, -5.118186854384000561 ) ) ;
#30919 = LINE ( 'NONE', #3782, #11834 ) ;
#30921 = CARTESIAN_POINT ( 'NONE',  ( 1.288803220532000138, -78.00908736353699169, 0.2820490268708999437 ) ) ;
#30920 = CARTESIAN_POINT ( 'NONE',  ( 6.585791278903703194, -80.14058402040107865, 8.809977328666299456 ) ) ;
#30922 = EDGE_LOOP ( 'NONE', ( #4561, #52704, #57603, #25535 ) ) ;
#30923 = EDGE_CURVE ( 'NONE', #7174, #23068, #16448, .T. ) ;
#30924 = CARTESIAN_POINT ( 'NONE',  ( -10.42272502865000128, -20.24546192895000019, -7.691893942754999713 ) ) ;
#30925 = CARTESIAN_POINT ( 'NONE',  ( 7.303865428629999990, -79.08185514870999100, 9.528096774331999086 ) ) ;
#30926 = CARTESIAN_POINT ( 'NONE',  ( 3.207556080690000311, -80.92498568429859063, 10.58040010179999868 ) ) ;
#30927 = CARTESIAN_POINT ( 'NONE',  ( 11.70000000000000107, -76.00000000000000000, 0.000000000000000000 ) ) ;
#30928 = CARTESIAN_POINT ( 'NONE',  ( -4.531904799951000484, -77.42579691695999600, -10.26060180864999971 ) ) ;
#30929 = DIRECTION ( 'NONE',  ( 0.000000000000000000, -1.000000000000000000, 0.000000000000000000 ) ) ;
#30930 = FACE_OUTER_BOUND ( 'NONE', #19740, .T. ) ;
#30931 = CARTESIAN_POINT ( 'NONE',  ( -9.666799225812999552, -79.71909680386698938, -1.488628203271999961 ) ) ;
#30932 = CARTESIAN_POINT ( 'NONE',  ( 12.43640309385000009, -24.91747517602999906, 0.05224034426415000154 ) ) ;
#30933 = CYLINDRICAL_SURFACE ( 'NONE', #19873, 9.500000000000000000 ) ;
#30934 = ORIENTED_EDGE ( 'NONE', *, *, #6029, .T. ) ;
#30935 = CARTESIAN_POINT ( 'NONE',  ( -12.74365836111545391, -55.27810168844658278, 1.980611005600371399 ) ) ;
#30936 = CARTESIAN_POINT ( 'NONE',  ( 8.179414028892216137, -24.74093020614164473, -9.502908389697516611 ) ) ;
#30937 = CIRCLE ( 'NONE', #38515, 2.299999999999999822 ) ;
#30938 = CARTESIAN_POINT ( 'NONE',  ( -2.316740560951787486, -1.663670436995591473, -2.311895541344660909 ) ) ;
#30939 = CARTESIAN_POINT ( 'NONE',  ( -10.55910102243999837, -56.01514526721999943, -7.642147947524999374 ) ) ;
#30940 = CARTESIAN_POINT ( 'NONE',  ( 1.096228918643000094, -84.23117953870900010, 3.373845695877999873 ) ) ;
#30941 = EDGE_CURVE ( 'NONE', #12936, #35380, #34272, .T. ) ;
#30942 = VERTEX_POINT ( 'NONE', #25713 ) ;
#30943 = CARTESIAN_POINT ( 'NONE',  ( -8.488829372234999227, -77.37345827014598854, 7.154399614211999214 ) ) ;
#30944 = DIRECTION ( 'NONE',  ( 1.000000000000000000, 0.000000000000000000, 0.000000000000000000 ) ) ;
#30945 = CARTESIAN_POINT ( 'NONE',  ( -0.8506806241676574398, -1.104166666666666963, -3.165411199172027068 ) ) ;
#30946 = EDGE_LOOP ( 'NONE', ( #41999, #39615, #30657, #23884, #17205 ) ) ;
#30947 = ORIENTED_EDGE ( 'NONE', *, *, #31613, .T. ) ;
#30948 = CARTESIAN_POINT ( 'NONE',  ( -9.778561352688999619, -53.75143577336000078, -8.284566532368000225 ) ) ;
#30949 = CARTESIAN_POINT ( 'NONE',  ( 9.202039358297998461, -80.10013463714798831, 2.360608321670000453 ) ) ;
#30950 = ORIENTED_EDGE ( 'NONE', *, *, #13889, .F. ) ;
#30951 = ORIENTED_EDGE ( 'NONE', *, *, #23726, .T. ) ;
#30952 = CARTESIAN_POINT ( 'NONE',  ( 10.22898553533000054, -76.39377822758400782, -6.925005706880000389 ) ) ;
#30953 = CARTESIAN_POINT ( 'NONE',  ( 0.000000000000000000, -60.04999999966999980, 12.00000000000000000 ) ) ;
#30954 = CARTESIAN_POINT ( 'NONE',  ( -0.07270704760602998695, -78.82788729812999406, -1.533131890934999797 ) ) ;
#30955 = VERTEX_POINT ( 'NONE', #12142 ) ;
#30956 = EDGE_CURVE ( 'NONE', #2822, #15288, #40052, .T. ) ;
#30957 = CARTESIAN_POINT ( 'NONE',  ( 10.01752115541999899, -18.80828330197000042, 7.660412752602000275 ) ) ;
#30958 = CARTESIAN_POINT ( 'NONE',  ( -1.072066298137815732, -79.31286409919876235, -1.082357936291675538 ) ) ;
#30959 = CARTESIAN_POINT ( 'NONE',  ( 1.222783487291517757, -80.33365183381954466, -0.2622213962109313790 ) ) ;
#30960 = CARTESIAN_POINT ( 'NONE',  ( -3.187445619818999987, -77.97624008069000467, 12.55797944092000051 ) ) ;
#30961 = PRODUCT_DEFINITION_CONTEXT ( 'detailed design', #54170, 'design' ) ;
#30962 = CARTESIAN_POINT ( 'NONE',  ( -0.8253947190444999027, -77.36913936749189702, -11.18645762290999990 ) ) ;
#30963 = CARTESIAN_POINT ( 'NONE',  ( -7.714303428875997959, -15.69705297113999443, 12.53545825868000385 ) ) ;
#30964 = CARTESIAN_POINT ( 'NONE',  ( 4.443227334435309039, -86.36264283715698298, 0.5100107989077657944 ) ) ;
#30965 = CARTESIAN_POINT ( 'NONE',  ( 6.879576957522999692, -79.22414080250499069, 8.859431780707000215 ) ) ;
#30966 = CARTESIAN_POINT ( 'NONE',  ( -0.1991013119907288076, -79.97697863826387277, 9.262774322989109521 ) ) ;
#30967 = FACE_OUTER_BOUND ( 'NONE', #37297, .T. ) ;
#30968 = VERTEX_POINT ( 'NONE', #25135 ) ;
#30969 = CARTESIAN_POINT ( 'NONE',  ( 3.390474011741000382, -79.27013871977898418, -10.74400392503999946 ) ) ;
#30970 = CARTESIAN_POINT ( 'NONE',  ( 9.569482281372000188, -76.74786216769000191, -7.743360016082000641 ) ) ;
#30971 = CARTESIAN_POINT ( 'NONE',  ( -1.499766830043999910, -80.34094972420699321, 0.2228039671692000068 ) ) ;
#30972 = CARTESIAN_POINT ( 'NONE',  ( -1.242864761025999965, -77.64406422756130155, 0.2245736866142999943 ) ) ;
#30973 = CARTESIAN_POINT ( 'NONE',  ( -0.1607120884409986850, -2.970659796132148589, -3.515337033079625417 ) ) ;
#30974 = CONICAL_SURFACE ( 'NONE', #20643, 5.599999999950999729, 0.2449786631268792425 ) ;
#30975 = CARTESIAN_POINT ( 'NONE',  ( -10.10712711932128549, -17.53345760874380588, 7.860996423953121592 ) ) ;
#30976 = DIRECTION ( 'NONE',  ( -1.000000000000000000, 0.000000000000000000, 0.000000000000000000 ) ) ;
#30977 = CARTESIAN_POINT ( 'NONE',  ( -8.130811096204000776, -61.48523690322999613, -9.546858433459998849 ) ) ;
#30978 = CARTESIAN_POINT ( 'NONE',  ( 6.829411927397999627, -79.23435533332899183, -8.823306204757001225 ) ) ;
#30979 = CARTESIAN_POINT ( 'NONE',  ( -4.504865641233999796, -77.29261498579799650, 8.632419597676001644 ) ) ;
#30980 = DIRECTION ( 'NONE',  ( -0.7071067811865475727, 0.000000000000000000, -0.7071067811865475727 ) ) ;
#30981 = CARTESIAN_POINT ( 'NONE',  ( 0.4713521909880000194, -79.02188087448040221, 12.02020425643999957 ) ) ;
#30982 = CARTESIAN_POINT ( 'NONE',  ( 0.000000000000000000, -81.89999999962999766, 0.000000000000000000 ) ) ;
#30983 = LINE ( 'NONE', #31275, #18730 ) ;
#30984 = ORIENTED_EDGE ( 'NONE', *, *, #53645, .F. ) ;
#30986 = B_SPLINE_CURVE_WITH_KNOTS ( 'NONE', 3,
 ( #24021, #11050, #19020, #55319, #14574, #32568, #42036, #29031 ),
 .UNSPECIFIED., .F., .F.,
 ( 4, 2, 2, 4 ),
 ( 0.000000000000000000, 0.5000000000000000000, 0.7500000000000000000, 1.000000000000000000 ),
 .UNSPECIFIED. ) ;
#30985 = CARTESIAN_POINT ( 'NONE',  ( 1.533821497824999991, -81.66375084183000865, 0.4022281561003999695 ) ) ;
#30987 = CARTESIAN_POINT ( 'NONE',  ( 0.3265465218672000125, -80.09950314121999781, -1.431717670164000200 ) ) ;
#30988 = CARTESIAN_POINT ( 'NONE',  ( 9.249483092228999226, -79.25084128437099196, 0.09778817195952001218 ) ) ;
#30989 = CARTESIAN_POINT ( 'NONE',  ( 0.000000000000000000, -75.15999999999999659, 0.000000000000000000 ) ) ;
#30990 = CARTESIAN_POINT ( 'NONE',  ( 0.000000000000000000, -79.65000000003199432, -9.349999999968000353 ) ) ;
#30991 = CARTESIAN_POINT ( 'NONE',  ( -0.1931105070826031334, -78.86330530744118050, -1.260507006898233806 ) ) ;
#30992 = VECTOR ( 'NONE', #32870, 1000.000000000000114 ) ;
#30993 = LINE ( 'NONE', #31579, #50637 ) ;
#30994 = CARTESIAN_POINT ( 'NONE',  ( -3.230363664242999810, -78.10789415034599870, -9.171071524558000121 ) ) ;
#30995 = CARTESIAN_POINT ( 'NONE',  ( 4.657000555087000393, -77.30872832793998839, -8.305583776142999142 ) ) ;
#30996 = CARTESIAN_POINT ( 'NONE',  ( -1.295048492664000017, -54.27106480841000291, -12.54716442233000073 ) ) ;
#30997 = CARTESIAN_POINT ( 'NONE',  ( 9.770618005419288821, -75.99681979438835810, 6.526589924811744936 ) ) ;
#30998 = FACE_OUTER_BOUND ( 'NONE', #19787, .T. ) ;
#30999 = EDGE_LOOP ( 'NONE', ( #35732, #40511, #32348, #8529 ) ) ;
#31000 = CARTESIAN_POINT ( 'NONE',  ( 8.082524092276875294, -78.79166666666665719, 4.658475568430836766 ) ) ;
#31001 = EDGE_CURVE ( 'NONE', #5420, #5785, #26287, .T. ) ;
#31002 = CARTESIAN_POINT ( 'NONE',  ( -11.28059581212394846, -77.17303457489015273, 3.843385645491329772 ) ) ;
#31003 = CARTESIAN_POINT ( 'NONE',  ( -3.484880015263546404, -78.48547957940618858, 0.06569681124688563079 ) ) ;
#31004 = EDGE_CURVE ( 'NONE', #2177, #43339, #52592, .T. ) ;
#31005 = CARTESIAN_POINT ( 'NONE',  ( -0.6811744818814000624, -82.42108714457998531, -1.520282978132999840 ) ) ;
#31006 = CARTESIAN_POINT ( 'NONE',  ( -10.69701368780000017, -79.92224720141999228, 1.066019776055000090 ) ) ;
#31007 = CARTESIAN_POINT ( 'NONE',  ( 0.2678032734880190224, -16.78567224710744199, 12.70526550769191410 ) ) ;
#31008 = CARTESIAN_POINT ( 'NONE',  ( 12.05139359237000107, -76.67257108724299997, -2.863729330572000187 ) ) ;
#31009 = CARTESIAN_POINT ( 'NONE',  ( -5.747123378374999980, -78.61567021304000491, 10.24856442990000005 ) ) ;
#31010 = CARTESIAN_POINT ( 'NONE',  ( 7.444278262535061863, -76.81467768451751965, 7.855135693196025670 ) ) ;
#31011 = EDGE_LOOP ( 'NONE', ( #11472, #3116, #26972, #9029, #21118, #317 ) ) ;
#31012 = CARTESIAN_POINT ( 'NONE',  ( 2.143349548760000278, -78.50057660935300419, 10.82163513946999878 ) ) ;
#31013 = CARTESIAN_POINT ( 'NONE',  ( 0.4724532946902580410, -79.94440778530983494, 1.157109430825660867 ) ) ;
#31014 = CARTESIAN_POINT ( 'NONE',  ( 0.7999999999999001243, -23.15000000002000036, -12.00000000000000000 ) ) ;
#31015 = CARTESIAN_POINT ( 'NONE',  ( 2.318769420003345072, -78.62148118236264338, 4.014936390581685721 ) ) ;
#31016 = EDGE_CURVE ( 'NONE', #17140, #12818, #16865, .T. ) ;
#31017 = CARTESIAN_POINT ( 'NONE',  ( 3.357763675545999860, -78.89238723821299004, -10.64034880800999971 ) ) ;
#31018 = CARTESIAN_POINT ( 'NONE',  ( -12.50239399162999909, -54.11640749821000185, 1.003653728895000041 ) ) ;
#31019 = CARTESIAN_POINT ( 'NONE',  ( -1.135826688880000157, -81.40663953506998496, -0.9797437077257000748 ) ) ;
#31020 = CARTESIAN_POINT ( 'NONE',  ( 11.65296779515999859, -78.05105294172599883, -3.873515295708999773 ) ) ;
#31021 = AXIS2_PLACEMENT_3D ( 'NONE', #57136, #34684, #3694 ) ;
#31022 = CARTESIAN_POINT ( 'NONE',  ( -1.460959015002473382, -81.02083333333331439, -0.3926218265389205819 ) ) ;
#31023 = DIRECTION ( 'NONE',  ( 0.000000000000000000, -1.000000000000000000, 0.000000000000000000 ) ) ;
#31024 = CARTESIAN_POINT ( 'NONE',  ( 9.469145113845355510, -79.49323344442748862, 5.723973398464534235 ) ) ;
#31025 = FACE_OUTER_BOUND ( 'NONE', #24557, .T. ) ;
#31026 = EDGE_LOOP ( 'NONE', ( #5560, #43863, #14826, #10811, #4774, #26599 ) ) ;
#31027 = VERTEX_POINT ( 'NONE', #12712 ) ;
#31028 = LINE ( 'NONE', #8615, #14539 ) ;
#31029 = CIRCLE ( 'NONE', #29159, 5.000000000000000000 ) ;
#31030 = ORIENTED_EDGE ( 'NONE', *, *, #19517, .F. ) ;
#31031 = DIRECTION ( 'NONE',  ( -1.000000000000000000, 0.000000000000000000, 0.000000000000000000 ) ) ;
#31032 = ORIENTED_EDGE ( 'NONE', *, *, #8416, .T. ) ;
#31033 = CARTESIAN_POINT ( 'NONE',  ( -7.919595949288999570, -59.94999999446000771, 8.768124086549999419 ) ) ;
#31034 = CARTESIAN_POINT ( 'NONE',  ( -6.771245932390999478, -78.21354745617999527, -8.709304295962999376 ) ) ;
#31035 = AXIS2_PLACEMENT_3D ( 'NONE', #35330, #53357, #44500 ) ;
#31036 = CARTESIAN_POINT ( 'NONE',  ( -5.743104117080999771, -79.05483998579799731, 7.801152530868000312 ) ) ;
#31037 = CARTESIAN_POINT ( 'NONE',  ( -5.053239713898484808, -78.17904410541564175, -7.747788339080754483 ) ) ;
#31038 = CARTESIAN_POINT ( 'NONE',  ( 11.14115696400000033, -78.93906611367098947, -1.301050381412999890 ) ) ;
#31039 = CARTESIAN_POINT ( 'NONE',  ( -0.4018693904811616591, -79.50120578641283942, 1.186371210911240759 ) ) ;
#31040 = ORIENTED_EDGE ( 'NONE', *, *, #3026, .F. ) ;
#31041 = VERTEX_POINT ( 'NONE', #43739 ) ;
#31042 = CARTESIAN_POINT ( 'NONE',  ( 2.855611011456188120, -77.45020245399071257, 8.798067008888779128 ) ) ;
#31043 = CARTESIAN_POINT ( 'NONE',  ( -6.065106684382000068, -77.29113158382398296, 9.224892016835999797 ) ) ;
#31044 = CARTESIAN_POINT ( 'NONE',  ( -9.252740428349001789, -77.42083333333333428, -2.486604901413163926 ) ) ;
#31045 = EDGE_CURVE ( 'NONE', #44782, #29606, #37562, .T. ) ;
#31046 = CARTESIAN_POINT ( 'NONE',  ( 7.890274420948999001, -79.09100735980197783, -5.649267206312000411 ) ) ;
#31047 = CARTESIAN_POINT ( 'NONE',  ( 11.36243170732000074, -76.64353223351000111, -3.693170977796000010 ) ) ;
#31048 = CARTESIAN_POINT ( 'NONE',  ( -6.759806091175823539, -79.46177246518648474, -6.674805502530112733 ) ) ;
#31049 = CARTESIAN_POINT ( 'NONE',  ( -0.6580604922749000441, -79.30303859595998972, -1.488334326434000099 ) ) ;
#31050 = B_SPLINE_CURVE_WITH_KNOTS ( 'NONE', 3,
 ( #35148, #8304, #26304, #3874 ),
 .UNSPECIFIED., .F., .F.,
 ( 4, 4 ),
 ( 0.000000000000000000, 1.000000000000000000 ),
 .UNSPECIFIED. ) ;
#31051 = CARTESIAN_POINT ( 'NONE',  ( 12.89999999994999769, -2.999999999951000085, 1.886268220167000189E-09 ) ) ;
#31052 = CARTESIAN_POINT ( 'NONE',  ( -9.250000000000000000, -77.59999999999999432, 0.000000000000000000 ) ) ;
#31053 = CARTESIAN_POINT ( 'NONE',  ( -10.19019669286999985, -23.19643762568000156, -7.646965578493999161 ) ) ;
#31054 = CARTESIAN_POINT ( 'NONE',  ( -2.485321053156992477, -79.19615742320637253, 9.250752650985239356 ) ) ;
#31055 = VERTEX_POINT ( 'NONE', #39004 ) ;
#31056 = CARTESIAN_POINT ( 'NONE',  ( 11.41978910860999896, -79.65576480666599934, 4.917167810709999642 ) ) ;
#31057 = DIRECTION ( 'NONE',  ( 1.000000000000000000, 0.000000000000000000, 0.000000000000000000 ) ) ;
#31058 = CARTESIAN_POINT ( 'NONE',  ( -2.132471413802949467, -77.99102497083757157, 10.53628444161482847 ) ) ;
#31059 = CARTESIAN_POINT ( 'NONE',  ( 10.18066396183999878, -78.42807224564398894, 6.314281093748000728 ) ) ;
#31060 = CARTESIAN_POINT ( 'NONE',  ( -12.70395504303452761, -61.40679290093079601, 1.447100708791914769 ) ) ;
#31062 = CARTESIAN_POINT ( 'NONE',  ( -0.5506765233279000693, -16.74045707756000212, -12.77514798311000099 ) ) ;
#31061 = CARTESIAN_POINT ( 'NONE',  ( 7.641012305241000391, -60.08917723397000543, 10.18589226633000067 ) ) ;
#31063 = CARTESIAN_POINT ( 'NONE',  ( -0.9356112496366845166, -54.05892169592745233, 12.50329130245003206 ) ) ;
#31064 = CARTESIAN_POINT ( 'NONE',  ( 8.563134967179999890, -80.25043697167899381, -7.360427151328000406 ) ) ;
#31065 = CARTESIAN_POINT ( 'NONE',  ( -0.4831833036036000117, -82.24511132376299827, -1.158768654956999988 ) ) ;
#31066 = CARTESIAN_POINT ( 'NONE',  ( -5.774605976465999824, -77.90556621773498591, -9.668913608825000949 ) ) ;
#31067 = LINE ( 'NONE', #8655, #8136 ) ;
#31068 = CARTESIAN_POINT ( 'NONE',  ( 7.473878879214000293, -80.13975433285759209, 8.225614977841999576 ) ) ;
#31069 = ORIENTED_EDGE ( 'NONE', *, *, #9126, .T. ) ;
#31070 = CARTESIAN_POINT ( 'NONE',  ( 0.000000000000000000, -32.88214388149999934, 0.000000000000000000 ) ) ;
#31071 = CARTESIAN_POINT ( 'NONE',  ( -1.044910384896000188, -53.74473505772000692, 12.77260826194999943 ) ) ;
#31072 = DIRECTION ( 'NONE',  ( -0.0001178721535674749112, 0.000000000000000000, 0.9999999930530777403 ) ) ;
#31073 = CARTESIAN_POINT ( 'NONE',  ( 1.522081929427000047, -1.790731624101999930, -3.312820992749999860 ) ) ;
#31074 = EDGE_CURVE ( 'NONE', #18799, #34669, #39580, .T. ) ;
#31075 = CARTESIAN_POINT ( 'NONE',  ( 1.250000000000000000, -18.75000000000000000, -12.50000000000000000 ) ) ;
#31076 = CARTESIAN_POINT ( 'NONE',  ( 11.00000000000000000, -77.34999999999999432, 0.000000000000000000 ) ) ;
#31077 = CARTESIAN_POINT ( 'NONE',  ( -2.065394024360999836, -60.22161432612999477, 12.82193048530000112 ) ) ;
#31078 = LINE ( 'NONE', #40551, #9675 ) ;
#31079 = CIRCLE ( 'NONE', #35815, 9.199999999999999289 ) ;
#31080 = CARTESIAN_POINT ( 'NONE',  ( 4.045881407263999918, -84.06599735065199752, 1.029778334665000017 ) ) ;
#31081 = DIRECTION ( 'NONE',  ( 1.000000000000000000, 0.000000000000000000, 0.000000000000000000 ) ) ;
#31082 = CARTESIAN_POINT ( 'NONE',  ( 9.101979256333937229, -77.14561836503926884, -8.015291124465097283 ) ) ;
#31083 = CARTESIAN_POINT ( 'NONE',  ( -5.417662631175000243, -78.99125755395999704, 11.58939433055000023 ) ) ;
#31084 = EDGE_CURVE ( 'NONE', #35308, #15664, #3857, .T. ) ;
#31085 = CARTESIAN_POINT ( 'NONE',  ( 0.2665495375979999859, -78.40347427100999766, -11.25891151133000001 ) ) ;
#31086 = CARTESIAN_POINT ( 'NONE',  ( 0.1378349583326383687, -81.96685064740351834, 1.242146068417951499 ) ) ;
#31087 = CARTESIAN_POINT ( 'NONE',  ( 0.1658659358825000096, -77.75907607421000023, 1.418096705561000093 ) ) ;
#31088 = CARTESIAN_POINT ( 'NONE',  ( -0.5065222552852000071, -77.26962377378099234, 9.658707080791000266 ) ) ;
#31089 = CARTESIAN_POINT ( 'NONE',  ( -0.1834284358448134977, -82.86537657464923257, -1.499716752024290889 ) ) ;
#31090 = CARTESIAN_POINT ( 'NONE',  ( -12.44180635032999938, -60.89260544892000127, 1.459447571596000026 ) ) ;
#31091 = CARTESIAN_POINT ( 'NONE',  ( 2.105548162849785854, -80.24105674942582311, -10.54154672537324267 ) ) ;
#31092 = CARTESIAN_POINT ( 'NONE',  ( 0.000000000000000000, -76.89999999999999147, 0.000000000000000000 ) ) ;
#31093 = CARTESIAN_POINT ( 'NONE',  ( 10.05842956770407604, -79.06342084472876763, -4.964836713854746009 ) ) ;
#31094 = CARTESIAN_POINT ( 'NONE',  ( 1.166166863406513210, -81.82083417477375065, -0.4499332933408479729 ) ) ;
#31095 = CARTESIAN_POINT ( 'NONE',  ( 0.000000000000000000, -79.79999999999999716, 0.000000000000000000 ) ) ;
#31096 = CARTESIAN_POINT ( 'NONE',  ( -9.674930971187000850, -79.34977615539300189, 5.536272326541999078 ) ) ;
#31097 = CARTESIAN_POINT ( 'NONE',  ( 7.342377162853147787, -55.56980390652891799, 8.190817883596530180 ) ) ;
#31098 = VERTEX_POINT ( 'NONE', #43160 ) ;
#31099 = VERTEX_POINT ( 'NONE', #57877 ) ;
#31100 = AXIS2_PLACEMENT_3D ( 'NONE', #27851, #5428, #55908 ) ;
#31101 = CARTESIAN_POINT ( 'NONE',  ( 12.50000000000000000, -60.04999999966999980, 1.250000000000000000 ) ) ;
#31102 = VERTEX_POINT ( 'NONE', #49029 ) ;
#31103 = ORIENTED_EDGE ( 'NONE', *, *, #39099, .T. ) ;
#31104 = CARTESIAN_POINT ( 'NONE',  ( 0.1963495408493571015, -78.36458333333328596, 1.500000000000000444 ) ) ;
#31105 = CARTESIAN_POINT ( 'NONE',  ( -6.103876716051000351, -79.56279398642399769, 9.189364690594999274 ) ) ;
#31106 = CARTESIAN_POINT ( 'NONE',  ( -0.4356486348715999934, -24.88064955810000001, -12.43591427121000237 ) ) ;
#31107 = CARTESIAN_POINT ( 'NONE',  ( -3.888947658978999744, -79.05095254773289071, -0.7626656263158999582 ) ) ;
#31108 = CARTESIAN_POINT ( 'NONE',  ( 1.400971506258957167, -79.26317057520080311, 9.396169613821864885 ) ) ;
#31109 = ORIENTED_EDGE ( 'NONE', *, *, #57827, .F. ) ;
#31110 = DIRECTION ( 'NONE',  ( 1.158066155992000047E-14, 0.000000000000000000, -1.000000000000000000 ) ) ;
#31111 = CARTESIAN_POINT ( 'NONE',  ( 6.740316367734999758, -78.83471566304000078, 10.35856724650999894 ) ) ;
#31112 = ORIENTED_EDGE ( 'NONE', *, *, #56593, .T. ) ;
#31113 = EDGE_LOOP ( 'NONE', ( #33144, #29710, #53238, #33075 ) ) ;
#31114 = CARTESIAN_POINT ( 'NONE',  ( 6.668756384172233709, -79.48666666666666458, -6.812569087104355603 ) ) ;
#31115 = EDGE_CURVE ( 'NONE', #3607, #42830, #50230, .T. ) ;
#31116 = CARTESIAN_POINT ( 'NONE',  ( -0.9102058945833000347, -80.70043851714099503, 0.9747214924314999696 ) ) ;
#31117 = AXIS2_PLACEMENT_3D ( 'NONE', #48853, #53869, #26110 ) ;
#31118 = CARTESIAN_POINT ( 'NONE',  ( -3.536681740116999872, -78.11423136717898785, 9.036735673663999435 ) ) ;
#31119 = CIRCLE ( 'NONE', #13214, 13.89999999999999858 ) ;
#31120 = CARTESIAN_POINT ( 'NONE',  ( -3.622867166186615417, -86.09999999999976694, 1.695533395769283080 ) ) ;
#31121 = CARTESIAN_POINT ( 'NONE',  ( 2.038851226788696458, -85.88796493201749627, 2.830303225609521078 ) ) ;
#31122 = CARTESIAN_POINT ( 'NONE',  ( -9.767718346792999995, -78.45544818976000556, 7.129174073149000534 ) ) ;
#31123 = EDGE_CURVE ( 'NONE', #18435, #30464, #10816, .T. ) ;
#31124 = CARTESIAN_POINT ( 'NONE',  ( -12.60796396291999955, -77.75016851287999486, -0.9189346901731000328 ) ) ;
#31125 = CARTESIAN_POINT ( 'NONE',  ( 6.220862042517180335, -77.86622231854060772, 6.858636509587040742 ) ) ;
#31126 = CARTESIAN_POINT ( 'NONE',  ( 8.485281374238999419, -60.04999999966999980, 8.485281374238999419 ) ) ;
#31127 = CARTESIAN_POINT ( 'NONE',  ( 3.459248248861000352, -79.77631457584399755, 2.256571552193000318 ) ) ;
#31128 = CYLINDRICAL_SURFACE ( 'NONE', #12011, 0.6000000000000008660 ) ;
#31129 = CARTESIAN_POINT ( 'NONE',  ( -8.556714653534148951, -76.76008902517540378, -8.154008032208290402 ) ) ;
#31130 = CARTESIAN_POINT ( 'NONE',  ( 0.4737152913811000232, -79.05050264934789084, -3.512914691605000250 ) ) ;
#31131 = DIRECTION ( 'NONE',  ( -1.000000000000000000, 0.000000000000000000, 0.000000000000000000 ) ) ;
#31132 = DIRECTION ( 'NONE',  ( 0.000000000000000000, -1.000000000000000000, 9.256484467811999056E-14 ) ) ;
#31133 = CARTESIAN_POINT ( 'NONE',  ( 2.113064247614999669, -3.489169774745999764, -3.165785623842000351 ) ) ;
#31134 = CARTESIAN_POINT ( 'NONE',  ( -1.274005267229903593, -80.24673294587803696, 0.05895105347379184929 ) ) ;
#31135 = ORIENTED_EDGE ( 'NONE', *, *, #2786, .T. ) ;
#31136 = CARTESIAN_POINT ( 'NONE',  ( 0.3116081091750318444, -23.68684619778880673, 10.99615594221777215 ) ) ;
#31137 = DIRECTION ( 'NONE',  ( 1.000000000000000000, 0.000000000000000000, 0.000000000000000000 ) ) ;
#31138 = CARTESIAN_POINT ( 'NONE',  ( -0.5935892672256000147, -82.04604609890299116, 1.194249225580000129 ) ) ;
#31139 = CONICAL_SURFACE ( 'NONE', #24605, 12.84999999995999964, 0.7853981633972997312 ) ;
#31140 = B_SPLINE_CURVE_WITH_KNOTS ( 'NONE', 3,
 ( #57206, #38907, #7047, #16486, #30324, #7903, #12052, #25905, #3476, #21482, #39489, #57490, #53070, #12619, #30616, #17934 ),
 .UNSPECIFIED., .F., .F.,
 ( 4, 2, 2, 2, 2, 2, 2, 4 ),
 ( 0.000000000000000000, 0.2500000000000038303, 0.3750000000000026090, 0.4375000000000021094, 0.5000000000000015543, 0.6250000000000005551, 0.7499999999999995559, 1.000000000000000000 ),
 .UNSPECIFIED. ) ;
#31141 = CARTESIAN_POINT ( 'NONE',  ( -12.54673279573000144, -17.17202488779000191, -0.9078290272348999990 ) ) ;
#31142 = CARTESIAN_POINT ( 'NONE',  ( 12.51033564907000084, -78.24514168465999830, -3.582046052171000028 ) ) ;
#31143 = CARTESIAN_POINT ( 'NONE',  ( -2.335995526795000110, -79.61238667140099778, -9.341389049788000776 ) ) ;
#31144 = CARTESIAN_POINT ( 'NONE',  ( 12.69616050747999836, -20.24828923609000242, -1.799475304559999822 ) ) ;
#31145 = EDGE_LOOP ( 'NONE', ( #18304, #22612, #57417, #27432 ) ) ;
#31146 = CARTESIAN_POINT ( 'NONE',  ( -13.94241845804000057, -69.26002936526001008, -4.312607201944000624E-05 ) ) ;
#31147 = FACE_OUTER_BOUND ( 'NONE', #3270, .T. ) ;
#31148 = EDGE_CURVE ( 'NONE', #39698, #34245, #26249, .T. ) ;
#31149 = CARTESIAN_POINT ( 'NONE',  ( -0.9700586308955000403, -81.80063324571399619, -0.8813666596095000028 ) ) ;
#31150 = CARTESIAN_POINT ( 'NONE',  ( -2.062502994258999856, -21.75648180056000314, -12.92181194095000052 ) ) ;
#31151 = AXIS2_PLACEMENT_3D ( 'NONE', #43181, #51755, #11020 ) ;
#31152 = CARTESIAN_POINT ( 'NONE',  ( 8.959721679174998954, -77.67945172698098588, -3.223936051704999972 ) ) ;
#31153 = EDGE_CURVE ( 'NONE', #5887, #4102, #53778, .T. ) ;
#31155 = CARTESIAN_POINT ( 'NONE',  ( -3.754890333716000228, -1.276863097741000042, -1.424957469106999941 ) ) ;
#31154 = CARTESIAN_POINT ( 'NONE',  ( -3.379256011433000140, -85.86543811554798822, 2.374592366029999901 ) ) ;
#31156 = CARTESIAN_POINT ( 'NONE',  ( -1.092232985442824100, -82.45833333333330017, 0.6295237254636200097 ) ) ;
#31157 = CARTESIAN_POINT ( 'NONE',  ( -1.290198984414000050, -80.63668858139899953, -0.5875878301326999953 ) ) ;
#31158 = EDGE_LOOP ( 'NONE', ( #19367, #34508, #39689, #13989 ) ) ;
#31159 = CARTESIAN_POINT ( 'NONE',  ( -4.684264787344456948, -77.18914283860964076, -9.675737980290284312 ) ) ;
#31160 = CARTESIAN_POINT ( 'NONE',  ( 9.404538367153106648, -79.10366911081999319, 7.521839627124906613 ) ) ;
#31161 = VECTOR ( 'NONE', #45394, 1000.000000000000000 ) ;
#31162 = CARTESIAN_POINT ( 'NONE',  ( 1.358304078313203656, -78.93004670938226752, -3.649112436916695401 ) ) ;
#31163 = EDGE_LOOP ( 'NONE', ( #57066, #2607, #16976, #27115 ) ) ;
#31164 = EDGE_LOOP ( 'NONE', ( #51636, #47422, #13636, #26678 ) ) ;
#31165 = CARTESIAN_POINT ( 'NONE',  ( 0.2605153439964000284, -79.49770874343499827, -10.93709047653000077 ) ) ;
#31166 = CARTESIAN_POINT ( 'NONE',  ( -11.45718701969090070, -76.06302083320471752, -3.078158446385449665 ) ) ;
#31167 = CARTESIAN_POINT ( 'NONE',  ( 7.000000000000000000, -80.99999999999998579, 0.000000000000000000 ) ) ;
#31168 = VERTEX_POINT ( 'NONE', #40752 ) ;
#31169 = CARTESIAN_POINT ( 'NONE',  ( 2.713377469415999776, -77.83421086662899313, -11.74024507335000145 ) ) ;
#31170 = ORIENTED_EDGE ( 'NONE', *, *, #44498, .T. ) ;
#31171 = ORIENTED_EDGE ( 'NONE', *, *, #37817, .T. ) ;
#31172 = CARTESIAN_POINT ( 'NONE',  ( 7.356278612544861595, -60.10416868444998784, 8.178338515874330028 ) ) ;
#31173 = EDGE_CURVE ( 'NONE', #9948, #41659, #29689, .T. ) ;
#31174 = CARTESIAN_POINT ( 'NONE',  ( -12.00166164432143923, -76.40995231629973716, -1.570587690725778085 ) ) ;
#31175 = CARTESIAN_POINT ( 'NONE',  ( 2.630134112433684113, -1.666103305045204319, 3.040499453435629995 ) ) ;
#31176 = ORIENTED_EDGE ( 'NONE', *, *, #8069, .F. ) ;
#31177 = CARTESIAN_POINT ( 'NONE',  ( 11.00000000000000178, -18.25000000000000355, 0.1607611550154312841 ) ) ;
#31178 = ORIENTED_EDGE ( 'NONE', *, *, #17446, .T. ) ;
#31179 = CARTESIAN_POINT ( 'NONE',  ( -0.7340933969682582605, -79.57407930420207265, 1.041093327151733305 ) ) ;
#31180 = DIRECTION ( 'NONE',  ( 0.000000000000000000, 0.000000000000000000, -1.000000000000000000 ) ) ;
#31181 = B_SPLINE_CURVE_WITH_KNOTS ( 'NONE', 3,
 ( #44957, #57942, #116, #48801, #8061, #40816, #34908, #8347, #18094, #53514, #39926, #52940, #26056, #54107, #3632, #21636, #8642, #35192 ),
 .UNSPECIFIED., .F., .F.,
 ( 4, 2, 2, 2, 2, 2, 2, 2, 4 ),
 ( 0.000000000000000000, 0.1250000000000000278, 0.2500000000000000555, 0.3750000000000001665, 0.5000000000000001110, 0.6250000000000001110, 0.7500000000000002220, 0.8750000000000001110, 1.000000000000000000 ),
 .UNSPECIFIED. ) ;
#31182 = DIRECTION ( 'NONE',  ( -1.000000000000000000, 0.000000000000000000, 0.000000000000000000 ) ) ;
#31183 = CARTESIAN_POINT ( 'NONE',  ( 7.247844507162001015, -18.75000000000000000, 9.722718241315000398 ) ) ;
#31184 = CARTESIAN_POINT ( 'NONE',  ( 11.37984331015203487, -77.42617268424514521, -3.047297811426050718 ) ) ;
#31185 = ADVANCED_FACE ( 'NONE', ( #40158 ), #58170, .F. ) ;
#31186 = DIRECTION ( 'NONE',  ( 4.222607431054999479E-09, 0.9999999999999998890, -1.485891339405999759E-08 ) ) ;
#31187 = CARTESIAN_POINT ( 'NONE',  ( -8.557169117579000783, -77.71168682925997473, -8.383968101560002495 ) ) ;
#31188 = CARTESIAN_POINT ( 'NONE',  ( 9.599999999916001059, -87.30000000008399752, -6.531555804621000072E-10 ) ) ;
#31189 = CARTESIAN_POINT ( 'NONE',  ( -9.523353692535000192, -24.81947015623000041, 8.220363114681999761 ) ) ;
#31190 = CARTESIAN_POINT ( 'NONE',  ( -10.23602166438972638, -76.87166118683381910, 3.794243155524493982 ) ) ;
#31191 = TOROIDAL_SURFACE ( 'NONE', #7662, 1.250000000000000000, 0.5000000000000000000 ) ;
#31192 = CARTESIAN_POINT ( 'NONE',  ( -2.067319464631000248, -79.96130496681199418, 3.624396850766999911 ) ) ;
#31193 = CARTESIAN_POINT ( 'NONE',  ( 3.145085892150000006, -77.47146001420199468, -9.358399194681000566 ) ) ;
#31194 = CARTESIAN_POINT ( 'NONE',  ( -12.54980553589999914, -16.95222688865000293, -0.05649961219507999843 ) ) ;
#31195 = CARTESIAN_POINT ( 'NONE',  ( 10.99999999999999645, -77.86041666666663730, 1.439896632895345974 ) ) ;
#31196 = CARTESIAN_POINT ( 'NONE',  ( -9.500000000000000000, -78.79999999999999716, 0.000000000000000000 ) ) ;
#31197 = CARTESIAN_POINT ( 'NONE',  ( 1.252145818528037857, -81.52670456029824209, 0.4338495457226560492 ) ) ;
#31198 = CARTESIAN_POINT ( 'NONE',  ( -12.54435915808567970, -60.32412882177197844, -1.733925320397640357 ) ) ;
#31199 = CARTESIAN_POINT ( 'NONE',  ( 3.950759981329000414, -1.627363918999999992, -0.2034811876873000025 ) ) ;
#31200 = CARTESIAN_POINT ( 'NONE',  ( 8.395992668097999712, -79.43960095943374711, 4.560928606276999808 ) ) ;
#31201 = B_SPLINE_CURVE_WITH_KNOTS ( 'NONE', 3,
 ( #33175, #51221, #10774, #6620, #46802, #24344, #20209, #15483, #2209, #38200 ),
 .UNSPECIFIED., .F., .F.,
 ( 4, 2, 2, 2, 4 ),
 ( 0.000000000000000000, 0.09375005742280677346, 0.1875001148456135469, 0.2812501722684203065, 0.3750002296912270938 ),
 .UNSPECIFIED. ) ;
#31202 = CARTESIAN_POINT ( 'NONE',  ( -1.092633038097045262, -80.78858985991051611, 1.044221283387572807 ) ) ;
#31203 = CARTESIAN_POINT ( 'NONE',  ( -0.4442664572140017087, -78.50400959573080684, 1.174863755326367221 ) ) ;
#31204 = FACE_OUTER_BOUND ( 'NONE', #36218, .T. ) ;
#31205 = DIRECTION ( 'NONE',  ( 0.000000000000000000, 0.000000000000000000, -1.000000000000000000 ) ) ;
#31206 = CARTESIAN_POINT ( 'NONE',  ( -2.127308605635999772, -78.13598375397499751, -10.70747048031000048 ) ) ;
#31207 = CARTESIAN_POINT ( 'NONE',  ( 8.990136242696999958, -78.68304436543799341, 8.365012251980999736 ) ) ;
#31208 = CARTESIAN_POINT ( 'NONE',  ( 1.310679582531385279, -80.79166666666667140, 0.7554284705563519831 ) ) ;
#31209 = CARTESIAN_POINT ( 'NONE',  ( -9.393203674808267678, -79.04166666666665719, -5.413904038987171319 ) ) ;
#31211 = CARTESIAN_POINT ( 'NONE',  ( 1.240545393080999981, -79.00709889550499554, -0.6863720704128000172 ) ) ;
#31210 = CARTESIAN_POINT ( 'NONE',  ( -5.000000000000000000, -75.19999999999998863, 0.000000000000000000 ) ) ;
#31212 = CARTESIAN_POINT ( 'NONE',  ( -0.8340143124269999708, -81.28758988526999474, -1.348286063383000055 ) ) ;
#31213 = B_SPLINE_CURVE_WITH_KNOTS ( 'NONE', 3,
 ( #17652, #9092, #31501, #48950, #13508, #49547, #49242, #27081, #31801, #4063, #4671, #40682, #54266, #22067, #35640, #31203, #49844, #9390, #22964, #40974, #18543, #36535, #54559, #11372, #6344, #10789, #15789, #47108, #11086, #42657, #1646, #29065, #56524, #6639, #6927, #15200, #42952, #11943, #42372, #29636, #24645, #24359, #19933, #19635, #16371, #1940, #16083, #2224, #38509, #20791, #29921, #34063, #34352, #47688, #33490, #29349, #52389, #37923, #38794, #52101, #20226, #42076, #20512, #55948, #51237, #51529, #47971, #38217, #15498, #28769, #7216, #56239, #33777, #7508, #11659, #56814, #51817, #47395 ),
 .UNSPECIFIED., .F., .F.,
 ( 4, 2, 2, 2, 2, 2, 2, 2, 2, 2, 2, 2, 1, 1, 1, 2, 2, 2, 2, 2, 1, 2, 2, 2, 2, 2, 2, 1, 2, 2, 2, 2, 2, 2, 2, 1, 2, 2, 2, 2, 2, 4 ),
 ( 0.000000000000000000, 0.1249999999998231415, 0.1874999999997343791, 0.2187499999996899980, 0.2343749999996676270, 0.2421874999996563860, 0.2499999999996451727, 0.3124999999995554667, 0.3749999999994657607, 0.4374999999993760547, 0.4687499999993312016, 0.4843749999993087196, 0.4921874999992975064, 0.4960937499992897348, 0.4980468749992857935, 0.4990234374992869038, 0.4999999999992880140, 0.5624999999993739452, 0.5937499999994173550, 0.6015624999994276800, 0.6093749999994378941, 0.6249999999994585442, 0.6874999999995418110, 0.7031249999995625721, 0.7187499999995833333, 0.7343749999996040945, 0.7382812499996094235, 0.7421874999996148636, 0.7499999999996260769, 0.7812499999996731503, 0.8124999999997201128, 0.8437499999997671862, 0.8749999999998142597, 0.8906249999998374633, 0.8945312499998431255, 0.8984374999998487876, 0.9062499999998611111, 0.9374999999999086286, 0.9453124999999201750, 0.9531249999999316103, 0.9687499999999545919, 1.000000000000000000 ),
 .UNSPECIFIED. ) ;
#31214 = EDGE_LOOP ( 'NONE', ( #19893, #51770, #56810, #43026 ) ) ;
#31215 = CARTESIAN_POINT ( 'NONE',  ( -3.015791237393999680, -83.35221544543098560, 2.239724409143000194 ) ) ;
#31216 = CARTESIAN_POINT ( 'NONE',  ( -2.822678701150000080, -79.01742403547800109, 11.58741885751999945 ) ) ;
#31217 = CARTESIAN_POINT ( 'NONE',  ( 9.902297125457000249, -80.85282200469704605, -5.173806094917000387 ) ) ;
#31218 = LINE ( 'NONE', #27682, #43590 ) ;
#31219 = CARTESIAN_POINT ( 'NONE',  ( -1.750000000000000000, -76.29999999999999716, 0.5000000000000000000 ) ) ;
#31220 = CARTESIAN_POINT ( 'NONE',  ( -7.849238557987999521, -76.77212468491599395, 7.706455349885999340 ) ) ;
#31221 = CARTESIAN_POINT ( 'NONE',  ( -10.15831671673000081, -61.01991983010999832, 7.756223511098000678 ) ) ;
#31222 = CARTESIAN_POINT ( 'NONE',  ( -4.491587152465999822, -78.91604404360498393, -8.642068059767000321 ) ) ;
#31223 = CARTESIAN_POINT ( 'NONE',  ( 1.500000000000000000, -79.75000000000000000, 0.000000000000000000 ) ) ;
#31224 = CARTESIAN_POINT ( 'NONE',  ( -12.50000000000000000, -23.24999999688999708, -1.750000000000000000 ) ) ;
#31225 = CARTESIAN_POINT ( 'NONE',  ( -11.89999999977000122, -18.84999999999999787, 0.000000000000000000 ) ) ;
#31226 = CARTESIAN_POINT ( 'NONE',  ( -2.062597299672999540, -59.58485473249000108, 12.87022657274000004 ) ) ;
#31227 = EDGE_LOOP ( 'NONE', ( #17394, #17462, #4439, #56783 ) ) ;
#31228 = LINE ( 'NONE', #26232, #22943 ) ;
#31229 = CARTESIAN_POINT ( 'NONE',  ( -1.863129461298999923, -79.73813998579800000, -9.025265489830999854 ) ) ;
#31230 = LINE ( 'NONE', #49271, #15818 ) ;
#31231 = CARTESIAN_POINT ( 'NONE',  ( -10.21381326473999884, -59.57129148919000272, -7.668949790015999746 ) ) ;
#31232 = CARTESIAN_POINT ( 'NONE',  ( 0.4771943503223999850, -80.53694300351999402, -1.596102929133000004 ) ) ;
#31233 = ORIENTED_EDGE ( 'NONE', *, *, #22348, .T. ) ;
#31234 = CARTESIAN_POINT ( 'NONE',  ( -4.420137786970999905, -77.33677356148098170, 10.18371445122000019 ) ) ;
#31235 = VECTOR ( 'NONE', #32294, 1000.000000000000000 ) ;
#31236 = CARTESIAN_POINT ( 'NONE',  ( -9.722718241315000398, -23.25000000000000000, -7.954951288349001004 ) ) ;
#31237 = CARTESIAN_POINT ( 'NONE',  ( -3.250000000000001332, -1.010416666666666963, -0.4254240051736181139 ) ) ;
#31238 = VERTEX_POINT ( 'NONE', #18028 ) ;
#31239 = EDGE_CURVE ( 'NONE', #13029, #6729, #36020, .T. ) ;
#31240 = CARTESIAN_POINT ( 'NONE',  ( -7.631896578914999729, -55.57877526445999905, -10.36221705163000095 ) ) ;
#31241 =( NAMED_UNIT ( * ) PLANE_ANGLE_UNIT ( ) SI_UNIT ( $, .RADIAN. ) );
#31242 = CARTESIAN_POINT ( 'NONE',  ( 9.630577183392999174, -79.03317930548099923, 1.628483183780000010 ) ) ;
#31243 = VERTEX_POINT ( 'NONE', #13584 ) ;
#31244 = ORIENTED_EDGE ( 'NONE', *, *, #12890, .T. ) ;
#31245 = CARTESIAN_POINT ( 'NONE',  ( -12.12874067409000034, -76.61293033130499452, 1.606456333463999853 ) ) ;
#31246 = FACE_OUTER_BOUND ( 'NONE', #43120, .T. ) ;
#31247 = CARTESIAN_POINT ( 'NONE',  ( 0.8811371538135999160, -78.88031886790999181, -1.256732680173000105 ) ) ;
#31248 = VERTEX_POINT ( 'NONE', #49624 ) ;
#31249 = CARTESIAN_POINT ( 'NONE',  ( -2.712012240502000182, -77.58820584965398837, 9.099584490865000319 ) ) ;
#31250 = CARTESIAN_POINT ( 'NONE',  ( -9.627143703009355846, -78.33986286729894744, 1.221446647086100734 ) ) ;
#31251 = CARTESIAN_POINT ( 'NONE',  ( 0.1620520141055530050, -80.23568876084854651, -1.239762908316072387 ) ) ;
#31252 = CARTESIAN_POINT ( 'NONE',  ( -12.91626791057999846, -77.58770759395000027, -1.016208772393999871 ) ) ;
#31253 = CARTESIAN_POINT ( 'NONE',  ( 2.854969924326999919, -78.10452062854089661, 10.84745395575999893 ) ) ;
#31255 = ADVANCED_FACE ( 'NONE', ( #15345 ), #35615, .F. ) ;
#31254 = CARTESIAN_POINT ( 'NONE',  ( -8.000000000000000000, -81.19999999999998863, 0.000000000000000000 ) ) ;
#31256 = CARTESIAN_POINT ( 'NONE',  ( 1.558396630254053949, -86.31452044229999387, 3.590921352246257747 ) ) ;
#31257 = CARTESIAN_POINT ( 'NONE',  ( -8.286771986066998608, -78.84283200047998719, 7.559597915363999832 ) ) ;
#31258 = CARTESIAN_POINT ( 'NONE',  ( 8.698361121289734044, -79.87801218299412653, 3.168218995563596430 ) ) ;
#31259 = CARTESIAN_POINT ( 'NONE',  ( 4.505934350724444926, -80.10858973450639553, -10.15323451728369797 ) ) ;
#31260 = EDGE_LOOP ( 'NONE', ( #27272, #37339, #18802, #16333 ) ) ;
#31261 = CARTESIAN_POINT ( 'NONE',  ( -0.5065222552852000071, -77.12916933416629206, 9.658707080791000266 ) ) ;
#31262 = CARTESIAN_POINT ( 'NONE',  ( 10.54796701376999835, -75.84510257978999448, 6.346365727669000201 ) ) ;
#31263 = CARTESIAN_POINT ( 'NONE',  ( -1.527286180810999872, -79.42060648544099877, -0.2382966983378000114 ) ) ;
#31264 = CARTESIAN_POINT ( 'NONE',  ( 3.529139221787363390, -2.612568796686050909, 0.6082355383969471063 ) ) ;
#31265 = CARTESIAN_POINT ( 'NONE',  ( -8.266608573609707022, -17.02766203690127966, 9.697383820329660509 ) ) ;
#31266 = EDGE_CURVE ( 'NONE', #25387, #10013, #31536, .T. ) ;
#31267 = CARTESIAN_POINT ( 'NONE',  ( -7.650089724727000551, -76.77316923444898578, -9.607224057717001386 ) ) ;
#31268 = CARTESIAN_POINT ( 'NONE',  ( 0.000000000000000000, -78.00000000000000000, -7.200000000000000178 ) ) ;
#31269 = CARTESIAN_POINT ( 'NONE',  ( -10.30593458266999995, -78.58823118367698157, -4.275431210322000020 ) ) ;
#31270 = CARTESIAN_POINT ( 'NONE',  ( 1.761422869556999782, -77.51881498579798802, -9.576527127505000792 ) ) ;
#31271 = CARTESIAN_POINT ( 'NONE',  ( 6.487909909861338420, -77.22037378120354845, -10.11762090100198819 ) ) ;
#31272 = CARTESIAN_POINT ( 'NONE',  ( 0.000000000000000000, -76.75499999999999545, 0.000000000000000000 ) ) ;
#31273 = CARTESIAN_POINT ( 'NONE',  ( -9.945248159053452497, -76.00840104940344588, -8.414435792164686845 ) ) ;
#31274 = EDGE_CURVE ( 'NONE', #28197, #26455, #21347, .T. ) ;
#31275 = CARTESIAN_POINT ( 'NONE',  ( 1.249999996278000181, -76.50000000037098857, 0.4999999996289999915 ) ) ;
#31276 = ORIENTED_EDGE ( 'NONE', *, *, #43462, .F. ) ;
#31277 = CARTESIAN_POINT ( 'NONE',  ( 0.3489451476548999787, -81.60074910037999985, -1.426530384489999914 ) ) ;
#31278 = CARTESIAN_POINT ( 'NONE',  ( -0.7224186015757000368, -79.59438689399999589, -0.9790252285018000711 ) ) ;
#31279 = CARTESIAN_POINT ( 'NONE',  ( -1.384806900013862530, -80.53538967717265962, -0.6660020126448532585 ) ) ;
#31280 = AXIS2_PLACEMENT_3D ( 'NONE', #24339, #54751, #5736 ) ;
#31281 = CARTESIAN_POINT ( 'NONE',  ( -10.86788298907000083, -77.53287430722599538, -5.040355520269000245 ) ) ;
#31282 = CARTESIAN_POINT ( 'NONE',  ( 12.50000000000000000, -55.54999999966999980, 0.000000000000000000 ) ) ;
#31283 = AXIS2_PLACEMENT_3D ( 'NONE', #57036, #21592, #57601 ) ;
#31284 = CARTESIAN_POINT ( 'NONE',  ( -0.08487245167304000026, -78.45215651189698747, 11.93433278878999992 ) ) ;
#31285 = CARTESIAN_POINT ( 'NONE',  ( -5.600962501326000265, -77.93369415034599967, 7.948110234177999445 ) ) ;
#31286 = CARTESIAN_POINT ( 'NONE',  ( -0.4802748259363999739, -53.79473092685000069, -12.54896097830000024 ) ) ;
#31287 = CARTESIAN_POINT ( 'NONE',  ( 2.491388965909014708, -76.05772791729621929, 11.48290208440257665 ) ) ;
#31288 = CARTESIAN_POINT ( 'NONE',  ( -3.953505135776000046, -79.36303053380299843, 10.29910343295999908 ) ) ;
#31289 = CARTESIAN_POINT ( 'NONE',  ( -8.485281374238999419, 0.000000000000000000, -8.485281374238999419 ) ) ;
#31290 = VERTEX_POINT ( 'NONE', #24968 ) ;
#31291 = CARTESIAN_POINT ( 'NONE',  ( -7.342331066867000544, -59.94999999967000548, 8.190859204290999784 ) ) ;
#31292 = CARTESIAN_POINT ( 'NONE',  ( 8.342172210693000522, -79.14070433617399658, 8.687562991252999467 ) ) ;
#31293 = CARTESIAN_POINT ( 'NONE',  ( -3.444390624473300910, -78.62148120184446043, -1.946200917927131790 ) ) ;
#31295 = CARTESIAN_POINT ( 'NONE',  ( -6.528377880799854260, -76.27803772958627349, -9.769420381365502948 ) ) ;
#31294 = CARTESIAN_POINT ( 'NONE',  ( -13.94241847916999966, -46.33997059779999717, -4.312626734219999997E-05 ) ) ;
#31296 = CARTESIAN_POINT ( 'NONE',  ( 10.31626776183999894, -78.21273180413199100, -3.746764721243999841 ) ) ;
#31297 = CARTESIAN_POINT ( 'NONE',  ( 0.000000000000000000, -76.19999999999998863, 0.000000000000000000 ) ) ;
#31298 = EDGE_CURVE ( 'NONE', #45201, #15410, #42115, .T. ) ;
#31299 = CARTESIAN_POINT ( 'NONE',  ( -9.719066392145998989, -76.06110886216698930, -7.489235019707000340 ) ) ;
#31300 = CARTESIAN_POINT ( 'NONE',  ( -10.35238666240951844, -79.67168035550133709, 3.845238516216011870 ) ) ;
#31301 = CARTESIAN_POINT ( 'NONE',  ( -9.645974121302039350, -76.96251239198622329, 4.906691233381782702 ) ) ;
#31302 = ORIENTED_EDGE ( 'NONE', *, *, #25293, .F. ) ;
#31304 = AXIS2_PLACEMENT_3D ( 'NONE', #33209, #28494, #10809 ) ;
#31303 = CARTESIAN_POINT ( 'NONE',  ( 5.645478026989999343, -79.94337520226639526, -9.744872608167998607 ) ) ;
#31305 = CARTESIAN_POINT ( 'NONE',  ( 1.250000000000000000, -79.84999999999999432, 0.000000000000000000 ) ) ;
#31306 = CARTESIAN_POINT ( 'NONE',  ( -5.539808784079886195, -77.68333333333333712, -9.611650271896841957 ) ) ;
#31307 = DIRECTION ( 'NONE',  ( 1.000000000000000000, 0.000000000000000000, 0.000000000000000000 ) ) ;
#31308 = CARTESIAN_POINT ( 'NONE',  ( 11.05620287758999964, -79.48232667919899086, -1.500659051079999973 ) ) ;
#31309 = CARTESIAN_POINT ( 'NONE',  ( -9.358624512123094874, -76.45833333333334281, 5.407950800604276687 ) ) ;
#31310 = FACE_OUTER_BOUND ( 'NONE', #21325, .T. ) ;
#31311 = CARTESIAN_POINT ( 'NONE',  ( 11.07343986574985450, -76.91880255752919027, -4.079208564647556656 ) ) ;
#31312 = DIRECTION ( 'NONE',  ( 0.000000000000000000, 0.000000000000000000, -1.000000000000000000 ) ) ;
#31313 = DIRECTION ( 'NONE',  ( 1.194281197986999840E-10, 1.000000000000000000, 5.211300245735000371E-10 ) ) ;
#31314 = CARTESIAN_POINT ( 'NONE',  ( -12.74366183110831052, -60.32185227186467102, -1.980611001123811388 ) ) ;
#31315 =( LENGTH_UNIT ( ) NAMED_UNIT ( * ) SI_UNIT ( .MILLI., .METRE. ) );
#31316 = CARTESIAN_POINT ( 'NONE',  ( -12.43410103865999972, -24.44137177768999791, 1.192638008239000014 ) ) ;
#31317 = ORIENTED_EDGE ( 'NONE', *, *, #44317, .F. ) ;
#31318 = VERTEX_POINT ( 'NONE', #51276 ) ;
#31319 = CARTESIAN_POINT ( 'NONE',  ( 1.243547092045969915, -78.53541666666666288, -9.500000000000000000 ) ) ;
#31320 = AXIS2_PLACEMENT_3D ( 'NONE', #43426, #2414, #37830 ) ;
#31321 = ORIENTED_EDGE ( 'NONE', *, *, #58078, .T. ) ;
#31322 = CARTESIAN_POINT ( 'NONE',  ( 4.096584555840107278, -79.58967318748072728, 8.607303473720193665 ) ) ;
#31323 = VERTEX_POINT ( 'NONE', #34098 ) ;
#31324 = CARTESIAN_POINT ( 'NONE',  ( 9.963467980702999327, -23.68274967071999981, 7.659239661648999942 ) ) ;
#31325 = CARTESIAN_POINT ( 'NONE',  ( 8.150146600852352208, -55.38467666605773587, -7.387512494710277267 ) ) ;
#31327 = ADVANCED_FACE ( 'NONE', ( #33529 ), #36601, .F. ) ;
#31326 = CARTESIAN_POINT ( 'NONE',  ( 0.1639602171826417543, -82.46524421910949343, 1.249637490365603343 ) ) ;
#31328 = CARTESIAN_POINT ( 'NONE',  ( -6.347401566831289976, -78.16496885166350239, -6.728806251054260557 ) ) ;
#31329 = CIRCLE ( 'NONE', #46476, 1.750000000000001332 ) ;
#31330 = CARTESIAN_POINT ( 'NONE',  ( -9.066796825632000179, -78.74841171265799744, -6.603885667862000375 ) ) ;
#31331 = DIRECTION ( 'NONE',  ( -1.000000000000000000, 0.000000000000000000, 0.000000000000000000 ) ) ;
#31332 = ORIENTED_EDGE ( 'NONE', *, *, #20652, .T. ) ;
#31334 = ORIENTED_EDGE ( 'NONE', *, *, #24763, .T. ) ;
#31333 = EDGE_CURVE ( 'NONE', #31523, #3819, #12864, .T. ) ;
#31335 = CARTESIAN_POINT ( 'NONE',  ( 1.422220956165613170, -77.46272989785457241, 9.140013063714238939 ) ) ;
#31336 = CARTESIAN_POINT ( 'NONE',  ( -9.050627908549000011, -77.47867334415599316, -6.322205650057999726 ) ) ;
#31337 =( NAMED_UNIT ( * ) SI_UNIT ( $, .STERADIAN. ) SOLID_ANGLE_UNIT ( ) );
#31338 = CARTESIAN_POINT ( 'NONE',  ( 0.000000000000000000, -77.40000000000736691, -3.899999999992999733 ) ) ;
#31339 = CARTESIAN_POINT ( 'NONE',  ( 9.690463944985998168, -78.63622609373899763, -0.5153813127049999832 ) ) ;
#31340 = CIRCLE ( 'NONE', #23820, 0.5999999999999999778 ) ;
#31341 = CARTESIAN_POINT ( 'NONE',  ( 12.38384620286000093, -76.22877954592999572, -4.343081969281999299 ) ) ;
#31342 = CARTESIAN_POINT ( 'NONE',  ( -8.475401746435078820, -79.43728386678893116, -4.291540307597959902 ) ) ;
#31343 = LINE ( 'NONE', #4212, #35540 ) ;
#31344 = CARTESIAN_POINT ( 'NONE',  ( -11.11771682179999843, -80.47802048182499846, 1.751409206030000165 ) ) ;
#31345 = VECTOR ( 'NONE', #34069, 1000.000000000000000 ) ;
#31346 = CARTESIAN_POINT ( 'NONE',  ( 12.46164872708000004, -18.32834420040999746, -1.631615798668999862 ) ) ;
#31347 = CARTESIAN_POINT ( 'NONE',  ( -1.250000000000000000, -78.00000000000000000, 2.658254822585999717E-14 ) ) ;
#31348 = EDGE_CURVE ( 'NONE', #38883, #48634, #4197, .T. ) ;
#31349 = CARTESIAN_POINT ( 'NONE',  ( -11.17196203841501756, -76.67470515005034315, 3.660625636545362660 ) ) ;
#31350 = CARTESIAN_POINT ( 'NONE',  ( -1.472243751803000045, -82.87075447013299367, 3.224510409186000182 ) ) ;
#31351 = ORIENTED_EDGE ( 'NONE', *, *, #21756, .F. ) ;
#31352 = CARTESIAN_POINT ( 'NONE',  ( -5.714083337146000474, -78.85452609989098960, 10.91123161796000041 ) ) ;
#31353 = CARTESIAN_POINT ( 'NONE',  ( -10.37257800205000180, -76.67949600664098853, 3.987904220598999405 ) ) ;
#31354 = CARTESIAN_POINT ( 'NONE',  ( -6.916021889377625520, -78.03068784888290566, 8.229964326230533089 ) ) ;
#31355 = CARTESIAN_POINT ( 'NONE',  ( -5.687706977064000746, -78.04826182971200410, 10.54353137130999940 ) ) ;
#31356 = DIRECTION ( 'NONE',  ( 0.000000000000000000, 0.000000000000000000, 1.000000000000000000 ) ) ;
#31357 = DIRECTION ( 'NONE',  ( 0.000000000000000000, 1.000000000000000000, 0.000000000000000000 ) ) ;
#31358 = CARTESIAN_POINT ( 'NONE',  ( 3.308356911591999960, -86.39318692614399708, -1.472975398278999926 ) ) ;
#31359 = CARTESIAN_POINT ( 'NONE',  ( 10.35747158360999975, -55.48415522678000400, -7.626500902197000720 ) ) ;
#31360 = CARTESIAN_POINT ( 'NONE',  ( 9.252740428349003565, -78.52916666666668277, -2.486604901413146607 ) ) ;
#31361 = CARTESIAN_POINT ( 'NONE',  ( -7.800315838420999626, -76.82936687607200099, 7.658422569234000221 ) ) ;
#31362 = CARTESIAN_POINT ( 'NONE',  ( 7.374560639698954034, -78.12291666666664014, 9.596002108778181494 ) ) ;
#31363 = CARTESIAN_POINT ( 'NONE',  ( -2.879226727952121312, -80.09583333334906285, 10.71369944335146052 ) ) ;
#31364 = ORIENTED_EDGE ( 'NONE', *, *, #28267, .F. ) ;
#31365 = DIRECTION ( 'NONE',  ( 1.000000000000000000, -6.386278974555000074E-09, 1.411448851650999890E-10 ) ) ;
#31366 = CARTESIAN_POINT ( 'NONE',  ( 1.632307027713000069, -55.13072810409999391, 12.46200249210000166 ) ) ;
#31367 = DIRECTION ( 'NONE',  ( 0.000000000000000000, 1.000000000000000000, 0.000000000000000000 ) ) ;
#31368 = CARTESIAN_POINT ( 'NONE',  ( 0.7674396588794000218, -2.946116667230000097, -3.891291548070999973 ) ) ;
#31369 = CARTESIAN_POINT ( 'NONE',  ( 7.508079800428999917, -76.88167466538000383, -8.333477563431999968 ) ) ;
#31370 = AXIS2_PLACEMENT_3D ( 'NONE', #25498, #11079, #29059 ) ;
#31371 = CARTESIAN_POINT ( 'NONE',  ( 3.165411199172027512, -1.729166666666666519, -0.8506806241676553304 ) ) ;
#31372 = CARTESIAN_POINT ( 'NONE',  ( 10.89775144040313215, -77.33749999999999147, -1.727831697829316893 ) ) ;
#31373 = EDGE_CURVE ( 'NONE', #21042, #16896, #40504, .T. ) ;
#31374 = CARTESIAN_POINT ( 'NONE',  ( 0.000000000000000000, -75.19999999999998863, 0.000000000000000000 ) ) ;
#31375 = CARTESIAN_POINT ( 'NONE',  ( 12.61112375831999977, -18.78433928967000099, 1.798929377342999736 ) ) ;
#31376 = CARTESIAN_POINT ( 'NONE',  ( 4.129967680665999730, -85.64082450217398446, 0.04325065736083000267 ) ) ;
#31377 = CYLINDRICAL_SURFACE ( 'NONE', #11269, 10.75000000000000000 ) ;
#31378 = AXIS2_PLACEMENT_3D ( 'NONE', #48638, #56915, #39477 ) ;
#31379 = CARTESIAN_POINT ( 'NONE',  ( 12.50000000000000000, -55.55000000278000272, -1.750000000000000000 ) ) ;
#31380 = CARTESIAN_POINT ( 'NONE',  ( -10.31240102133999947, -78.61950547832000780, 7.304110959076998810 ) ) ;
#31381 = B_SPLINE_SURFACE_WITH_KNOTS ( 'NONE', 3, 3, ( 
 ( #42438, #27952, #33260, #46588 ),
 ( #1420, #20002, #15562, #23535 ),
 ( #24122, #41548, #28830, #19702 ),
 ( #10857, #37109, #47172, #14669 ),
 ( #11152, #46878, #6408, #32667 ),
 ( #6704, #10259, #43016, #48039 ),
 ( #29985, #7858, #24995, #20854 ),
 ( #2572, #7569, #53020, #12006 ),
 ( #44169, #52447, #25569, #34123 ),
 ( #3716, #3153, #21141, #56586 ),
 ( #43589, #38858, #2857, #34418 ),
 ( #38572, #56879, #16435, #33841 ),
 ( #7281, #39149, #25857, #51878 ),
 ( #16146, #11722, #11433, #8149 ),
 ( #12573, #21719, #29698, #43886 ),
 ( #17008, #57157, #29415, #57449 ),
 ( #39724, #16722, #34705, #25283 ) ),
 .UNSPECIFIED., .F., .F., .F.,
 ( 4, 1, 1, 1, 1, 1, 1, 1, 1, 1, 1, 1, 1, 1, 4 ),
 ( 4, 4 ),
 ( -0.01011400514355000058, 0.000000000000000000, 0.08333333333333001192, 0.1666666666667000196, 0.2500000000000000000, 0.3333333333333000081, 0.4166666666666999919, 0.5000000000000000000, 0.5833333333333000637, 0.6666666666667000474, 0.7500000000000000000, 0.8333333333333000637, 0.9166666666667000474, 1.000000000000000000, 1.010365328128000062 ),
 ( -0.3559705546945999832, 1.357612395640000136 ),
 .UNSPECIFIED. ) ;
#31382 = CARTESIAN_POINT ( 'NONE',  ( -8.674044796698000326, -76.65617272148499239, 6.768505387188000988 ) ) ;
#31383 = DIRECTION ( 'NONE',  ( 0.7071067811865969777, 0.7071067811864980568, 1.033971025369995989E-10 ) ) ;
#31384 = CARTESIAN_POINT ( 'NONE',  ( -1.514795774450999888, -78.36393822280000165, -0.6877011994091001279 ) ) ;
#31385 = CARTESIAN_POINT ( 'NONE',  ( 1.718598680008210700, -61.04962933004735959, 12.71111582771794701 ) ) ;
#31386 = CARTESIAN_POINT ( 'NONE',  ( 1.347270232873278406, -82.54148316382753592, 0.7639118359693641835 ) ) ;
#31387 = CARTESIAN_POINT ( 'NONE',  ( -12.83675988122999989, -60.02754371127999633, 2.062832873794000044 ) ) ;
#31388 = CARTESIAN_POINT ( 'NONE',  ( -3.353102485753966633, -80.20021897257370824, -10.21483153731809068 ) ) ;
#31389 = EDGE_CURVE ( 'NONE', #21891, #33033, #47421, .T. ) ;
#31390 = CARTESIAN_POINT ( 'NONE',  ( -5.747123378374999980, -78.61567021304000491, 10.24856442990000005 ) ) ;
#31391 = CARTESIAN_POINT ( 'NONE',  ( 10.89891958939809413, -79.58091136176375358, -2.652387744565959160 ) ) ;
#31392 = AXIS2_PLACEMENT_3D ( 'NONE', #6717, #12300, #43028 ) ;
#31393 = VECTOR ( 'NONE', #22537, 1000.000000000000000 ) ;
#31394 = CARTESIAN_POINT ( 'NONE',  ( 12.00000000000000000, -77.64999999999999147, 0.000000000000000000 ) ) ;
#31395 = CARTESIAN_POINT ( 'NONE',  ( 2.879226727952084897, -79.45416666666667993, 10.71369944335147295 ) ) ;
#31396 = CARTESIAN_POINT ( 'NONE',  ( 9.317996701405999005, -79.59490324240999826, -6.117968457212000111 ) ) ;
#31397 = DIRECTION ( 'NONE',  ( 0.000000000000000000, -1.000000000000000000, 0.000000000000000000 ) ) ;
#31398 = ORIENTED_EDGE ( 'NONE', *, *, #18627, .F. ) ;
#31399 = VERTEX_POINT ( 'NONE', #54089 ) ;
#31400 = CARTESIAN_POINT ( 'NONE',  ( 0.7536588245869000335, -81.65558647677399051, -1.428009912074000187 ) ) ;
#31401 = ORIENTED_EDGE ( 'NONE', *, *, #7408, .F. ) ;
#31402 = LINE ( 'NONE', #58289, #36788 ) ;
#31403 = ORIENTED_EDGE ( 'NONE', *, *, #2566, .T. ) ;
#31404 = CARTESIAN_POINT ( 'NONE',  ( 10.42531125070999920, -60.06485145371000556, -7.624341767111000756 ) ) ;
#31405 = CARTESIAN_POINT ( 'NONE',  ( 1.980584515752000119, -18.73514853375999678, 12.76303204602000108 ) ) ;
#31406 = DIRECTION ( 'NONE',  ( 0.000000000000000000, 0.000000000000000000, -1.000000000000000000 ) ) ;
#31407 = CARTESIAN_POINT ( 'NONE',  ( -0.4077927620925000385, -79.26319421340399174, -11.02431129116999919 ) ) ;
#31409 = EDGE_CURVE ( 'NONE', #12786, #22441, #388, .T. ) ;
#31408 = CARTESIAN_POINT ( 'NONE',  ( -0.8445585116435000428, -24.71040443242999984, -12.43380736237000050 ) ) ;
#31410 = CARTESIAN_POINT ( 'NONE',  ( 3.415484286716000017, -79.65220467013898542, -1.563917429438999918 ) ) ;
#31411 = CARTESIAN_POINT ( 'NONE',  ( 1.224189701827945287, -79.26463158461723424, 9.420864478166739886 ) ) ;
#31412 = CARTESIAN_POINT ( 'NONE',  ( 10.75000000000000000, -78.35000000000000853, 1.923335087985999915E-14 ) ) ;
#31413 = CARTESIAN_POINT ( 'NONE',  ( 6.659420128180999932, -78.74763481331000037, 10.23424531685000005 ) ) ;
#31414 = ORIENTED_EDGE ( 'NONE', *, *, #49397, .F. ) ;
#31416 = EDGE_CURVE ( 'NONE', #11901, #23950, #13639, .T. ) ;
#31415 = ORIENTED_EDGE ( 'NONE', *, *, #28885, .T. ) ;
#31417 = CARTESIAN_POINT ( 'NONE',  ( -4.582365512893316506, -76.99392094393498098, -11.13666644834476038 ) ) ;
#31418 = B_SPLINE_SURFACE_WITH_KNOTS ( 'NONE', 3, 3, ( 
 ( #22083, #40097, #17971, #9406, #58110, #27100, #17673, #53689, #31222, #22981, #40399, #49260, #53987, #8812, #45137, #35963, #4687, #26804, #13526, #31518, #49567, #9696, #9113, #22686, #291, #18270, #36262, #54285, #13822, #31821, #582, #33574, #1729, #29144, #47190, #15579, #11169, #19431, #2023, #32690, #50740, #33278, #6722, #28261, #51612, #24730, #32982, #28848, #42743, #55740, #14985, #15870, #46899, #33856, #2306, #38298, #6426, #24441, #20303, #42455, #23846, #20021, #55143, #6134, #51894, #38004, #56320 ),
 ( #19137, #56030, #10281, #27974, #46024, #55443, #5545, #37132, #51028, #46315, #24141, #23555, #14689, #10577, #5840, #41571, #1152, #15284, #41863, #19722, #51319, #37718, #1440, #37423, #28560, #46608, #10877, #42160, #34142, #38589, #3445, #20872, #52182, #21449, #16164, #3731, #2874, #17306, #16452, #48617, #34433, #11737, #12304, #57749, #38875, #56604, #29431, #39164, #44184, #43032, #7298, #29715, #26165, #21732, #47763, #8164, #11452, #39739, #57462, #20592, #17023, #43901, #52750, #30586, #35292, #30294, #39458 ),
 ( #47483, #48333, #7872, #7009, #25874, #25300, #35007, #43318, #48056, #25011, #53040, #2593, #16739, #56895, #52463, #12021, #12587, #30002, #7587, #25586, #43608, #3168, #21158, #57173, #34720, #49494, #27327, #44463, #40331, #53618, #45656, #50084, #40629, #41205, #27029, #18202, #45066, #8743, #13747, #35590, #4014, #22617, #224, #17601, #22020, #45361, #4314, #13156, #4910, #58041, #5198, #44765, #795, #58340, #32039, #17903, #31152, #54212, #18777, #22314, #40028, #12867, #36194, #27616, #26441, #49191, #26734 ),
 ( #35892, #9628, #53923, #4618, #13456, #48905, #53322, #31452, #23200, #9338, #9043, #40921, #22909, #54508, #31747, #49792, #510, #30869, #18486, #36479, #8445, #14045, #24371, #55368, #24070, #24661, #42383, #41498, #1953, #19947, #19646, #6649, #14912, #51540, #1083, #45948, #54787, #37935, #55076, #11097, #19070, #14623, #51250, #32326, #42670, #32615, #50666, #33504, #29077, #47122, #2238, #10209, #5769, #41791, #36769, #15211, #42087, #50373, #9920, #27901, #10504, #1656, #5479, #23485, #28188, #23776, #1363 ) ),
 .UNSPECIFIED., .F., .F., .F.,
 ( 4, 4 ),
 ( 4, 1, 1, 1, 1, 1, 1, 1, 1, 1, 1, 1, 1, 1, 1, 1, 1, 1, 1, 1, 1, 1, 1, 1, 1, 1, 1, 1, 1, 1, 1, 1, 1, 1, 1, 1, 1, 1, 1, 1, 1, 1, 1, 1, 1, 1, 1, 1, 1, 1, 1, 1, 1, 1, 1, 1, 1, 1, 1, 1, 1, 1, 1, 1, 4 ),
 ( -0.1387574078320000237, 1.138757407831999968 ),
 ( -0.02000000000000000042, -0.003749999999999999861, 0.01250000000000000069, 0.02875000000000000125, 0.04499999999999999833, 0.06124999999999999889, 0.07749999999999999944, 0.09375000000000000000, 0.1100000000000000006, 0.1262500000000000011, 0.1424999999999999878, 0.1587500000000000022, 0.1749999999999999889, 0.1912500000000000033, 0.2074999999999999900, 0.2237500000000000044, 0.2399999999999999911, 0.2562499999999999778, 0.2725000000000000200, 0.2887500000000000067, 0.3049999999999999933, 0.3212499999999999800, 0.3375000000000000222, 0.3537500000000000089, 0.3699999999999999956, 0.3862499999999999822, 0.4025000000000000244, 0.4187500000000000111, 0.4349999999999999978, 0.4512499999999999845, 0.4675000000000000266, 0.4837500000000000133, 0.5000000000000000000, 0.5162499999999999867, 0.5324999999999999734, 0.5487499999999999600, 0.5649999999999999467, 0.5812500000000000444, 0.5975000000000000311, 0.6137500000000000178, 0.6300000000000000044, 0.6462499999999999911, 0.6624999999999999778, 0.6787499999999999645, 0.6949999999999999512, 0.7112500000000000488, 0.7275000000000000355, 0.7437500000000000222, 0.7600000000000000089, 0.7762499999999999956, 0.7924999999999999822, 0.8087499999999999689, 0.8249999999999999556, 0.8412500000000000533, 0.8575000000000000400, 0.8737500000000000266, 0.8900000000000000133, 0.9062500000000000000, 0.9224999999999999867, 0.9387499999999999734, 0.9549999999999999600, 0.9712499999999999467, 0.9875000000000000444, 1.003749999999999920, 1.020000000000000018 ),
 .UNSPECIFIED. ) ;
#31419 = CARTESIAN_POINT ( 'NONE',  ( -1.980584515756000030, -60.06485150062000145, -12.76303204342999997 ) ) ;
#31420 = CARTESIAN_POINT ( 'NONE',  ( -7.203390125892000562, -78.76797943714498729, -6.502451851937000704 ) ) ;
#31421 = CARTESIAN_POINT ( 'NONE',  ( -4.623525823813485758, -86.09999999999976694, -0.4425863276891531251 ) ) ;
#31422 = FACE_BOUND ( 'NONE', #7003, .T. ) ;
#31423 = CARTESIAN_POINT ( 'NONE',  ( 11.74505801343999956, -76.70322811118001027, 5.470698999298999610 ) ) ;
#31424 = CARTESIAN_POINT ( 'NONE',  ( -0.7407245532275998912, -81.15447863951000329, -1.017507444502999903 ) ) ;
#31425 = CARTESIAN_POINT ( 'NONE',  ( 7.324086682717548591, -77.85317212802200970, 5.812447148214148207 ) ) ;
#31426 = EDGE_CURVE ( 'NONE', #52567, #20634, #11982, .T. ) ;
#31427 = CARTESIAN_POINT ( 'NONE',  ( -12.50000000000000000, -60.04999999966999980, 0.000000000000000000 ) ) ;
#31428 = CARTESIAN_POINT ( 'NONE',  ( 0.6604400869868999324, -77.13741167140099719, -9.497136025460999775 ) ) ;
#31429 = CARTESIAN_POINT ( 'NONE',  ( -2.265283964738999956, -80.73445849046999001, -3.251842360486000061 ) ) ;
#31430 = CARTESIAN_POINT ( 'NONE',  ( 10.07210119001000059, -80.55306440022908987, 5.045985883512999592 ) ) ;
#31431 = DIRECTION ( 'NONE',  ( -0.7071067811865474617, -0.7071067811865474617, -6.518272650013434745E-10 ) ) ;
#31432 = CARTESIAN_POINT ( 'NONE',  ( -0.5536213250151708065, -76.82071496306311076, -11.80762683626677401 ) ) ;
#31433 = CARTESIAN_POINT ( 'NONE',  ( 3.481401174418000011, -82.24559216449299015, -0.2294707599881000148 ) ) ;
#31434 = AXIS2_PLACEMENT_3D ( 'NONE', #4149, #40460, #51 ) ;
#31435 = CARTESIAN_POINT ( 'NONE',  ( -26.50000000000000000, -39.49523982883999906, -1.535553829236000105E-05 ) ) ;
#31436 = CARTESIAN_POINT ( 'NONE',  ( 1.500000000000000000, -79.75000000000000000, 0.000000000000000000 ) ) ;
#31437 = CARTESIAN_POINT ( 'NONE',  ( 0.2017531936662588510, -79.38804522922356455, -1.258586820450570798 ) ) ;
#31438 = AXIS2_PLACEMENT_3D ( 'NONE', #26510, #17678, #25942 ) ;
#31439 = VERTEX_POINT ( 'NONE', #47721 ) ;
#31440 = CARTESIAN_POINT ( 'NONE',  ( 12.00000000000000000, -18.84999999997999964, -0.7999999999999001243 ) ) ;
#31441 = CARTESIAN_POINT ( 'NONE',  ( -9.546819346760001324, -61.48527546573999558, 8.130850182904000079 ) ) ;
#31442 = CARTESIAN_POINT ( 'NONE',  ( 0.9432352957733999288, -81.99059486971999888, 0.9428059748164999698 ) ) ;
#31443 = CARTESIAN_POINT ( 'NONE',  ( -12.57354471038000021, -18.27622323986999930, -1.757967544833999973 ) ) ;
#31444 = CARTESIAN_POINT ( 'NONE',  ( 12.53073434187000146, -77.74559991600001752, -3.509976885708000260 ) ) ;
#31445 = CARTESIAN_POINT ( 'NONE',  ( -10.10713367727843881, -61.26653151295378308, -7.860990029236842425 ) ) ;
#31446 = CARTESIAN_POINT ( 'NONE',  ( 12.83044039274999903, -23.30639625649999758, -2.062670899148999926 ) ) ;
#31447 = ORIENTED_EDGE ( 'NONE', *, *, #37279, .F. ) ;
#31448 = DIRECTION ( 'NONE',  ( 1.000000000000000000, 0.000000000000000000, 0.000000000000000000 ) ) ;
#31449 = LINE ( 'NONE', #9039, #43681 ) ;
#31450 = CARTESIAN_POINT ( 'NONE',  ( -0.3145193548456999832, -81.84765799895200189, -1.272359429009000120 ) ) ;
#31451 = CARTESIAN_POINT ( 'NONE',  ( -1.570796326794884790, -79.01458333333329165, -12.00000000000000355 ) ) ;
#31452 = CARTESIAN_POINT ( 'NONE',  ( -1.146763852601999867, -79.13609509508398787, -9.343239705575001608 ) ) ;
#31454 = CARTESIAN_POINT ( 'NONE',  ( 4.010845454633999552, -1.597904343863999932, -0.2065758488482999922 ) ) ;
#31453 = CARTESIAN_POINT ( 'NONE',  ( 4.002556386389000131, -83.82118105601298907, 1.018850255173999964 ) ) ;
#31455 = CARTESIAN_POINT ( 'NONE',  ( -1.931043742978000077, -59.57795407677000554, -12.75763395697999947 ) ) ;
#31456 = ORIENTED_EDGE ( 'NONE', *, *, #26680, .F. ) ;
#31457 = EDGE_CURVE ( 'NONE', #12549, #44267, #12708, .T. ) ;
#31458 = CARTESIAN_POINT ( 'NONE',  ( 7.807927427423821065, -77.28985569457718441, -7.389794798826798683 ) ) ;
#31459 = CARTESIAN_POINT ( 'NONE',  ( 1.500000000000000000, -79.14999999999999147, 0.000000000000000000 ) ) ;
#31460 = CARTESIAN_POINT ( 'NONE',  ( 3.999999999999675371, -78.70000000000000284, 7.999999999999384492 ) ) ;
#31461 = ORIENTED_EDGE ( 'NONE', *, *, #19630, .F. ) ;
#31462 = ORIENTED_EDGE ( 'NONE', *, *, #37223, .F. ) ;
#31463 = CARTESIAN_POINT ( 'NONE',  ( -5.092641036025000290, -79.61146918641900072, 10.89826376711000044 ) ) ;
#31464 = CARTESIAN_POINT ( 'NONE',  ( 2.914848389051019506, -80.35326446144532042, 10.39463640418927248 ) ) ;
#31465 = ORIENTED_EDGE ( 'NONE', *, *, #21803, .F. ) ;
#31466 = CARTESIAN_POINT ( 'NONE',  ( 11.49150497439000063, -78.85165641916699997, -3.221926464390000078 ) ) ;
#31467 = CLOSED_SHELL ( 'NONE', ( #6465, #36270, #40556, #51546, #7891, #7311, #13849, #47798, #48449, #36540, #24418, #42817, #35173, #49631, #50992, #1509, #21707, #33747, #38378, #19507, #2792, #34386, #56950, #9142, #591, #54238, #41490, #48337, #56691, #9424, #38335, #8986, #51664, #49199, #51159, #56044, #28481, #4712, #44804, #17107, #15780, #20180, #6684, #30187, #55419, #11962, #39202, #2979, #33266, #35329, #11530, #45511, #34725, #49777, #1823, #42839, #17883, #19895, #4874, #18444, #27278, #30436, #13691, #51527, #26019, #30280, #53489, #43074, #24950, #53177, #7242, #12149, #36937, #32596, #39626, #48068, #42977, #21623, #52351, #13511, #4674, #41652, #46786, #29806, #36567, #44400, #16466, #28228, #36144, #24906, #16566, #50504, #53700, #38738, #28748, #37961, #33306, #42241, #40189, #922, #35792, #40125, #26207, #52808, #10699, #9057, #52369, #13464, #42827, #47531, #36212, #4653, #39873, #3705, #44259, #21049, #24250 ) ) ;
#31468 = ORIENTED_EDGE ( 'NONE', *, *, #52639, .T. ) ;
#31469 = ORIENTED_EDGE ( 'NONE', *, *, #24696, .T. ) ;
#31470 = CARTESIAN_POINT ( 'NONE',  ( 0.1070836934507127802, -2.728288973199432199, -3.247988223077748593 ) ) ;
#31471 = CARTESIAN_POINT ( 'NONE',  ( 11.99957818660027442, -76.64406117551696696, -0.7855671627053041339 ) ) ;
#31472 = CARTESIAN_POINT ( 'NONE',  ( 4.014948207387869061, -1.593756223004204609, -0.2067871583196793928 ) ) ;
#31473 = ORIENTED_EDGE ( 'NONE', *, *, #31457, .F. ) ;
#31475 = ADVANCED_FACE ( 'NONE', ( #52424 ), #12634, .F. ) ;
#31474 = ORIENTED_EDGE ( 'NONE', *, *, #31836, .F. ) ;
#31476 = CYLINDRICAL_SURFACE ( 'NONE', #45030, 12.00000000000000000 ) ;
#31477 = DIRECTION ( 'NONE',  ( 2.273768121930269862E-11, -5.258082751534180400E-20, -1.000000000000000000 ) ) ;
#31478 = CARTESIAN_POINT ( 'NONE',  ( 0.000000000000000000, -75.20000000000000284, 6.200000000000000178 ) ) ;
#31479 = DIRECTION ( 'NONE',  ( 0.000000000000000000, 0.000000000000000000, -1.000000000000000000 ) ) ;
#31480 = CARTESIAN_POINT ( 'NONE',  ( 7.220923959705223716, -77.12291666666664014, 9.396085398178630754 ) ) ;
#31481 = CARTESIAN_POINT ( 'NONE',  ( 6.436424241555000592, -79.92391735373439587, 8.610165096135999008 ) ) ;
#31482 = VECTOR ( 'NONE', #53290, 1000.000000000000000 ) ;
#31483 = CARTESIAN_POINT ( 'NONE',  ( 11.36821324764999908, -77.87446272180213214, -3.778861202892000559 ) ) ;
#31484 = EDGE_CURVE ( 'NONE', #44555, #52418, #15675, .T. ) ;
#31485 = CARTESIAN_POINT ( 'NONE',  ( 0.1338524678202104856, -78.72631179971439508, -9.249082273563699275 ) ) ;
#31486 = CARTESIAN_POINT ( 'NONE',  ( -9.213114944024999531, -25.00524898755999814, 8.533795138592999763 ) ) ;
#31487 = ADVANCED_FACE ( 'NONE', ( #11259 ), #33382, .F. ) ;
#31488 = DIRECTION ( 'NONE',  ( 0.000000000000000000, 1.000000000000000000, 0.000000000000000000 ) ) ;
#31489 = CARTESIAN_POINT ( 'NONE',  ( 3.795949068449000041, -79.29100264934788811, -1.737921346834000014 ) ) ;
#31490 = CARTESIAN_POINT ( 'NONE',  ( 7.443337284218999983, -78.06288667140100301, 6.317073012428999768 ) ) ;
#31491 = CARTESIAN_POINT ( 'NONE',  ( 1.061928034666324239, -79.70442635671331288, -0.6832555422594198680 ) ) ;
#31492 = CARTESIAN_POINT ( 'NONE',  ( 17.49999999998999911, -65.72928575305999743, 1.613072089394999983E-05 ) ) ;
#31493 = LINE ( 'NONE', #58085, #21029 ) ;
#31494 = CARTESIAN_POINT ( 'NONE',  ( -0.6826850050872016462, -80.83097677460143871, -1.092173985590070506 ) ) ;
#31495 = DIRECTION ( 'NONE',  ( 0.000000000000000000, 1.000000000000000000, 0.000000000000000000 ) ) ;
#31496 = CARTESIAN_POINT ( 'NONE',  ( 3.921473243360999561, -1.120934344713000019, -0.5217135850094999361 ) ) ;
#31497 = CARTESIAN_POINT ( 'NONE',  ( 3.938458446976999205, -79.30999999999998806, -8.369650235310999165 ) ) ;
#31498 = CIRCLE ( 'NONE', #6074, 0.8000000000000011546 ) ;
#31500 = B_SPLINE_CURVE_WITH_KNOTS ( 'NONE', 3,
 ( #48087, #29463, #25045, #38908, #29745, #34177, #7330, #38330, #47797, #57207, #25331, #25619, #43643, #3201, #16775, #34755, #38624, #12336, #56354, #30325, #7905, #15905, #43068, #2627, #25906, #56641, #43929, #20624, #16199, #2905, #3477, #40060, #35926, #22946, #44497, #45398, #4654, #8777, #35327, #13492, #4049, #36226, #31483, #48650, #18238, #8194, #17338, #54247, #31187, #22051, #546, #40662, #27361, #53652, #13781, #36515, #9075, #49529, #40956, #31782, #49825, #9371, #58076, #22652, #17636 ),
 .UNSPECIFIED., .F., .F.,
 ( 4, 1, 1, 1, 1, 1, 1, 1, 1, 1, 1, 1, 1, 1, 1, 1, 1, 1, 1, 1, 1, 1, 1, 1, 1, 1, 1, 1, 1, 1, 1, 1, 1, 1, 1, 1, 1, 1, 1, 1, 1, 1, 1, 1, 1, 1, 1, 1, 1, 1, 1, 1, 1, 1, 1, 1, 1, 1, 1, 1, 1, 1, 4 ),
 ( 0.000000000000000000, 0.01249978000642217729, 0.02874978733919649962, 0.04499979467197081501, 0.06124980200474514080, 0.07749980933751947354, 0.09374981667029379240, 0.1099998240030681113, 0.1262498313358424162, 0.1424998386686167351, 0.1587498460013910540, 0.1749998533341653728, 0.1912498606669397194, 0.2074998679997140105, 0.2237498753324883571, 0.2399998826652626760, 0.2562498899980369949, 0.2724998973308113137, 0.2887499046635856326, 0.3049999119963599514, 0.3212499193291342703, 0.3374999266619086447, 0.3537499339946829635, 0.3699999413274572269, 0.3862499486602315457, 0.4024999559930059201, 0.4187499633257802389, 0.4349999706585545578, 0.4512499779913288211, 0.4674999853241031955, 0.4837499926568775144, 0.4999999999896518332, 0.5162500073224260966, 0.5325000146552004709, 0.5487500219879747343, 0.5650000293207491087, 0.5812500366535234830, 0.5975000439862977464, 0.6137500513190721207, 0.6300000586518463841, 0.6462500659846207585, 0.6625000733173950218, 0.6787500806501692852, 0.6950000879829436595, 0.7112500953157180339, 0.7275001026484924083, 0.7437501099812666716, 0.7600001173140410460, 0.7762501246468153093, 0.7925001319795895727, 0.8087501393123639470, 0.8250001466451382104, 0.8412501539779126958, 0.8575001613106869591, 0.8737501686434612225, 0.8900001759762355968, 0.9062501833090098602, 0.9225001906417842346, 0.9387501979745584979, 0.9550002053073327613, 0.9712502126401071356, 0.9875002199728815100, 1.000000000000000000 ),
 .UNSPECIFIED. ) ;
#31499 = CARTESIAN_POINT ( 'NONE',  ( -0.6252223470676733230, -80.94041847728219352, -1.378227358566912919 ) ) ;
#31501 = CARTESIAN_POINT ( 'NONE',  ( -1.252361392338912749, -78.59141244381495994, 0.1411392993344418867 ) ) ;
#31502 = CYLINDRICAL_SURFACE ( 'NONE', #21229, 4.100000000000000533 ) ;
#31503 = CARTESIAN_POINT ( 'NONE',  ( 13.63885489310999510, -19.21421830981000056, -7.254376133916000668 ) ) ;
#31504 = CONICAL_SURFACE ( 'NONE', #51322, 10.29999999990999981, 0.7853981633972997312 ) ;
#31505 = CARTESIAN_POINT ( 'NONE',  ( -9.204454400623999888, -78.57176524200400536, -5.869700187727000085 ) ) ;
#31506 = CARTESIAN_POINT ( 'NONE',  ( -4.862705500402999981, -78.46600984204799545, -11.27607530993000040 ) ) ;
#31507 = CARTESIAN_POINT ( 'NONE',  ( -1.980464439859999981, -57.04527982639000072, 12.85144117157999943 ) ) ;
#31508 = ADVANCED_FACE ( 'NONE', ( #29240 ), #28728, .F. ) ;
#31510 = CARTESIAN_POINT ( 'NONE',  ( 0.2218511837006999776, -78.65981053183800498, 1.400300479361000106 ) ) ;
#31509 = CYLINDRICAL_SURFACE ( 'NONE', #36405, 1.750000000000000000 ) ;
#31511 = CARTESIAN_POINT ( 'NONE',  ( -1.495211702480000016, -81.28774735892999104, -0.3395960383748000133 ) ) ;
#31512 = ORIENTED_EDGE ( 'NONE', *, *, #35189, .F. ) ;
#31513 = CARTESIAN_POINT ( 'NONE',  ( -3.341467261686000167, -84.79907450217399401, 1.310852413871999911 ) ) ;
#31514 = CARTESIAN_POINT ( 'NONE',  ( 3.241375870716999508, -80.99271274871159676, 10.69195759319000061 ) ) ;
#31515 = CARTESIAN_POINT ( 'NONE',  ( -8.841085912879560027, -79.99999999999998579, -2.882805647535432669 ) ) ;
#31516 = CARTESIAN_POINT ( 'NONE',  ( 0.3926218265389220807, -81.64583333333334281, -1.460959015002473382 ) ) ;
#31517 = CARTESIAN_POINT ( 'NONE',  ( 5.694538069269999623E-14, -72.89999999999999147, -14.00000000000097877 ) ) ;
#31518 = CARTESIAN_POINT ( 'NONE',  ( 9.292856425461000214, -78.60338192318698702, 2.915907262279999745 ) ) ;
#31519 = CARTESIAN_POINT ( 'NONE',  ( 11.45970853605999906, -77.04030896091001068, 5.337786833297999856 ) ) ;
#31520 = CARTESIAN_POINT ( 'NONE',  ( 11.75000000000000000, -79.79999999999999716, -4.009019365174000020E-13 ) ) ;
#31521 = CARTESIAN_POINT ( 'NONE',  ( -3.164582902296511069, -3.121138013161445457, -0.8488383203591168824 ) ) ;
#31522 = CARTESIAN_POINT ( 'NONE',  ( -1.931086388578000079, -60.09778754156999980, 12.71798269388000158 ) ) ;
#31523 = VERTEX_POINT ( 'NONE', #25109 ) ;
#31524 = EDGE_CURVE ( 'NONE', #56598, #13233, #20400, .T. ) ;
#31525 = CARTESIAN_POINT ( 'NONE',  ( 1.208267227088423823, -53.97409317822796027, -12.70228502419097794 ) ) ;
#31526 = CARTESIAN_POINT ( 'NONE',  ( -9.501130936298000762, -79.68751332859899605, 0.6697165097470000328 ) ) ;
#31527 = DIRECTION ( 'NONE',  ( 0.000000000000000000, 0.000000000000000000, -1.000000000000000000 ) ) ;
#31528 = ADVANCED_FACE ( 'NONE', ( #38396 ), #55837, .T. ) ;
#31529 = CARTESIAN_POINT ( 'NONE',  ( -1.199500263597270244, -81.45208333333334849, -0.9218200799623728070 ) ) ;
#31530 = CARTESIAN_POINT ( 'NONE',  ( 1.941425054909000192, -82.66792953870898941, 2.969069166356000267 ) ) ;
#31531 = AXIS2_PLACEMENT_3D ( 'NONE', #35195, #3636, #12493 ) ;
#31532 = CARTESIAN_POINT ( 'NONE',  ( 0.000000000000000000, -77.50000000000000000, 0.000000000000000000 ) ) ;
#31533 = ORIENTED_EDGE ( 'NONE', *, *, #57406, .T. ) ;
#31534 = CARTESIAN_POINT ( 'NONE',  ( -1.529773069620000037, -77.10717163294118848, -11.10696160730999971 ) ) ;
#31535 = CARTESIAN_POINT ( 'NONE',  ( -0.7699595307336942751, -77.81793362728524244, -11.75325798414018941 ) ) ;
#31536 = CIRCLE ( 'NONE', #46677, 9.000000000000000000 ) ;
#31537 = CARTESIAN_POINT ( 'NONE',  ( 11.99999999979999821, -23.14999999072999870, -0.7999999997951999786 ) ) ;
#31538 = ORIENTED_EDGE ( 'NONE', *, *, #14140, .F. ) ;
#31539 = ORIENTED_EDGE ( 'NONE', *, *, #22302, .T. ) ;
#31540 = CARTESIAN_POINT ( 'NONE',  ( -10.52693198617000014, -55.37847693893999690, -7.606025555747000233 ) ) ;
#31541 = AXIS2_PLACEMENT_3D ( 'NONE', #52689, #30235, #34083 ) ;
#31542 = CARTESIAN_POINT ( 'NONE',  ( 9.534323188421000239, -78.95122794097099472, -1.008198710029000189 ) ) ;
#31543 = ORIENTED_EDGE ( 'NONE', *, *, #7086, .T. ) ;
#31544 = CARTESIAN_POINT ( 'NONE',  ( 2.538881527327999876, -76.98177497604999076, 11.96833873699999984 ) ) ;
#31545 = PLANE ( 'NONE',  #12633 ) ;
#31546 = CARTESIAN_POINT ( 'NONE',  ( -0.2514447808355999570, -78.15716200999000307, 1.629006369695999767 ) ) ;
#31547 = VERTEX_POINT ( 'NONE', #29810 ) ;
#31548 = CARTESIAN_POINT ( 'NONE',  ( 3.861138328465000047, -76.97116028321799774, 8.493887087553000370 ) ) ;
#31549 = DIRECTION ( 'NONE',  ( 0.7071067811865475727, 0.000000000000000000, -0.7071067811865475727 ) ) ;
#31550 = CARTESIAN_POINT ( 'NONE',  ( 12.66594527011999816, -76.72356177075999994, -3.392478259704000187 ) ) ;
#31551 = CARTESIAN_POINT ( 'NONE',  ( -10.54491486739000017, -77.77768451251904480, -3.823987582478999947 ) ) ;
#31552 = CARTESIAN_POINT ( 'NONE',  ( -3.268206247460667235, -86.36264282632899381, 1.381888203336044896 ) ) ;
#31553 = CARTESIAN_POINT ( 'NONE',  ( 3.042547531669000271, -78.64783470746900207, -10.31045122763999977 ) ) ;
#31554 = CARTESIAN_POINT ( 'NONE',  ( 7.006148741439892191, -79.90670744298051886, 6.039518869995502470 ) ) ;
#31555 = CYLINDRICAL_SURFACE ( 'NONE', #32175, 9.250000000000000000 ) ;
#31556 = ORIENTED_EDGE ( 'NONE', *, *, #56491, .T. ) ;
#31557 = CARTESIAN_POINT ( 'NONE',  ( -10.85153605587000136, -80.10354523164899376, 2.386335476490000218 ) ) ;
#31558 = CARTESIAN_POINT ( 'NONE',  ( 2.859706235832604193, -77.25018302167970319, -8.796733326739918368 ) ) ;
#31559 = CARTESIAN_POINT ( 'NONE',  ( -1.034826241750000264, -80.78746333463699614, 1.108174957742000144 ) ) ;
#31560 = B_SPLINE_SURFACE_WITH_KNOTS ( 'NONE', 3, 3, ( 
 ( #6226, #56699, #7103, #43130 ),
 ( #2686, #28657, #24821, #42545 ),
 ( #46705, #1824, #11545, #46993 ),
 ( #51706, #52271, #38391, #20679 ),
 ( #37812, #33379, #33079, #29802 ),
 ( #11255, #16257, #20112, #11825 ),
 ( #47857, #10967, #6812, #24243 ),
 ( #43403, #28951, #7387, #29522 ),
 ( #15083, #33951, #6521, #42259 ),
 ( #2964, #56123, #24531, #15669 ),
 ( #25388, #38678, #20963, #25103 ),
 ( #19820, #51124, #10677, #56410 ),
 ( #33667, #55833, #2113, #38103 ),
 ( #29234, #47284, #42837, #2396 ),
 ( #20393, #15960, #51990, #34814 ),
 ( #8541, #48143, #44561, #12960 ),
 ( #58137, #17704, #21825, #30957 ) ),
 .UNSPECIFIED., .F., .F., .F.,
 ( 4, 1, 1, 1, 1, 1, 1, 1, 1, 1, 1, 1, 1, 1, 4 ),
 ( 4, 4 ),
 ( -0.01011837001263999995, 0.000000000000000000, 0.08333333333333001192, 0.1666666666667000196, 0.2500000000000000000, 0.3333333333333000081, 0.4166666666666999919, 0.5000000000000000000, 0.5833333333333000637, 0.6666666666667000474, 0.7500000000000000000, 0.8333333333333000637, 0.9166666666667000474, 1.000000000000000000, 1.010372850415000023 ),
 ( -0.3559705548695000221, 1.357613361108999994 ),
 .UNSPECIFIED. ) ;
#31561 = CARTESIAN_POINT ( 'NONE',  ( -2.185466470362367630, -3.277594938514446277, 2.760202041691888208 ) ) ;
#31562 = CARTESIAN_POINT ( 'NONE',  ( -8.610991514544377168, -16.82512235768486875, 9.355860133801421341 ) ) ;
#31563 = B_SPLINE_CURVE_WITH_KNOTS ( 'NONE', 3,
 ( #24475, #42489, #2059, #56070, #15614, #33609, #51652, #11203, #29179, #47226, #6757, #24767, #42779, #20336, #38331, #56355, #12055, #13194 ),
 .UNSPECIFIED., .F., .F.,
 ( 4, 2, 2, 2, 2, 2, 2, 2, 4 ),
 ( 0.000000000000000000, 0.1250000000000000000, 0.2500000000000000000, 0.3750000000000000000, 0.5000000000000000000, 0.6250000000000000000, 0.7500000000000000000, 0.8750000000000000000, 1.000000000000000000 ),
 .UNSPECIFIED. ) ;
#31564 = CARTESIAN_POINT ( 'NONE',  ( 0.03250568004163000707, -76.07646268326499239, 11.74995503739000036 ) ) ;
#31565 = CARTESIAN_POINT ( 'NONE',  ( -9.723174507563001612, -61.27697503937000079, -7.958760295438001009 ) ) ;
#31566 = CARTESIAN_POINT ( 'NONE',  ( -9.104587144006000443, -77.46948832859899881, -3.133183417595999831 ) ) ;
#31567 = CARTESIAN_POINT ( 'NONE',  ( 11.28168611626732698, -76.82899490262227005, 4.307594075494947106 ) ) ;
#31568 = CARTESIAN_POINT ( 'NONE',  ( 9.376438147752001129, -79.45376715878452956, -6.156339679782000474 ) ) ;
#31569 = AXIS2_PLACEMENT_3D ( 'NONE', #36475, #4614, #49187 ) ;
#31570 = DIRECTION ( 'NONE',  ( 0.000000000000000000, -1.000000000000000000, 0.000000000000000000 ) ) ;
#31571 = ORIENTED_EDGE ( 'NONE', *, *, #21366, .T. ) ;
#31572 = CARTESIAN_POINT ( 'NONE',  ( 0.5015714934020000237, -83.24273121958398747, 1.504246450876000063 ) ) ;
#31573 = AXIS2_PLACEMENT_3D ( 'NONE', #35323, #21761, #4046 ) ;
#31574 = CARTESIAN_POINT ( 'NONE',  ( -1.214718215476999985, -80.98388962642000877, 0.5919720313516000365 ) ) ;
#31575 = CYLINDRICAL_SURFACE ( 'NONE', #50290, 1.750000000000000000 ) ;
#31576 = DIRECTION ( 'NONE',  ( -0.7071067811864970576, -3.534300184300985629E-08, -0.7071067811865970887 ) ) ;
#31577 = DIRECTION ( 'NONE',  ( -0.7071067812088192017, 2.829527200303080525E-07, 0.7071067811642192114 ) ) ;
#31578 = VECTOR ( 'NONE', #27082, 1000.000000000000000 ) ;
#31579 = CARTESIAN_POINT ( 'NONE',  ( 0.5999999999999999778, -5.200000000000000178, 0.5999999999999999778 ) ) ;
#31580 = CARTESIAN_POINT ( 'NONE',  ( -8.871933854994999535, -78.60349805011500735, -3.979018739998999354 ) ) ;
#31581 = EDGE_CURVE ( 'NONE', #30600, #20755, #33997, .T. ) ;
#31582 = CARTESIAN_POINT ( 'NONE',  ( 2.299484790252942723, -76.05912199685272412, 11.52265691577497897 ) ) ;
#31583 = CARTESIAN_POINT ( 'NONE',  ( -2.801579282652000291, -79.06343076078299248, -10.67018687299000135 ) ) ;
#31584 = CARTESIAN_POINT ( 'NONE',  ( -2.662296488502435832, -85.83735716284300565, 3.593683008806336066 ) ) ;
#31585 = ORIENTED_EDGE ( 'NONE', *, *, #33943, .T. ) ;
#31586 = B_SPLINE_CURVE_WITH_KNOTS ( 'NONE', 3,
 ( #29480, #7634, #2357, #52229, #21498, #16500 ),
 .UNSPECIFIED., .F., .F.,
 ( 4, 2, 4 ),
 ( 0.000000000000000000, 0.5000000000000000000, 1.000000000000000000 ),
 .UNSPECIFIED. ) ;
#31587 = DIRECTION ( 'NONE',  ( 0.7071067811865475727, 0.000000000000000000, 0.7071067811865475727 ) ) ;
#31588 = AXIS2_PLACEMENT_3D ( 'NONE', #55348, #55938, #29055 ) ;
#31589 = ADVANCED_FACE ( 'NONE', ( #29526 ), #36277, .F. ) ;
#31590 = CARTESIAN_POINT ( 'NONE',  ( -0.03204405817076288326, -78.67390000031814168, -3.399848993460840685 ) ) ;
#31592 = CARTESIAN_POINT ( 'NONE',  ( -6.192097496234715059, -76.28079615762941046, -9.993622780947980289 ) ) ;
#31591 = CARTESIAN_POINT ( 'NONE',  ( -10.47020627418440242, -77.47916666666667140, 2.813789756862221214 ) ) ;
#31593 = CARTESIAN_POINT ( 'NONE',  ( 9.304500756975000897, -79.13566128010499767, -5.821536072646999571 ) ) ;
#31594 = DIRECTION ( 'NONE',  ( 1.000000000000000000, 0.000000000000000000, 0.000000000000000000 ) ) ;
#31595 = CARTESIAN_POINT ( 'NONE',  ( 4.656680505379999779, -76.71804223774499576, 11.60471035503999992 ) ) ;
#31596 = CARTESIAN_POINT ( 'NONE',  ( -1.370379768245999841E-14, -74.59999999999999432, 0.000000000000000000 ) ) ;
#31597 = DIRECTION ( 'NONE',  ( 0.000000000000000000, -1.000000000000000000, 0.000000000000000000 ) ) ;
#31598 = ORIENTED_EDGE ( 'NONE', *, *, #4478, .F. ) ;
#31599 = CARTESIAN_POINT ( 'NONE',  ( 6.836697942985000331, -79.03132150479699192, 8.804212730688998789 ) ) ;
#31600 = CARTESIAN_POINT ( 'NONE',  ( 12.70228549156958486, -53.97187149228901859, 1.205357499425017132 ) ) ;
#31601 = CARTESIAN_POINT ( 'NONE',  ( 11.00000000000000000, -77.94999999999998863, 0.000000000000000000 ) ) ;
#31602 = CARTESIAN_POINT ( 'NONE',  ( 3.621447497675000626, -78.40681307385641219, 2.137281866361618654 ) ) ;
#31603 = EDGE_CURVE ( 'NONE', #40579, #39052, #19348, .T. ) ;
#31605 = CARTESIAN_POINT ( 'NONE',  ( 9.000000000000000000, -92.39999999999999147, 0.000000000000000000 ) ) ;
#31604 = CARTESIAN_POINT ( 'NONE',  ( -1.187238164339999846, -80.68061120219299198, -0.3457930548265999993 ) ) ;
#31606 = CARTESIAN_POINT ( 'NONE',  ( 1.695617993698999904, -78.16967705768098540, 10.91800231797999921 ) ) ;
#31607 = DIRECTION ( 'NONE',  ( 0.000000000000000000, 0.000000000000000000, -1.000000000000000000 ) ) ;
#31608 = CARTESIAN_POINT ( 'NONE',  ( -10.19999999921000011, -0.2000000007865999907, 1.811583764860000079E-09 ) ) ;
#31609 = CARTESIAN_POINT ( 'NONE',  ( -1.500000000000000000, -81.00000000000000000, 0.000000000000000000 ) ) ;
#31610 = EDGE_CURVE ( 'NONE', #3043, #2890, #20116, .T. ) ;
#31611 = CARTESIAN_POINT ( 'NONE',  ( -9.250000000000000000, -79.99999999999998579, 2.662757480928999879E-14 ) ) ;
#31612 = CARTESIAN_POINT ( 'NONE',  ( -5.239266479141340582, -79.61428708882451133, 9.745699944792932001 ) ) ;
#31613 = EDGE_CURVE ( 'NONE', #30461, #55907, #28344, .T. ) ;
#31614 = COLOUR_RGB ( '', 0.40784314, 0.44705882, 0.49803922) ;
#31615 = CARTESIAN_POINT ( 'NONE',  ( -12.77649794757999935, -25.30831393477999924, -0.06464137375187999079 ) ) ;
#31616 = ORIENTED_EDGE ( 'NONE', *, *, #4584, .F. ) ;
#31617 = ORIENTED_EDGE ( 'NONE', *, *, #18449, .T. ) ;
#31618 = CARTESIAN_POINT ( 'NONE',  ( 9.500000000000000000, -78.64999999999999147, 0.000000000000000000 ) ) ;
#31619 = VERTEX_POINT ( 'NONE', #53419 ) ;
#31620 = CARTESIAN_POINT ( 'NONE',  ( -9.512960740429173612, -76.70695994172498899, 5.706843784427905852 ) ) ;
#31621 = ORIENTED_EDGE ( 'NONE', *, *, #27360, .F. ) ;
#31622 = CARTESIAN_POINT ( 'NONE',  ( 7.631889049354000143, -23.22121504852000129, 10.36222434949000082 ) ) ;
#31623 = CARTESIAN_POINT ( 'NONE',  ( 5.176319218327999572, -77.80500231115298959, -9.742045664616000522 ) ) ;
#31624 = B_SPLINE_CURVE_WITH_KNOTS ( 'NONE', 3,
 ( #2450, #6576, #20739, #38737 ),
 .UNSPECIFIED., .F., .F.,
 ( 4, 4 ),
 ( 0.000000000000000000, 1.000000000000000000 ),
 .UNSPECIFIED. ) ;
#31625 = CARTESIAN_POINT ( 'NONE',  ( -1.250000000000000000, -83.09999999999999432, 0.000000000000000000 ) ) ;
#31626 = CARTESIAN_POINT ( 'NONE',  ( -5.485200302047999799, -78.70643998579799927, -7.984597978739000901 ) ) ;
#31627 = CARTESIAN_POINT ( 'NONE',  ( -5.117438655294176186, -78.17837365130638716, -7.705456670207614600 ) ) ;
#31628 = CARTESIAN_POINT ( 'NONE',  ( -4.152600241220000044, -79.29313857269499977, -10.41988588363999924 ) ) ;
#31629 = CARTESIAN_POINT ( 'NONE',  ( 8.826328960311670357, -81.00000000000001421, 6.438658266756784876 ) ) ;
#31630 = ORIENTED_EDGE ( 'NONE', *, *, #47775, .T. ) ;
#31631 = CARTESIAN_POINT ( 'NONE',  ( -3.708203932498999933, -79.79999999999999716, 11.41267819554000162 ) ) ;
#31632 = ORIENTED_EDGE ( 'NONE', *, *, #40495, .F. ) ;
#31633 = CARTESIAN_POINT ( 'NONE',  ( -0.003049617359667225382, -77.47517976812264351, 9.249906914136946767 ) ) ;
#31634 = CARTESIAN_POINT ( 'NONE',  ( 9.391860901740999523, -77.28449860050398001, 5.803232400709999794 ) ) ;
#31635 = DIRECTION ( 'NONE',  ( 0.000000000000000000, 1.000000000000000000, 7.261213190611999915E-14 ) ) ;
#31636 = CARTESIAN_POINT ( 'NONE',  ( -9.139898499914998808, -77.30632546697400187, 2.826942883852999966 ) ) ;
#31637 = CARTESIAN_POINT ( 'NONE',  ( -1.871685860826000081, -76.53201366967000752, -12.83051903312999897 ) ) ;
#31638 = CARTESIAN_POINT ( 'NONE',  ( -9.034242263150824570, -79.42472277150091031, -2.937518930512160509 ) ) ;
#31639 = CARTESIAN_POINT ( 'NONE',  ( 0.1429208184976999974, -78.57917818882999939, 1.621183732314999792 ) ) ;
#31640 = CYLINDRICAL_SURFACE ( 'NONE', #30859, 10.75000000000000000 ) ;
#31641 = CARTESIAN_POINT ( 'NONE',  ( 8.291742182491999458, -78.23574086744999079, 7.136865503491999441 ) ) ;
#31642 = CARTESIAN_POINT ( 'NONE',  ( -10.35398566681999988, -23.40788276239999988, -7.619388279076999559 ) ) ;
#31643 = CARTESIAN_POINT ( 'NONE',  ( -10.84978627008842444, -76.66831054839785509, 4.509941008725813383 ) ) ;
#31644 = CARTESIAN_POINT ( 'NONE',  ( 0.2703574106265999588, -82.61867690334500480, 3.579198825151999941 ) ) ;
#31645 = ORIENTED_EDGE ( 'NONE', *, *, #53837, .T. ) ;
#31646 = CARTESIAN_POINT ( 'NONE',  ( -11.53293850418999966, -79.34293712903799189, 4.645575608415999369 ) ) ;
#31647 = CARTESIAN_POINT ( 'NONE',  ( -10.74259976513999959, -76.69405063463399586, 2.023095082799000188 ) ) ;
#31648 = CARTESIAN_POINT ( 'NONE',  ( -7.284620157678814323, -78.03426350768698683, 7.905984289670053400 ) ) ;
#31649 = CARTESIAN_POINT ( 'NONE',  ( 10.42503750987000011, -77.41068818197000212, -5.902083371034000159 ) ) ;
#31650 = CARTESIAN_POINT ( 'NONE',  ( -10.01749678875999905, -18.80819056997000160, 7.660430392568000180 ) ) ;
#31652 = CARTESIAN_POINT ( 'NONE',  ( 12.50000000000000000, -49.87071422276000021, 0.000000000000000000 ) ) ;
#31651 = DIRECTION ( 'NONE',  ( 0.000000000000000000, 0.000000000000000000, -1.000000000000000000 ) ) ;
#31653 = LINE ( 'NONE', #4224, #12883 ) ;
#31654 = CARTESIAN_POINT ( 'NONE',  ( 4.625011536115999355, -80.27905154712398428, -10.42155147329000009 ) ) ;
#31655 = DIRECTION ( 'NONE',  ( 0.000000000000000000, 1.000000000000000000, 0.000000000000000000 ) ) ;
#31656 = CARTESIAN_POINT ( 'NONE',  ( 11.01685767354999967, -77.12896664909099798, -1.698071721886999841 ) ) ;
#31657 = DIRECTION ( 'NONE',  ( -1.000000000000000000, 0.000000000000000000, 0.000000000000000000 ) ) ;
#31658 = CARTESIAN_POINT ( 'NONE',  ( -8.276171816746000331, -80.33277059862079739, 7.458027891273999899 ) ) ;
#31659 = ORIENTED_EDGE ( 'NONE', *, *, #7385, .T. ) ;
#31660 = CARTESIAN_POINT ( 'NONE',  ( 1.669724228661999987, -55.43102323432999867, 12.48434610065999983 ) ) ;
#31661 = VECTOR ( 'NONE', #45718, 1000.000000000000000 ) ;
#31662 = CARTESIAN_POINT ( 'NONE',  ( -6.013262726775999489, -77.57957403538303254, 7.348341287529000176 ) ) ;
#31663 = CARTESIAN_POINT ( 'NONE',  ( 3.261288468347999903, -3.007443126209999651, -2.257235270949999872 ) ) ;
#31664 = CARTESIAN_POINT ( 'NONE',  ( 6.433795189870999742, -77.37192883941298760, -9.188274595716000803 ) ) ;
#31665 = CARTESIAN_POINT ( 'NONE',  ( 10.71369944335147828, -79.92916666666667425, -2.879226727952064913 ) ) ;
#31666 = CARTESIAN_POINT ( 'NONE',  ( 9.500000000000005329, -77.53958333333333997, -1.243547092045939939 ) ) ;
#31667 = DIRECTION ( 'NONE',  ( 0.000000000000000000, -1.000000000000000000, 0.000000000000000000 ) ) ;
#31668 = CARTESIAN_POINT ( 'NONE',  ( -1.405334850318079587, -24.31492947778725977, -12.50716844834618868 ) ) ;
#31669 = CARTESIAN_POINT ( 'NONE',  ( 0.000000000000000000, -80.99999999999998579, -5.499999999999927169 ) ) ;
#31670 = VECTOR ( 'NONE', #48958, 1000.000000000000000 ) ;
#31671 = CARTESIAN_POINT ( 'NONE',  ( -2.639344177053999818, -84.67882450217399537, 3.176848410495999975 ) ) ;
#31672 = DIRECTION ( 'NONE',  ( -1.000000000000000000, 0.000000000000000000, 0.000000000000000000 ) ) ;
#31673 = VECTOR ( 'NONE', #57610, 1000.000000000000000 ) ;
#31674 = ADVANCED_FACE ( 'NONE', ( #30676 ), #40432, .T. ) ;
#31675 = CARTESIAN_POINT ( 'NONE',  ( 9.783235115916999902, -54.26434390361999505, -7.961033122292000108 ) ) ;
#31676 = CARTESIAN_POINT ( 'NONE',  ( 5.284336329618000150, -77.94045643997900186, -9.945338310677000138 ) ) ;
#31677 = CARTESIAN_POINT ( 'NONE',  ( -0.8906226101088000613, -79.28558737503999509, -1.206976125017999779 ) ) ;
#31678 = CARTESIAN_POINT ( 'NONE',  ( -0.9359438995330000566, -78.25257508323998934, 1.375335667459000044 ) ) ;
#31679 = CARTESIAN_POINT ( 'NONE',  ( -1.782734487945632607, -60.92245368521469828, 12.71547286929785514 ) ) ;
#31680 = CARTESIAN_POINT ( 'NONE',  ( -1.508012578157784445, -82.75403821467907051, -0.07803458566731928669 ) ) ;
#31681 = CARTESIAN_POINT ( 'NONE',  ( -12.61271904362000029, -59.99692351013000291, 1.798332623270000097 ) ) ;
#31682 = CARTESIAN_POINT ( 'NONE',  ( -8.631379868284000167, -78.29701580198705813, 6.779623747091000574 ) ) ;
#31683 = CARTESIAN_POINT ( 'NONE',  ( -5.413904038987160661, -77.08333333333334281, -9.393203674808278336 ) ) ;
#31684 = CARTESIAN_POINT ( 'NONE',  ( 1.088575500396492979, -77.85671926408777210, -0.6620644299734026461 ) ) ;
#31685 = CARTESIAN_POINT ( 'NONE',  ( 1.249621047773330496, -81.84926137039978755, -0.02155140958586815314 ) ) ;
#31686 = DIRECTION ( 'NONE',  ( 0.000000000000000000, -1.000000000000000000, 0.000000000000000000 ) ) ;
#31687 = EDGE_CURVE ( 'NONE', #30430, #1042, #15150, .T. ) ;
#31688 = CARTESIAN_POINT ( 'NONE',  ( 11.07171638148000170, -79.13188541137900245, -1.292941197001999942 ) ) ;
#31689 = CARTESIAN_POINT ( 'NONE',  ( 0.000000000000000000, -76.75499999999999545, 0.000000000000000000 ) ) ;
#31690 = ORIENTED_EDGE ( 'NONE', *, *, #19352, .T. ) ;
#31691 = ORIENTED_EDGE ( 'NONE', *, *, #14350, .T. ) ;
#31692 = CARTESIAN_POINT ( 'NONE',  ( 1.416683027186000254, -80.76831832026100244, -0.5403291534934999696 ) ) ;
#31693 = B_SPLINE_CURVE_WITH_KNOTS ( 'NONE', 3,
 ( #15671, #33669, #51707, #37518, #1826, #45019, #55536, #5645, #41667, #31702, #19235, #19822, #37227, #55243, #15085, #32785, #23942, #37813 ),
 .UNSPECIFIED., .F., .F.,
 ( 4, 2, 2, 2, 2, 2, 2, 2, 4 ),
 ( 0.000000000000000000, 0.1249999999999999722, 0.2499999999999999445, 0.3749999999999998890, 0.4999999999999998890, 0.6249999999999998890, 0.7499999999999997780, 0.8749999999999998890, 1.000000000000000000 ),
 .UNSPECIFIED. ) ;
#31694 = EDGE_LOOP ( 'NONE', ( #32624, #13170, #7705, #48142 ) ) ;
#31695 = CARTESIAN_POINT ( 'NONE',  ( 0.5999999999999999778, -5.000000000000000000, 4.000000000000000000 ) ) ;
#31696 = EDGE_LOOP ( 'NONE', ( #19968, #885, #27147, #34230 ) ) ;
#31697 = CARTESIAN_POINT ( 'NONE',  ( 1.143767095131633660, -80.38318895732449221, 0.5041385401734318483 ) ) ;
#31698 = PLANE ( 'NONE',  #30072 ) ;
#31699 = CARTESIAN_POINT ( 'NONE',  ( 12.04999999926000243, -79.29999999926000953, 5.384918141074000180E-09 ) ) ;
#31700 = CARTESIAN_POINT ( 'NONE',  ( 1.798368564625000054, -23.19636757045999786, -12.61278090841000044 ) ) ;
#31701 = CARTESIAN_POINT ( 'NONE',  ( -3.686243627255000099, -79.05095254773289071, -0.7229131249021999439 ) ) ;
#31702 = CARTESIAN_POINT ( 'NONE',  ( -0.1963495408493673156, -80.28541666666667709, 1.499999999999999556 ) ) ;
#31703 = CARTESIAN_POINT ( 'NONE',  ( 5.196088533839524182, -78.26493743760516963, -9.481230459712604031 ) ) ;
#31704 = CARTESIAN_POINT ( 'NONE',  ( 2.549865490971999549, -78.60221383193000122, 11.63742185847999977 ) ) ;
#31705 = VERTEX_POINT ( 'NONE', #37456 ) ;
#31706 = EDGE_LOOP ( 'NONE', ( #48079, #32751, #49378, #50453 ) ) ;
#31707 = CARTESIAN_POINT ( 'NONE',  ( -1.649952397703835505, -77.01404686049248483, -11.92900123064598361 ) ) ;
#31708 = EDGE_CURVE ( 'NONE', #16896, #24330, #45761, .T. ) ;
#31709 = CARTESIAN_POINT ( 'NONE',  ( 1.199918086393000127, -80.55160064699700229, 0.5820416783086000967 ) ) ;
#31710 = CARTESIAN_POINT ( 'NONE',  ( -3.907230163516999699, -77.80156924675998198, -8.882807090995999744 ) ) ;
#31711 = CARTESIAN_POINT ( 'NONE',  ( 0.4861418710279412081, -86.12610001270962812, -4.619149248742044911 ) ) ;
#31712 = CARTESIAN_POINT ( 'NONE',  ( 3.180025244547568519, -85.83115353646098811, 1.616841368705626891 ) ) ;
#31713 = AXIS2_PLACEMENT_3D ( 'NONE', #40906, #58030, #35577 ) ;
#31714 = VECTOR ( 'NONE', #334, 1000.000000000000000 ) ;
#31715 = CARTESIAN_POINT ( 'NONE',  ( 12.34410331423999985, -77.06018438914000512, -3.381164140480000135 ) ) ;
#31716 = CARTESIAN_POINT ( 'NONE',  ( -3.110005734825000090, -77.63915923096000427, 12.25287980954000133 ) ) ;
#31717 = CARTESIAN_POINT ( 'NONE',  ( 10.79726974137000006, -76.19359237496099979, -2.097837960889999742 ) ) ;
#31718 = VECTOR ( 'NONE', #56804, 1000.000000000000000 ) ;
#31719 = LINE ( 'NONE', #770, #32059 ) ;
#31720 = CARTESIAN_POINT ( 'NONE',  ( -4.007874235025999710, -81.68874464050298911, 1.168997190988000145 ) ) ;
#31721 = AXIS2_PLACEMENT_3D ( 'NONE', #27350, #45386, #14352 ) ;
#31722 = CARTESIAN_POINT ( 'NONE',  ( -4.454457568640999732, -80.74124369751984887, 10.34731867136000005 ) ) ;
#31723 = CARTESIAN_POINT ( 'NONE',  ( 7.374560639698954034, -76.62291666666664014, 9.596002108778181494 ) ) ;
#31724 = CARTESIAN_POINT ( 'NONE',  ( -6.652173553828778729, -78.22269769528665506, 9.741036272413309050 ) ) ;
#31725 = CARTESIAN_POINT ( 'NONE',  ( -0.3708117234359000203, -80.56882046129099706, -3.528037880666999637 ) ) ;
#31726 = CARTESIAN_POINT ( 'NONE',  ( 1.196963559360000096, -78.43554551434779398, -0.5880938590690999446 ) ) ;
#31727 = PLANE ( 'NONE',  #56274 ) ;
#31728 = CARTESIAN_POINT ( 'NONE',  ( -9.421357847594000745, -80.44786001875249326, -6.176342950743000770 ) ) ;
#31729 = CARTESIAN_POINT ( 'NONE',  ( -3.750250575282000121, -2.303689136176000130, 0.6493866540274000343 ) ) ;
#31730 = CARTESIAN_POINT ( 'NONE',  ( 8.405424692078989679, -77.20000000000001705, -6.846044140412126389 ) ) ;
#31731 = ORIENTED_EDGE ( 'NONE', *, *, #51109, .F. ) ;
#31732 = CARTESIAN_POINT ( 'NONE',  ( 0.4764073897457280493, -23.51691643868322856, 10.98970030907948114 ) ) ;
#31733 = DIRECTION ( 'NONE',  ( 0.000000000000000000, -1.000000000000000000, 0.000000000000000000 ) ) ;
#31734 = CARTESIAN_POINT ( 'NONE',  ( -1.297058042903999953, -81.28434093078000444, -0.3101879797029999941 ) ) ;
#31735 = B_SPLINE_CURVE_WITH_KNOTS ( 'NONE', 3,
 ( #45322, #22870, #45026, #9882, #14005, #1045, #32002, #4579 ),
 .UNSPECIFIED., .F., .F.,
 ( 4, 2, 2, 4 ),
 ( 0.000000000000000000, 0.4999999999999973355, 0.7499999999999986677, 1.000000000000000000 ),
 .UNSPECIFIED. ) ;
#31736 = CARTESIAN_POINT ( 'NONE',  ( 1.667916687244999974, -55.50150862742999891, 12.49168433577000137 ) ) ;
#31737 = CARTESIAN_POINT ( 'NONE',  ( 5.715297388934000189, -78.35615096658000311, 11.69132169264999987 ) ) ;
#31738 = CARTESIAN_POINT ( 'NONE',  ( -9.447769977218822390, -79.56055520885148269, 5.131292296675055375 ) ) ;
#31739 = CARTESIAN_POINT ( 'NONE',  ( 1.807226454530999948, -79.43046001420199786, 9.346133917991000573 ) ) ;
#31740 = DIRECTION ( 'NONE',  ( -1.000000000000000000, 0.000000000000000000, 0.000000000000000000 ) ) ;
#31741 = ORIENTED_EDGE ( 'NONE', *, *, #39701, .T. ) ;
#31742 = EDGE_CURVE ( 'NONE', #57621, #19974, #46053, .T. ) ;
#31743 = CYLINDRICAL_SURFACE ( 'NONE', #36131, 9.250000000000000000 ) ;
#31744 = EDGE_CURVE ( 'NONE', #20296, #1042, #18608, .T. ) ;
#31745 = CARTESIAN_POINT ( 'NONE',  ( 0.07798313963709001262, -81.66790592049099473, 1.406311399563000109 ) ) ;
#31746 = CARTESIAN_POINT ( 'NONE',  ( 7.626500902217000721, -23.31584477285000290, -10.35747158362999976 ) ) ;
#31747 = CARTESIAN_POINT ( 'NONE',  ( -4.670571261811000241, -78.93712829118099705, 8.172940633331000626 ) ) ;
#31749 = CARTESIAN_POINT ( 'NONE',  ( -1.182840957218999955, -1.418543513115000154, -3.838043326965000279 ) ) ;
#31748 = CARTESIAN_POINT ( 'NONE',  ( -3.852741965086999620, -83.09967856441200240, -1.488251573779999948 ) ) ;
#31750 = CARTESIAN_POINT ( 'NONE',  ( 0.9995835529977233902, -82.30208333333331439, 0.7681833999686461523 ) ) ;
#31751 = DIRECTION ( 'NONE',  ( -0.7071067811865475727, 0.000000000000000000, -0.7071067811865475727 ) ) ;
#31752 = EDGE_LOOP ( 'NONE', ( #13042, #36977, #6885 ) ) ;
#31753 = AXIS2_PLACEMENT_3D ( 'NONE', #33249, #1410, #46870 ) ;
#31754 = CARTESIAN_POINT ( 'NONE',  ( -2.404116552999463696, -77.20721653822319297, -10.47761388392037141 ) ) ;
#31755 = LINE ( 'NONE', #19078, #55865 ) ;
#31756 = VERTEX_POINT ( 'NONE', #23588 ) ;
#31757 = AXIS2_PLACEMENT_3D ( 'NONE', #43356, #46945, #56651 ) ;
#31758 = ORIENTED_EDGE ( 'NONE', *, *, #9886, .F. ) ;
#31759 = CARTESIAN_POINT ( 'NONE',  ( -1.499999999971000086, -77.75000000002998490, -1.761798912373000190E-09 ) ) ;
#31760 = CARTESIAN_POINT ( 'NONE',  ( -10.29007107286421885, -76.07604166640594201, -5.929850701927606771 ) ) ;
#31761 = ADVANCED_FACE ( 'NONE', ( #55179 ), #52347, .T. ) ;
#31762 = CARTESIAN_POINT ( 'NONE',  ( -5.701258714434006336, -80.41929545379491628, 9.167358189660777867 ) ) ;
#31763 = CIRCLE ( 'NONE', #39319, 0.8000000000000011546 ) ;
#31764 = ORIENTED_EDGE ( 'NONE', *, *, #53025, .F. ) ;
#31765 = CARTESIAN_POINT ( 'NONE',  ( -11.12530226251999999, -78.15976265171399007, 4.628544181647000322 ) ) ;
#31766 = VECTOR ( 'NONE', #34930, 1000.000000000000000 ) ;
#31767 = ORIENTED_EDGE ( 'NONE', *, *, #43956, .T. ) ;
#31768 = ORIENTED_EDGE ( 'NONE', *, *, #21568, .T. ) ;
#31769 = CARTESIAN_POINT ( 'NONE',  ( 7.342331066867000544, -59.94999999967000548, 8.190859204290999784 ) ) ;
#31770 = CARTESIAN_POINT ( 'NONE',  ( -3.140974612311405512, -78.69583333333332575, 11.68767212001977640 ) ) ;
#31771 = CARTESIAN_POINT ( 'NONE',  ( 0.000000000000000000, -87.25000000009099210, 0.000000000000000000 ) ) ;
#31772 = ORIENTED_EDGE ( 'NONE', *, *, #52223, .T. ) ;
#31773 = CARTESIAN_POINT ( 'NONE',  ( -8.179400488414586334, -54.05908162288749708, -9.502921777750872323 ) ) ;
#31774 = B_SPLINE_CURVE_WITH_KNOTS ( 'NONE', 3,
 ( #4977, #42164, #28265, #54580, #10580, #23559, #1155, #9700, #32694, #19141, #37136, #41866, #14120, #54857, #32116, #27689, #46318, #28564 ),
 .UNSPECIFIED., .F., .F.,
 ( 4, 2, 2, 2, 2, 2, 2, 2, 4 ),
 ( 0.000000000000000000, 0.1250000000000000000, 0.2500000000000000000, 0.3750000000000000000, 0.5000000000000000000, 0.6250000000000000000, 0.7500000000000000000, 0.8750000000000000000, 1.000000000000000000 ),
 .UNSPECIFIED. ) ;
#31775 = VERTEX_POINT ( 'NONE', #36872 ) ;
#31776 = CARTESIAN_POINT ( 'NONE',  ( -0.2692648470245010972, -80.25784302387772584, -1.245099868093910933 ) ) ;
#31777 = CARTESIAN_POINT ( 'NONE',  ( -11.82602479988079303, -79.79999999999998295, -1.911466474616787536 ) ) ;
#31778 = CARTESIAN_POINT ( 'NONE',  ( 10.19022281664999952, -55.60366258855000154, 7.646946378492000207 ) ) ;
#31779 = CARTESIAN_POINT ( 'NONE',  ( -7.678667886032999768, -21.75736537952000305, -10.59548767697000038 ) ) ;
#31780 = CARTESIAN_POINT ( 'NONE',  ( 1.538071403319964281, -77.16458333333332575, 11.75000000000000711 ) ) ;
#31781 = CARTESIAN_POINT ( 'NONE',  ( 11.75000000000000000, -76.55000000000001137, 0.000000000000000000 ) ) ;
#31782 = CARTESIAN_POINT ( 'NONE',  ( 11.81379047889000233, -77.41326435959814489, 1.987564636421000008 ) ) ;
#31783 = CARTESIAN_POINT ( 'NONE',  ( 6.545892007090739817, -78.78773550716071838, -6.535419499853671432 ) ) ;
#31784 = CARTESIAN_POINT ( 'NONE',  ( -10.13694968398000107, -23.70834319340999841, 7.646073915527999532 ) ) ;
#31785 = CARTESIAN_POINT ( 'NONE',  ( 2.425729133266999670E-14, -6.000000000000000000, 0.000000000000000000 ) ) ;
#31786 = CARTESIAN_POINT ( 'NONE',  ( -11.44417895085272008, -76.77916666666666856, 3.075537641221497420 ) ) ;
#31787 = VECTOR ( 'NONE', #35914, 1000.000000000000000 ) ;
#31788 = CARTESIAN_POINT ( 'NONE',  ( -1.492232953141999774, -78.79842549782625838, -3.851191634116000184 ) ) ;
#31790 = EDGE_CURVE ( 'NONE', #7116, #13712, #613, .T. ) ;
#31789 = DIRECTION ( 'NONE',  ( 0.000000000000000000, 1.000000000000000000, 0.000000000000000000 ) ) ;
#31791 = CARTESIAN_POINT ( 'NONE',  ( 3.712057368508056676, -76.26875000000272564, 11.41729714079631819 ) ) ;
#31792 = CARTESIAN_POINT ( 'NONE',  ( 4.324825231101488754, -77.06249999999998579, -8.491324637162149358 ) ) ;
#31793 = CARTESIAN_POINT ( 'NONE',  ( 1.382886570147999983, -24.63098219832000169, 12.65982054476000052 ) ) ;
#31794 = CARTESIAN_POINT ( 'NONE',  ( 3.088701407003000110, -85.59158141794600283, 1.744844263460000100 ) ) ;
#31795 = B_SPLINE_SURFACE_WITH_KNOTS ( 'NONE', 3, 3, ( 
 ( #18522, #53355, #54540, #14081 ),
 ( #40365, #48936, #27062, #26769 ),
 ( #255, #39769, #35624, #57783 ),
 ( #44797, #26197, #4349, #44215 ),
 ( #22350, #58373, #8478, #3763 ),
 ( #17935, #53956, #12901, #30901 ),
 ( #13193, #49227, #45100, #21763 ),
 ( #26473, #19103, #41830, #23812 ) ),
 .UNSPECIFIED., .F., .F., .F.,
 ( 4, 1, 1, 1, 1, 4 ),
 ( 4, 4 ),
 ( -0.01200407345747999885, 0.000000000000000000, 0.3333333333333000081, 0.6666666666667000474, 1.000000000000000000, 1.011997855551999947 ),
 ( -0.3559705542741999906, 1.355970554273999928 ),
 .UNSPECIFIED. ) ;
#31796 = CARTESIAN_POINT ( 'NONE',  ( -3.066224723149000297, -0.9186268662769999649, 2.224133471770000092 ) ) ;
#31797 = CARTESIAN_POINT ( 'NONE',  ( -5.045247388522612120, -78.18634793776142544, -9.528564678276634226 ) ) ;
#31798 = TOROIDAL_SURFACE ( 'NONE', #36532, 17.50000000000000000, 5.000000000000000000 ) ;
#31799 = CARTESIAN_POINT ( 'NONE',  ( 10.01332844635999919, -55.51943307300000185, 7.654537085013999764 ) ) ;
#31800 = CARTESIAN_POINT ( 'NONE',  ( 0.7543631752853537931, -80.51529834865404212, -1.353141125584138793 ) ) ;
#31801 = CARTESIAN_POINT ( 'NONE',  ( -0.9772521179090640775, -78.54668683268188545, 0.7800898177333105421 ) ) ;
#31802 = CARTESIAN_POINT ( 'NONE',  ( 14.00000000000000000, -69.50420297070000686, 0.000000000000000000 ) ) ;
#31803 = CIRCLE ( 'NONE', #8251, 4.000000000000001776 ) ;
#31804 = DIRECTION ( 'NONE',  ( 0.000000000000000000, -1.000000000000000000, 0.000000000000000000 ) ) ;
#31805 = CARTESIAN_POINT ( 'NONE',  ( 9.410240357728000049, -77.31889346392100038, 5.533781925607000218 ) ) ;
#31806 = CARTESIAN_POINT ( 'NONE',  ( -4.989874071371793285, -77.36354942115313804, 9.622404567693822131 ) ) ;
#31807 = DIRECTION ( 'NONE',  ( 0.000000000000000000, -1.000000000000000000, 0.000000000000000000 ) ) ;
#31808 = AXIS2_PLACEMENT_3D ( 'NONE', #17381, #17979, #44539 ) ;
#31810 = CARTESIAN_POINT ( 'NONE',  ( -1.335620631414000004, -77.78332085210550417, 0.2413337786383999983 ) ) ;
#31809 = CARTESIAN_POINT ( 'NONE',  ( -0.1963495408493673156, -79.78541666666667709, 1.499999999999999556 ) ) ;
#31811 = CARTESIAN_POINT ( 'NONE',  ( -0.7740797122817000275, -83.18252381223099690, 1.516913212488000040 ) ) ;
#31812 = EDGE_LOOP ( 'NONE', ( #2467, #26238, #44426, #3226 ) ) ;
#31813 = CARTESIAN_POINT ( 'NONE',  ( -3.559173281348999573, -84.91932450217399264, -0.4647828150262000024 ) ) ;
#31814 = B_SPLINE_CURVE_WITH_KNOTS ( 'NONE', 3,
 ( #44524, #30641, #39514, #11795 ),
 .UNSPECIFIED., .F., .F.,
 ( 4, 4 ),
 ( 0.000000000000000000, 1.000000000000000000 ),
 .UNSPECIFIED. ) ;
#31815 = CARTESIAN_POINT ( 'NONE',  ( -11.92598335260000120, -79.12395855886799723, -0.08230123318516001374 ) ) ;
#31816 = CARTESIAN_POINT ( 'NONE',  ( -2.537458031822000137, -80.74790394668615079, -10.88048998642999976 ) ) ;
#31817 = EDGE_CURVE ( 'NONE', #10196, #26643, #5217, .T. ) ;
#31818 = DIRECTION ( 'NONE',  ( 0.000000000000000000, 0.000000000000000000, -1.000000000000000000 ) ) ;
#31819 = CARTESIAN_POINT ( 'NONE',  ( -11.75000000000000000, -77.70000000000000284, 0.000000000000000000 ) ) ;
#31820 = LINE ( 'NONE', #40990, #51243 ) ;
#31821 = CARTESIAN_POINT ( 'NONE',  ( -9.662137344075999223, -78.31914363189699202, 1.225886475437000023 ) ) ;
#31822 = DIRECTION ( 'NONE',  ( -4.762546956201999894E-11, 1.000000000000000000, 4.762495317921000031E-11 ) ) ;
#31823 = CARTESIAN_POINT ( 'NONE',  ( 6.055527902613000002, -78.11999999999999034, 7.319875806370000682 ) ) ;
#31824 = CARTESIAN_POINT ( 'NONE',  ( -9.546819346760001324, -61.48527546573999558, 8.130850182904000079 ) ) ;
#31825 = CARTESIAN_POINT ( 'NONE',  ( 11.00000000000000355, -78.83958333333332291, -1.439896632895299566 ) ) ;
#31826 = ORIENTED_EDGE ( 'NONE', *, *, #40075, .F. ) ;
#31827 = CARTESIAN_POINT ( 'NONE',  ( -1.722320550011157581, -54.56336311145560103, -12.71171904433065691 ) ) ;
#31828 = CARTESIAN_POINT ( 'NONE',  ( 8.000597322312000159, -79.42353998579800134, 4.965221403244999721 ) ) ;
#31829 = CARTESIAN_POINT ( 'NONE',  ( 8.335705697175322726, -75.88712408948835275, -8.333479323607702938 ) ) ;
#31830 = CARTESIAN_POINT ( 'NONE',  ( -0.8668440880359000733, -77.70303337523669995, -1.013523202003999923 ) ) ;
#31831 = EDGE_CURVE ( 'NONE', #313, #35853, #15783, .T. ) ;
#31832 = FACE_OUTER_BOUND ( 'NONE', #54526, .T. ) ;
#31833 = ORIENTED_EDGE ( 'NONE', *, *, #31817, .F. ) ;
#31834 = CARTESIAN_POINT ( 'NONE',  ( 2.277955858752000129, -78.13434347557100068, -10.97804107101999982 ) ) ;
#31835 = CARTESIAN_POINT ( 'NONE',  ( 10.42531125070999920, -60.06485145371000556, -7.624341767111000756 ) ) ;
#31836 = EDGE_CURVE ( 'NONE', #41593, #15380, #53095, .T. ) ;
#31837 = EDGE_LOOP ( 'NONE', ( #44378, #6088, #6001, #40349 ) ) ;
#31838 = VERTEX_POINT ( 'NONE', #6167 ) ;
#31839 = CARTESIAN_POINT ( 'NONE',  ( -8.199999995296000321, -81.00000000470399186, -2.775962740116999943E-08 ) ) ;
#31840 = CARTESIAN_POINT ( 'NONE',  ( -0.6514213267380000172, -79.71046273805198723, 9.745581310452999801 ) ) ;
#31841 = CIRCLE ( 'NONE', #29945, 4.000000000000000000 ) ;
#31842 = ORIENTED_EDGE ( 'NONE', *, *, #13441, .F. ) ;
#31843 = CARTESIAN_POINT ( 'NONE',  ( -1.937110260509999904, -76.80360561063299940, -12.19981367617000068 ) ) ;
#31844 = CARTESIAN_POINT ( 'NONE',  ( 10.36745710147586230, -23.76601929542621150, -7.635228183621981302 ) ) ;
#31845 = CARTESIAN_POINT ( 'NONE',  ( -1.502510403038999964, -78.72302415856999858, -0.3134361142718999904 ) ) ;
#31846 = VERTEX_POINT ( 'NONE', #34174 ) ;
#31847 = CARTESIAN_POINT ( 'NONE',  ( -8.383077572658999443, -77.59115194988500264, 4.458862939031999595 ) ) ;
#31848 = CIRCLE ( 'NONE', #33756, 1.250000000000000000 ) ;
#31849 = CARTESIAN_POINT ( 'NONE',  ( 0.01540432062990471779, -80.22651900916568479, -1.249598698544762687 ) ) ;
#31850 = CARTESIAN_POINT ( 'NONE',  ( 5.554685856605999561, -76.83457105268000475, 11.87889705760999881 ) ) ;
#31851 = CARTESIAN_POINT ( 'NONE',  ( 9.596002108778172612, -78.99791666666665435, -7.374560639698962028 ) ) ;
#31852 = CARTESIAN_POINT ( 'NONE',  ( -0.5721033155193936404, -86.17851881763701272, 4.600989486740316714 ) ) ;
#31853 = CARTESIAN_POINT ( 'NONE',  ( 9.253844781852635037, -78.97679066890853505, -2.773644284455852649 ) ) ;
#31854 = CARTESIAN_POINT ( 'NONE',  ( 8.176365817920217438, -79.88921606808585807, 4.324880645766660869 ) ) ;
#31855 = CARTESIAN_POINT ( 'NONE',  ( -1.423904377506350016, -24.30512805201053084, 12.50677628656577056 ) ) ;
#31856 = VERTEX_POINT ( 'NONE', #28883 ) ;
#31857 = DIRECTION ( 'NONE',  ( 0.000000000000000000, 0.000000000000000000, 1.000000000000000000 ) ) ;
#31858 = CARTESIAN_POINT ( 'NONE',  ( -11.84062247810999935, -76.52995468096000309, 3.366775603358000080 ) ) ;
#31859 = CARTESIAN_POINT ( 'NONE',  ( -0.2660992726780999629, -80.24172447744500403, 1.492693313845999903 ) ) ;
#31860 = CARTESIAN_POINT ( 'NONE',  ( 1.288803220532000138, -77.92520242672080144, 0.2820490268708999437 ) ) ;
#31861 = CARTESIAN_POINT ( 'NONE',  ( 2.033676212217215618, -3.175283224387012826, 2.872998029602974679 ) ) ;
#31862 = CARTESIAN_POINT ( 'NONE',  ( 7.948089776799000639, -61.24033979686999629, -9.636757666110000287 ) ) ;
#31863 = CARTESIAN_POINT ( 'NONE',  ( -4.802691730569000228, -78.39023052333000408, 11.09149278351999968 ) ) ;
#31864 = CARTESIAN_POINT ( 'NONE',  ( -6.018890980713000438, -76.11744542156999671, 10.70471907396000155 ) ) ;
#31865 = EDGE_CURVE ( 'NONE', #1043, #53170, #29176, .T. ) ;
#31866 = CARTESIAN_POINT ( 'NONE',  ( -7.146006657343000334, -77.38466332859900376, 6.453288637825999707 ) ) ;
#31867 = CARTESIAN_POINT ( 'NONE',  ( 10.05087014954224500, -76.84678485164965878, 6.687395104276451008 ) ) ;
#31868 = CARTESIAN_POINT ( 'NONE',  ( 10.63562707217000103, -80.02573036182266719, 3.563914325689000240 ) ) ;
#31869 = B_SPLINE_SURFACE_WITH_KNOTS ( 'NONE', 3, 3, ( 
 ( #55465, #54598, #14713, #23578 ),
 ( #15312, #19454, #37447, #33305 ),
 ( #50467, #27708, #46922, #32711 ),
 ( #23871, #51341, #28287, #27997 ),
 ( #5570, #28586, #41594, #1174 ),
 ( #55172, #50763, #46336, #5862 ),
 ( #46630, #6160, #24168, #42185 ),
 ( #1753, #10900, #28876, #38035 ),
 ( #7607, #2330, #29450, #25607 ),
 ( #15604, #21181, #56918, #39183 ),
 ( #56628, #47787, #38613, #20893 ) ),
 .UNSPECIFIED., .F., .F., .F.,
 ( 4, 1, 1, 1, 1, 1, 1, 1, 4 ),
 ( 4, 4 ),
 ( -0.02001211456242000045, 0.000000000000000000, 0.1666666666667000196, 0.3333333333333000081, 0.5000000000000000000, 0.6666666666667000474, 0.8333333333333000637, 1.000000000000000000, 1.020273719995999917 ),
 ( -0.3582002740308999900, 1.358863140970000050 ),
 .UNSPECIFIED. ) ;
#31870 = ORIENTED_EDGE ( 'NONE', *, *, #50508, .F. ) ;
#31871 = CARTESIAN_POINT ( 'NONE',  ( -0.6004489902433000070, -82.54813732702999118, -1.340115349862999850 ) ) ;
#31872 = CARTESIAN_POINT ( 'NONE',  ( -12.00000000000000000, -60.04999999966999980, 0.000000000000000000 ) ) ;
#31873 = CARTESIAN_POINT ( 'NONE',  ( -1.092232985442824100, -79.45833333333330017, 0.6295237254636200097 ) ) ;
#31874 = CARTESIAN_POINT ( 'NONE',  ( 4.374544387491000386, -77.15306389129399633, -11.15253550093999912 ) ) ;
#31875 = CARTESIAN_POINT ( 'NONE',  ( 6.737116832614598927, -76.94999999999998863, -6.739285137172449147 ) ) ;
#31876 = CARTESIAN_POINT ( 'NONE',  ( 11.66178877871000097, -78.34363925020198849, 2.537357863477000208 ) ) ;
#31877 = CARTESIAN_POINT ( 'NONE',  ( 4.316051676898999823, -78.90834805011499498, 8.712949996777000550 ) ) ;
#31878 = CARTESIAN_POINT ( 'NONE',  ( 4.710185975415000392, -77.37260406872297835, -8.400437955132002088 ) ) ;
#31879 = AXIS2_PLACEMENT_3D ( 'NONE', #30408, #25982, #30976 ) ;
#31880 = CARTESIAN_POINT ( 'NONE',  ( 2.574494627908628264, -76.05712420562880993, 11.46441856251786717 ) ) ;
#31881 = CARTESIAN_POINT ( 'NONE',  ( -7.180765598437999664, -79.39026687680399164, 8.374863569145000852 ) ) ;
#31882 = CARTESIAN_POINT ( 'NONE',  ( 3.965107357240976071, -85.94828564506400426, 0.4551303408112303273 ) ) ;
#31883 = ORIENTED_EDGE ( 'NONE', *, *, #49680, .F. ) ;
#31884 = CARTESIAN_POINT ( 'NONE',  ( 1.623944433304999935, -76.18552953598467070, -12.20239005717999881 ) ) ;
#31885 = CARTESIAN_POINT ( 'NONE',  ( 2.103055900234938491, -78.40681307385639798, -3.641429946303727405 ) ) ;
#31886 = CARTESIAN_POINT ( 'NONE',  ( -1.297526016723000053, -78.54572183911899685, -10.89864408161000142 ) ) ;
#31887 = CARTESIAN_POINT ( 'NONE',  ( -4.000000000000000000, -5.000000000000000000, 0.5999999999999999778 ) ) ;
#31888 = CARTESIAN_POINT ( 'NONE',  ( 12.50000000000000000, -17.31640971966000109, -1.003652782652999953 ) ) ;
#31889 = CARTESIAN_POINT ( 'NONE',  ( -0.1834469635243000107, -79.21327907014000402, -1.236465612773999911 ) ) ;
#31890 = CARTESIAN_POINT ( 'NONE',  ( 10.75000000000000000, -76.75000000000000000, 0.000000000000000000 ) ) ;
#31891 = VERTEX_POINT ( 'NONE', #52211 ) ;
#31892 = CARTESIAN_POINT ( 'NONE',  ( -2.721343196572999723, -79.67101177224800779, 10.92832355692000057 ) ) ;
#31893 = CARTESIAN_POINT ( 'NONE',  ( 12.70722357733919949, -17.58971352782045017, 1.610228312194780687 ) ) ;
#31894 = PRESENTATION_LAYER_ASSIGNMENT (  '', '', ( #21528 ) ) ;
#31895 = LINE ( 'NONE', #18639, #28262 ) ;
#31896 = CARTESIAN_POINT ( 'NONE',  ( 3.485499217011999828, -78.48547957940618858, -4.268505459544351420E-16 ) ) ;
#31898 = CARTESIAN_POINT ( 'NONE',  ( -1.228243686087402642, -81.58562147598921399, 0.2329788977900838498 ) ) ;
#31897 = CARTESIAN_POINT ( 'NONE',  ( 0.08545339522192001158, -81.02789956585999676, 1.316534626873000047 ) ) ;
#31899 = EDGE_CURVE ( 'NONE', #45259, #35427, #22146, .T. ) ;
#31900 = CARTESIAN_POINT ( 'NONE',  ( -10.88870934378999955, -79.29337123098800078, 1.874540603341000145 ) ) ;
#31901 = CARTESIAN_POINT ( 'NONE',  ( -5.407950800604208297, -76.41666666666667140, 9.358624512123132178 ) ) ;
#31902 = CARTESIAN_POINT ( 'NONE',  ( 1.911540947291000103, -3.081127687535999637, 3.291214574437999918 ) ) ;
#31903 = ADVANCED_FACE ( 'NONE', ( #37752, #47516 ), #10909, .F. ) ;
#31904 = CARTESIAN_POINT ( 'NONE',  ( 0.1963495408493638184, -81.13541666666668561, -1.499999999999999778 ) ) ;
#31905 = CARTESIAN_POINT ( 'NONE',  ( 7.624341764906000130, -55.53514850498000044, 10.42531124851000079 ) ) ;
#31906 = CARTESIAN_POINT ( 'NONE',  ( -2.813789756862300262, -78.39583333333332860, 10.47020627418438465 ) ) ;
#31907 = CARTESIAN_POINT ( 'NONE',  ( -12.77656765293000163, -25.31198129913999750, 0.1555235816856000153 ) ) ;
#31908 = VERTEX_POINT ( 'NONE', #51646 ) ;
#31909 = ORIENTED_EDGE ( 'NONE', *, *, #13062, .T. ) ;
#31910 = CARTESIAN_POINT ( 'NONE',  ( -8.300970689365447797, -78.44166666666664867, -4.784380313523547201 ) ) ;
#31911 = DIRECTION ( 'NONE',  ( 0.000000000000000000, 0.000000000000000000, 1.000000000000000000 ) ) ;
#31912 = EDGE_LOOP ( 'NONE', ( #7310, #7129, #16827, #43397 ) ) ;
#31913 = CARTESIAN_POINT ( 'NONE',  ( -4.800187936532999800, -76.16030212922053977, 10.10109298474000106 ) ) ;
#31914 = CARTESIAN_POINT ( 'NONE',  ( 7.647093862755999893, -23.36895637638999901, 10.00844027276999881 ) ) ;
#31916 = EDGE_CURVE ( 'NONE', #11190, #9459, #3136, .T. ) ;
#31915 = CONICAL_SURFACE ( 'NONE', #6483, 0.6999999997694995590, 0.7853981633972997312 ) ;
#31917 = CARTESIAN_POINT ( 'NONE',  ( 9.770427757074999775, -61.85529868422999300, 8.292768371773000524 ) ) ;
#31918 = CARTESIAN_POINT ( 'NONE',  ( -0.6297930565811739045, -82.51732734865008467, 1.093430612505388311 ) ) ;
#31919 = CARTESIAN_POINT ( 'NONE',  ( -6.514807376190594468, -78.16298481418483846, -6.566430754354078303 ) ) ;
#31920 = CARTESIAN_POINT ( 'NONE',  ( -0.2291600886666000092, -78.38949755890598681, -11.06898422383999936 ) ) ;
#31921 = CARTESIAN_POINT ( 'NONE',  ( -6.090801878186413276, -79.47970282387936436, 7.362514718212188392 ) ) ;
#31922 = ORIENTED_EDGE ( 'NONE', *, *, #20329, .F. ) ;
#31923 = CARTESIAN_POINT ( 'NONE',  ( 7.634645133894655267, -60.27584427251623111, -10.10912661257307477 ) ) ;
#31924 = ORIENTED_EDGE ( 'NONE', *, *, #46695, .F. ) ;
#31925 = CARTESIAN_POINT ( 'NONE',  ( 2.297844492628001500, -77.45516506021056102, 8.961078302872612866 ) ) ;
#31926 = CARTESIAN_POINT ( 'NONE',  ( 6.574300740938999077, -77.54560925314699205, -8.869200617850999890 ) ) ;
#31927 = DIRECTION ( 'NONE',  ( 1.000000000000000000, 0.000000000000000000, -0.000000000000000000 ) ) ;
#31928 = CARTESIAN_POINT ( 'NONE',  ( 5.417083560473000325, -79.06258353067298117, -8.051455326762999576 ) ) ;
#31929 = CARTESIAN_POINT ( 'NONE',  ( 3.629361671790999999, -75.76997015003999536, 11.72003014384999986 ) ) ;
#31930 = CONICAL_SURFACE ( 'NONE', #13097, 1.099999997158000120, 0.7853981633972997312 ) ;
#31931 = CARTESIAN_POINT ( 'NONE',  ( -10.48543666025109289, -78.44166666666666288, -6.043427764450796325 ) ) ;
#31932 = CARTESIAN_POINT ( 'NONE',  ( -1.560595261880000084, -77.74748939621999000, 0.4619550309703999713 ) ) ;
#31933 = CARTESIAN_POINT ( 'NONE',  ( 0.000000000000000000, -87.20000000000000284, -9.699999999999976197 ) ) ;
#31934 = ADVANCED_FACE ( 'NONE', ( #30899 ), #16478, .T. ) ;
#31935 = CARTESIAN_POINT ( 'NONE',  ( 8.838457456548999502, -78.62903382810698361, -6.447440276951000193 ) ) ;
#31936 = CARTESIAN_POINT ( 'NONE',  ( 1.799502287743000029, -60.10716934574000447, -12.60413652834999887 ) ) ;
#31937 = CARTESIAN_POINT ( 'NONE',  ( -8.188331488387625257, -60.02841244176944713, 7.345153731672212416 ) ) ;
#31938 = CARTESIAN_POINT ( 'NONE',  ( 1.972671892376000047, -85.38829592649000233, 3.196865563702000035 ) ) ;
#31939 = ORIENTED_EDGE ( 'NONE', *, *, #44540, .F. ) ;
#31940 = CARTESIAN_POINT ( 'NONE',  ( 3.529477632267000065, -79.79300913277400298, 11.80040848444000012 ) ) ;
#31941 = CARTESIAN_POINT ( 'NONE',  ( 11.23661113560000047, -76.47573121474299285, 2.418095604914000329 ) ) ;
#31942 = CARTESIAN_POINT ( 'NONE',  ( -6.653298097564936953, -78.02821361607915662, 8.446342938638746745 ) ) ;
#31943 = CARTESIAN_POINT ( 'NONE',  ( -11.61454496413000115, -77.68198133620698798, 2.935712811417999557 ) ) ;
#31944 = CARTESIAN_POINT ( 'NONE',  ( 1.636761686205415067, -3.333333333333333481, 2.839805762151342616 ) ) ;
#31945 = CARTESIAN_POINT ( 'NONE',  ( -12.00000000000000000, -23.25000000000000000, -1.250000000000000000 ) ) ;
#31946 = DIRECTION ( 'NONE',  ( 0.000000000000000000, -1.000000000000000000, 0.000000000000000000 ) ) ;
#31947 = CARTESIAN_POINT ( 'NONE',  ( 7.768420291617568196, -80.91093204606768552, 7.431500403707722135 ) ) ;
#31948 = CARTESIAN_POINT ( 'NONE',  ( 9.372653703366999878, -78.83658701837899230, 0.8742135494153999709 ) ) ;
#31949 = CARTESIAN_POINT ( 'NONE',  ( -3.380118192975993807, -85.79678895079199208, 1.504925579246014111 ) ) ;
#31950 = CARTESIAN_POINT ( 'NONE',  ( 4.249074618647000534, -77.04725762008598622, -10.30533674824999935 ) ) ;
#31951 = CARTESIAN_POINT ( 'NONE',  ( -1.570796326794938524, -78.18541666666665435, 11.99999999999999645 ) ) ;
#31952 = CARTESIAN_POINT ( 'NONE',  ( 1.917328231603999900, -80.31995460502288608, 10.85776984013000046 ) ) ;
#31953 = VERTEX_POINT ( 'NONE', #53352 ) ;
#31954 = FACE_OUTER_BOUND ( 'NONE', #50977, .T. ) ;
#31955 = B_SPLINE_CURVE_WITH_KNOTS ( 'NONE', 3,
 ( #15601, #33877, #46919, #15309, #24462, #19745, #47505, #42474, #15010, #20044, #36352, #54380, #13918, #9499, #10598, #37740, #28583, #46626, #55763, #33302 ),
 .UNSPECIFIED., .F., .F.,
 ( 4, 2, 2, 2, 2, 2, 2, 2, 2, 4 ),
 ( 0.000000000000000000, 0.1250000000000000555, 0.2500000000000001110, 0.3750000000000001665, 0.5000000000000002220, 0.5625000000000002220, 0.6250000000000002220, 0.7500000000000002220, 0.8750000000000001110, 1.000000000000000000 ),
 .UNSPECIFIED. ) ;
#31956 = DIRECTION ( 'NONE',  ( 0.000000000000000000, -1.000000000000000000, 0.000000000000000000 ) ) ;
#31957 = CARTESIAN_POINT ( 'NONE',  ( 3.549182112775000064, -1.939138932809999938, -1.374451376799000091 ) ) ;
#31958 = AXIS2_PLACEMENT_3D ( 'NONE', #10168, #10454, #29312 ) ;
#31959 = CARTESIAN_POINT ( 'NONE',  ( -2.185791986076000004, -77.80771032744199545, -11.00183730042999919 ) ) ;
#31960 = CARTESIAN_POINT ( 'NONE',  ( 9.611650271896843734, -79.90833333333331723, -5.539808784079876425 ) ) ;
#31961 = DIRECTION ( 'NONE',  ( 0.000000000000000000, 0.000000000000000000, -1.000000000000000000 ) ) ;
#31962 = CARTESIAN_POINT ( 'NONE',  ( 0.000000000000000000, 4.040000000000000036, 0.000000000000000000 ) ) ;
#31963 = DIRECTION ( 'NONE',  ( 0.000000000000000000, -1.000000000000000000, 0.000000000000000000 ) ) ;
#31964 = CARTESIAN_POINT ( 'NONE',  ( 12.54983130239999944, -16.94901607458999848, 0.1356732392833999989 ) ) ;
#31965 = CARTESIAN_POINT ( 'NONE',  ( -1.752823108115999950, -84.95894503318798741, -3.786512042056999761 ) ) ;
#31966 = AXIS2_PLACEMENT_3D ( 'NONE', #20965, #12110, #8255 ) ;
#31967 = CARTESIAN_POINT ( 'NONE',  ( -10.22919423528282046, -76.04999999999999716, 5.911015989525015613 ) ) ;
#31968 = CARTESIAN_POINT ( 'NONE',  ( 9.389188763448000685, -54.08956227294000740, -8.194870530143999687 ) ) ;
#31969 = CARTESIAN_POINT ( 'NONE',  ( 11.12204776531999961, -77.46418423053899005, 0.7447510167176000229 ) ) ;
#31970 = CARTESIAN_POINT ( 'NONE',  ( -1.542698325316999908, -81.23958015220999584, 0.6290719308543000210 ) ) ;
#31971 = CARTESIAN_POINT ( 'NONE',  ( 0.1781252944802999838, -77.69575938543998461, 1.522910005212999796 ) ) ;
#31972 = CARTESIAN_POINT ( 'NONE',  ( 1.930860503475322121, -60.57417505891291398, 12.72930866334770705 ) ) ;
#31973 = CARTESIAN_POINT ( 'NONE',  ( 1.381772510957646194, -82.96659326553100300, -0.6148152531492157014 ) ) ;
#31974 = AXIS2_PLACEMENT_3D ( 'NONE', #50947, #55068, #36760 ) ;
#31975 = CARTESIAN_POINT ( 'NONE',  ( -12.77651065753999937, -62.10896598063000340, -0.04308629978602999955 ) ) ;
#31976 = CARTESIAN_POINT ( 'NONE',  ( -8.864117045829161157, -80.14852009318845205, -6.142631186442469193 ) ) ;
#31977 = CARTESIAN_POINT ( 'NONE',  ( 5.940599228801999379E-14, -5.899999999999999467, -13.99999999999886491 ) ) ;
#31978 = CARTESIAN_POINT ( 'NONE',  ( -12.70556836347999941, -16.77227722772000007, 1.774192816106000118E-09 ) ) ;
#31979 = CIRCLE ( 'NONE', #31035, 5.100000000000000533 ) ;
#31980 = ORIENTED_EDGE ( 'NONE', *, *, #40478, .F. ) ;
#31981 = CARTESIAN_POINT ( 'NONE',  ( 9.298479816477872362, -53.91187382742512568, 8.385858173805548432 ) ) ;
#31982 = FACE_OUTER_BOUND ( 'NONE', #42616, .T. ) ;
#31983 = CARTESIAN_POINT ( 'NONE',  ( -10.97184146967999929, -79.37701249839500406, 1.968068935562000243 ) ) ;
#31984 = CARTESIAN_POINT ( 'NONE',  ( 1.092232985442823212, -80.20833333333332860, -0.6295237254636224522 ) ) ;
#31985 = ORIENTED_EDGE ( 'NONE', *, *, #14180, .F. ) ;
#31986 = VERTEX_POINT ( 'NONE', #25616 ) ;
#31987 = DIRECTION ( 'NONE',  ( 0.000000000000000000, 1.000000000000000000, 0.000000000000000000 ) ) ;
#31988 = ORIENTED_EDGE ( 'NONE', *, *, #28484, .T. ) ;
#31989 = CARTESIAN_POINT ( 'NONE',  ( -1.370379768245999841E-14, -74.59999999999999432, 0.000000000000000000 ) ) ;
#31990 = ORIENTED_EDGE ( 'NONE', *, *, #46126, .F. ) ;
#31991 = FACE_OUTER_BOUND ( 'NONE', #13733, .T. ) ;
#31992 = DIRECTION ( 'NONE',  ( 0.000000000000000000, 1.000000000000000000, 0.000000000000000000 ) ) ;
#31993 = EDGE_CURVE ( 'NONE', #13771, #51311, #46121, .T. ) ;
#31994 = DIRECTION ( 'NONE',  ( 0.000000000000000000, 1.000000000000000000, 0.000000000000000000 ) ) ;
#31995 = CARTESIAN_POINT ( 'NONE',  ( 0.9212224518303999687, -24.81954101839000160, -12.54670315981999984 ) ) ;
#31996 = CARTESIAN_POINT ( 'NONE',  ( -2.532729724196000287, -81.70032136754298335, 2.543427862400999828 ) ) ;
#31997 = CARTESIAN_POINT ( 'NONE',  ( 11.99999999979999821, -18.85000000927000130, 0.7999999997951999786 ) ) ;
#31998 = CARTESIAN_POINT ( 'NONE',  ( -5.373789810023999358, -78.83213957653998705, -10.63267532885000044 ) ) ;
#31999 = VERTEX_POINT ( 'NONE', #53068 ) ;
#32000 = ORIENTED_EDGE ( 'NONE', *, *, #9972, .F. ) ;
#32001 = CARTESIAN_POINT ( 'NONE',  ( -4.000000000000000000, -77.29999999999999716, 0.000000000000000000 ) ) ;
#32002 = CARTESIAN_POINT ( 'NONE',  ( -1.749899258077675324, -18.61283151237003963, -12.55433901290727405 ) ) ;
#32003 = CYLINDRICAL_SURFACE ( 'NONE', #11068, 1.500000000000000000 ) ;
#32004 = CARTESIAN_POINT ( 'NONE',  ( -1.248430190247999949, -79.26167243909000604, 0.06262635289305999720 ) ) ;
#32005 = CARTESIAN_POINT ( 'NONE',  ( -4.475245744599999576, -78.79640326627398395, -8.610626265545000990 ) ) ;
#32006 = DIRECTION ( 'NONE',  ( 0.000000000000000000, -1.000000000000000000, 0.000000000000000000 ) ) ;
#32007 = CARTESIAN_POINT ( 'NONE',  ( -1.746263085257492076, -86.01534311877844630, 3.604194403367339650 ) ) ;
#32008 = CARTESIAN_POINT ( 'NONE',  ( 12.36191581903000092, -76.56064262049000035, -3.311046255921999748 ) ) ;
#32009 = EDGE_CURVE ( 'NONE', #43036, #38390, #41933, .T. ) ;
#32010 = CARTESIAN_POINT ( 'NONE',  ( -1.468405992501000012, -81.17584665853000558, 0.5987774653158000060 ) ) ;
#32011 = CARTESIAN_POINT ( 'NONE',  ( -12.49306752634999995, -23.28056692670000061, -1.667917367010000040 ) ) ;
#32012 = CARTESIAN_POINT ( 'NONE',  ( -0.6999999999999999556, -21.00000000000000000, 11.90000000000000036 ) ) ;
#32013 = CARTESIAN_POINT ( 'NONE',  ( -2.945856725507999929, -81.56849421602200323, 2.958299893872000208 ) ) ;
#32014 = CARTESIAN_POINT ( 'NONE',  ( -2.895922040489999905, -80.09400592890570181, 10.88681414971999928 ) ) ;
#32015 = CARTESIAN_POINT ( 'NONE',  ( -9.067070616629999691, -78.97593667140100138, 3.715721191563000403 ) ) ;
#32016 = CARTESIAN_POINT ( 'NONE',  ( -11.75000000000000178, -78.29297251775329869, 1.037641870170390002 ) ) ;
#32017 = CARTESIAN_POINT ( 'NONE',  ( 3.225488960277000050, -79.36632046129089701, -1.476744291601000070 ) ) ;
#32018 = CIRCLE ( 'NONE', #29197, 2.000000000000000000 ) ;
#32019 = CARTESIAN_POINT ( 'NONE',  ( -1.256362333281000110, -77.70789370475868907, 0.2270125678640999844 ) ) ;
#32020 = DIRECTION ( 'NONE',  ( 1.000000000000000000, 0.000000000000000000, 0.000000000000000000 ) ) ;
#32021 = CARTESIAN_POINT ( 'NONE',  ( -9.421357847594000745, -80.38007146547629134, -6.176342950743000770 ) ) ;
#32022 = ADVANCED_FACE ( 'NONE', ( #44212 ), #7119, .F. ) ;
#32023 = CARTESIAN_POINT ( 'NONE',  ( 8.437633008360455378, -77.19999999999998863, -6.805276374351061364 ) ) ;
#32024 = ORIENTED_EDGE ( 'NONE', *, *, #17429, .F. ) ;
#32025 = CARTESIAN_POINT ( 'NONE',  ( 0.000000000000000000, -74.64999999999999147, 0.000000000000000000 ) ) ;
#32026 = CARTESIAN_POINT ( 'NONE',  ( -0.5999999999999999778, -18.84999999999999787, -10.98362417419999915 ) ) ;
#32027 = ADVANCED_FACE ( 'NONE', ( #30032 ), #45782, .F. ) ;
#32028 = DIRECTION ( 'NONE',  ( 0.000000000000000000, 1.000000000000000000, 0.000000000000000000 ) ) ;
#32029 = CARTESIAN_POINT ( 'NONE',  ( 0.000000000000000000, -74.64999999999999147, 0.000000000000000000 ) ) ;
#32030 = CARTESIAN_POINT ( 'NONE',  ( 1.667961430005999945, -57.05111654290000445, 12.58335110165999993 ) ) ;
#32031 = CARTESIAN_POINT ( 'NONE',  ( 5.647598101448999763, -77.85660919792000811, 11.72364604052000203 ) ) ;
#32032 = CARTESIAN_POINT ( 'NONE',  ( -8.697106840384998705, -79.54218667140099797, -4.132666167052000183 ) ) ;
#32033 = CARTESIAN_POINT ( 'NONE',  ( 9.850513606030963487, -17.69492088480771841, 7.836738268704446675 ) ) ;
#32034 = ORIENTED_EDGE ( 'NONE', *, *, #16089, .F. ) ;
#32035 = CARTESIAN_POINT ( 'NONE',  ( -9.319163437353997992, -77.78947964090998823, -6.149666482694000180 ) ) ;
#32036 = CIRCLE ( 'NONE', #33937, 14.00000000000000000 ) ;
#32037 = CARTESIAN_POINT ( 'NONE',  ( -0.6245130753102998700, -81.38575740106399792, -1.262448629235000119 ) ) ;
#32038 = FACE_BOUND ( 'NONE', #3748, .T. ) ;
#32039 = CARTESIAN_POINT ( 'NONE',  ( 8.881263526186000234, -77.73629938523899341, 3.434171575746000293 ) ) ;
#32041 = CARTESIAN_POINT ( 'NONE',  ( 4.010845454633999552, -1.493904343864000062, -0.2065758488482999922 ) ) ;
#32040 = CARTESIAN_POINT ( 'NONE',  ( -3.935772911773000704, -85.98568853081499697, 0.4301246578429000489 ) ) ;
#32042 = DIRECTION ( 'NONE',  ( 1.000000000000000000, 0.000000000000000000, 0.000000000000000000 ) ) ;
#32043 = CYLINDRICAL_SURFACE ( 'NONE', #45326, 1.750000000000001332 ) ;
#32044 = ADVANCED_FACE ( 'NONE', ( #3199, #21189 ), #57204, .F. ) ;
#32045 = ORIENTED_EDGE ( 'NONE', *, *, #26796, .F. ) ;
#32046 = CARTESIAN_POINT ( 'NONE',  ( -2.388504738132872340, -77.20733432141381058, -10.48118357590753291 ) ) ;
#32047 = CARTESIAN_POINT ( 'NONE',  ( -1.199500263597270244, -78.95208333333333428, -0.9218200799623728070 ) ) ;
#32048 = DIRECTION ( 'NONE',  ( 0.000000000000000000, 1.000000000000000000, 0.000000000000000000 ) ) ;
#32049 = ORIENTED_EDGE ( 'NONE', *, *, #57492, .F. ) ;
#32050 = ORIENTED_EDGE ( 'NONE', *, *, #43438, .T. ) ;
#32051 = CARTESIAN_POINT ( 'NONE',  ( 4.025753977166000475, -79.52580109776799588, -10.17256709246999868 ) ) ;
#32052 = DIRECTION ( 'NONE',  ( 0.000000000000000000, -1.000000000000000000, 0.000000000000000000 ) ) ;
#32053 = FACE_OUTER_BOUND ( 'NONE', #10895, .T. ) ;
#32054 = VERTEX_POINT ( 'NONE', #57780 ) ;
#32055 = CARTESIAN_POINT ( 'NONE',  ( -1.368150018649999966, -77.80708155120599656, -11.97179757597999838 ) ) ;
#32056 = ORIENTED_EDGE ( 'NONE', *, *, #31001, .F. ) ;
#32057 = B_SPLINE_SURFACE_WITH_KNOTS ( 'NONE', 3, 3, ( 
 ( #54867, #16895, #14414, #4477, #877, #30734, #22179, #30453, #57907, #50458, #36855, #52907, #53782, #48771, #26023, #26315, #5561, #17461, #53193, #35449, #27988, #32413, #18863, #46037, #8903, #10010, #21884, #35159, #22476, #41294, #44328, #57613, #41585, #53481, #8027, #49058, #44052, #3600, #17173, #8316, #3883, #26895, #39892, #31020, #40187, #8606, #26592, #44628, #4182, #58201, #17764, #35751, #13317, #46620, #47496, #11181, #28278, #33869, #56334, #38022, #56045, #15886, #15594, #55455, #33589, #46329, #37732 ),
 ( #6440, #10591, #32997, #50752, #20034, #5853, #51910, #11470, #28575, #29441, #10297, #6149, #23859, #55756, #51627, #41875, #24158, #51044, #28866, #1452, #7023, #15300, #24454, #42175, #25026, #10889, #1743, #15001, #29157, #46912, #42468, #19446, #19737, #37439, #47206, #6736, #33295, #51332, #1164, #2035, #24742, #42757, #2321, #20317, #38313, #19151, #37147, #55159, #14705, #32704, #48347, #57764, #56910, #48633, #17321, #48071, #21465, #35307, #30307, #30016, #30886, #53050, #25313, #8459, #2608, #17038, #12604 ),
 ( #16465, #38603, #56618, #16177, #34446, #34156, #52195, #12037, #7600, #43620, #3183, #21173, #16756, #34735, #7886, #54804, #44480, #41222, #9354, #27630, #22924, #811, #22036, #22333, #40646, #36783, #49208, #18794, #4924, #13762, #49806, #27341, #40939, #54227, #31765, #35607, #45673, #18502, #14061, #45379, #18218, #526, #22634, #14345, #53939, #26456, #31169, #32055, #32342, #50390, #23214, #58059, #9060, #8759, #4030, #26751, #4330, #40042, #17619, #44780, #36497, #27044, #54524, #53634, #40348, #5212, #58356 ),
 ( #17918, #50099, #13172, #45082, #35907, #13470, #31466, #9643, #49510, #4633, #238, #36209, #10520, #46259, #28503, #20251, #24675, #51554, #38242, #1969, #47136, #6078, #42398, #1099, #55382, #1380, #37662, #14637, #56262, #24084, #15228, #37366, #15814, #19662, #19374, #5786, #19963, #55677, #33220, #32629, #37072, #42102, #14928, #32924, #46552, #37951, #1672, #50683, #42685, #51265, #41514, #10819, #33803, #10225, #55974, #50967, #45966, #28796, #46843, #2250, #15525, #33519, #6371, #24386, #9936, #28203, #6664 ) ),
 .UNSPECIFIED., .F., .F., .F.,
 ( 4, 4 ),
 ( 4, 1, 1, 1, 1, 1, 1, 1, 1, 1, 1, 1, 1, 1, 1, 1, 1, 1, 1, 1, 1, 1, 1, 1, 1, 1, 1, 1, 1, 1, 1, 1, 1, 1, 1, 1, 1, 1, 1, 1, 1, 1, 1, 1, 1, 1, 1, 1, 1, 1, 1, 1, 1, 1, 1, 1, 1, 1, 1, 1, 1, 1, 1, 1, 4 ),
 ( -0.1772706441294000235, 1.177270644128999955 ),
 ( -0.02000000000000000042, -0.003749999999999999861, 0.01250000000000000069, 0.02875000000000000125, 0.04499999999999999833, 0.06124999999999999889, 0.07749999999999999944, 0.09375000000000000000, 0.1100000000000000006, 0.1262500000000000011, 0.1424999999999999878, 0.1587500000000000022, 0.1749999999999999889, 0.1912500000000000033, 0.2074999999999999900, 0.2237500000000000044, 0.2399999999999999911, 0.2562499999999999778, 0.2725000000000000200, 0.2887500000000000067, 0.3049999999999999933, 0.3212499999999999800, 0.3375000000000000222, 0.3537500000000000089, 0.3699999999999999956, 0.3862499999999999822, 0.4025000000000000244, 0.4187500000000000111, 0.4349999999999999978, 0.4512499999999999845, 0.4675000000000000266, 0.4837500000000000133, 0.5000000000000000000, 0.5162499999999999867, 0.5324999999999999734, 0.5487499999999999600, 0.5649999999999999467, 0.5812500000000000444, 0.5975000000000000311, 0.6137500000000000178, 0.6300000000000000044, 0.6462499999999999911, 0.6624999999999999778, 0.6787499999999999645, 0.6949999999999999512, 0.7112500000000000488, 0.7275000000000000355, 0.7437500000000000222, 0.7600000000000000089, 0.7762499999999999956, 0.7924999999999999822, 0.8087499999999999689, 0.8249999999999999556, 0.8412500000000000533, 0.8575000000000000400, 0.8737500000000000266, 0.8900000000000000133, 0.9062500000000000000, 0.9224999999999999867, 0.9387499999999999734, 0.9549999999999999600, 0.9712499999999999467, 0.9875000000000000444, 1.003749999999999920, 1.020000000000000018 ),
 .UNSPECIFIED. ) ;
#32058 = VERTEX_POINT ( 'NONE', #3761 ) ;
#32059 = VECTOR ( 'NONE', #8717, 1000.000000000000000 ) ;
#32060 = VECTOR ( 'NONE', #9693, 1000.000000000000000 ) ;
#32061 = CARTESIAN_POINT ( 'NONE',  ( -1.192446808648067735, -2.695995745449793812, -3.022765882159190731 ) ) ;
#32062 = CIRCLE ( 'NONE', #52844, 9.549999999999998934 ) ;
#32063 = CARTESIAN_POINT ( 'NONE',  ( -12.00000000000000000, -78.79999999999999716, 0.000000000000000000 ) ) ;
#32064 = CARTESIAN_POINT ( 'NONE',  ( 9.425400508419963685, -79.15997041332948925, 1.202743096264716982 ) ) ;
#32065 = B_SPLINE_CURVE_WITH_KNOTS ( 'NONE', 3,
 ( #15677, #29242, #10977, #7682, #33674, #7393, #15967, #29812, #48151, #51711, #12115, #47289, #43136, #42551, #28956, #39262, #6817, #25683 ),
 .UNSPECIFIED., .F., .F.,
 ( 4, 2, 2, 2, 2, 2, 2, 2, 4 ),
 ( 0.000000000000000000, 0.1250000000000000833, 0.2500000000000001665, 0.3750000000000001665, 0.5000000000000002220, 0.6250000000000002220, 0.7500000000000001110, 0.8750000000000001110, 1.000000000000000000 ),
 .UNSPECIFIED. ) ;
#32066 = VERTEX_POINT ( 'NONE', #9659 ) ;
#32067 = CARTESIAN_POINT ( 'NONE',  ( 1.234997842510089372, -82.83803313528682111, -0.1925883613549776718 ) ) ;
#32068 = EDGE_LOOP ( 'NONE', ( #18953, #53378, #46777, #43112, #40867, #54513, #5156, #22722 ) ) ;
#32069 = CARTESIAN_POINT ( 'NONE',  ( -0.6379005857648086808, -79.73309412273128771, -1.103986640637640848 ) ) ;
#32070 = CARTESIAN_POINT ( 'NONE',  ( -0.03734840871947565227, -78.85171438276199751, -3.962636352599350875 ) ) ;
#32071 = DIRECTION ( 'NONE',  ( -3.552713678801000121E-14, 1.000000000000000000, 3.403984144012999683E-13 ) ) ;
#32072 = CARTESIAN_POINT ( 'NONE',  ( -7.860507001410999450, -76.70312894181100205, 7.955276143908999842 ) ) ;
#32073 = LINE ( 'NONE', #5511, #8976 ) ;
#32074 = ADVANCED_FACE ( 'NONE', ( #45985, #9073 ), #41239, .T. ) ;
#32075 = CARTESIAN_POINT ( 'NONE',  ( 3.075537641221509411, -78.65416666666668277, 11.44417895085272008 ) ) ;
#32076 = CARTESIAN_POINT ( 'NONE',  ( 8.027846440818999341, -76.63502291188399340, 7.850949632255998623 ) ) ;
#32077 = CARTESIAN_POINT ( 'NONE',  ( 0.003320946630736449148, -78.72517372709556582, -9.249912909581682996 ) ) ;
#32078 = CARTESIAN_POINT ( 'NONE',  ( 11.48655120864317425, -76.46745349848808360, 2.565345163985293553 ) ) ;
#32079 = CIRCLE ( 'NONE', #27410, 14.00000000000000000 ) ;
#32080 = EDGE_CURVE ( 'NONE', #17178, #33530, #14362, .T. ) ;
#32081 = CARTESIAN_POINT ( 'NONE',  ( -0.5847500590555335664, -23.30655143820058228, -10.98448857562232028 ) ) ;
#32082 = CARTESIAN_POINT ( 'NONE',  ( -1.319155384867000125, -80.12260285397499615, 0.1959724986398999891 ) ) ;
#32083 = CARTESIAN_POINT ( 'NONE',  ( 1.210716439189422733, -77.73555344446525339, -9.249687892553014379 ) ) ;
#32084 = CARTESIAN_POINT ( 'NONE',  ( 10.50409585618203501, -78.24416319518880414, 5.966360771605526025 ) ) ;
#32085 = CARTESIAN_POINT ( 'NONE',  ( 0.6322550835224000076, -81.80853455456798429, -3.912310357318999454 ) ) ;
#32086 = FACE_OUTER_BOUND ( 'NONE', #21466, .T. ) ;
#32087 = CARTESIAN_POINT ( 'NONE',  ( -9.299222834567000717, -77.67151332859899071, 2.587993818716000316 ) ) ;
#32088 = CARTESIAN_POINT ( 'NONE',  ( 1.250000000000000000, -79.73860658917831756, -0.1789672786810340421 ) ) ;
#32089 = CARTESIAN_POINT ( 'NONE',  ( -13.79999999994999982, 4.699973049637762301E-11, -2.072309110287000051E-09 ) ) ;
#32090 = CARTESIAN_POINT ( 'NONE',  ( -1.761265949708000100, -23.70858218785999938, 12.57448205042999945 ) ) ;
#32091 = CARTESIAN_POINT ( 'NONE',  ( 11.80100040496257563, -79.25000000000001421, -2.513071059627543846 ) ) ;
#32092 = CARTESIAN_POINT ( 'NONE',  ( 8.067746785342526650, -79.99999999999998579, 4.933239913214655381 ) ) ;
#32093 = CARTESIAN_POINT ( 'NONE',  ( -1.116072162164000181, -1.569750604645999914, -3.621394142857999654 ) ) ;
#32094 = CARTESIAN_POINT ( 'NONE',  ( 0.6295237254636211199, -80.83333333333334281, 1.092232985442824322 ) ) ;
#32095 = EDGE_CURVE ( 'NONE', #12885, #29148, #18811, .T. ) ;
#32096 = CARTESIAN_POINT ( 'NONE',  ( 10.04115011118999945, -56.03513569577999931, 7.682331425181999407 ) ) ;
#32097 = CARTESIAN_POINT ( 'NONE',  ( 0.7146743994145193790, -79.68530190706071892, 1.333844887466810292 ) ) ;
#32098 = DIRECTION ( 'NONE',  ( -1.000000000000000000, 0.000000000000000000, 0.000000000000000000 ) ) ;
#32099 = DIRECTION ( 'NONE',  ( 3.788597347406000047E-11, 1.000000000000000000, 0.000000000000000000 ) ) ;
#32100 = CARTESIAN_POINT ( 'NONE',  ( -3.634457760627999523, -77.27231996340199771, 11.72972702006000034 ) ) ;
#32101 = CARTESIAN_POINT ( 'NONE',  ( -14.00000000000000000, -9.295797029142999435, 3.101241903103999638E-11 ) ) ;
#32103 = CARTESIAN_POINT ( 'NONE',  ( 0.6064284284549000814, -78.95748627212400095, -1.281524057860000010 ) ) ;
#32102 = DIRECTION ( 'NONE',  ( 0.000000000000000000, -1.000000000000000000, 0.000000000000000000 ) ) ;
#32104 = CARTESIAN_POINT ( 'NONE',  ( 1.413069887183999951, -81.91918203637000317, -0.7194652256120001033 ) ) ;
#32105 = VERTEX_POINT ( 'NONE', #54538 ) ;
#32106 = CARTESIAN_POINT ( 'NONE',  ( 3.478486924372000022, -84.19782450217398662, 0.8853622020908999968 ) ) ;
#32107 = CARTESIAN_POINT ( 'NONE',  ( 4.140345854158000272, -79.47019575988599627, 11.18451558619000075 ) ) ;
#32108 = CARTESIAN_POINT ( 'NONE',  ( -10.60751049107999933, -80.05066853420788675, 3.116614351438999897 ) ) ;
#32109 = CARTESIAN_POINT ( 'NONE',  ( -1.980584515752000119, -55.53514853344000102, -12.76303204600000107 ) ) ;
#32110 = CARTESIAN_POINT ( 'NONE',  ( -2.243884148121614075, -84.90520834277080553, -2.611532020247723906 ) ) ;
#32111 = CARTESIAN_POINT ( 'NONE',  ( -9.998780405325002008, -77.37132423095599165, -5.083552005986999411 ) ) ;
#32112 = CARTESIAN_POINT ( 'NONE',  ( 9.546819346421999697, -24.68527546640000025, -8.130850183241999929 ) ) ;
#32113 = DIRECTION ( 'NONE',  ( 1.000000000000000000, 0.000000000000000000, 0.000000000000000000 ) ) ;
#32114 = FACE_OUTER_BOUND ( 'NONE', #50089, .T. ) ;
#32115 = CARTESIAN_POINT ( 'NONE',  ( 11.00000000000000000, -78.94999999999998863, -1.064824513673000067E-14 ) ) ;
#32116 = CARTESIAN_POINT ( 'NONE',  ( -10.01013066307207744, -76.15416666665846890, 4.451642991118897719 ) ) ;
#32117 = ORIENTED_EDGE ( 'NONE', *, *, #29786, .T. ) ;
#32118 = CARTESIAN_POINT ( 'NONE',  ( -1.318114156661947423, -54.06427522772299454, -12.70261578158667248 ) ) ;
#32119 = CARTESIAN_POINT ( 'NONE',  ( 8.158537514794998557, -79.33773998579800946, -4.701213835425000376 ) ) ;
#32120 = DIRECTION ( 'NONE',  ( 0.000000000000000000, 0.000000000000000000, 1.000000000000000000 ) ) ;
#32121 = CARTESIAN_POINT ( 'NONE',  ( 0.8912423865758999364, -77.95109649214209924, 0.9921004264782997684 ) ) ;
#32122 = CARTESIAN_POINT ( 'NONE',  ( -12.64502302235999842, -56.02870851050000311, -1.799490220168999954 ) ) ;
#32123 = CARTESIAN_POINT ( 'NONE',  ( 10.98362417419999915, -23.15000000000000213, 0.5999999999999999778 ) ) ;
#32124 = VERTEX_POINT ( 'NONE', #27358 ) ;
#32125 = CIRCLE ( 'NONE', #6692, 11.05000000000000071 ) ;
#32126 = DIRECTION ( 'NONE',  ( 0.000000000000000000, 1.000000000000000000, 0.000000000000000000 ) ) ;
#32127 = VERTEX_POINT ( 'NONE', #1401 ) ;
#32128 = EDGE_CURVE ( 'NONE', #14347, #44860, #20194, .T. ) ;
#32129 = ORIENTED_EDGE ( 'NONE', *, *, #22513, .T. ) ;
#32130 = CARTESIAN_POINT ( 'NONE',  ( -1.130640822228425435, -80.56483172200898935, 0.5346059543193828478 ) ) ;
#32131 = CARTESIAN_POINT ( 'NONE',  ( 6.653382217586999658, -79.82567319065550748, 7.150748904218000135 ) ) ;
#32132 = EDGE_LOOP ( 'NONE', ( #8404, #23323, #38637, #34534 ) ) ;
#32133 = DIRECTION ( 'NONE',  ( 0.000000000000000000, 1.000000000000000000, 0.000000000000000000 ) ) ;
#32134 = DIRECTION ( 'NONE',  ( 1.000000000000000000, 0.000000000000000000, 0.000000000000000000 ) ) ;
#32135 = B_SPLINE_CURVE_WITH_KNOTS ( 'NONE', 3,
 ( #5467, #5754, #41776, #9905, #14897, #32604, #32895, #46816, #27886, #10487, #1067, #14608, #45934, #51526, #37629, #37920, #11083, #28472 ),
 .UNSPECIFIED., .F., .F.,
 ( 4, 2, 2, 2, 2, 2, 2, 2, 4 ),
 ( 0.000000000000000000, 0.1250000000000000000, 0.2500000000000000000, 0.3750000000000000000, 0.5000000000000000000, 0.6250000000000000000, 0.7500000000000000000, 0.8750000000000000000, 1.000000000000000000 ),
 .UNSPECIFIED. ) ;
#32136 = CARTESIAN_POINT ( 'NONE',  ( -1.379901750132000116, -78.67059258879000083, 0.6720497516175000241 ) ) ;
#32137 = ORIENTED_EDGE ( 'NONE', *, *, #4076, .T. ) ;
#32138 = CARTESIAN_POINT ( 'NONE',  ( -8.123853732960998997, -77.02664805011499993, 4.915330883505999893 ) ) ;
#32139 = B_SPLINE_CURVE_WITH_KNOTS ( 'NONE', 3,
 ( #36395, #33915, #6192, #49999 ),
 .UNSPECIFIED., .F., .F.,
 ( 4, 4 ),
 ( 0.000000000000000000, 1.000000000000000000 ),
 .UNSPECIFIED. ) ;
#32140 = CIRCLE ( 'NONE', #40638, 12.50000000000000000 ) ;
#32141 = CARTESIAN_POINT ( 'NONE',  ( -1.150140635162034908, -80.13221033398477289, -0.4892649414430590427 ) ) ;
#32142 = CARTESIAN_POINT ( 'NONE',  ( -9.359366689070000689, -77.55613138518998539, -9.185202947203000790 ) ) ;
#32143 = CARTESIAN_POINT ( 'NONE',  ( -3.399999999999999911, -78.67389998024768261, 5.715921273723000819E-07 ) ) ;
#32144 = CARTESIAN_POINT ( 'NONE',  ( 6.922407739197930177, -79.90780257099709161, 6.135667632505162672 ) ) ;
#32145 = CARTESIAN_POINT ( 'NONE',  ( 4.039219890226469545, -79.43229165378355106, -0.3057202085838180983 ) ) ;
#32146 = ORIENTED_EDGE ( 'NONE', *, *, #21764, .F. ) ;
#32147 = CARTESIAN_POINT ( 'NONE',  ( 7.596835002782697188, -77.60208333333335418, 5.838193839761710358 ) ) ;
#32148 = EDGE_CURVE ( 'NONE', #27639, #5204, #53845, .T. ) ;
#32149 = CARTESIAN_POINT ( 'NONE',  ( 5.894077591580000330, -76.64739919339000096, -10.80721126921000064 ) ) ;
#32150 = CARTESIAN_POINT ( 'NONE',  ( 0.3985939703966000502, -79.55290681445698908, -1.564707112294000169 ) ) ;
#32151 = CARTESIAN_POINT ( 'NONE',  ( 0.8323291101560614802, -2.493205130203935749, -3.480095087541390519 ) ) ;
#32152 = CARTESIAN_POINT ( 'NONE',  ( 7.658900562732000594, -60.00940503048000352, -10.01676248783999945 ) ) ;
#32153 = CARTESIAN_POINT ( 'NONE',  ( 12.21456857099000004, -78.76020556754998836, -1.096995930408000142 ) ) ;
#32154 = LINE ( 'NONE', #44580, #13083 ) ;
#32155 = CARTESIAN_POINT ( 'NONE',  ( 7.648026768008000076, -55.55000001556999933, -10.12290050216000026 ) ) ;
#32156 = CARTESIAN_POINT ( 'NONE',  ( 5.344729029608000559, -77.70731498579799279, 7.975868177029001416 ) ) ;
#32157 = CARTESIAN_POINT ( 'NONE',  ( 9.229604799106443380, -76.85567982616369420, 7.771863644200966981 ) ) ;
#32158 = CARTESIAN_POINT ( 'NONE',  ( 2.039250879084999912, -79.88954864681358004, -11.02993955029000084 ) ) ;
#32159 = EDGE_CURVE ( 'NONE', #36426, #17327, #32073, .T. ) ;
#32160 = ORIENTED_EDGE ( 'NONE', *, *, #29906, .F. ) ;
#32161 = CARTESIAN_POINT ( 'NONE',  ( 10.69999999999999929, -77.19999999999998863, 0.000000000000000000 ) ) ;
#32162 = CARTESIAN_POINT ( 'NONE',  ( -12.50000000000000000, -18.75000000310999937, 1.750000000000000000 ) ) ;
#32163 = CARTESIAN_POINT ( 'NONE',  ( -1.750000000001000089, -56.04899163641999849, -12.60354432391000046 ) ) ;
#32164 = CARTESIAN_POINT ( 'NONE',  ( 0.3271848554490964789, -82.85416666666665719, 1.217465845835395521 ) ) ;
#32165 = CARTESIAN_POINT ( 'NONE',  ( 6.233080334754680152, -77.00000000000000000, 6.909364586181893308 ) ) ;
#32166 = CARTESIAN_POINT ( 'NONE',  ( -10.82689242272999941, -77.61114773376000642, -5.021344731552000340 ) ) ;
#32167 = CARTESIAN_POINT ( 'NONE',  ( -6.715271092063999525, -77.77053767652898841, -6.903502308617000871 ) ) ;
#32168 = CARTESIAN_POINT ( 'NONE',  ( 0.3917937483749863725, -76.07213746520410780, 11.74425345321102299 ) ) ;
#32169 = CARTESIAN_POINT ( 'NONE',  ( 9.125560752801000319, -79.73035737123599631, -5.991619725684000031 ) ) ;
#32170 = CARTESIAN_POINT ( 'NONE',  ( 4.177667811529485853, -85.80681307385597734, 0.4795288509369720620 ) ) ;
#32171 = ORIENTED_EDGE ( 'NONE', *, *, #45223, .F. ) ;
#32172 = CARTESIAN_POINT ( 'NONE',  ( 1.980584515756000030, -18.73514849905999924, -12.76303204340999997 ) ) ;
#32173 = CARTESIAN_POINT ( 'NONE',  ( 3.621447497674998850, -78.40681307385639798, -2.137281964302801374 ) ) ;
#32174 = CARTESIAN_POINT ( 'NONE',  ( -14.00000000000000000, -46.13782243168999742, -5.544480864478000239E-06 ) ) ;
#32175 = AXIS2_PLACEMENT_3D ( 'NONE', #57560, #7686, #39839 ) ;
#32176 = CARTESIAN_POINT ( 'NONE',  ( 10.87588596538000019, -79.72971893809699395, -1.476184626237000197 ) ) ;
#32177 = DIRECTION ( 'NONE',  ( 0.000000000000000000, 1.000000000000000000, 0.000000000000000000 ) ) ;
#32178 = CARTESIAN_POINT ( 'NONE',  ( 9.441578396167999543, -76.68030949943998564, 8.198205470971000608 ) ) ;
#32179 = PLANE ( 'NONE',  #30243 ) ;
#32180 = CARTESIAN_POINT ( 'NONE',  ( 9.389188763474001220, -17.28956227326999695, -8.194870530173000489 ) ) ;
#32181 = DIRECTION ( 'NONE',  ( 0.7071067812087692417, 2.829525585096875613E-07, -0.7071067811642691714 ) ) ;
#32182 = EDGE_LOOP ( 'NONE', ( #58136, #19213, #47238, #53641, #39532, #50173, #23288, #33150, #53492, #24459, #47137 ) ) ;
#32183 = CIRCLE ( 'NONE', #20862, 4.000000000000000888 ) ;
#32184 = CARTESIAN_POINT ( 'NONE',  ( 5.828547835402000388, -78.37764927275399884, -9.501726143737000640 ) ) ;
#32185 = FACE_BOUND ( 'NONE', #39286, .T. ) ;
#32186 = CARTESIAN_POINT ( 'NONE',  ( -7.763928192766062608, -79.61790123138683839, -8.933202951673855807 ) ) ;
#32187 = CARTESIAN_POINT ( 'NONE',  ( -1.157498849743237246, -81.56938687382739772, 0.4716165995993014670 ) ) ;
#32188 = CARTESIAN_POINT ( 'NONE',  ( 6.124581921013000141, -78.47869295534098910, -9.196052954390001588 ) ) ;
#32189 = CARTESIAN_POINT ( 'NONE',  ( 12.50659871789738276, -61.77347219457124083, -0.3508073943565040431 ) ) ;
#32190 = DIRECTION ( 'NONE',  ( 0.9999476293090542312, 0.000000000000000000, 0.01023418971888952027 ) ) ;
#32191 = EDGE_CURVE ( 'NONE', #6077, #11225, #14648, .T. ) ;
#32192 = CARTESIAN_POINT ( 'NONE',  ( -0.9218200799623716968, -81.07291666666667140, -1.199500263597270910 ) ) ;
#32193 = CARTESIAN_POINT ( 'NONE',  ( 0.000000000000000000, -3.749999999256000027, 0.000000000000000000 ) ) ;
#32194 = EDGE_CURVE ( 'NONE', #42541, #3955, #27836, .T. ) ;
#32195 = CARTESIAN_POINT ( 'NONE',  ( -10.90777360733681789, -78.95896512884534957, -1.219956472363630917 ) ) ;
#32196 = CARTESIAN_POINT ( 'NONE',  ( 1.570796326794857478, -77.16458333333332575, 12.00000000000000533 ) ) ;
#32197 = ORIENTED_EDGE ( 'NONE', *, *, #29942, .T. ) ;
#32198 = ORIENTED_EDGE ( 'NONE', *, *, #2631, .T. ) ;
#32199 = CARTESIAN_POINT ( 'NONE',  ( -4.855043705795098141, -77.81750000000000966, 8.214633846514278304 ) ) ;
#32200 = PRESENTATION_LAYER_ASSIGNMENT (  '', '', ( #57667 ) ) ;
#32201 = CARTESIAN_POINT ( 'NONE',  ( 8.337885974442610149, -78.79578023353073490, -6.785440158440498415 ) ) ;
#32202 = B_SPLINE_CURVE_WITH_KNOTS ( 'NONE', 3,
 ( #23735, #754, #28148, #46788, #10171, #46200, #5725, #19026, #50910, #19602, #45904, #18733, #10458, #46494, #50326, #41456, #54463, #40875 ),
 .UNSPECIFIED., .F., .F.,
 ( 4, 2, 2, 2, 2, 2, 2, 2, 4 ),
 ( 0.000000000000000000, 0.1250000000000000000, 0.2499999999999999722, 0.3750000000000000000, 0.5000000000000000000, 0.6250000000000000000, 0.7500000000000000000, 0.8750000000000000000, 1.000000000000000000 ),
 .UNSPECIFIED. ) ;
#32203 = ORIENTED_EDGE ( 'NONE', *, *, #568, .F. ) ;
#32204 = CARTESIAN_POINT ( 'NONE',  ( -1.660522255173999984, -76.63685902701352859, 11.05968181062000077 ) ) ;
#32205 = CARTESIAN_POINT ( 'NONE',  ( 1.602084971415322467, -82.70833334961002947, 3.011342165955993799 ) ) ;
#32206 = CARTESIAN_POINT ( 'NONE',  ( 7.646092217304000904, -60.50851177880000620, 10.13691708059000085 ) ) ;
#32207 = CARTESIAN_POINT ( 'NONE',  ( 12.50000000000000000, -55.54999999966999980, 0.000000000000000000 ) ) ;
#32208 = CARTESIAN_POINT ( 'NONE',  ( -8.557286188203086397, -77.61159000152036924, -8.384082802621019681 ) ) ;
#32209 = CARTESIAN_POINT ( 'NONE',  ( 5.622824352109999424, -80.00067888228510071, -9.705769245306999693 ) ) ;
#32210 = CARTESIAN_POINT ( 'NONE',  ( 1.924380748938630393E-07, -79.75000000000001421, -9.249538042332323684 ) ) ;
#32211 = EDGE_LOOP ( 'NONE', ( #57424, #44335, #57536, #31690 ) ) ;
#32212 = CARTESIAN_POINT ( 'NONE',  ( -10.36745710147586230, -23.76601929542621150, 7.635228183621981302 ) ) ;
#32213 = VERTEX_POINT ( 'NONE', #27060 ) ;
#32214 = EDGE_CURVE ( 'NONE', #25015, #26696, #18422, .T. ) ;
#32215 = CARTESIAN_POINT ( 'NONE',  ( 2.655231642783967949, -77.45200555099675910, 8.860774034763510443 ) ) ;
#32216 = CARTESIAN_POINT ( 'NONE',  ( -1.776188306762000124, -77.54229276148697636, -10.89629776253999971 ) ) ;
#32217 = CARTESIAN_POINT ( 'NONE',  ( -8.022734517049746273E-06, -82.01564364893640402, -1.484164386985079798 ) ) ;
#32218 = VECTOR ( 'NONE', #42099, 999.9999999999998863 ) ;
#32219 = CARTESIAN_POINT ( 'NONE',  ( 1.260641617779999946, -77.75508739074000175, 9.621927669549000584 ) ) ;
#32220 = LINE ( 'NONE', #5952, #20991 ) ;
#32221 = CARTESIAN_POINT ( 'NONE',  ( -10.75000000000000355, -80.98958333333331439, 1.407171709420384609 ) ) ;
#32222 = CARTESIAN_POINT ( 'NONE',  ( -1.491326706514000122, -77.74395464212999229, -0.6515838025032999470 ) ) ;
#32223 = CARTESIAN_POINT ( 'NONE',  ( -10.49924843836999955, -80.51978164716398112, -4.054558598941000014 ) ) ;
#32224 = CARTESIAN_POINT ( 'NONE',  ( -7.484260875330000395, -78.99423443443198778, -7.979577400219000083 ) ) ;
#32225 = CARTESIAN_POINT ( 'NONE',  ( 2.062670899361999766, -60.10639784916000394, -12.83044027763000017 ) ) ;
#32226 = CARTESIAN_POINT ( 'NONE',  ( 12.83044039277999993, -60.10639625617000092, -2.062670899148999926 ) ) ;
#32227 = ADVANCED_FACE ( 'NONE', ( #28224 ), #50702, .F. ) ;
#32228 = CARTESIAN_POINT ( 'NONE',  ( -2.279403987710999946, -83.35175613119999127, -2.714643365851999945 ) ) ;
#32229 = ORIENTED_EDGE ( 'NONE', *, *, #35938, .F. ) ;
#32230 = CARTESIAN_POINT ( 'NONE',  ( 4.696081959528999761, -78.78500883819499734, 11.38644304057999967 ) ) ;
#32231 = CARTESIAN_POINT ( 'NONE',  ( 10.73633472751000006, -76.36434026635200212, -3.758393515045000299 ) ) ;
#32232 = CARTESIAN_POINT ( 'NONE',  ( 9.586126626853495480, -77.88753870104096677, 4.864810896429621501 ) ) ;
#32233 = ADVANCED_FACE ( 'NONE', ( #18520 ), #8036, .F. ) ;
#32234 = CARTESIAN_POINT ( 'NONE',  ( -10.47513558174000003, -18.19636614430000066, 7.624778818008999259 ) ) ;
#32235 = LINE ( 'NONE', #31652, #714 ) ;
#32236 = CARTESIAN_POINT ( 'NONE',  ( -1.250013176831791695, -78.10006463709670754, 4.053087819277079897E-06 ) ) ;
#32237 = CARTESIAN_POINT ( 'NONE',  ( -7.608915353569000395, -77.52909087844598446, 5.542165790529000269 ) ) ;
#32238 = CARTESIAN_POINT ( 'NONE',  ( -5.884117869723990424, -86.02148120184399716, -4.839282714492908255 ) ) ;
#32239 = CARTESIAN_POINT ( 'NONE',  ( -2.295071999339000079, -77.78263888113500002, 10.90812747857000176 ) ) ;
#32240 = CARTESIAN_POINT ( 'NONE',  ( -3.630949683904999947, -76.04999999999999716, 11.17491406647000041 ) ) ;
#32241 = CARTESIAN_POINT ( 'NONE',  ( -8.119375762549999820, -81.01799444111729542, -7.459417917149000488 ) ) ;
#32242 = EDGE_LOOP ( 'NONE', ( #7114, #4565, #45153, #24586 ) ) ;
#32243 = LINE ( 'NONE', #19277, #32460 ) ;
#32244 = CARTESIAN_POINT ( 'NONE',  ( 1.540744644154000031, -2.148872700496999855, 3.654751654090000024 ) ) ;
#32245 = CARTESIAN_POINT ( 'NONE',  ( -7.849238557987999521, -76.63654757836398801, 7.706455349885999340 ) ) ;
#32246 = CARTESIAN_POINT ( 'NONE',  ( 10.31626776183999894, -78.09212595279097968, -3.746764721243999841 ) ) ;
#32247 = CARTESIAN_POINT ( 'NONE',  ( 8.227501432777001966, -24.82538814609000255, -9.516269854983999466 ) ) ;
#32248 = LINE ( 'NONE', #45577, #21317 ) ;
#32249 = CARTESIAN_POINT ( 'NONE',  ( 0.8522304910899691777, -1.955669459018320122, 3.167342208975652440 ) ) ;
#32250 = CARTESIAN_POINT ( 'NONE',  ( -1.249999996278000181, -76.50000000037098857, -0.4999999996289999915 ) ) ;
#32251 = B_SPLINE_CURVE_WITH_KNOTS ( 'NONE', 3,
 ( #34270, #20997, #16863, #34844 ),
 .UNSPECIFIED., .F., .F.,
 ( 4, 4 ),
 ( 0.000000000000000000, 1.000000000000000000 ),
 .UNSPECIFIED. ) ;
#32252 = CARTESIAN_POINT ( 'NONE',  ( 4.172307908842999957, -85.43994503318799616, 0.04369406100051999309 ) ) ;
#32253 = EDGE_CURVE ( 'NONE', #39245, #22854, #13490, .T. ) ;
#32254 = CARTESIAN_POINT ( 'NONE',  ( 0.7554284705563509839, -79.66666666666668561, -1.310679582531385945 ) ) ;
#32255 = DIRECTION ( 'NONE',  ( 0.000000000000000000, 1.000000000000000000, 0.000000000000000000 ) ) ;
#32256 = CARTESIAN_POINT ( 'NONE',  ( -1.331888048429999971, -78.29475676510899973, -11.18726993471000064 ) ) ;
#32257 = CARTESIAN_POINT ( 'NONE',  ( -1.603789611582999930, -80.29219192556000451, -0.4506860216877000558 ) ) ;
#32258 = CARTESIAN_POINT ( 'NONE',  ( -1.280656172315000063, -79.50047497536000662, 0.3202611811242000450 ) ) ;
#32259 = CARTESIAN_POINT ( 'NONE',  ( 9.596002108778145967, -77.60208333333332575, 7.374560639699001996 ) ) ;
#32260 = CARTESIAN_POINT ( 'NONE',  ( 0.2394845634073196894, -81.38761288777696734, -1.493279160396979721 ) ) ;
#32261 = CIRCLE ( 'NONE', #23804, 11.05000000000000071 ) ;
#32262 = CARTESIAN_POINT ( 'NONE',  ( 1.251175831454664156, -83.14694854564174875, 0.8506124265937500262 ) ) ;
#32263 = CARTESIAN_POINT ( 'NONE',  ( -7.599813437125216176, -80.16297796562771794, -7.602572481944763538 ) ) ;
#32264 = CARTESIAN_POINT ( 'NONE',  ( -1.243547092045951041, -77.91458333333331154, -9.500000000000000000 ) ) ;
#32265 = EDGE_CURVE ( 'NONE', #42393, #5429, #57396, .T. ) ;
#32266 = ORIENTED_EDGE ( 'NONE', *, *, #38780, .F. ) ;
#32267 = EDGE_CURVE ( 'NONE', #17032, #23858, #539, .T. ) ;
#32268 = CARTESIAN_POINT ( 'NONE',  ( -1.154629675336898531, -81.63141643927103530, -0.4786478767419468094 ) ) ;
#32269 = VECTOR ( 'NONE', #20413, 1000.000000000000000 ) ;
#32270 = CARTESIAN_POINT ( 'NONE',  ( -5.360806944915999850, -79.97621204443510123, -9.773246618612999370 ) ) ;
#32271 = FACE_OUTER_BOUND ( 'NONE', #26445, .T. ) ;
#32272 = ORIENTED_EDGE ( 'NONE', *, *, #23041, .T. ) ;
#32273 = ORIENTED_EDGE ( 'NONE', *, *, #56086, .T. ) ;
#32274 = CARTESIAN_POINT ( 'NONE',  ( -0.1262356271553999876, -81.22059099503800894, -1.412134535654999912 ) ) ;
#32275 = VERTEX_POINT ( 'NONE', #11707 ) ;
#32276 = ORIENTED_EDGE ( 'NONE', *, *, #42593, .T. ) ;
#32277 = CARTESIAN_POINT ( 'NONE',  ( 10.75000000000000000, -77.35000000000000853, 0.000000000000000000 ) ) ;
#32278 = VECTOR ( 'NONE', #45956, 1000.000000000000000 ) ;
#32279 = CARTESIAN_POINT ( 'NONE',  ( 9.500000000000000000, -91.89999999999999147, -7.290811810668999158E-14 ) ) ;
#32280 = CARTESIAN_POINT ( 'NONE',  ( 3.194519230552451905, -80.85833332211321078, -1.285379839507373667 ) ) ;
#32281 = AXIS2_PLACEMENT_3D ( 'NONE', #15134, #23993, #54710 ) ;
#32282 = CARTESIAN_POINT ( 'NONE',  ( 5.202079365288874158, -78.27269934739146606, -7.648514488450266491 ) ) ;
#32283 = CARTESIAN_POINT ( 'NONE',  ( 0.000000000000000000, -23.25000000000000000, -12.00000000000000000 ) ) ;
#32284 = ORIENTED_EDGE ( 'NONE', *, *, #33310, .F. ) ;
#32285 = ORIENTED_EDGE ( 'NONE', *, *, #7335, .T. ) ;
#32286 = CARTESIAN_POINT ( 'NONE',  ( 5.246383657897999875, -77.06100733245999379, -10.79237965019999912 ) ) ;
#32287 = DIRECTION ( 'NONE',  ( 0.000000000000000000, 0.000000000000000000, 1.000000000000000000 ) ) ;
#32288 = DIRECTION ( 'NONE',  ( -1.000000000000000000, 0.000000000000000000, 0.000000000000000000 ) ) ;
#32289 = CARTESIAN_POINT ( 'NONE',  ( -9.626984307556000431, -78.19950285456599204, 1.221426423741999834 ) ) ;
#32290 = CARTESIAN_POINT ( 'NONE',  ( -1.181111693982000110, -79.27654225787900089, -0.4092372983238000139 ) ) ;
#32291 = CARTESIAN_POINT ( 'NONE',  ( -10.53101990620000095, -23.30639784948999704, 7.613962745608000127 ) ) ;
#32292 = CARTESIAN_POINT ( 'NONE',  ( 12.32442898454999813, -77.55972615780000012, -3.452188809138999837 ) ) ;
#32293 = CARTESIAN_POINT ( 'NONE',  ( 6.644230831661016801, -77.23692193750341062, -6.715582363013730571 ) ) ;
#32294 = DIRECTION ( 'NONE',  ( 0.000000000000000000, 1.000000000000000000, 0.000000000000000000 ) ) ;
#32295 = CARTESIAN_POINT ( 'NONE',  ( -5.178558594642320934, -76.61041601060691164, 10.57677830698726851 ) ) ;
#32296 = CARTESIAN_POINT ( 'NONE',  ( -4.168302257862000815, -80.17668722926399028, 0.1879600432223000051 ) ) ;
#32298 = AXIS2_PLACEMENT_3D ( 'NONE', #29838, #25710, #47890 ) ;
#32297 = CARTESIAN_POINT ( 'NONE',  ( 5.620590082324000036, -80.43267365621458964, -9.763102121971000358 ) ) ;
#32299 = CARTESIAN_POINT ( 'NONE',  ( 4.349579488465999511, -78.84528667140098435, 8.780633650160998727 ) ) ;
#32300 = CARTESIAN_POINT ( 'NONE',  ( 3.249790610657787848, -2.854537099176947201, 0.1710447749874229040 ) ) ;
#32301 = DIRECTION ( 'NONE',  ( -0.009503199022040095811, 0.000000000000000000, 0.9999548435846228323 ) ) ;
#32302 = CARTESIAN_POINT ( 'NONE',  ( -1.295435361468000091, -77.78474280459130341, -0.3166359884281000348 ) ) ;
#32303 = CARTESIAN_POINT ( 'NONE',  ( 9.579193661067588295, -77.49808761060164386, -7.313663711862211869 ) ) ;
#32304 = DIRECTION ( 'NONE',  ( -1.000000000000000000, 0.000000000000000000, 0.000000000000000000 ) ) ;
#32305 = B_SPLINE_CURVE_WITH_KNOTS ( 'NONE', 3,
 ( #14725, #18598, #45466, #5008, #45172, #23883, #40734, #45763, #28297, #14146, #1474, #23013, #19463, #36587, #899, #325, #4723, #37459, #54608, #15025, #23591, #49603, #9150, #28010, #32145, #18303, #50185, #22721, #27719, #5297, #23307, #36296, #41314, #32723, #18880, #19175, #36876, #54887, #14437, #55183, #50774, #32432, #50477, #10029, #46057, #42196, #51067, #56642, #33318, #47799, #37756, #55777, #47520, #10615, #38909, #28889, #46937, #2628, #1766, #38625, #7049, #16200, #2343, #20060, #20907, #33892, #56928, #11771, #43349, #11491, #29464, #7331, #25047, #6462, #43069, #19759, #15326, #51354, #20625, #28596, #33020, #34178, #10912, #52214, #29746, #38047, #51932, #25332 ),
 .UNSPECIFIED., .F., .F.,
 ( 4, 2, 2, 2, 2, 2, 1, 2, 2, 2, 2, 2, 2, 2, 2, 2, 2, 2, 2, 2, 2, 2, 2, 2, 2, 2, 2, 2, 2, 2, 2, 2, 2, 2, 2, 2, 2, 2, 1, 2, 2, 2, 2, 2, 4 ),
 ( 0.000000000000000000, 0.01562500000000002776, 0.03125000000000005551, 0.04687500000000008327, 0.06250000000000011102, 0.07812500000000012490, 0.09375000000000013878, 0.1093750000000001388, 0.1250000000000001388, 0.1406250000000001388, 0.1562500000000001388, 0.1718750000000001388, 0.1875000000000001388, 0.2187500000000001388, 0.2500000000000001110, 0.2812500000000001110, 0.3125000000000001110, 0.3437500000000001110, 0.3750000000000001110, 0.4062500000000000555, 0.4375000000000000000, 0.4687499999999999445, 0.4999999999999998890, 0.5312499999999997780, 0.5624999999999997780, 0.5937499999999996669, 0.6249999999999996669, 0.6562499999999995559, 0.6874999999999995559, 0.7187499999999994449, 0.7499999999999995559, 0.7812499999999995559, 0.8124999999999996669, 0.8281249999999996669, 0.8437499999999996669, 0.8593749999999997780, 0.8749999999999997780, 0.8906249999999997780, 0.9062499999999997780, 0.9218749999999998890, 0.9374999999999998890, 0.9531249999999998890, 0.9687499999999998890, 0.9843750000000000000, 1.000000000000000000 ),
 .UNSPECIFIED. ) ;
#32306 = CARTESIAN_POINT ( 'NONE',  ( -0.8385792221450999451, -2.924655184951000297, -3.712528424878000166 ) ) ;
#32307 = CARTESIAN_POINT ( 'NONE',  ( 1.092232985442823212, -79.20833333333331439, -0.6295237254636224522 ) ) ;
#32308 = ORIENTED_EDGE ( 'NONE', *, *, #24040, .T. ) ;
#32309 = CARTESIAN_POINT ( 'NONE',  ( 9.243123480653681057, -61.71653773532028708, 8.441201026288084108 ) ) ;
#32310 = CARTESIAN_POINT ( 'NONE',  ( 7.452378523309729275, -60.34721902435785523, -8.090910852015744226 ) ) ;
#32311 = CARTESIAN_POINT ( 'NONE',  ( 1.537589725670525764, -77.56258520800980705, 11.74337905373031532 ) ) ;
#32312 = CARTESIAN_POINT ( 'NONE',  ( 1.930989144707000005, -58.55365779174999830, 12.80900240954000147 ) ) ;
#32313 = CARTESIAN_POINT ( 'NONE',  ( 12.55073801092999908, -77.17672481401000084, -3.437763296274999991 ) ) ;
#32314 = CARTESIAN_POINT ( 'NONE',  ( -6.658246499064939705, -79.52821171827558544, 8.443780454546217840 ) ) ;
#32315 = CIRCLE ( 'NONE', #14419, 4.100000000000000533 ) ;
#32316 = ADVANCED_FACE ( 'NONE', ( #15247 ), #28815, .F. ) ;
#32317 = CARTESIAN_POINT ( 'NONE',  ( 9.027693294681998992, -79.16251332859900458, -3.653265801962000126 ) ) ;
#32318 = CARTESIAN_POINT ( 'NONE',  ( 9.609171231144982173, -78.49653939831271998, 6.760579772709885304 ) ) ;
#32319 = EDGE_LOOP ( 'NONE', ( #15458, #48010, #20603, #23936, #35849 ) ) ;
#32320 = AXIS2_PLACEMENT_3D ( 'NONE', #10279, #41570, #41278 ) ;
#32321 = DIRECTION ( 'NONE',  ( -0.6489586469986102779, 0.04890178910784081373, -0.7592504787669123179 ) ) ;
#32322 = EDGE_CURVE ( 'NONE', #50939, #2832, #45384, .T. ) ;
#32323 = CARTESIAN_POINT ( 'NONE',  ( -0.9778317140632999394, -77.36108401092899101, -11.12245703213999981 ) ) ;
#32324 = CARTESIAN_POINT ( 'NONE',  ( -0.7112551523747999704, -81.49650077651999425, -1.437797105698000122 ) ) ;
#32325 = DIRECTION ( 'NONE',  ( 0.7071067811705344930, 1.925105116903093482E-07, 0.7071067812025343402 ) ) ;
#32326 = CARTESIAN_POINT ( 'NONE',  ( -3.790141024232000166, -78.11283724644100346, -8.616613344227999960 ) ) ;
#32328 = CARTESIAN_POINT ( 'NONE',  ( 3.981113306789000106, -1.056808102910000047, -0.5296481109823999445 ) ) ;
#32327 = CARTESIAN_POINT ( 'NONE',  ( -3.886561630247999943, -84.55426028386798976, 1.524548671433000102 ) ) ;
#32329 = CARTESIAN_POINT ( 'NONE',  ( -1.667961445601999992, -58.54800977479000323, -12.58338334669999981 ) ) ;
#32330 = CARTESIAN_POINT ( 'NONE',  ( -1.249999999999999778, -82.51041666666662877, -0.1636246173744686228 ) ) ;
#32331 = CARTESIAN_POINT ( 'NONE',  ( -0.3926218265389255779, -81.39583333333337123, 1.460959015002472494 ) ) ;
#32332 = VERTEX_POINT ( 'NONE', #11416 ) ;
#32333 = LINE ( 'NONE', #27907, #42828 ) ;
#32334 = CARTESIAN_POINT ( 'NONE',  ( 1.310679582531388387, -79.10833333333333428, -0.7554284705563470981 ) ) ;
#32335 = EDGE_LOOP ( 'NONE', ( #55646, #15306, #12759 ) ) ;
#32337 = EDGE_CURVE ( 'NONE', #20296, #54955, #12322, .T. ) ;
#32336 = ORIENTED_EDGE ( 'NONE', *, *, #11339, .T. ) ;
#32338 = CARTESIAN_POINT ( 'NONE',  ( 0.000000000000000000, -9.295797029142999435, 0.000000000000000000 ) ) ;
#32339 = SURFACE_STYLE_USAGE ( .BOTH. , #40039 ) ;
#32340 = DIRECTION ( 'NONE',  ( 1.000000000000000000, 0.000000000000000000, 0.000000000000000000 ) ) ;
#32341 = VERTEX_POINT ( 'NONE', #20270 ) ;
#32342 = CARTESIAN_POINT ( 'NONE',  ( -5.292199200464000164, -77.77995223578199102, -10.82535908394999957 ) ) ;
#32343 = AXIS2_PLACEMENT_3D ( 'NONE', #56370, #48100, #37772 ) ;
#32344 = ORIENTED_EDGE ( 'NONE', *, *, #43659, .T. ) ;
#32345 = ORIENTED_EDGE ( 'NONE', *, *, #2842, .T. ) ;
#32346 = CARTESIAN_POINT ( 'NONE',  ( -0.7260205774406525148, -2.708476618800434998, -3.168507982638361309 ) ) ;
#32347 = ADVANCED_FACE ( 'NONE', ( #38263 ), #38555, .F. ) ;
#32348 = ORIENTED_EDGE ( 'NONE', *, *, #38954, .T. ) ;
#32349 = CIRCLE ( 'NONE', #339, 1.750000000000000000 ) ;
#32350 = CARTESIAN_POINT ( 'NONE',  ( -2.718916690774999534, -78.85393255997098549, -2.277985697799999709 ) ) ;
#32351 = CARTESIAN_POINT ( 'NONE',  ( 10.45205659047999980, -59.56232685193999998, 7.651160337235999975 ) ) ;
#32352 = ADVANCED_FACE ( 'NONE', ( #38843 ), #33492, .F. ) ;
#32353 = ORIENTED_EDGE ( 'NONE', *, *, #15329, .T. ) ;
#32354 = LINE ( 'NONE', #10235, #41250 ) ;
#32355 = ORIENTED_EDGE ( 'NONE', *, *, #2068, .T. ) ;
#32356 = CARTESIAN_POINT ( 'NONE',  ( -9.393203674808267678, -80.54166666666665719, -5.413904038987171319 ) ) ;
#32357 = CARTESIAN_POINT ( 'NONE',  ( 9.690624391480906041, -78.59567732945993157, -0.5153898459522678888 ) ) ;
#32358 = CARTESIAN_POINT ( 'NONE',  ( -11.87945358116625094, -79.79999999999999716, -1.588021400056299548 ) ) ;
#32359 = VECTOR ( 'NONE', #29138, 1000.000000000000000 ) ;
#32360 = CARTESIAN_POINT ( 'NONE',  ( 1.250000000000000000, -83.24999999999998579, 0.000000000000000000 ) ) ;
#32361 = CARTESIAN_POINT ( 'NONE',  ( -8.096452064242996016, -22.78578169018999944, 13.15643568217000769 ) ) ;
#32362 = CARTESIAN_POINT ( 'NONE',  ( -10.67244467921999984, -76.74493217846000448, 2.904229794498999873 ) ) ;
#32363 = DIRECTION ( 'NONE',  ( 0.000000000000000000, 1.000000000000000000, 0.000000000000000000 ) ) ;
#32364 = VECTOR ( 'NONE', #13604, 1000.000000000000000 ) ;
#32365 = CARTESIAN_POINT ( 'NONE',  ( -7.718368845804999268, -57.05199022587000002, -10.07722254368999870 ) ) ;
#32366 = CARTESIAN_POINT ( 'NONE',  ( -1.608690456112285672, -78.71114049471292162, -9.109175791259589872 ) ) ;
#32367 = CARTESIAN_POINT ( 'NONE',  ( 6.792517171462394643, -76.52567734522683907, 9.587677660702928151 ) ) ;
#32368 = CARTESIAN_POINT ( 'NONE',  ( 1.980584515752000119, -23.26485146623999967, -12.76303204602000108 ) ) ;
#32369 = CARTESIAN_POINT ( 'NONE',  ( -0.6056189234361001317, -80.22182810073799430, -1.188192690176999911 ) ) ;
#32370 = CARTESIAN_POINT ( 'NONE',  ( -9.274707012308825327, -80.14539018384232349, -5.914949570800462908 ) ) ;
#32371 = CARTESIAN_POINT ( 'NONE',  ( 2.256974249120885290, -78.09294649791769416, -11.85744693861532539 ) ) ;
#32372 = CARTESIAN_POINT ( 'NONE',  ( 0.5519595447327000359, -78.91867549782628544, -4.093147992351998887 ) ) ;
#32373 = CARTESIAN_POINT ( 'NONE',  ( 5.848847972528999684, -77.01631332859899715, 7.678821120301999592 ) ) ;
#32374 = CARTESIAN_POINT ( 'NONE',  ( -12.46164872708000004, -18.32834420040999746, 1.631615798668999862 ) ) ;
#32375 = CARTESIAN_POINT ( 'NONE',  ( -11.95950202284999975, -79.14141539787040358, 1.295167635372999948 ) ) ;
#32376 = CARTESIAN_POINT ( 'NONE',  ( 6.739285134038754066, -77.08750000000004832, -6.737116835514523672 ) ) ;
#32377 = CARTESIAN_POINT ( 'NONE',  ( -1.196500474958131388, -81.71480357325025068, 0.5696325066958111139 ) ) ;
#32378 = DIRECTION ( 'NONE',  ( 0.000000000000000000, 1.000000000000000000, 1.184237892934000027E-14 ) ) ;
#32379 = CARTESIAN_POINT ( 'NONE',  ( -3.562349398201000383, -1.892636553150000012, -0.5356682315460999932 ) ) ;
#32380 = CARTESIAN_POINT ( 'NONE',  ( 9.250000000000000000, -79.84999999999999432, 0.000000000000000000 ) ) ;
#32381 = CARTESIAN_POINT ( 'NONE',  ( 10.21381326473999884, -59.57129148919000272, 7.668949790015999746 ) ) ;
#32382 = CARTESIAN_POINT ( 'NONE',  ( -1.194090705999000024, -24.44031658902999737, -12.43436538489999954 ) ) ;
#32383 = CARTESIAN_POINT ( 'NONE',  ( 10.36873448126860886, -78.11209359995925183, -2.835127193485178054 ) ) ;
#32384 = CARTESIAN_POINT ( 'NONE',  ( 1.722652182756000183, -2.378241823149000123, 3.030129174318000107 ) ) ;
#32385 = CARTESIAN_POINT ( 'NONE',  ( 1.382886570148999850, -54.16901780135000166, -12.65982054472000051 ) ) ;
#32386 = DIRECTION ( 'NONE',  ( -1.000000000000000000, 0.000000000000000000, 0.000000000000000000 ) ) ;
#32387 = DIRECTION ( 'NONE',  ( 0.000000000000000000, 0.000000000000000000, -1.000000000000000000 ) ) ;
#32389 = CARTESIAN_POINT ( 'NONE',  ( 0.2372582530112999910, -78.71518221956600314, 1.497548220759000071 ) ) ;
#32388 = CARTESIAN_POINT ( 'NONE',  ( -0.3926218265389256890, -79.79583333333334849, 1.460959015002472050 ) ) ;
#32390 = CARTESIAN_POINT ( 'NONE',  ( 4.857361268487999872, -76.91360380131999364, -11.04062220482000001 ) ) ;
#32391 = EDGE_LOOP ( 'NONE', ( #29020, #9218, #12861, #2039 ) ) ;
#32392 = CARTESIAN_POINT ( 'NONE',  ( -2.936671086216000148, -86.24207450217399185, 2.063821221035999631 ) ) ;
#32393 = AXIS2_PLACEMENT_3D ( 'NONE', #43484, #56771, #16903 ) ;
#32394 = CARTESIAN_POINT ( 'NONE',  ( 3.309015450773000300, -81.12816687753750955, 10.91507257597000091 ) ) ;
#32395 = CARTESIAN_POINT ( 'NONE',  ( -7.958763980599000476, -17.52301961032999955, -9.723170659105999647 ) ) ;
#32396 = CARTESIAN_POINT ( 'NONE',  ( 0.7554284705563509839, -81.66666666666669983, -1.310679582531385945 ) ) ;
#32397 = CARTESIAN_POINT ( 'NONE',  ( -7.712695008784000272, -77.46634912723399680, -8.144473358846001432 ) ) ;
#32398 = CARTESIAN_POINT ( 'NONE',  ( 12.43652237957999951, -53.87935153028999480, -0.1283967009859000308 ) ) ;
#32399 = FACE_OUTER_BOUND ( 'NONE', #36588, .T. ) ;
#32400 = CARTESIAN_POINT ( 'NONE',  ( -3.500000000146000101, -0.7499999998540000101, 2.054632350152999929E-08 ) ) ;
#32401 = CARTESIAN_POINT ( 'NONE',  ( 7.909611445628718762, -79.80000000000001137, -8.777180137641350299 ) ) ;
#32402 = CARTESIAN_POINT ( 'NONE',  ( 1.930387568569762236, -77.00000000000001421, 9.098804631813305122 ) ) ;
#32403 = ORIENTED_EDGE ( 'NONE', *, *, #45098, .T. ) ;
#32404 = CONICAL_SURFACE ( 'NONE', #39954, 11.84999999993000053, 0.7853981633972997312 ) ;
#32405 = DIRECTION ( 'NONE',  ( 0.000000000000000000, 1.000000000000000000, 0.000000000000000000 ) ) ;
#32406 = CARTESIAN_POINT ( 'NONE',  ( 8.252635040182997983, -79.40151332859900890, -4.755435880420999517 ) ) ;
#32407 = CARTESIAN_POINT ( 'NONE',  ( -0.002438198160231863729, -75.82452515419292638, -11.78599345671029752 ) ) ;
#32408 = ORIENTED_EDGE ( 'NONE', *, *, #31836, .T. ) ;
#32409 = EDGE_CURVE ( 'NONE', #56909, #17250, #36313, .T. ) ;
#32410 = CARTESIAN_POINT ( 'NONE',  ( -12.83044039271999992, -55.49360374314999689, -2.062670899148999926 ) ) ;
#32411 = DIRECTION ( 'NONE',  ( 0.000000000000000000, 1.000000000000000000, 0.000000000000000000 ) ) ;
#32412 = ORIENTED_EDGE ( 'NONE', *, *, #39411, .F. ) ;
#32413 = CARTESIAN_POINT ( 'NONE',  ( 7.671012283914000029, -78.64789788104899060, 9.589126640163000204 ) ) ;
#32414 = CARTESIAN_POINT ( 'NONE',  ( 11.21715554180000041, -77.31778620838598215, 1.538714659179999833 ) ) ;
#32415 = CARTESIAN_POINT ( 'NONE',  ( 7.624341764943999955, -60.06485149430999826, -10.42531124854999902 ) ) ;
#32416 = EDGE_LOOP ( 'NONE', ( #25707, #43564, #57457, #1800 ) ) ;
#32417 = CARTESIAN_POINT ( 'NONE',  ( 12.50659871785095589, -24.97347219492458592, -0.3508073941908030347 ) ) ;
#32418 = CARTESIAN_POINT ( 'NONE',  ( -8.396223008680999911, -79.93312895501298954, -4.990405176070999538 ) ) ;
#32419 = EDGE_CURVE ( 'NONE', #48994, #42771, #48212, .T. ) ;
#32420 = AXIS2_PLACEMENT_3D ( 'NONE', #57141, #17270, #3697 ) ;
#32421 = ORIENTED_EDGE ( 'NONE', *, *, #40763, .T. ) ;
#32422 = CARTESIAN_POINT ( 'NONE',  ( -7.678655902623767737, -55.00623020231261506, 10.03844298032656823 ) ) ;
#32423 = DIRECTION ( 'NONE',  ( 0.000000000000000000, 1.000000000000000000, 0.000000000000000000 ) ) ;
#32424 = CARTESIAN_POINT ( 'NONE',  ( -12.54987272477000104, -25.05113590135999857, -0.1385846084899000075 ) ) ;
#32425 = CARTESIAN_POINT ( 'NONE',  ( 1.529609450199000076, -76.93207305011499386, 9.371081266747001592 ) ) ;
#32426 = CARTESIAN_POINT ( 'NONE',  ( -1.127633102446787161, -80.13579083371682543, -0.5390502240130501388 ) ) ;
#32427 = CARTESIAN_POINT ( 'NONE',  ( 1.980611416588510032, -18.47402268194409203, -12.74335092663070057 ) ) ;
#32428 = CARTESIAN_POINT ( 'NONE',  ( -3.914500761937000028, -78.48547955772869500, -9.512529912660000101E-10 ) ) ;
#32429 = B_SPLINE_CURVE_WITH_KNOTS ( 'NONE', 3,
 ( #15127, #56455, #28997, #55878, #28110, #11299 ),
 .UNSPECIFIED., .F., .F.,
 ( 4, 1, 1, 4 ),
 ( 0.000000000000000000, 0.3333333333333000081, 0.6666666666667000474, 1.000000000000000000 ),
 .UNSPECIFIED. ) ;
#32430 = VECTOR ( 'NONE', #41213, 1000.000000000000000 ) ;
#32431 = CARTESIAN_POINT ( 'NONE',  ( 0.5497657648701759214, -78.19577990788877742, 1.434553788796227858 ) ) ;
#32432 = CARTESIAN_POINT ( 'NONE',  ( -2.759188190257293449, -80.39583333119153963, -2.967398781983584310 ) ) ;
#32433 = ORIENTED_EDGE ( 'NONE', *, *, #51653, .T. ) ;
#32434 = CARTESIAN_POINT ( 'NONE',  ( -9.500000000000007105, -77.78958333333335418, 1.243547092045919733 ) ) ;
#32435 = CARTESIAN_POINT ( 'NONE',  ( 3.007117222848000093, -75.83802852838000774, 11.93703523519999976 ) ) ;
#32436 = CARTESIAN_POINT ( 'NONE',  ( -2.813789756862251856, -77.60416666666665719, -10.47020627418439709 ) ) ;
#32437 = ADVANCED_FACE ( 'NONE', ( #21127 ), #6474, .F. ) ;
#32438 = CARTESIAN_POINT ( 'NONE',  ( -3.004631399418401294, -2.305633654303593350, 1.836342379236549860 ) ) ;
#32439 = DIRECTION ( 'NONE',  ( 0.000000000000000000, 1.000000000000000000, 0.000000000000000000 ) ) ;
#32440 = CARTESIAN_POINT ( 'NONE',  ( -12.10179013622999911, -78.49561315626999658, -1.986401539992999954 ) ) ;
#32441 = CARTESIAN_POINT ( 'NONE',  ( 9.406806676749999596, -76.89611744936398452, -7.895227358184000899 ) ) ;
#32442 = CARTESIAN_POINT ( 'NONE',  ( -3.654181822837000215, -86.09999999943198645, 1.626946589673999854 ) ) ;
#32443 = CARTESIAN_POINT ( 'NONE',  ( 10.55330385607999943, -78.39927573546698625, 3.944190366796999303 ) ) ;
#32444 = CARTESIAN_POINT ( 'NONE',  ( 11.00000000000000000, -23.75000000000000000, -1.203259120426999909E-14 ) ) ;
#32445 = CARTESIAN_POINT ( 'NONE',  ( -4.227663776733128209, -76.95352454581043844, 11.31097848705637965 ) ) ;
#32446 = CARTESIAN_POINT ( 'NONE',  ( 3.371435477143000181, -79.39929447278066732, -10.69820234502000034 ) ) ;
#32447 = VERTEX_POINT ( 'NONE', #8417 ) ;
#32448 = CARTESIAN_POINT ( 'NONE',  ( -1.183213148269000259, -81.97986186469999836, 0.6526699808710000328 ) ) ;
#32449 = CARTESIAN_POINT ( 'NONE',  ( -9.502046381818999521, -77.31279324197298308, 1.985581014958000212 ) ) ;
#32450 = CARTESIAN_POINT ( 'NONE',  ( -9.497876546326999403, -77.25168256874098915, -0.2008509664869000122 ) ) ;
#32451 = CARTESIAN_POINT ( 'NONE',  ( -1.500000000000000000, -80.00000000000000000, 0.000000000000000000 ) ) ;
#32452 = CARTESIAN_POINT ( 'NONE',  ( 8.689834030816680155, -76.99999999999998579, 3.513648003987066115 ) ) ;
#32453 = CARTESIAN_POINT ( 'NONE',  ( 10.42985624311000059, -77.36698389494598871, 5.801172517007000096 ) ) ;
#32454 = CARTESIAN_POINT ( 'NONE',  ( -2.166619587182999851, -77.59999470175499425, 9.383974079751000730 ) ) ;
#32455 = CARTESIAN_POINT ( 'NONE',  ( 8.318892879164591747, -76.01180963423074388, 8.297585421471344702 ) ) ;
#32456 = CARTESIAN_POINT ( 'NONE',  ( 3.535142739574999915, -80.37495082227849252, 10.17871189313000002 ) ) ;
#32457 = CARTESIAN_POINT ( 'NONE',  ( -0.4871519710310731610, -86.10000000000017906, 3.917790784212267674 ) ) ;
#32458 = ORIENTED_EDGE ( 'NONE', *, *, #34985, .T. ) ;
#32459 = CARTESIAN_POINT ( 'NONE',  ( 0.000000000000000000, -76.75499999999999545, 0.000000000000000000 ) ) ;
#32460 = VECTOR ( 'NONE', #9838, 1000.000000000000114 ) ;
#32461 = CARTESIAN_POINT ( 'NONE',  ( 10.42531124905999995, -23.26485148473999942, 7.624341765453999997 ) ) ;
#32462 = CARTESIAN_POINT ( 'NONE',  ( 12.00000000000000000, -78.64999999999999147, 0.000000000000000000 ) ) ;
#32463 = CARTESIAN_POINT ( 'NONE',  ( 9.694840914897000062, -79.70162658376399634, -5.145296513660000848 ) ) ;
#32464 = FACE_OUTER_BOUND ( 'NONE', #6667, .T. ) ;
#32465 = CARTESIAN_POINT ( 'NONE',  ( 8.400975614893999577, -76.18978390147600521, 9.261618890420999506 ) ) ;
#32466 = CARTESIAN_POINT ( 'NONE',  ( 0.6799804141806697899, -79.27066170111446297, -1.062685189815249620 ) ) ;
#32467 = CARTESIAN_POINT ( 'NONE',  ( 7.622784390062999904, -18.21288991773999655, -10.47836615826999918 ) ) ;
#32468 = CARTESIAN_POINT ( 'NONE',  ( 13.63885489310999510, -56.01421830980998351, -7.254376133916000668 ) ) ;
#32469 = ORIENTED_EDGE ( 'NONE', *, *, #10165, .F. ) ;
#32470 = CARTESIAN_POINT ( 'NONE',  ( 2.165712778014000417, -78.56830367376599611, 10.93454565734000106 ) ) ;
#32471 = CARTESIAN_POINT ( 'NONE',  ( 12.70255494770093918, -54.05391159002875412, 1.306413223725076067 ) ) ;
#32472 = CARTESIAN_POINT ( 'NONE',  ( -10.75000000000000355, -79.98958333333332860, 1.407171709420384609 ) ) ;
#32473 = CARTESIAN_POINT ( 'NONE',  ( 2.236739823803636451, -78.43735716284257364, 3.872902599707189530 ) ) ;
#32474 = CARTESIAN_POINT ( 'NONE',  ( -8.425436799864590043, -77.01663941737371033, -8.658731487823875028 ) ) ;
#32475 = B_SPLINE_CURVE_WITH_KNOTS ( 'NONE', 3,
 ( #432, #17015, #12012, #40546, #57454, #30577, #3438, #16730, #27241, #4828 ),
 .UNSPECIFIED., .F., .F.,
 ( 4, 2, 2, 2, 4 ),
 ( 0.000000000000000000, 0.2500000000000000000, 0.5000000000000000000, 0.7500000000000000000, 1.000000000000000000 ),
 .UNSPECIFIED. ) ;
#32476 = ADVANCED_FACE ( 'NONE', ( #26705 ), #47532, .F. ) ;
#32478 = CARTESIAN_POINT ( 'NONE',  ( -1.159531907918516458, -81.56974165474723293, 0.4665971513285117056 ) ) ;
#32477 = CIRCLE ( 'NONE', #18383, 1.000000000000000000 ) ;
#32479 = EDGE_CURVE ( 'NONE', #12183, #26753, #41043, .T. ) ;
#32480 = CARTESIAN_POINT ( 'NONE',  ( -3.300471783580745999, -77.00000000000002842, -8.910846386529984287 ) ) ;
#32481 = CARTESIAN_POINT ( 'NONE',  ( 10.42531125074000009, -18.73514854687000053, 7.624341767140999870 ) ) ;
#32482 = CARTESIAN_POINT ( 'NONE',  ( 2.813789756862229652, -79.35416666666667140, 10.47020627418440064 ) ) ;
#32483 = CARTESIAN_POINT ( 'NONE',  ( 10.55673762599399090, -78.67804158551905402, -3.003849123923255426 ) ) ;
#32484 = CARTESIAN_POINT ( 'NONE',  ( -7.374560639699022424, -77.22708333333333997, 9.596002108778135309 ) ) ;
#32485 = ORIENTED_EDGE ( 'NONE', *, *, #27096, .T. ) ;
#32486 = ADVANCED_FACE ( 'NONE', ( #34334 ), #52368, .F. ) ;
#32487 = ORIENTED_EDGE ( 'NONE', *, *, #9512, .T. ) ;
#32488 = CARTESIAN_POINT ( 'NONE',  ( -3.234762833941022819, -77.80249999999999488, 8.977080150340215781 ) ) ;
#32489 = CARTESIAN_POINT ( 'NONE',  ( 8.939664771278220456, -78.80329824956528739, -5.970164743213411285 ) ) ;
#32490 = VERTEX_POINT ( 'NONE', #30486 ) ;
#32491 = CARTESIAN_POINT ( 'NONE',  ( 0.000000000000000000, 4.040000000000000036, 0.000000000000000000 ) ) ;
#32492 = CARTESIAN_POINT ( 'NONE',  ( -1.073871440473841865, -82.90104168234370263, 3.271588444796262873 ) ) ;
#32493 = CARTESIAN_POINT ( 'NONE',  ( 8.643979526188999785, -62.05953772878000052, 9.422807787405000468 ) ) ;
#32494 = CARTESIAN_POINT ( 'NONE',  ( 1.093346996216985056, -82.39232783775085522, 0.6296573929790432178 ) ) ;
#32495 = CARTESIAN_POINT ( 'NONE',  ( 7.919950863376441497, -77.36742616270637996, 8.988568817287896806 ) ) ;
#32496 = CARTESIAN_POINT ( 'NONE',  ( -8.382198119002001846, -79.89173351027790204, -7.453647783897999979 ) ) ;
#32497 = CARTESIAN_POINT ( 'NONE',  ( 4.889518234483114512, -81.00000000000000000, 9.699724439954369615 ) ) ;
#32498 = VECTOR ( 'NONE', #2668, 1000.000000000000000 ) ;
#32499 = EDGE_LOOP ( 'NONE', ( #19665, #32996, #53567, #1325 ) ) ;
#32500 = FACE_OUTER_BOUND ( 'NONE', #33403, .T. ) ;
#32501 = EDGE_LOOP ( 'NONE', ( #45305, #54647, #20310, #12044 ) ) ;
#32502 = CARTESIAN_POINT ( 'NONE',  ( 7.455184149750110123, -77.40051399983991587, 5.475553992661359004 ) ) ;
#32503 = CARTESIAN_POINT ( 'NONE',  ( 10.65102452230999930, -77.64103837914298367, 2.905137941168000282 ) ) ;
#32504 = VECTOR ( 'NONE', #6333, 1000.000000000000000 ) ;
#32505 = CARTESIAN_POINT ( 'NONE',  ( 8.485281374238999419, -23.25000000000000000, -8.485281374238999419 ) ) ;
#32506 = CARTESIAN_POINT ( 'NONE',  ( -0.1356420093736999954, -77.61024949339380896, -1.608970710047999964 ) ) ;
#32507 = CARTESIAN_POINT ( 'NONE',  ( -9.102137320389529052, -17.02814024879980792, 8.583672455348743568 ) ) ;
#32508 = CARTESIAN_POINT ( 'NONE',  ( -3.206516299415000049, -2.013032031398999777, -0.5298615117031000299 ) ) ;
#32509 = CARTESIAN_POINT ( 'NONE',  ( -0.1732310466989999687, -77.65468677991998447, 1.530487294790999986 ) ) ;
#32510 = CARTESIAN_POINT ( 'NONE',  ( 2.570908280542000046, -82.25232046129099217, -3.285908224385000409 ) ) ;
#32511 = CARTESIAN_POINT ( 'NONE',  ( 9.663556473158999793, -79.64035858408298907, -5.128693071642000056 ) ) ;
#32512 = AXIS2_PLACEMENT_3D ( 'NONE', #6492, #41634, #2086 ) ;
#32513 = CARTESIAN_POINT ( 'NONE',  ( -7.969039355681999837, -24.62377467844000023, -9.934746417635000881 ) ) ;
#32514 = CARTESIAN_POINT ( 'NONE',  ( 12.80896991328000034, -57.04546192861999998, -1.930989179114000143 ) ) ;
#32515 = CARTESIAN_POINT ( 'NONE',  ( 2.986993022240000073, -82.13767524227699823, -1.707903102581999955 ) ) ;
#32516 = EDGE_LOOP ( 'NONE', ( #47507, #49630 ) ) ;
#32517 = CARTESIAN_POINT ( 'NONE',  ( -10.89546045048518508, -77.19999999999998863, 1.402775879548545213 ) ) ;
#32518 = CARTESIAN_POINT ( 'NONE',  ( 1.533663219811999934, -76.20928543398198940, -11.15151220388999853 ) ) ;
#32519 = CARTESIAN_POINT ( 'NONE',  ( 10.28683214875539953, -77.87376456324562923, 3.156758843427483363 ) ) ;
#32520 = CARTESIAN_POINT ( 'NONE',  ( -8.557169117579000783, -77.69558072920298741, -8.383968101560000719 ) ) ;
#32521 = CARTESIAN_POINT ( 'NONE',  ( 7.000000000000000000, -80.99999999999998579, -1.199999999999970424 ) ) ;
#32522 = ADVANCED_FACE ( 'NONE', ( #30765 ), #44660, .F. ) ;
#32524 = DIRECTION ( 'NONE',  ( 4.762546956201999894E-11, -1.000000000000000000, 4.762495317921000031E-11 ) ) ;
#32523 = DIRECTION ( 'NONE',  ( 0.000000000000000000, 1.000000000000000000, 0.000000000000000000 ) ) ;
#32525 = CARTESIAN_POINT ( 'NONE',  ( 3.534803853715930089, -2.486768684982593847, -0.6079085174694663918 ) ) ;
#32526 = CARTESIAN_POINT ( 'NONE',  ( 1.672085670906209298, -80.96293633418511604, 10.61893514166530927 ) ) ;
#32527 = DIRECTION ( 'NONE',  ( 0.9999813732757145690, 0.000000000000000000, -0.006103531896856088240 ) ) ;
#32528 = CARTESIAN_POINT ( 'NONE',  ( 0.3409554497599163736, -86.02148120184399716, -7.610863924474937647 ) ) ;
#32529 = CARTESIAN_POINT ( 'NONE',  ( 9.087383623426001478, -77.59198448012199378, -6.455544860934000262 ) ) ;
#32530 = CARTESIAN_POINT ( 'NONE',  ( 11.61133755414000035, -76.92639651314304672, 3.999933378912999604 ) ) ;
#32531 = CARTESIAN_POINT ( 'NONE',  ( 10.99151865632000025, -80.62809514466069061, -1.817614465157000092 ) ) ;
#32532 = ORIENTED_EDGE ( 'NONE', *, *, #47427, .F. ) ;
#32533 = CARTESIAN_POINT ( 'NONE',  ( 1.009320482739999969, -77.51652403538301428, 9.441330439200999791 ) ) ;
#32534 = CARTESIAN_POINT ( 'NONE',  ( -3.607726709122000219, -2.271525618455999762, 1.647853588899000021 ) ) ;
#32535 = CARTESIAN_POINT ( 'NONE',  ( 8.196653188619999142, -77.50811055442200370, 7.657217973713000170 ) ) ;
#32536 = CARTESIAN_POINT ( 'NONE',  ( -10.57157196544999955, -79.79227723196800071, 2.324769239444999691 ) ) ;
#32537 = CARTESIAN_POINT ( 'NONE',  ( 0.000000000000000000, -74.64999999999999147, 0.000000000000000000 ) ) ;
#32538 = CARTESIAN_POINT ( 'NONE',  ( -10.31401527466070256, -76.78841872786956912, 3.823154250450220282 ) ) ;
#32539 = CARTESIAN_POINT ( 'NONE',  ( -1.532229594837823505, -24.12298963131021168, -12.51228690880890682 ) ) ;
#32540 = CARTESIAN_POINT ( 'NONE',  ( -8.894932048704164984, -53.57190732453712201, -9.073469156659786705 ) ) ;
#32541 = B_SPLINE_SURFACE_WITH_KNOTS ( 'NONE', 3, 3, ( 
 ( #16921, #16631, #33754, #34617 ),
 ( #29893, #57358, #47665, #43796 ),
 ( #38192, #47083, #52644, #29323 ),
 ( #51793, #11346, #43498, #6612 ),
 ( #24910, #42927, #57071, #56211 ),
 ( #3059, #47950, #48233, #7769 ),
 ( #21055, #47371, #34900, #52930 ),
 ( #39056, #29042, #2482, #12199 ),
 ( #30184, #25772, #3343, #20486 ),
 ( #21339, #15759, #39351, #24623 ),
 ( #7191, #2201, #34038, #6901 ) ),
 .UNSPECIFIED., .F., .F., .F.,
 ( 4, 1, 1, 1, 1, 1, 1, 1, 4 ),
 ( 4, 4 ),
 ( -0.01994534136800000038, 0.000000000000000000, 0.1666666666667000196, 0.3333333333333000081, 0.5000000000000000000, 0.6666666666667000474, 0.8333333333333000637, 1.000000000000000000, 1.020519780480000138 ),
 ( -0.3582002740342999925, 1.358566136078000142 ),
 .UNSPECIFIED. ) ;
#32542 = CARTESIAN_POINT ( 'NONE',  ( -0.8075106742674000859, -83.50967953870899407, -4.093222644815999622 ) ) ;
#32543 = CARTESIAN_POINT ( 'NONE',  ( -7.686941364964000378, -58.55472017773000459, 10.48774103561000182 ) ) ;
#32544 = CARTESIAN_POINT ( 'NONE',  ( 12.90058126069000011, -78.75123239577999357, 1.113827872717999989 ) ) ;
#32545 = VECTOR ( 'NONE', #19926, 1000.000000000000000 ) ;
#32546 = CARTESIAN_POINT ( 'NONE',  ( 11.23392183412000023, -78.43521853677198408, 0.8531908288953000685 ) ) ;
#32547 = EDGE_CURVE ( 'NONE', #14715, #19368, #54240, .T. ) ;
#32548 = CARTESIAN_POINT ( 'NONE',  ( 1.417725061834000044, -79.91717952614000353, -0.8748226493128999914 ) ) ;
#32549 = CARTESIAN_POINT ( 'NONE',  ( -0.8071124281214000495, -78.37920846078000636, 1.186022485533999804 ) ) ;
#32550 = VECTOR ( 'NONE', #9368, 1000.000000000000000 ) ;
#32551 = CARTESIAN_POINT ( 'NONE',  ( -1.811016405462463119, -60.86173555340016605, 12.71771640067393605 ) ) ;
#32552 = CARTESIAN_POINT ( 'NONE',  ( 1.394813767835870522, -81.46858624048219610, -0.5832741237438665571 ) ) ;
#32553 = CARTESIAN_POINT ( 'NONE',  ( 0.000000000000000000, -81.19999999999998863, 7.000000000000000000 ) ) ;
#32554 = DIRECTION ( 'NONE',  ( 0.000000000000000000, -1.000000000000000000, 0.000000000000000000 ) ) ;
#32555 = CARTESIAN_POINT ( 'NONE',  ( 1.159203040753797431, -79.81982044965684508, -0.4672302196274162878 ) ) ;
#32556 = ORIENTED_EDGE ( 'NONE', *, *, #28146, .F. ) ;
#32557 = CARTESIAN_POINT ( 'NONE',  ( -1.134601249923181232, -81.63469519395181351, -0.5245280893132442390 ) ) ;
#32558 = CARTESIAN_POINT ( 'NONE',  ( -11.02198032011999906, -79.96223007984259823, -0.4665663988222000236 ) ) ;
#32559 = DIRECTION ( 'NONE',  ( 4.762557283857999921E-11, 1.000000000000000000, -4.762495317921000031E-11 ) ) ;
#32560 = ORIENTED_EDGE ( 'NONE', *, *, #28194, .T. ) ;
#32561 = ADVANCED_FACE ( 'NONE', ( #48798 ), #38541, .F. ) ;
#32562 = ORIENTED_EDGE ( 'NONE', *, *, #29375, .T. ) ;
#32563 = CARTESIAN_POINT ( 'NONE',  ( -1.403112730325000168, -81.01638143716699858, 0.5746449548680000463 ) ) ;
#32564 = EDGE_CURVE ( 'NONE', #53569, #51194, #8638, .T. ) ;
#32565 = ORIENTED_EDGE ( 'NONE', *, *, #656, .T. ) ;
#32566 = VERTEX_POINT ( 'NONE', #31052 ) ;
#32567 = CARTESIAN_POINT ( 'NONE',  ( 2.019183793707000074, -18.21279722757000030, 12.79944116704999857 ) ) ;
#32568 = CARTESIAN_POINT ( 'NONE',  ( -10.09635500651677553, -55.27627834093888026, -7.644087038098057896 ) ) ;
#32569 = CARTESIAN_POINT ( 'NONE',  ( 0.000000000000000000, 0.000000000000000000, 0.000000000000000000 ) ) ;
#32570 = CARTESIAN_POINT ( 'NONE',  ( 3.437653462762137568, -80.93541665514577232, -0.2151425978537864214 ) ) ;
#32571 = CARTESIAN_POINT ( 'NONE',  ( 9.665471083832999355, -78.54936001420199432, -2.650702293911000318 ) ) ;
#32572 = CARTESIAN_POINT ( 'NONE',  ( 5.263805209930564111, -78.27334790553378241, -7.606318086626214559 ) ) ;
#32573 = B_SPLINE_CURVE_WITH_KNOTS ( 'NONE', 3,
 ( #1330, #50917, #28156, #45620, #55331, #46207, #1047, #23161, #14876, #10466 ),
 .UNSPECIFIED., .F., .F.,
 ( 4, 2, 2, 2, 4 ),
 ( 0.000000000000000000, 0.2500000000000000000, 0.5000000000000000000, 0.7500000000000000000, 1.000000000000000000 ),
 .UNSPECIFIED. ) ;
#32574 = DIRECTION ( 'NONE',  ( 0.000000000000000000, 0.000000000000000000, -1.000000000000000000 ) ) ;
#32575 = EDGE_LOOP ( 'NONE', ( #12773, #35678, #15384, #22996 ) ) ;
#32576 = EDGE_LOOP ( 'NONE', ( #28139, #5668, #2712, #6887 ) ) ;
#32577 = CARTESIAN_POINT ( 'NONE',  ( -8.801507186371804181, -77.57514545457918587, 2.845283712962050071 ) ) ;
#32578 = CARTESIAN_POINT ( 'NONE',  ( 3.370554742410903248, -77.04759005475500544, -11.56126178251549241 ) ) ;
#32579 = CARTESIAN_POINT ( 'NONE',  ( -1.500000000000000000, -79.50000000000000000, 0.000000000000000000 ) ) ;
#32580 = CARTESIAN_POINT ( 'NONE',  ( 7.256139241522999939, -77.57763388114098291, 6.443535727668999513 ) ) ;
#32581 = EDGE_CURVE ( 'NONE', #44860, #35917, #56136, .T. ) ;
#32582 = CARTESIAN_POINT ( 'NONE',  ( 8.130811096541000538, -24.68523690389000080, 9.546858433121998999 ) ) ;
#32583 = CARTESIAN_POINT ( 'NONE',  ( -10.35747145892000098, -23.31584731985000047, 7.626500777234999973 ) ) ;
#32584 = CARTESIAN_POINT ( 'NONE',  ( 5.622921568558999716, -77.75781628945000534, 11.67242091225999978 ) ) ;
#32585 = B_SPLINE_SURFACE_WITH_KNOTS ( 'NONE', 3, 3, ( 
 ( #18980, #50570, #31948, #36972, #28396, #54985, #37261, #45564, #14821, #1859, #14241, #1562, #10125, #49993, #32819, #50865, #46741, #37552, #55569, #28103, #46153, #6261, #24276, #5677, #19854, #1277, #41116, #23688, #710, #33116, #9539, #41701, #37849, #51157, #13952, #10411, #9831, #36681, #23401, #27522, #19270, #10712, #46443, #54697, #28690, #5971, #5109, #23976, #32237, #50280, #27812, #45859, #5392, #2147, #42873, #3007, #7716, #25717, #52596, #28987, #38428, #20148, #21288, #38135, #33702, #33412, #30134 ),
 ( #16001, #48183, #43743, #52027, #3296, #43165, #6558, #2430, #24566, #25431, #51450, #56446, #55869, #16579, #15419, #34276, #51741, #42583, #6847, #11002, #33988, #11290, #56158, #43446, #11580, #29270, #47028, #47896, #34564, #20433, #15707, #21003, #39009, #24857, #47318, #29559, #47614, #57017, #7138, #12147, #25139, #2722, #20718, #52311, #56739, #7428, #11867, #29844, #26292, #35423, #39295, #58174, #22153, #49329, #53755, #49033, #13292, #16870, #30995, #39868, #4449, #36024, #26869, #22450, #9174, #27157, #44305 ),
 ( #45197, #3861, #34849, #52881, #44023, #3575, #39584, #57588, #21859, #17149, #57881, #53453, #26568, #4154, #44600, #36611, #23904, #19199, #37477, #18328, #18620, #36898, #33040, #45490, #15048, #1207, #10053, #46079, #638, #45788, #28318, #19484, #37190, #55204, #55498, #14747, #54634, #32746, #49922, #925, #10636, #23614, #51086, #28035, #32167, #14170, #13884, #41627, #9467, #41051, #32454, #54911, #40755, #18905, #5324, #50206, #14463, #50794, #31878, #9756, #27741, #50499, #27452, #28618, #5603, #10340, #23331 ),
 ( #46663, #22745, #46371, #5895, #5033, #23035, #41922, #41339, #1494, #349, #36321, #54344, #20642, #51672, #29483, #37776, #7066, #34486, #6482, #52232, #29199, #42220, #25067, #43091, #38927, #34195, #11789, #11219, #24784, #56944, #16503, #2360, #52516, #51952, #15347, #47244, #33341, #29764, #1785, #6775, #12072, #25350, #6190, #2649, #2078, #51374, #15634, #30053, #42799, #42507, #10931, #47820, #20358, #20076, #24203, #56662, #43367, #38353, #24494, #7351, #2925, #33630, #46956, #19781, #56375, #20926, #15925 ) ),
 .UNSPECIFIED., .F., .F., .F.,
 ( 4, 4 ),
 ( 4, 1, 1, 1, 1, 1, 1, 1, 1, 1, 1, 1, 1, 1, 1, 1, 1, 1, 1, 1, 1, 1, 1, 1, 1, 1, 1, 1, 1, 1, 1, 1, 1, 1, 1, 1, 1, 1, 1, 1, 1, 1, 1, 1, 1, 1, 1, 1, 1, 1, 1, 1, 1, 1, 1, 1, 1, 1, 1, 1, 1, 1, 1, 1, 4 ),
 ( -0.1387574078320999993, 1.138757407831999968 ),
 ( -0.02000000000000000042, -0.003749999999999999861, 0.01250000000000000069, 0.02875000000000000125, 0.04499999999999999833, 0.06124999999999999889, 0.07749999999999999944, 0.09375000000000000000, 0.1100000000000000006, 0.1262500000000000011, 0.1424999999999999878, 0.1587500000000000022, 0.1749999999999999889, 0.1912500000000000033, 0.2074999999999999900, 0.2237500000000000044, 0.2399999999999999911, 0.2562499999999999778, 0.2725000000000000200, 0.2887500000000000067, 0.3049999999999999933, 0.3212499999999999800, 0.3375000000000000222, 0.3537500000000000089, 0.3699999999999999956, 0.3862499999999999822, 0.4025000000000000244, 0.4187500000000000111, 0.4349999999999999978, 0.4512499999999999845, 0.4675000000000000266, 0.4837500000000000133, 0.5000000000000000000, 0.5162499999999999867, 0.5324999999999999734, 0.5487499999999999600, 0.5649999999999999467, 0.5812500000000000444, 0.5975000000000000311, 0.6137500000000000178, 0.6300000000000000044, 0.6462499999999999911, 0.6624999999999999778, 0.6787499999999999645, 0.6949999999999999512, 0.7112500000000000488, 0.7275000000000000355, 0.7437500000000000222, 0.7600000000000000089, 0.7762499999999999956, 0.7924999999999999822, 0.8087499999999999689, 0.8249999999999999556, 0.8412500000000000533, 0.8575000000000000400, 0.8737500000000000266, 0.8900000000000000133, 0.9062500000000000000, 0.9224999999999999867, 0.9387499999999999734, 0.9549999999999999600, 0.9712499999999999467, 0.9875000000000000444, 1.003749999999999920, 1.020000000000000018 ),
 .UNSPECIFIED. ) ;
#32586 = CARTESIAN_POINT ( 'NONE',  ( -1.494795747725999879, -80.73373215275999826, -0.5291335979940999801 ) ) ;
#32587 = VECTOR ( 'NONE', #32599, 1000.000000000000000 ) ;
#32588 = CARTESIAN_POINT ( 'NONE',  ( 5.216320339343518242, -77.37829693750339288, 7.876220663163953972 ) ) ;
#32589 = CARTESIAN_POINT ( 'NONE',  ( -9.022574137301845099, -76.64453523234787724, 7.529641841958728321 ) ) ;
#32590 = CARTESIAN_POINT ( 'NONE',  ( -3.743424489665999833, -80.36598997120898957, -1.848346091329999830 ) ) ;
#32591 = CARTESIAN_POINT ( 'NONE',  ( -10.58783149161999937, -80.79384588825814717, -3.847989116766000084 ) ) ;
#32592 = CARTESIAN_POINT ( 'NONE',  ( -11.68767212001979594, -76.77916666666666856, 3.140974612311315806 ) ) ;
#32593 = CARTESIAN_POINT ( 'NONE',  ( 10.75000000000000000, -76.85000000000000853, 0.000000000000000000 ) ) ;
#32594 = CARTESIAN_POINT ( 'NONE',  ( -3.180808344062000081, -80.32832046129098558, -1.570672117285999869 ) ) ;
#32595 = AXIS2_PLACEMENT_3D ( 'NONE', #15265, #32665, #50132 ) ;
#32596 = ADVANCED_FACE ( 'NONE', ( #41978 ), #28610, .F. ) ;
#32597 = CARTESIAN_POINT ( 'NONE',  ( -1.210921577777000158, -78.18748239744249418, 0.5587889421650999999 ) ) ;
#32598 = CARTESIAN_POINT ( 'NONE',  ( 0.000000000000000000, -32.88214388149999934, 0.000000000000000000 ) ) ;
#32599 = DIRECTION ( 'NONE',  ( 0.000000000000000000, 1.000000000000000000, 0.000000000000000000 ) ) ;
#32600 = CARTESIAN_POINT ( 'NONE',  ( -2.809159726167000048, -3.410933523454000138, -2.568020482856000264 ) ) ;
#32601 = CARTESIAN_POINT ( 'NONE',  ( 7.658490574713046506, -77.20000000000000284, -7.714358540288501764 ) ) ;
#32602 = EDGE_CURVE ( 'NONE', #39052, #43853, #35236, .T. ) ;
#32603 = EDGE_LOOP ( 'NONE', ( #57838, #55541, #186, #55874 ) ) ;
#32604 = CARTESIAN_POINT ( 'NONE',  ( -8.782705133629537642, -78.85833333333333428, -7.901937437515731411 ) ) ;
#32605 = CARTESIAN_POINT ( 'NONE',  ( 0.5847500590554981503, -18.69344856180424941, -10.98448857562232028 ) ) ;
#32606 = CARTESIAN_POINT ( 'NONE',  ( -1.439896632895333317, -79.08541666666666003, 10.99999999999999822 ) ) ;
#32607 = CARTESIAN_POINT ( 'NONE',  ( -0.4864526504254000350, -79.20815779017299008, 9.739263145490999918 ) ) ;
#32608 = DIRECTION ( 'NONE',  ( 1.000000000000000000, 0.000000000000000000, 0.000000000000000000 ) ) ;
#32609 = CARTESIAN_POINT ( 'NONE',  ( 7.575877328000173883, -79.41276128209595697, 7.626825700000964048 ) ) ;
#32610 = DIRECTION ( 'NONE',  ( 0.000000000000000000, 1.000000000000000000, 0.000000000000000000 ) ) ;
#32611 = LINE ( 'NONE', #36763, #13677 ) ;
#32612 = CARTESIAN_POINT ( 'NONE',  ( 4.447146149678999905, -77.08500682716429253, 10.06768414028999992 ) ) ;
#32613 = CARTESIAN_POINT ( 'NONE',  ( -1.467516833711000057, -82.33459940031100643, 0.3393247902666000071 ) ) ;
#32614 = CARTESIAN_POINT ( 'NONE',  ( 0.000000000000000000, -76.19999999999998863, -10.50000000000000000 ) ) ;
#32615 = CARTESIAN_POINT ( 'NONE',  ( -8.508571376020000798, -78.05598958818299593, -4.026835934908000070 ) ) ;
#32617 = CARTESIAN_POINT ( 'NONE',  ( -2.302038976840258933, -80.20520833350919077, -10.81263029561343103 ) ) ;
#32616 = CARTESIAN_POINT ( 'NONE',  ( 0.2779842904343000076, -84.78704385015599598, -3.953316927815999637 ) ) ;
#32618 = CARTESIAN_POINT ( 'NONE',  ( 4.067416459488999436, -79.35105584965398862, -8.418325902196000854 ) ) ;
#32619 = DIRECTION ( 'NONE',  ( 0.000000000000000000, 1.000000000000000000, 0.000000000000000000 ) ) ;
#32620 = CARTESIAN_POINT ( 'NONE',  ( 0.9683804214594998738, -79.84864567164899540, -0.8959938446301999315 ) ) ;
#32621 = CARTESIAN_POINT ( 'NONE',  ( -7.589549450764452310, -77.16263193562646450, -7.613205801859955990 ) ) ;
#32622 = CARTESIAN_POINT ( 'NONE',  ( -0.5999999999999999778, -5.200000000000000178, -0.5999999999999999778 ) ) ;
#32623 = CARTESIAN_POINT ( 'NONE',  ( -3.851650068366999857, -78.96264283715740362, -1.616138016926814209E-14 ) ) ;
#32624 = ORIENTED_EDGE ( 'NONE', *, *, #1131, .T. ) ;
#32625 = CARTESIAN_POINT ( 'NONE',  ( 11.77452260639999970, -79.82453443975478535, 1.259536412044000020 ) ) ;
#32626 = DIRECTION ( 'NONE',  ( 0.000000000000000000, -1.000000000000000000, 0.000000000000000000 ) ) ;
#32627 = DIRECTION ( 'NONE',  ( 1.000000000000000000, 0.000000000000000000, 0.000000000000000000 ) ) ;
#32628 = ORIENTED_EDGE ( 'NONE', *, *, #47114, .F. ) ;
#32629 = CARTESIAN_POINT ( 'NONE',  ( 6.013200962235000446, -77.95638901018298839, 10.30906962990999887 ) ) ;
#32630 = ADVANCED_FACE ( 'NONE', ( #9442 ), #22723, .F. ) ;
#32631 = VERTEX_POINT ( 'NONE', #18009 ) ;
#32632 = TOROIDAL_SURFACE ( 'NONE', #8127, 17.50000000000000000, 5.000000000000000000 ) ;
#32633 = ORIENTED_EDGE ( 'NONE', *, *, #7027, .F. ) ;
#32634 = CARTESIAN_POINT ( 'NONE',  ( -10.47020627418440242, -78.97916666666667140, 2.813789756862221214 ) ) ;
#32635 = ORIENTED_EDGE ( 'NONE', *, *, #26596, .T. ) ;
#32636 = AXIS2_PLACEMENT_3D ( 'NONE', #11565, #48167, #25125 ) ;
#32637 = CARTESIAN_POINT ( 'NONE',  ( -1.194690127457000095, -81.97417810200299471, -3.340252635762999578 ) ) ;
#32638 = CARTESIAN_POINT ( 'NONE',  ( 11.79999999999999893, -18.84999999999000053, -0.5999999999999999778 ) ) ;
#32639 = EDGE_LOOP ( 'NONE', ( #29305, #11056, #18283, #12886 ) ) ;
#32640 = CARTESIAN_POINT ( 'NONE',  ( 1.249294810647472387, -82.84741769837783920, -0.04986753284709229822 ) ) ;
#32641 = AXIS2_PLACEMENT_3D ( 'NONE', #13360, #36387, #48812 ) ;
#32642 = ORIENTED_EDGE ( 'NONE', *, *, #45453, .T. ) ;
#32643 = CARTESIAN_POINT ( 'NONE',  ( -2.813789756862251856, -80.60416666666665719, -10.47020627418439709 ) ) ;
#32644 = CARTESIAN_POINT ( 'NONE',  ( -2.572168127912981106, -78.45355818381494828, -9.357231370006124038 ) ) ;
#32645 = LINE ( 'NONE', #55694, #13302 ) ;
#32646 = LINE ( 'NONE', #32360, #2911 ) ;
#32647 = EDGE_CURVE ( 'NONE', #54228, #34245, #21418, .T. ) ;
#32648 = CARTESIAN_POINT ( 'NONE',  ( 11.01994305158000031, -76.43468485262199863, -1.906499110313000234 ) ) ;
#32649 = CARTESIAN_POINT ( 'NONE',  ( -9.546819346421999697, -24.68527546640000025, 8.130850183241999929 ) ) ;
#32650 = B_SPLINE_CURVE_WITH_KNOTS ( 'NONE', 3,
 ( #42308, #47044, #24585, #33429, #9847, #19285 ),
 .UNSPECIFIED., .F., .F.,
 ( 4, 2, 4 ),
 ( 0.000000000000000000, 0.4999999999999998890, 1.000000000000000000 ),
 .UNSPECIFIED. ) ;
#32651 = ADVANCED_FACE ( 'NONE', ( #45468 ), #36298, .F. ) ;
#32652 = PLANE ( 'NONE',  #30831 ) ;
#32653 = CARTESIAN_POINT ( 'NONE',  ( -7.654537165450999936, -55.51943464808999806, -10.01332852686999964 ) ) ;
#32654 = CARTESIAN_POINT ( 'NONE',  ( 7.541194259660339405, -78.80083539858046038, -5.358726617299357287 ) ) ;
#32655 = CARTESIAN_POINT ( 'NONE',  ( 4.774437967263952309, -76.54142007752965071, 10.73626118653558947 ) ) ;
#32656 = CARTESIAN_POINT ( 'NONE',  ( -0.1577469407028221082, -23.75042584457683148, -11.00002392222777381 ) ) ;
#32657 = DIRECTION ( 'NONE',  ( -0.9999999999995751176, 0.000000000000000000, -9.217549095371770968E-07 ) ) ;
#32658 = CARTESIAN_POINT ( 'NONE',  ( -9.180191738191043171, -80.14658889808482911, -6.059864792341575601 ) ) ;
#32659 = DIRECTION ( 'NONE',  ( 0.000000000000000000, -1.000000000000000000, 0.000000000000000000 ) ) ;
#32660 = CARTESIAN_POINT ( 'NONE',  ( 1.604500897319000030, -80.48192549782599770, -3.805795630178999911 ) ) ;
#32661 = CYLINDRICAL_SURFACE ( 'NONE', #42701, 12.00000000000000000 ) ;
#32662 = CARTESIAN_POINT ( 'NONE',  ( 1.036004598597317639, -82.89747191575634133, 0.6991915507269829133 ) ) ;
#32663 = CARTESIAN_POINT ( 'NONE',  ( 4.980329458316080427, -77.06875000000002274, -8.124224631303468058 ) ) ;
#32664 = DIRECTION ( 'NONE',  ( 0.000000000000000000, 1.000000000000000000, 0.000000000000000000 ) ) ;
#32665 = DIRECTION ( 'NONE',  ( 0.000000000000000000, 1.000000000000000000, 0.000000000000000000 ) ) ;
#32666 = EDGE_CURVE ( 'NONE', #37266, #30862, #4427, .T. ) ;
#32667 = CARTESIAN_POINT ( 'NONE',  ( -9.830801209645999350, -60.89088557979000171, -7.765011064359000237 ) ) ;
#32668 = DIRECTION ( 'NONE',  ( 0.000000000000000000, -1.000000000000000000, 0.000000000000000000 ) ) ;
#32669 = CARTESIAN_POINT ( 'NONE',  ( 1.157527094954509117, -79.54359519752044605, -0.9749728451049136657 ) ) ;
#32670 = CARTESIAN_POINT ( 'NONE',  ( 14.00000000000000000, -69.46217755556000384, 5.544640311636000234E-06 ) ) ;
#32671 = CARTESIAN_POINT ( 'NONE',  ( 3.346724862759000274, -2.316915364169000124, 0.9739846248380000793 ) ) ;
#32672 = DIRECTION ( 'NONE',  ( 1.000000000000000000, 0.000000000000000000, 0.000000000000000000 ) ) ;
#32673 = AXIS2_PLACEMENT_3D ( 'NONE', #38444, #46756, #16015 ) ;
#32674 = CARTESIAN_POINT ( 'NONE',  ( 9.388046065757025715, -77.24119165340866289, 5.283002242768499279 ) ) ;
#32675 = DIRECTION ( 'NONE',  ( -0.7071067811865475727, 0.000000000000000000, -0.7071067811865475727 ) ) ;
#32677 = CARTESIAN_POINT ( 'NONE',  ( -9.438868967565998247, -79.39261762096144537, -5.601050722391000214 ) ) ;
#32676 = DIRECTION ( 'NONE',  ( 0.000000000000000000, -1.000000000000000000, 0.000000000000000000 ) ) ;
#32678 = CARTESIAN_POINT ( 'NONE',  ( -8.570684284043998957, -76.19351098207999939, 8.487147852098999579 ) ) ;
#32679 = ORIENTED_EDGE ( 'NONE', *, *, #41033, .F. ) ;
#32680 = AXIS2_PLACEMENT_3D ( 'NONE', #41651, #14770, #54933 ) ;
#32681 = CARTESIAN_POINT ( 'NONE',  ( -3.193955991187000354, -85.15596544543099355, -2.346193924555000088 ) ) ;
#32682 = EDGE_CURVE ( 'NONE', #16336, #34323, #42548, .T. ) ;
#32683 = B_SPLINE_CURVE_WITH_KNOTS ( 'NONE', 3,
 ( #53496, #49073, #8623, #4199, #8920, #58218 ),
 .UNSPECIFIED., .F., .F.,
 ( 4, 2, 4 ),
 ( 0.000000000000000000, 0.5000000000000000000, 1.000000000000000000 ),
 .UNSPECIFIED. ) ;
#32684 = CARTESIAN_POINT ( 'NONE',  ( -2.563933300740000032, -80.81563101109908587, -10.99401458260000020 ) ) ;
#32685 = VECTOR ( 'NONE', #418, 1000.000000000000000 ) ;
#32686 = CARTESIAN_POINT ( 'NONE',  ( 9.188646138531803231, -78.34088890680163786, -1.063366993189087228 ) ) ;
#32687 = CARTESIAN_POINT ( 'NONE',  ( 8.121706841766027196, -53.96372996663640009, 9.841114038326725932 ) ) ;
#32688 = CARTESIAN_POINT ( 'NONE',  ( -9.302864017704999711, -76.94885861019999140, -6.266965030821000759 ) ) ;
#32689 = CARTESIAN_POINT ( 'NONE',  ( 9.499178638196321245, -79.00092112126561972, 0.1004274591880019996 ) ) ;
#32690 = CARTESIAN_POINT ( 'NONE',  ( 8.270224399031000928, -78.03490534060698280, -5.144228231339999624 ) ) ;
#32691 = AXIS2_PLACEMENT_3D ( 'NONE', #33793, #30523, #52687 ) ;
#32692 = CARTESIAN_POINT ( 'NONE',  ( 1.571434226476000173, -83.11189561955099236, -0.5530452149683998675 ) ) ;
#32693 = CARTESIAN_POINT ( 'NONE',  ( 3.407095545933000569, -78.77851879815550262, 0.000000000000000000 ) ) ;
#32694 = CARTESIAN_POINT ( 'NONE',  ( -2.292169028871041903, -76.10729166666139633, 10.76107357871677550 ) ) ;
#32695 = ORIENTED_EDGE ( 'NONE', *, *, #31687, .F. ) ;
#32696 = CARTESIAN_POINT ( 'NONE',  ( -3.237754142234346322, -0.9583333333332144655, 0.6872744716274413745 ) ) ;
#32697 = DIRECTION ( 'NONE',  ( -1.000000000000000000, 0.000000000000000000, 0.000000000000000000 ) ) ;
#32698 = CARTESIAN_POINT ( 'NONE',  ( -0.3187246912203000049, -80.57556890496380220, 11.26088853021000169 ) ) ;
#32699 = CARTESIAN_POINT ( 'NONE',  ( 1.081559480311999888, -3.500000000000000000, -3.328697807033000000 ) ) ;
#32700 = ORIENTED_EDGE ( 'NONE', *, *, #1866, .T. ) ;
#32701 = DIRECTION ( 'NONE',  ( -1.000000000000000000, 0.000000000000000000, 0.000000000000000000 ) ) ;
#32702 = LINE ( 'NONE', #50750, #22760 ) ;
#32703 = ORIENTED_EDGE ( 'NONE', *, *, #41128, .T. ) ;
#32704 = CARTESIAN_POINT ( 'NONE',  ( -8.689305806348999184, -77.82054998477100582, -8.513430283325000403 ) ) ;
#32705 = CARTESIAN_POINT ( 'NONE',  ( 7.635939347835848601, -60.57525282293972424, -10.36595956260653217 ) ) ;
#32706 = ORIENTED_EDGE ( 'NONE', *, *, #55969, .T. ) ;
#32707 = CARTESIAN_POINT ( 'NONE',  ( -0.9351132745867291041, -80.54278198314504777, 0.8292394773563549482 ) ) ;
#32708 = SHAPE_REPRESENTATION_RELATIONSHIP ( 'NONE' , 'NONE' ,  #4074, #463 ) ;
#32709 = CARTESIAN_POINT ( 'NONE',  ( 8.193575559979001000, -79.18625781507998340, 5.316613930189999948 ) ) ;
#32710 = ORIENTED_EDGE ( 'NONE', *, *, #4344, .F. ) ;
#32711 = CARTESIAN_POINT ( 'NONE',  ( 12.48375942314000042, -55.42730665069999674, 1.669542353228000042 ) ) ;
#32712 = CARTESIAN_POINT ( 'NONE',  ( 0.000000000000000000, -87.20000000000000284, 0.000000000000000000 ) ) ;
#32713 = EDGE_LOOP ( 'NONE', ( #3747, #40178, #56409, #1385 ) ) ;
#32714 = CARTESIAN_POINT ( 'NONE',  ( -12.66232158686000098, -25.13482640580999927, -0.5080765942055999185 ) ) ;
#32715 = CARTESIAN_POINT ( 'NONE',  ( 5.102724688570000389, -77.89883971678199259, 7.811319209985999379 ) ) ;
#32716 = ADVANCED_FACE ( 'NONE', ( #54889 ), #6392, .T. ) ;
#32717 = CARTESIAN_POINT ( 'NONE',  ( 4.000000000000000000, -5.000000000000000000, -0.5999999999999999778 ) ) ;
#32718 = LINE ( 'NONE', #10315, #19511 ) ;
#32719 = CARTESIAN_POINT ( 'NONE',  ( 1.577629893834067598, -86.25171438276198899, 3.635239426043075373 ) ) ;
#32720 = CARTESIAN_POINT ( 'NONE',  ( 8.131718752285998164, -76.87468074736040080, -4.888939325748999920 ) ) ;
#32721 = AXIS2_PLACEMENT_3D ( 'NONE', #27359, #4348, #40955 ) ;
#32722 = CARTESIAN_POINT ( 'NONE',  ( 0.3846651997978238757, -79.20413038734237432, 1.459419617943195968 ) ) ;
#32723 = CARTESIAN_POINT ( 'NONE',  ( -1.781408810351462479, -79.93333332603567953, 3.639624897007596616 ) ) ;
#32724 = ORIENTED_EDGE ( 'NONE', *, *, #54272, .F. ) ;
#32725 = CARTESIAN_POINT ( 'NONE',  ( 6.153863461931999623, -76.14932493800000657, -10.66140155521000032 ) ) ;
#32726 = CARTESIAN_POINT ( 'NONE',  ( -0.7520647764090000464, -80.99167289250799229, -1.313341758254999991 ) ) ;
#32727 = AXIS2_PLACEMENT_3D ( 'NONE', #32553, #18713, #1590 ) ;
#32728 = CARTESIAN_POINT ( 'NONE',  ( -0.7965256724932753274, -1.956068631034633798, -3.427793819624585403 ) ) ;
#32729 = CARTESIAN_POINT ( 'NONE',  ( 12.60413670420000010, -18.69283319134000010, 1.799502287691000069 ) ) ;
#32730 = VECTOR ( 'NONE', #8904, 1000.000000000000114 ) ;
#32731 = CARTESIAN_POINT ( 'NONE',  ( 0.4482635754052999855, -78.61057602857999882, -12.25553529036999834 ) ) ;
#32732 = CARTESIAN_POINT ( 'NONE',  ( -10.85634995915000012, -76.10481652993199475, -5.741293403527000017 ) ) ;
#32733 = CARTESIAN_POINT ( 'NONE',  ( -3.140027144888993593, -85.94828564506399005, 1.398030157552013319 ) ) ;
#32734 = EDGE_CURVE ( 'NONE', #45676, #3012, #24407, .T. ) ;
#32735 = CARTESIAN_POINT ( 'NONE',  ( -6.314216249843999762, -76.81193998579799143, 7.143954968317999921 ) ) ;
#32736 = CARTESIAN_POINT ( 'NONE',  ( -5.598612431920771293, -78.13655615605678406, -10.68738653231515201 ) ) ;
#32737 = CARTESIAN_POINT ( 'NONE',  ( 9.453938376997999882, -79.04522201375752388, 6.036651369377000087 ) ) ;
#32738 = B_SPLINE_CURVE_WITH_KNOTS ( 'NONE', 3,
 ( #2623, #47221, #57203, #12333, #16196, #51928, #16771, #34752, #34173, #33887, #6753, #11765, #52779, #7326, #24760, #42775, #11487, #47794 ),
 .UNSPECIFIED., .F., .F.,
 ( 4, 2, 2, 2, 2, 2, 2, 2, 4 ),
 ( 0.000000000000000000, 0.1249999999999999722, 0.2499999999999999445, 0.3749999999999998890, 0.4999999999999998890, 0.6249999999999998890, 0.7499999999999997780, 0.8749999999999998890, 1.000000000000000000 ),
 .UNSPECIFIED. ) ;
#32739 = ORIENTED_EDGE ( 'NONE', *, *, #27863, .T. ) ;
#32740 = CARTESIAN_POINT ( 'NONE',  ( -1.295013057735999951, -82.04302107981000347, -0.3858917059242000236 ) ) ;
#32741 = CARTESIAN_POINT ( 'NONE',  ( 9.242241171838999847, -77.10391830622759812, 2.968601151647999536 ) ) ;
#32742 = DIRECTION ( 'NONE',  ( 0.7071067811865474617, 0.000000000000000000, 0.7071067811865474617 ) ) ;
#32743 = LINE ( 'NONE', #50791, #16304 ) ;
#32744 = CARTESIAN_POINT ( 'NONE',  ( 3.481453347827000222, -2.659774131856000423, 1.293805899609000054 ) ) ;
#32745 = CARTESIAN_POINT ( 'NONE',  ( 11.76923221829999910, -77.33985457952199738, 1.980068107414000300 ) ) ;
#32746 = CARTESIAN_POINT ( 'NONE',  ( 9.511010664898998712, -77.96950448043199344, 1.514558053418999961 ) ) ;
#32747 = EDGE_CURVE ( 'NONE', #29062, #1603, #1065, .T. ) ;
#32748 = CARTESIAN_POINT ( 'NONE',  ( -10.33041713801597972, -76.16000623662056057, 5.601055854838120851 ) ) ;
#32749 = CARTESIAN_POINT ( 'NONE',  ( -0.2648292726109000017, -79.40352125521398818, 10.91353432424999959 ) ) ;
#32750 = CARTESIAN_POINT ( 'NONE',  ( -3.335532751159927312, -85.80681307385599155, 1.410355715538893051 ) ) ;
#32751 = ORIENTED_EDGE ( 'NONE', *, *, #56017, .T. ) ;
#32752 = CARTESIAN_POINT ( 'NONE',  ( 11.99950779401364187, -75.80399128148174270, 0.6018682196318532185 ) ) ;
#32753 = EDGE_CURVE ( 'NONE', #49740, #18403, #43287, .T. ) ;
#32754 = CARTESIAN_POINT ( 'NONE',  ( 10.24628572959450779, -79.02087622563911395, -5.923537098732725603 ) ) ;
#32755 = CARTESIAN_POINT ( 'NONE',  ( -9.396085398178614767, -76.85208333333332575, -7.220923959705254802 ) ) ;
#32756 = CARTESIAN_POINT ( 'NONE',  ( 5.330173052271000245, -78.32510122146300091, 9.594439332582000546 ) ) ;
#32757 = CARTESIAN_POINT ( 'NONE',  ( -10.75000000000000000, -77.00000000000000000, 0.000000000000000000 ) ) ;
#32758 = CARTESIAN_POINT ( 'NONE',  ( -0.09698300086874001025, -79.76726403785698949, -9.669821086516000364 ) ) ;
#32759 = CARTESIAN_POINT ( 'NONE',  ( 8.188285776315000319, -17.29506253989999820, -9.395726099566001466 ) ) ;
#32760 = CARTESIAN_POINT ( 'NONE',  ( 7.624341764906000130, -55.53514850498000044, 10.42531124851000079 ) ) ;
#32761 = ORIENTED_EDGE ( 'NONE', *, *, #27660, .F. ) ;
#32762 = AXIS2_PLACEMENT_3D ( 'NONE', #27926, #1681, #19093 ) ;
#32763 = CARTESIAN_POINT ( 'NONE',  ( -0.4163023988263999664, -79.39864834222998979, -11.25436168207999899 ) ) ;
#32764 = CARTESIAN_POINT ( 'NONE',  ( 12.70305331333692855, -16.96853698854184245, 0.8727610012103214077 ) ) ;
#32765 = CARTESIAN_POINT ( 'NONE',  ( -8.787981800519466091, -79.60831884209565601, -7.924599827265385699 ) ) ;
#32766 = CARTESIAN_POINT ( 'NONE',  ( -3.913805356273367675, -78.48547955770028750, -0.07378243972141844409 ) ) ;
#32767 = CARTESIAN_POINT ( 'NONE',  ( -1.336644981821593081, -77.33686301158515164, 12.00120481110041659 ) ) ;
#32769 = CARTESIAN_POINT ( 'NONE',  ( -1.034407521427512133, -81.55267419125448214, 0.7041627674574237883 ) ) ;
#32768 = CARTESIAN_POINT ( 'NONE',  ( -1.195105308512000031, -81.62325104643299767, 0.5588281594584000311 ) ) ;
#32770 = VECTOR ( 'NONE', #37588, 1000.000000000000000 ) ;
#32771 = CARTESIAN_POINT ( 'NONE',  ( -6.507505845087319329, -76.99999999999998579, -6.850455418477346292 ) ) ;
#32772 = CARTESIAN_POINT ( 'NONE',  ( 10.98362417419999915, -23.15000000000000213, -0.5999999999999999778 ) ) ;
#32773 = EDGE_CURVE ( 'NONE', #14039, #52988, #7557, .T. ) ;
#32774 = CIRCLE ( 'NONE', #8256, 4.299999999999999822 ) ;
#32775 = CARTESIAN_POINT ( 'NONE',  ( -7.396918292183192634, -79.94791666666667140, 5.684557159767932077 ) ) ;
#32776 = CARTESIAN_POINT ( 'NONE',  ( 10.99999999999999645, -79.45864668888548010, 1.195232468347081189 ) ) ;
#32777 = CARTESIAN_POINT ( 'NONE',  ( -6.933189095244579825, -79.72395833333175119, -6.238628562272925393 ) ) ;
#32778 = ORIENTED_EDGE ( 'NONE', *, *, #1233, .T. ) ;
#32779 = ORIENTED_EDGE ( 'NONE', *, *, #8159, .T. ) ;
#32780 = CARTESIAN_POINT ( 'NONE',  ( 2.278690965393999956, -79.02258998579800675, -9.759650287631000509 ) ) ;
#32781 = CARTESIAN_POINT ( 'NONE',  ( 5.986666392495521904, -78.77217535623724132, -8.928609192334358013 ) ) ;
#32782 = ORIENTED_EDGE ( 'NONE', *, *, #19684, .T. ) ;
#32783 = CARTESIAN_POINT ( 'NONE',  ( -7.860507001410999450, -76.68702291099154422, 7.955276143908999842 ) ) ;
#32784 = CARTESIAN_POINT ( 'NONE',  ( -3.219061024817564842, -83.28645834781006840, -1.224520844437955613 ) ) ;
#32785 = CARTESIAN_POINT ( 'NONE',  ( -1.460959015002474493, -80.37916666666664867, 0.3926218265389144757 ) ) ;
#32786 = CARTESIAN_POINT ( 'NONE',  ( 8.478749451788999636, -61.67812788887000153, 9.108222796200001525 ) ) ;
#32787 = CARTESIAN_POINT ( 'NONE',  ( -11.18443158117183778, -76.51668518724613932, 4.872433950202917252 ) ) ;
#32788 = CARTESIAN_POINT ( 'NONE',  ( -4.743944233800447385, -78.64250398762337113, -11.00068109039020747 ) ) ;
#32789 = CARTESIAN_POINT ( 'NONE',  ( -10.75729140709000120, -78.78896392293299300, -3.177859684493999914 ) ) ;
#32790 = ORIENTED_EDGE ( 'NONE', *, *, #22137, .F. ) ;
#32791 = CARTESIAN_POINT ( 'NONE',  ( 1.568318300085000120E-14, -0.05000000003700048185, -12.84999999995999964 ) ) ;
#32792 = EDGE_LOOP ( 'NONE', ( #30209, #44458, #37807, #49141 ) ) ;
#32793 = CARTESIAN_POINT ( 'NONE',  ( 9.162130905092393363, -77.36116891436404330, 1.277012193982459687 ) ) ;
#32794 = CARTESIAN_POINT ( 'NONE',  ( 1.125436458607999901, -79.53562962141599257, 0.6884462015638999066 ) ) ;
#32795 = CARTESIAN_POINT ( 'NONE',  ( 0.000000000000000000, -75.15999999999999659, 0.000000000000000000 ) ) ;
#32796 = CARTESIAN_POINT ( 'NONE',  ( -0.2914033309752999679, -78.60250196101499398, -1.588174433604999880 ) ) ;
#32797 = DIRECTION ( 'NONE',  ( 0.7071067811865475727, 0.000000000000000000, -0.7071067811865475727 ) ) ;
#32798 = CARTESIAN_POINT ( 'NONE',  ( -12.00000000000000000, -23.15000000000000213, 0.000000000000000000 ) ) ;
#32799 = CARTESIAN_POINT ( 'NONE',  ( -1.573065832928000063, -78.74975765224999691, 0.4172852021023999991 ) ) ;
#32800 = CARTESIAN_POINT ( 'NONE',  ( -3.198229570894999707, -78.87905496681159434, -2.679852064138000145 ) ) ;
#32801 = AXIS2_PLACEMENT_3D ( 'NONE', #19122, #22965, #50723 ) ;
#32802 = CARTESIAN_POINT ( 'NONE',  ( 7.763360352781000451, -78.74140324543799352, 7.708310604078000061 ) ) ;
#32803 = ADVANCED_FACE ( 'NONE', ( #42422 ), #11135, .T. ) ;
#32804 = FACE_OUTER_BOUND ( 'NONE', #47781, .T. ) ;
#32805 = CARTESIAN_POINT ( 'NONE',  ( -7.761030428335000231, -24.08151201375000028, -9.835168816226998345 ) ) ;
#32806 = CARTESIAN_POINT ( 'NONE',  ( 12.49306764019000049, -60.08056535122999975, -1.667917367065999912 ) ) ;
#32807 = CARTESIAN_POINT ( 'NONE',  ( -3.299912862228999710, -84.55426028386798976, 1.294428919074000151 ) ) ;
#32808 = ORIENTED_EDGE ( 'NONE', *, *, #12073, .T. ) ;
#32809 = EDGE_CURVE ( 'NONE', #11254, #11325, #51771, .T. ) ;
#32810 = CARTESIAN_POINT ( 'NONE',  ( -10.99598848309850574, -77.19999999999996021, 0.3327073738962888494 ) ) ;
#32811 = CARTESIAN_POINT ( 'NONE',  ( -0.8211341099608999716, -80.41498426945000233, -1.491829658087999944 ) ) ;
#32812 = CARTESIAN_POINT ( 'NONE',  ( 9.133850598315257585, -77.89447637907150579, 5.680044527171443036 ) ) ;
#32813 = CARTESIAN_POINT ( 'NONE',  ( -10.26943924278000075, -78.52305958491099602, 6.168847710360999770 ) ) ;
#32814 = CARTESIAN_POINT ( 'NONE',  ( 0.000000000000000000, -75.15999999999999659, 0.000000000000000000 ) ) ;
#32815 = CARTESIAN_POINT ( 'NONE',  ( -6.606735055424326930, -79.02724754890354575, 8.596828543386198618 ) ) ;
#32816 = VECTOR ( 'NONE', #25720, 1000.000000000000000 ) ;
#32817 = CARTESIAN_POINT ( 'NONE',  ( 2.800339161470473570, -2.948150801642311691, -2.132651805043404902 ) ) ;
#32818 = CARTESIAN_POINT ( 'NONE',  ( 8.156436652089588790, -80.90677963425484620, 7.002206209730132080 ) ) ;
#32819 = CARTESIAN_POINT ( 'NONE',  ( -4.670571261811000241, -78.49550106883198453, 8.172940633331000626 ) ) ;
#32820 = B_SPLINE_CURVE_WITH_KNOTS ( 'NONE', 3,
 ( #16024, #42896, #24593, #7161, #30157, #2742, #42607, #2170, #20171, #38159 ),
 .UNSPECIFIED., .F., .F.,
 ( 4, 2, 2, 2, 4 ),
 ( 0.3750002296912270938, 0.5312501722684203065, 0.6875001148456134636, 0.8437500574228067318, 1.000000000000000000 ),
 .UNSPECIFIED. ) ;
#32821 = CARTESIAN_POINT ( 'NONE',  ( 0.3854429861649060207, -85.83735716284299144, -8.603922067879931745 ) ) ;
#32822 = CARTESIAN_POINT ( 'NONE',  ( -10.75275020201999965, -78.47680183458999181, -2.465785609032999925 ) ) ;
#32823 = CARTESIAN_POINT ( 'NONE',  ( -8.598496321198998871, -77.21327568127719587, -8.768570137950998600 ) ) ;
#32824 = CARTESIAN_POINT ( 'NONE',  ( -9.154119576699001115, -80.84287663268978008, 6.349747989568999884 ) ) ;
#32825 = ORIENTED_EDGE ( 'NONE', *, *, #57618, .F. ) ;
#32826 = CARTESIAN_POINT ( 'NONE',  ( -1.798336774605999944, -59.99644498018999883, -12.61277771568000006 ) ) ;
#32827 = EDGE_CURVE ( 'NONE', #28137, #48909, #35517, .T. ) ;
#32828 = FACE_OUTER_BOUND ( 'NONE', #49664, .T. ) ;
#32829 = CARTESIAN_POINT ( 'NONE',  ( -11.16975252231999960, -76.75880881764298636, 1.027088271520000040 ) ) ;
#32830 = CARTESIAN_POINT ( 'NONE',  ( -10.69701368780000017, -79.80164135007898096, 1.066019776055000090 ) ) ;
#32831 = CARTESIAN_POINT ( 'NONE',  ( 6.586108526242999694, -80.17391735373439587, 8.810401493720998900 ) ) ;
#32832 = CARTESIAN_POINT ( 'NONE',  ( -2.134093098436142366, -82.95885415248338290, 3.397881310131980470 ) ) ;
#32833 = LINE ( 'NONE', #45578, #661 ) ;
#32834 = DIRECTION ( 'NONE',  ( 3.497202527557000183E-12, 1.000000000000000000, 1.787522907329000142E-11 ) ) ;
#32835 = CARTESIAN_POINT ( 'NONE',  ( -1.752646046354000120, -84.95267953870899191, -3.786129546818000069 ) ) ;
#32836 = CARTESIAN_POINT ( 'NONE',  ( -1.460959015002474937, -80.47916666666665719, 0.3926218265389144757 ) ) ;
#32837 = CARTESIAN_POINT ( 'NONE',  ( 10.36289663187000087, -55.59893657650000165, -7.633501051906999457 ) ) ;
#32838 = CARTESIAN_POINT ( 'NONE',  ( 5.471330588277999674, -78.01383322178197943, 9.848526282906998830 ) ) ;
#32839 = CARTESIAN_POINT ( 'NONE',  ( 1.551146335801999898, -81.16853515462000246, 0.6076261867840000441 ) ) ;
#32840 = DIRECTION ( 'NONE',  ( 0.8090169943749182524, 0.000000000000000000, 0.5877852522925132162 ) ) ;
#32841 = CARTESIAN_POINT ( 'NONE',  ( 3.140974612311377090, -79.44583333333332575, -11.68767212001978528 ) ) ;
#32842 = CARTESIAN_POINT ( 'NONE',  ( -0.8592827076548754661, -81.32688287324717180, -1.244672245808209787 ) ) ;
#32843 = CARTESIAN_POINT ( 'NONE',  ( 0.3161824776153564498, -83.20767999258765713, 1.479864803184822497 ) ) ;
#32844 = CARTESIAN_POINT ( 'NONE',  ( 10.69999999999999929, -80.49999999999998579, 0.000000000000000000 ) ) ;
#32845 = CARTESIAN_POINT ( 'NONE',  ( -1.980584515756000030, -23.26485150094000076, -12.76303204340999997 ) ) ;
#32846 = VECTOR ( 'NONE', #51931, 1000.000000000000000 ) ;
#32847 = CARTESIAN_POINT ( 'NONE',  ( 9.500000000000000000, -77.54999999999999716, 0.000000000000000000 ) ) ;
#32848 = ORIENTED_EDGE ( 'NONE', *, *, #39847, .F. ) ;
#32849 = CARTESIAN_POINT ( 'NONE',  ( -0.6462729935705185946, -81.68201433982439141, -1.071111153078781353 ) ) ;
#32850 = CARTESIAN_POINT ( 'NONE',  ( -9.010285311145000975, -78.94123101036599621, -6.562724981485000164 ) ) ;
#32851 = CARTESIAN_POINT ( 'NONE',  ( 5.948961716885869500, -78.02087376917042150, 7.191048434022237146 ) ) ;
#32852 = ORIENTED_EDGE ( 'NONE', *, *, #20823, .T. ) ;
#32853 = ORIENTED_EDGE ( 'NONE', *, *, #58029, .F. ) ;
#32854 = CARTESIAN_POINT ( 'NONE',  ( 1.298531763578000264, -81.31981624179999812, -0.5690998499286999968 ) ) ;
#32855 = ORIENTED_EDGE ( 'NONE', *, *, #4587, .F. ) ;
#32857 = ADVANCED_FACE ( 'NONE', ( #10263 ), #33331, .F. ) ;
#32856 = ORIENTED_EDGE ( 'NONE', *, *, #50298, .F. ) ;
#32858 = CARTESIAN_POINT ( 'NONE',  ( 0.1963495408493571015, -81.86458333333975190, 1.500000000000000444 ) ) ;
#32859 = LINE ( 'NONE', #42625, #42417 ) ;
#32860 = VECTOR ( 'NONE', #6239, 1000.000000000000000 ) ;
#32861 = PRODUCT_CONTEXT ( 'NONE', #39066, 'mechanical' ) ;
#32862 = CARTESIAN_POINT ( 'NONE',  ( -1.514197290259749362, -79.93333332572275651, 3.093681355356981744 ) ) ;
#32863 = CARTESIAN_POINT ( 'NONE',  ( -7.762343146465000565, -78.37516001420199530, -6.339840787406999745 ) ) ;
#32864 = CARTESIAN_POINT ( 'NONE',  ( 1.818239999436394250, -78.24087318384329137, -9.069458920223979703 ) ) ;
#32865 = LINE ( 'NONE', #18446, #50827 ) ;
#32866 = ORIENTED_EDGE ( 'NONE', *, *, #15687, .F. ) ;
#32868 = EDGE_LOOP ( 'NONE', ( #2187, #57593, #54066, #8853 ) ) ;
#32867 = B_SPLINE_CURVE_WITH_KNOTS ( 'NONE', 3,
 ( #43178, #42887, #2159, #21015, #20160, #15719 ),
 .UNSPECIFIED., .F., .F.,
 ( 4, 1, 1, 4 ),
 ( 0.000000000000000000, 0.3333333333333000081, 0.6666666666667000474, 1.000000000000000000 ),
 .UNSPECIFIED. ) ;
#32869 = CARTESIAN_POINT ( 'NONE',  ( -7.805592913195344096, -77.55492559948099540, 4.964263552560149506 ) ) ;
#32870 = DIRECTION ( 'NONE',  ( -0.7071067811864970576, 3.544461080512985563E-08, 0.7071067811865970887 ) ) ;
#32871 = CARTESIAN_POINT ( 'NONE',  ( 0.9218200799623694763, -79.32291666666667140, 1.199500263597272465 ) ) ;
#32872 = B_SPLINE_CURVE_WITH_KNOTS ( 'NONE', 3,
 ( #17459, #35447, #58198, #17761, #13020, #31018 ),
 .UNSPECIFIED., .F., .F.,
 ( 4, 2, 4 ),
 ( 0.000000000000000000, 0.5000000000000000000, 1.000000000000000000 ),
 .UNSPECIFIED. ) ;
#32873 = CARTESIAN_POINT ( 'NONE',  ( 0.6484536762478674277, -61.92402982684195933, -12.70397497895977601 ) ) ;
#32874 = CARTESIAN_POINT ( 'NONE',  ( 9.131029190779001325, -77.49236239375397872, -3.285576857342999979 ) ) ;
#32875 = DIRECTION ( 'NONE',  ( 0.000000000000000000, 1.000000000000000000, 0.000000000000000000 ) ) ;
#32876 = CARTESIAN_POINT ( 'NONE',  ( 0.9182913743456745381, -85.93361904366226156, 3.850309887564324463 ) ) ;
#32877 = CARTESIAN_POINT ( 'NONE',  ( 3.140974612311326908, -76.75416666666663446, 11.68767212001979772 ) ) ;
#32878 = CARTESIAN_POINT ( 'NONE',  ( -1.274573384913999963, -80.10198252799999352, 0.7293221697183999153 ) ) ;
#32879 = DIRECTION ( 'NONE',  ( 0.7071067811865475727, 0.000000000000000000, 0.7071067811865475727 ) ) ;
#32880 = CARTESIAN_POINT ( 'NONE',  ( 0.05508875196996424611, -76.57451616085182877, 11.74980235316340682 ) ) ;
#32881 = EDGE_CURVE ( 'NONE', #36154, #42760, #5938, .T. ) ;
#32882 = CARTESIAN_POINT ( 'NONE',  ( 3.981833008139999741, -82.53049761187099875, 0.4016559218788000041 ) ) ;
#32883 = VECTOR ( 'NONE', #45613, 999.9999999999998863 ) ;
#32884 = CARTESIAN_POINT ( 'NONE',  ( 1.507312305499400207, -79.49486076828772241, -0.09857350602148712282 ) ) ;
#32885 = CARTESIAN_POINT ( 'NONE',  ( -0.8449659473473000171, -78.95261001420199420, 9.650246712936999316 ) ) ;
#32886 = CARTESIAN_POINT ( 'NONE',  ( -9.329288041359642847, -76.64178376729412889, -5.387529410381943329 ) ) ;
#32887 = DIRECTION ( 'NONE',  ( 0.000000000000000000, -1.000000000000000000, 1.134344766989000102E-14 ) ) ;
#32889 = CARTESIAN_POINT ( 'NONE',  ( -1.112801787005999854, -79.21864855312099962, -0.6258220204580999813 ) ) ;
#32888 = CARTESIAN_POINT ( 'NONE',  ( 0.000000000000000000, -78.49999999999998579, 0.000000000000000000 ) ) ;
#32890 = CARTESIAN_POINT ( 'NONE',  ( -7.374560639699019760, -78.32708333333330586, 9.596002108778129980 ) ) ;
#32891 = DIRECTION ( 'NONE',  ( 0.000000000000000000, 1.000000000000000000, 0.000000000000000000 ) ) ;
#32892 = CARTESIAN_POINT ( 'NONE',  ( 2.534829140202000008, -2.169001425904999891, 2.839140403360000509 ) ) ;
#32893 = CARTESIAN_POINT ( 'NONE',  ( 0.7681833999686451531, -79.17708333333332860, -0.9995835529977240563 ) ) ;
#32894 = EDGE_LOOP ( 'NONE', ( #20548, #23574, #50028, #19591, #2767, #45164 ) ) ;
#32895 = CARTESIAN_POINT ( 'NONE',  ( -7.901937437514109597, -78.86666666666667425, -8.782705133630996031 ) ) ;
#32896 = CARTESIAN_POINT ( 'NONE',  ( 11.06159046600000018, -78.35992084691199011, -1.510225926472999802 ) ) ;
#32897 = CARTESIAN_POINT ( 'NONE',  ( 8.796335266379989193, -79.00208333333331723, 6.760013919724051412 ) ) ;
#32898 = CARTESIAN_POINT ( 'NONE',  ( 12.54673349189000042, -61.62806887777999520, -0.9076721992841999542 ) ) ;
#32899 = ADVANCED_FACE ( 'NONE', ( #41454 ), #43274, .F. ) ;
#32900 = CARTESIAN_POINT ( 'NONE',  ( 4.903292266777000030, -79.99716956313798732, -8.177287202055998350 ) ) ;
#32901 = CARTESIAN_POINT ( 'NONE',  ( 11.85869973992999959, -77.73177122362999114, 5.358216250391999225 ) ) ;
#32902 = CARTESIAN_POINT ( 'NONE',  ( 10.70966587101897183, -79.35754135609677462, 1.004977551424543369 ) ) ;
#32903 = CIRCLE ( 'NONE', #11238, 12.50000000000000000 ) ;
#32904 = DIRECTION ( 'NONE',  ( -0.7071067811865474617, -3.445410891336226740E-11, -0.7071067811865474617 ) ) ;
#32905 = DIRECTION ( 'NONE',  ( 0.000000000000000000, 1.000000000000000000, 0.000000000000000000 ) ) ;
#32906 = CARTESIAN_POINT ( 'NONE',  ( -10.62852719317000094, -77.21828546760299616, 3.420469065344999837 ) ) ;
#32907 = CARTESIAN_POINT ( 'NONE',  ( 1.505061616724999940, -82.09947563412200111, -0.06074805737713000198 ) ) ;
#32908 = DIRECTION ( 'NONE',  ( 0.000000000000000000, 0.000000000000000000, 1.000000000000000000 ) ) ;
#32910 = CARTESIAN_POINT ( 'NONE',  ( -3.453171399369999950, -1.763032031398999999, -0.5706200895263999762 ) ) ;
#32909 = CARTESIAN_POINT ( 'NONE',  ( 1.204975038778999918, -83.34403886695498898, -3.775450321737999992 ) ) ;
#32911 = CARTESIAN_POINT ( 'NONE',  ( -9.554796630153999715, -79.57014805011500869, -0.02401403847836000235 ) ) ;
#32912 = CARTESIAN_POINT ( 'NONE',  ( 0.3926218265389159745, -80.75416666666666288, 1.460959015002474493 ) ) ;
#32913 = CARTESIAN_POINT ( 'NONE',  ( -1.141857967141000074, -79.69980780150500266, -0.6608524743567000259 ) ) ;
#32914 = CARTESIAN_POINT ( 'NONE',  ( 9.499157866768639380, -79.10080562451891240, 0.1004279358040388037 ) ) ;
#32915 = LINE ( 'NONE', #55965, #8693 ) ;
#32916 = ORIENTED_CLOSED_SHELL ( 'NONE', *, #50346, .F. );
#32917 = VERTEX_POINT ( 'NONE', #35770 ) ;
#32918 = ORIENTED_EDGE ( 'NONE', *, *, #39325, .F. ) ;
#32919 = CARTESIAN_POINT ( 'NONE',  ( 11.77452260639999970, -79.89232299303098728, 1.259536412044000020 ) ) ;
#32920 = DIRECTION ( 'NONE',  ( -0.9999999923520045408, 0.000000000000000000, -0.0001236769620559006555 ) ) ;
#32921 = DIRECTION ( 'NONE',  ( 0.7071067811865969777, -0.7071067811864980568, -1.459345738583993741E-08 ) ) ;
#32922 = ORIENTED_EDGE ( 'NONE', *, *, #54959, .F. ) ;
#32923 = PRESENTATION_LAYER_ASSIGNMENT (  '', '', ( #46405 ) ) ;
#32924 = CARTESIAN_POINT ( 'NONE',  ( 11.32533557775999888, -77.84787174848798941, -3.764608412264000226 ) ) ;
#32925 = VERTEX_POINT ( 'NONE', #49372 ) ;
#32927 = EDGE_CURVE ( 'NONE', #57120, #34348, #19343, .T. ) ;
#32926 = EDGE_LOOP ( 'NONE', ( #36914, #4031, #26906, #23618, #39600 ) ) ;
#32928 = CARTESIAN_POINT ( 'NONE',  ( -6.606377239730371720, -78.92708333333332860, 8.596418555780411808 ) ) ;
#32929 = AXIS2_PLACEMENT_3D ( 'NONE', #9320, #53310, #48891 ) ;
#32930 = VERTEX_POINT ( 'NONE', #44343 ) ;
#32931 = EDGE_CURVE ( 'NONE', #34281, #7212, #7306, .T. ) ;
#32932 = CARTESIAN_POINT ( 'NONE',  ( 2.784356622819999849, -80.77793935167099448, -2.197482209534999953 ) ) ;
#32933 = DIRECTION ( 'NONE',  ( -3.957428551341999799E-14, -1.534448722697999916E-11, 1.000000000000000000 ) ) ;
#32934 = ORIENTED_EDGE ( 'NONE', *, *, #53131, .F. ) ;
#32935 = CARTESIAN_POINT ( 'NONE',  ( -9.298479816475882842, -53.91187382742327827, -8.385858173807932303 ) ) ;
#32936 = CARTESIAN_POINT ( 'NONE',  ( -10.75000000000000000, -77.00000000000000000, 0.000000000000000000 ) ) ;
#32937 = VERTEX_POINT ( 'NONE', #1829 ) ;
#32938 = CARTESIAN_POINT ( 'NONE',  ( 1.232226823824853712, -17.47709088732368343, 12.50408896749734566 ) ) ;
#32939 = CARTESIAN_POINT ( 'NONE',  ( 6.240635229950907359, -78.16931989252493906, 7.431574511284630979 ) ) ;
#32940 = AXIS2_PLACEMENT_3D ( 'NONE', #34650, #12232, #39389 ) ;
#32941 = B_SPLINE_CURVE_WITH_KNOTS ( 'NONE', 3,
 ( #31565, #49614, #18016, #40, #26852, #8273, #40449, #57865, #13574, #30977 ),
 .UNSPECIFIED., .F., .F.,
 ( 4, 2, 2, 2, 4 ),
 ( 0.000000000000000000, 0.2500000000000000000, 0.5000000000000000000, 0.7500000000000000000, 1.000000000000000000 ),
 .UNSPECIFIED. ) ;
#32942 = CARTESIAN_POINT ( 'NONE',  ( -7.434989412783546747, -79.79999999999998295, -9.267694697335807419 ) ) ;
#32943 = DIRECTION ( 'NONE',  ( 0.7071067812863980340, 6.386292029988980325E-09, 0.7071067810866970005 ) ) ;
#32944 = AXIS2_PLACEMENT_3D ( 'NONE', #24331, #2199, #47368 ) ;
#32945 = CARTESIAN_POINT ( 'NONE',  ( 1.487026788147999934, -77.38724284451876656, -9.589549613196998834 ) ) ;
#32946 = CARTESIAN_POINT ( 'NONE',  ( 10.12567350656000009, -75.98320989681799631, 4.748118780173999909 ) ) ;
#32947 = CARTESIAN_POINT ( 'NONE',  ( -10.26699006316255591, -77.25833333333333997, 5.917523019358029934 ) ) ;
#32948 = CARTESIAN_POINT ( 'NONE',  ( -7.612971540256999958, -55.47547726255000100, -10.53003236230999917 ) ) ;
#32949 = CARTESIAN_POINT ( 'NONE',  ( -6.370113089561758812, -78.66462273621775125, -6.707093103444599969 ) ) ;
#32950 = CARTESIAN_POINT ( 'NONE',  ( 6.529670873989093849, -76.52793616002254851, 9.768490878051002468 ) ) ;
#32951 = CARTESIAN_POINT ( 'NONE',  ( 0.3135214471715045415, -23.68581381184938195, -10.99610567419499318 ) ) ;
#32952 = EDGE_CURVE ( 'NONE', #7885, #14050, #33325, .T. ) ;
#32953 = CARTESIAN_POINT ( 'NONE',  ( -0.2976639488673999967, -79.52725137340199524, 1.299989344602000108 ) ) ;
#32954 = CARTESIAN_POINT ( 'NONE',  ( -5.652729497046634854, -80.18219462805302555, -9.436345438157960785 ) ) ;
#32955 = CARTESIAN_POINT ( 'NONE',  ( -1.103931350765845476, -61.42083747905900282, -12.50298439261660199 ) ) ;
#32956 = CARTESIAN_POINT ( 'NONE',  ( 3.603372836998999684, -79.04278455456849883, -1.649753055453999862 ) ) ;
#32957 = CARTESIAN_POINT ( 'NONE',  ( 9.438309774439000321, -77.92631332859899373, -2.022706718371000356 ) ) ;
#32958 = CARTESIAN_POINT ( 'NONE',  ( -10.65912025651878281, -78.08960475230161080, 1.406514330260667078 ) ) ;
#32959 = CARTESIAN_POINT ( 'NONE',  ( 1.148760496143379495, -82.88227549639147185, 0.4927867763867777029 ) ) ;
#32960 = CARTESIAN_POINT ( 'NONE',  ( -0.001533218590079363447, -77.02500000000000568, -9.529255218666872196 ) ) ;
#32961 = CARTESIAN_POINT ( 'NONE',  ( -3.851650068366999857, -78.96264283715740362, -1.616138016926814209E-14 ) ) ;
#32962 = DIRECTION ( 'NONE',  ( 0.000000000000000000, -1.000000000000000000, 0.000000000000000000 ) ) ;
#32963 = CARTESIAN_POINT ( 'NONE',  ( -8.485281374238999419, -59.94999999967000548, -8.485281374238999419 ) ) ;
#32964 = CARTESIAN_POINT ( 'NONE',  ( 12.56594317989000054, -23.24999999414999863, 1.750000000001000089 ) ) ;
#32965 = EDGE_CURVE ( 'NONE', #26186, #36137, #34408, .T. ) ;
#32966 = CARTESIAN_POINT ( 'NONE',  ( 12.70305380112397309, -25.03154493769342182, -0.8725910145142433683 ) ) ;
#32967 = CARTESIAN_POINT ( 'NONE',  ( -2.015551294784000191, -23.80347704843999779, -12.79857978895000059 ) ) ;
#32968 = CYLINDRICAL_SURFACE ( 'NONE', #24838, 1.750000000000001332 ) ;
#32970 = ADVANCED_FACE ( 'NONE', ( #36650 ), #42263, .F. ) ;
#32969 = CARTESIAN_POINT ( 'NONE',  ( 2.013632425233999879, -78.15144415034599490, -9.512575055159999238 ) ) ;
#32971 = CARTESIAN_POINT ( 'NONE',  ( -7.792426477851446265, -24.29102098708791857, -10.18245125506949300 ) ) ;
#32972 = CARTESIAN_POINT ( 'NONE',  ( -10.81678667190517906, -77.45531774696169691, -0.6574978399008775121 ) ) ;
#32973 = CARTESIAN_POINT ( 'NONE',  ( -0.8804656548073503952, -25.02803394707816054, -12.70299681151469606 ) ) ;
#32974 = CARTESIAN_POINT ( 'NONE',  ( 3.706103181433999971, -75.90547385439001005, -11.47841872256999984 ) ) ;
#32975 = ORIENTED_EDGE ( 'NONE', *, *, #12591, .T. ) ;
#32976 = CARTESIAN_POINT ( 'NONE',  ( -3.689341079140000090, -84.91546544543099628, 1.447322771837999955 ) ) ;
#32977 = CARTESIAN_POINT ( 'NONE',  ( 6.405550539766999840, -80.53584952307009814, 9.295753483539000328 ) ) ;
#32978 = CARTESIAN_POINT ( 'NONE',  ( 9.192561553568495469, -78.34118095183893615, -1.028967211150572547 ) ) ;
#32979 = CARTESIAN_POINT ( 'NONE',  ( 14.00000000000000000, -72.70000000000000284, 0.000000000000000000 ) ) ;
#32980 = CARTESIAN_POINT ( 'NONE',  ( 7.199825537761999961, -77.22122204021799519, 8.601198917431998936 ) ) ;
#32981 = CARTESIAN_POINT ( 'NONE',  ( 0.000000000000000000, -81.99999999999998579, 0.000000000000000000 ) ) ;
#32982 = CARTESIAN_POINT ( 'NONE',  ( -9.704555048820999730, -77.83593853670399199, -0.8254132364208000006 ) ) ;
#32983 = CARTESIAN_POINT ( 'NONE',  ( 1.431241028886999889, -81.53685813303999907, -0.8524881072380000591 ) ) ;
#32984 = DIRECTION ( 'NONE',  ( -0.7071067811865475727, 0.000000000000000000, -0.7071067811865475727 ) ) ;
#32985 = CARTESIAN_POINT ( 'NONE',  ( 10.74305781343810295, -81.00000000000002842, -2.396161594354234481 ) ) ;
#32986 = VERTEX_POINT ( 'NONE', #19527 ) ;
#32987 = DIRECTION ( 'NONE',  ( -1.000000000000000000, 0.000000000000000000, 0.000000000000000000 ) ) ;
#32988 = VECTOR ( 'NONE', #33001, 999.9999999999998863 ) ;
#32989 = CARTESIAN_POINT ( 'NONE',  ( 8.828526701892000617, -80.39498278894200212, -6.997593314318000246 ) ) ;
#32990 = EDGE_CURVE ( 'NONE', #46203, #9574, #13681, .T. ) ;
#32991 = CARTESIAN_POINT ( 'NONE',  ( 2.981707138340699004, -78.99744281236651489, -2.266066515766057332 ) ) ;
#32992 = ORIENTED_EDGE ( 'NONE', *, *, #1306, .F. ) ;
#32993 = CARTESIAN_POINT ( 'NONE',  ( -1.320128238786999919, -78.64567321947700407, -0.1893081677438999966 ) ) ;
#32994 = CARTESIAN_POINT ( 'NONE',  ( -8.959657150203256037, -77.52237568801258760, -2.594892310216006859 ) ) ;
#32995 = DIRECTION ( 'NONE',  ( -1.000000000000000000, 0.000000000000000000, 0.000000000000000000 ) ) ;
#32996 = ORIENTED_EDGE ( 'NONE', *, *, #40173, .F. ) ;
#32997 = CARTESIAN_POINT ( 'NONE',  ( 5.622631719431000263, -79.09562780968799700, 10.78740717875000144 ) ) ;
#32998 = CARTESIAN_POINT ( 'NONE',  ( -1.559871468835000163, -77.23492311450797843, -11.32549190513999982 ) ) ;
#32999 = CARTESIAN_POINT ( 'NONE',  ( -1.799501877760999902, -18.71082434677000350, 12.60552522436000089 ) ) ;
#33000 = EDGE_LOOP ( 'NONE', ( #58127, #45380, #34165 ) ) ;
#33001 = DIRECTION ( 'NONE',  ( 0.5000000000000744960, -0.7071067811864422126, 0.5000000000000744960 ) ) ;
#33002 = EDGE_CURVE ( 'NONE', #19, #47968, #10891, .T. ) ;
#33003 = CARTESIAN_POINT ( 'NONE',  ( -10.48543666025111420, -79.75833333333331154, 6.043427764450754580 ) ) ;
#33004 = CARTESIAN_POINT ( 'NONE',  ( 3.269429986698999979, -79.73829300546499610, 9.203886808668999109 ) ) ;
#33005 = ORIENTED_EDGE ( 'NONE', *, *, #3630, .T. ) ;
#33006 = CARTESIAN_POINT ( 'NONE',  ( -0.6644248411249000785, -76.24408568656099305, -12.21661133770999896 ) ) ;
#33007 = CARTESIAN_POINT ( 'NONE',  ( -4.799999999787999627, -74.99999999978798826, -2.226280155659000170E-09 ) ) ;
#33008 = CIRCLE ( 'NONE', #45307, 4.100000000000000533 ) ;
#33009 = ORIENTED_EDGE ( 'NONE', *, *, #48848, .T. ) ;
#33010 = CARTESIAN_POINT ( 'NONE',  ( -12.82230166703000052, -23.42260938006999993, -2.065916748305000272 ) ) ;
#33011 = CARTESIAN_POINT ( 'NONE',  ( -8.123853732960998997, -76.96654415034599594, 4.915330883505999893 ) ) ;
#33012 = CYLINDRICAL_SURFACE ( 'NONE', #55549, 1.750000000000000000 ) ;
#33013 = CARTESIAN_POINT ( 'NONE',  ( -0.6633660878114170378, -80.18071131022675502, -1.060558990980815297 ) ) ;
#33014 = CARTESIAN_POINT ( 'NONE',  ( -0.8898229088992634095, -16.97675468815732103, -12.70296869045118626 ) ) ;
#33015 = CARTESIAN_POINT ( 'NONE',  ( -10.64922275351036340, -76.72873637915004963, 2.917915514433102597 ) ) ;
#33016 = CARTESIAN_POINT ( 'NONE',  ( -12.70722357733599495, -17.58971352776233132, -1.610228312168085818 ) ) ;
#33017 = CARTESIAN_POINT ( 'NONE',  ( 1.060894005001709495, -78.53487121956678152, -1.113722360277955792 ) ) ;
#33018 = B_SPLINE_CURVE_WITH_KNOTS ( 'NONE', 3,
 ( #51760, #24589, #34871, #20740, #57327, #11887, #39317, #29865, #12168, #16890, #6577, #43763, #47919, #20167, #30154, #29578, #38739, #47339 ),
 .UNSPECIFIED., .F., .F.,
 ( 4, 2, 2, 2, 2, 2, 2, 2, 4 ),
 ( 0.000000000000000000, 0.1250000000000000278, 0.2500000000000000000, 0.3750000000000001110, 0.5000000000000001110, 0.6250000000000001110, 0.7500000000000002220, 0.8750000000000001110, 1.000000000000000000 ),
 .UNSPECIFIED. ) ;
#33019 = APPLICATION_CONTEXT ( 'automotive_design' ) ;
#33020 = CARTESIAN_POINT ( 'NONE',  ( 2.112424695814874909, -82.20729168471808634, -3.411783024464547953 ) ) ;
#33021 = CARTESIAN_POINT ( 'NONE',  ( 11.88049207238000093, -76.21158421993000331, -3.223263369271999856 ) ) ;
#33022 = CARTESIAN_POINT ( 'NONE',  ( -1.469401861277999988, -80.94206026912699770, -0.6692011555514000287 ) ) ;
#33023 = B_SPLINE_SURFACE_WITH_KNOTS ( 'NONE', 3, 3, ( 
 ( #11071, #47380, #6621, #19619 ),
 ( #20496, #50927, #28461, #47675 ),
 ( #24632, #51222, #1630, #46803 ),
 ( #6330, #7199, #24345, #6911 ),
 ( #24919, #52085, #20210, #42936 ),
 ( #2490, #38201, #56221, #15771 ),
 ( #33763, #38492, #51801, #56508 ),
 ( #34047, #52654, #7781, #3352 ),
 ( #34628, #25488, #44366, #39364 ),
 ( #8645, #48805, #35487, #21349 ),
 ( #26348, #3918, #25780, #39068 ),
 ( #3069, #7491, #16356, #21921 ),
 ( #53517, #26630, #49094, #44086 ),
 ( #43807, #39929, #39644, #12209 ),
 ( #57371, #16930, #30196, #57945 ),
 ( #11926, #57651, #34911, #30491 ),
 ( #8350, #17499, #56797, #48244 ) ),
 .UNSPECIFIED., .F., .F., .F.,
 ( 4, 1, 1, 1, 1, 1, 1, 1, 1, 1, 1, 1, 1, 1, 4 ),
 ( 4, 4 ),
 ( -0.01011398171657000057, 0.000000000000000000, 0.08333333333333001192, 0.1666666666667000196, 0.2500000000000000000, 0.3333333333333000081, 0.4166666666666999919, 0.5000000000000000000, 0.5833333333333000637, 0.6666666666667000474, 0.7500000000000000000, 0.8333333333333000637, 0.9166666666667000474, 1.000000000000000000, 1.010365777941000021 ),
 ( -0.3559705546970000078, 1.357612346708999995 ),
 .UNSPECIFIED. ) ;
#33024 = AXIS2_PLACEMENT_3D ( 'NONE', #4290, #54758, #35867 ) ;
#33025 = CARTESIAN_POINT ( 'NONE',  ( 0.000000000000000000, -80.35000000001998899, 0.000000000000000000 ) ) ;
#33026 = CARTESIAN_POINT ( 'NONE',  ( 7.765022563386000165, -60.89093562068000409, -9.830785949133000301 ) ) ;
#33027 = CARTESIAN_POINT ( 'NONE',  ( -9.042566447131001439, -79.11102013304999048, -8.284387575507999202 ) ) ;
#33028 = CARTESIAN_POINT ( 'NONE',  ( 11.61133755414000035, -76.84250581942099245, 3.999933378912999604 ) ) ;
#33029 = CARTESIAN_POINT ( 'NONE',  ( -3.451066577810062874, -1.829698698065413964, -0.5702761658243397092 ) ) ;
#33030 = CARTESIAN_POINT ( 'NONE',  ( 3.034193154433733941, -2.821981570262439565, -1.163058261055952558 ) ) ;
#33031 = CARTESIAN_POINT ( 'NONE',  ( 11.22958103806566932, -78.26998077374973661, -4.439356378266488434 ) ) ;
#33032 = CARTESIAN_POINT ( 'NONE',  ( 8.645668071321999548, -78.55496783972452590, 7.146365085715999044 ) ) ;
#33033 = VERTEX_POINT ( 'NONE', #1249 ) ;
#33034 = CARTESIAN_POINT ( 'NONE',  ( 0.5930780265196999856, -82.35881715536000058, 1.214178601635999888 ) ) ;
#33035 = CARTESIAN_POINT ( 'NONE',  ( -7.220923959705244144, -77.87291666666665435, -9.396085398178621872 ) ) ;
#33036 = LINE ( 'NONE', #14458, #37035 ) ;
#33037 = CARTESIAN_POINT ( 'NONE',  ( -0.7681833999686477066, -78.92708333333332860, 0.9995835529977223910 ) ) ;
#33038 = CARTESIAN_POINT ( 'NONE',  ( -3.532530677088999926, -1.827872856414999969, -1.580970727500000006 ) ) ;
#33039 = CARTESIAN_POINT ( 'NONE',  ( -12.03258451680999919, -78.00461903155100174, 0.6424029262030001020 ) ) ;
#33040 = CARTESIAN_POINT ( 'NONE',  ( 6.930806504809000401, -78.39586191736599119, -6.687086896242999678 ) ) ;
#33042 = CARTESIAN_POINT ( 'NONE',  ( 7.545211986414574135, -77.01380208334457222, 5.799587084941282278 ) ) ;
#33041 = CARTESIAN_POINT ( 'NONE',  ( -8.251448334410120822, -76.13695544466607146, 8.365207622121904052 ) ) ;
#33043 = CARTESIAN_POINT ( 'NONE',  ( -10.06651861793999991, -78.99497611018699672, 4.223809761943999597 ) ) ;
#33044 = CARTESIAN_POINT ( 'NONE',  ( 3.274617103212182911, -85.88547957940600952, 2.378452838117370405 ) ) ;
#33045 = ORIENTED_EDGE ( 'NONE', *, *, #29377, .T. ) ;
#33046 = CARTESIAN_POINT ( 'NONE',  ( 12.70259419118077915, -24.73882758529050463, 1.314635108442414602 ) ) ;
#33047 = CARTESIAN_POINT ( 'NONE',  ( -11.11223348184000059, -79.79208530464400440, -4.928830210637000775 ) ) ;
#33048 = CARTESIAN_POINT ( 'NONE',  ( 0.000000000000000000, 4.040000000000000036, 0.000000000000000000 ) ) ;
#33049 = CIRCLE ( 'NONE', #30226, 10.14999999999999858 ) ;
#33050 = DIRECTION ( 'NONE',  ( 0.000000000000000000, -1.000000000000000000, 0.000000000000000000 ) ) ;
#33051 = CARTESIAN_POINT ( 'NONE',  ( 7.218984044805000444, -79.30833362310698931, 8.267423174273998754 ) ) ;
#33052 = CARTESIAN_POINT ( 'NONE',  ( -10.81039872835957816, -80.08464542082350590, 2.129203739267044426 ) ) ;
#33053 = CARTESIAN_POINT ( 'NONE',  ( 9.559470275639000647, -79.32991171449499745, 0.08713422356856999340 ) ) ;
#33054 = CARTESIAN_POINT ( 'NONE',  ( 9.992014434680999813, -17.83915351714000153, -7.762970980311999725 ) ) ;
#33055 = DIRECTION ( 'NONE',  ( 0.7071067811865470176, -0.7071067811865470176, 3.680441518142245308E-08 ) ) ;
#33056 = ORIENTED_EDGE ( 'NONE', *, *, #429, .T. ) ;
#33057 = FACE_OUTER_BOUND ( 'NONE', #7022, .T. ) ;
#33058 = CARTESIAN_POINT ( 'NONE',  ( -11.55240038170842709, -79.56519809028500845, -2.255166230233432323 ) ) ;
#33059 = CARTESIAN_POINT ( 'NONE',  ( -0.03211073419994320277, -78.62148120184446043, 3.406944226116074503 ) ) ;
#33060 = EDGE_CURVE ( 'NONE', #8180, #29038, #453, .T. ) ;
#33061 = CARTESIAN_POINT ( 'NONE',  ( 5.457687247930513408, -77.79051310338437020, 10.71434849429115310 ) ) ;
#33063 = DIRECTION ( 'NONE',  ( 1.000000000000000000, 0.000000000000000000, 0.000000000000000000 ) ) ;
#33062 = CARTESIAN_POINT ( 'NONE',  ( 12.50000000000000000, -17.31640971966000109, -1.003652782652999953 ) ) ;
#33064 = CARTESIAN_POINT ( 'NONE',  ( -4.152657972338684722, -79.44472964675378535, -10.42003074508492233 ) ) ;
#33065 = AXIS2_PLACEMENT_3D ( 'NONE', #3394, #48845, #52411 ) ;
#33066 = LINE ( 'NONE', #659, #41133 ) ;
#33067 = FACE_OUTER_BOUND ( 'NONE', #49286, .T. ) ;
#33068 = AXIS2_PLACEMENT_3D ( 'NONE', #41528, #45982, #14360 ) ;
#33069 = CARTESIAN_POINT ( 'NONE',  ( -0.06195931011014999684, -78.70125392059999569, -1.306500503017999915 ) ) ;
#33070 = CARTESIAN_POINT ( 'NONE',  ( 10.06780253793347413, -76.09155368262285890, -4.475612946776665879 ) ) ;
#33071 = CARTESIAN_POINT ( 'NONE',  ( -1.297546493877329565, -78.56567216818805832, -10.89881608063975804 ) ) ;
#33072 = EDGE_CURVE ( 'NONE', #16168, #30569, #42860, .T. ) ;
#33073 = CARTESIAN_POINT ( 'NONE',  ( -12.50728630775810402, -61.79975539279641339, 0.1757873579563377919 ) ) ;
#33074 = ORIENTED_EDGE ( 'NONE', *, *, #14932, .F. ) ;
#33075 = ORIENTED_EDGE ( 'NONE', *, *, #53719, .F. ) ;
#33076 = FACE_OUTER_BOUND ( 'NONE', #32068, .T. ) ;
#33077 = CARTESIAN_POINT ( 'NONE',  ( 7.286211459007912339, -78.78428004322132949, -7.904517777456380401 ) ) ;
#33078 = ORIENTED_EDGE ( 'NONE', *, *, #25555, .F. ) ;
#33079 = CARTESIAN_POINT ( 'NONE',  ( 7.762982794245000484, -17.83910040287999621, 9.991998894192999359 ) ) ;
#33080 = FACE_OUTER_BOUND ( 'NONE', #47605, .T. ) ;
#33081 = EDGE_CURVE ( 'NONE', #19448, #52807, #18947, .T. ) ;
#33082 = CARTESIAN_POINT ( 'NONE',  ( -11.75618103724999841, -78.25732521500999894, -1.929672871034000092 ) ) ;
#33083 = CARTESIAN_POINT ( 'NONE',  ( 9.310177428715999071, -61.93531023604000296, 8.596745825462999591 ) ) ;
#33084 = CARTESIAN_POINT ( 'NONE',  ( 0.000000000000000000, -86.39999999999999147, 0.000000000000000000 ) ) ;
#33085 = CARTESIAN_POINT ( 'NONE',  ( 11.36836877616901731, -77.77436589406271139, -3.778912901489055898 ) ) ;
#33086 = CARTESIAN_POINT ( 'NONE',  ( 4.653115705712000505, -78.99293419121799786, -10.20620521156999949 ) ) ;
#33087 = EDGE_CURVE ( 'NONE', #10113, #25256, #2328, .T. ) ;
#33088 = EDGE_LOOP ( 'NONE', ( #43916, #38897, #8618, #10226 ) ) ;
#33089 = CARTESIAN_POINT ( 'NONE',  ( -10.25201842917796924, -24.12180395215443696, 7.730408553586223697 ) ) ;
#33090 = PRESENTATION_LAYER_ASSIGNMENT (  '', '', ( #12365 ) ) ;
#33091 = VERTEX_POINT ( 'NONE', #2400 ) ;
#33092 = CARTESIAN_POINT ( 'NONE',  ( 7.482597622593881503, -77.40011871758873951, 5.438000268058704734 ) ) ;
#33093 = CARTESIAN_POINT ( 'NONE',  ( -10.84202097104999929, -77.47535685249599169, 2.082001701158999740 ) ) ;
#33094 = CARTESIAN_POINT ( 'NONE',  ( 0.000000000000000000, -6.100000000000000533, -13.99999999999798383 ) ) ;
#33095 = CARTESIAN_POINT ( 'NONE',  ( -0.7259747304966001069, -78.40405146749098719, 1.442281046339000117 ) ) ;
#33096 = CARTESIAN_POINT ( 'NONE',  ( -9.713030931998421380, -17.47705886690323140, -7.970419576809637974 ) ) ;
#33097 = CARTESIAN_POINT ( 'NONE',  ( -1.316790939146709416, -2.092021354265999999, -2.998527993510658352 ) ) ;
#33098 = CARTESIAN_POINT ( 'NONE',  ( 1.153380192234999990, -78.64192926678998674, 1.148206073167999941 ) ) ;
#33099 = B_SPLINE_CURVE_WITH_KNOTS ( 'NONE', 3,
 ( #28260, #1439, #54576, #9695 ),
 .UNSPECIFIED., .F., .F.,
 ( 4, 4 ),
 ( 0.000000000000000000, 1.000000000000000000 ),
 .UNSPECIFIED. ) ;
#33100 = CARTESIAN_POINT ( 'NONE',  ( 8.267239500339000458, -78.18724719090198505, -6.983083964283999912 ) ) ;
#33101 = CARTESIAN_POINT ( 'NONE',  ( -8.284635637485001425, -25.04861451557999885, -9.778492910169999774 ) ) ;
#33102 = CARTESIAN_POINT ( 'NONE',  ( 12.60413670423000099, -60.10716680829000325, -1.799502287691000069 ) ) ;
#33103 = CARTESIAN_POINT ( 'NONE',  ( -2.902137050060999979, -86.06631758453399073, 2.039322401418999675 ) ) ;
#33104 = EDGE_LOOP ( 'NONE', ( #19631, #4491, #12031, #22792 ) ) ;
#33105 = CARTESIAN_POINT ( 'NONE',  ( -10.39360022642970804, -77.19999999999998863, 3.478205997298121854 ) ) ;
#33106 = CIRCLE ( 'NONE', #14232, 30.49999999999999289 ) ;
#33107 = CARTESIAN_POINT ( 'NONE',  ( -0.5042965048037999498, -80.79409703377000085, 1.503356827960000031 ) ) ;
#33108 = CARTESIAN_POINT ( 'NONE',  ( 4.744749809752532244, -77.93878674868346934, 9.646253385772624256 ) ) ;
#33109 = CARTESIAN_POINT ( 'NONE',  ( 10.18066396183999878, -78.36028369236800017, 6.314281093748000728 ) ) ;
#33110 = EDGE_CURVE ( 'NONE', #237, #58179, #56705, .T. ) ;
#33111 = CARTESIAN_POINT ( 'NONE',  ( -9.029856014872001069, -16.66737842935999936, 9.038878718683999836 ) ) ;
#33112 = VECTOR ( 'NONE', #34305, 1000.000000000000000 ) ;
#33113 = CARTESIAN_POINT ( 'NONE',  ( 1.407073214895890878, -78.96473917796927822, 10.74996459197358689 ) ) ;
#33114 = CARTESIAN_POINT ( 'NONE',  ( -0.3640064567607090296, -2.866730428114151685, -3.502711746507367163 ) ) ;
#33115 = CARTESIAN_POINT ( 'NONE',  ( 10.10817968731031513, -80.87791439531011406, 3.669898630734008904 ) ) ;
#33116 = CARTESIAN_POINT ( 'NONE',  ( -9.338489578732000140, -78.06914363189699202, 1.184823571421999899 ) ) ;
#33117 = CARTESIAN_POINT ( 'NONE',  ( 0.3781279528989071603, -85.80681307243297340, -8.440634685827930639 ) ) ;
#33118 = CARTESIAN_POINT ( 'NONE',  ( 11.01479880718999915, -78.20443840457200224, -0.6131407820818999266 ) ) ;
#33119 = CARTESIAN_POINT ( 'NONE',  ( -3.164411967817999827, -77.25425841958221440, -11.86639179494000018 ) ) ;
#33120 = CARTESIAN_POINT ( 'NONE',  ( -10.48974755655999935, -80.54876778545759919, -3.001463441570999979 ) ) ;
#33121 = ORIENTED_EDGE ( 'NONE', *, *, #28961, .T. ) ;
#33122 = CARTESIAN_POINT ( 'NONE',  ( -0.2317941695893000198, -82.33204462758500597, -1.228320586388000013 ) ) ;
#33123 = CARTESIAN_POINT ( 'NONE',  ( -3.047436688878264466, -77.09406694292110274, 11.37773063511170157 ) ) ;
#33124 = CARTESIAN_POINT ( 'NONE',  ( 1.698401934075999931, -61.02014045872000025, -12.66748707616000047 ) ) ;
#33125 = CARTESIAN_POINT ( 'NONE',  ( -8.190859204290999784, -55.64999999967000122, 7.342331066867000544 ) ) ;
#33126 = CARTESIAN_POINT ( 'NONE',  ( 7.155101792066000499, -78.51525063703199692, -8.354909834651998324 ) ) ;
#33127 = CARTESIAN_POINT ( 'NONE',  ( -3.673218652927999539, -79.21170190909299436, 10.34270183798999909 ) ) ;
#33128 = CARTESIAN_POINT ( 'NONE',  ( -12.80088938719999803, -19.23743348210000192, 1.980532758767000301 ) ) ;
#33129 = CARTESIAN_POINT ( 'NONE',  ( 1.285423637123966012, -84.24999999971510078, 3.956127134342454887 ) ) ;
#33130 = CARTESIAN_POINT ( 'NONE',  ( 6.632299823822999763, -77.18051343188000146, -9.958931470938999553 ) ) ;
#33131 = CARTESIAN_POINT ( 'NONE',  ( -10.20679554288753010, -54.56427274255051429, -7.770327721632001250 ) ) ;
#33132 = CARTESIAN_POINT ( 'NONE',  ( -1.732798278134000114, -82.90842953870898668, 3.795253925594999966 ) ) ;
#33133 = CARTESIAN_POINT ( 'NONE',  ( -7.624341766639000539, -23.26485146254000114, -10.42531125024000005 ) ) ;
#33134 = CARTESIAN_POINT ( 'NONE',  ( 7.647094085174999556, -55.43104695408000282, -10.00844048069000003 ) ) ;
#33135 = CARTESIAN_POINT ( 'NONE',  ( -11.00476719864000152, -77.25954786493399240, 2.393546210564999832 ) ) ;
#33136 = CARTESIAN_POINT ( 'NONE',  ( -0.4240539849974000464, -80.22508981920998394, 1.611036072322000079 ) ) ;
#33137 = CARTESIAN_POINT ( 'NONE',  ( 1.429610420046000252, -78.71329787945998646, 0.1195568986375999954 ) ) ;
#33138 = CARTESIAN_POINT ( 'NONE',  ( -1.570796326794938524, -77.68541666666666856, 11.99999999999999645 ) ) ;
#33139 = DIRECTION ( 'NONE',  ( 1.000000000000000000, 0.000000000000000000, 0.000000000000000000 ) ) ;
#33140 = LINE ( 'NONE', #41142, #48769 ) ;
#33141 = ORIENTED_EDGE ( 'NONE', *, *, #9213, .T. ) ;
#33142 = CARTESIAN_POINT ( 'NONE',  ( 1.033908640164241222, -79.80255683383327892, -0.7040647445706786911 ) ) ;
#33143 = DIRECTION ( 'NONE',  ( -0.7071067811864980568, -1.534448722697995070E-11, -0.7071067811865969777 ) ) ;
#33144 = ORIENTED_EDGE ( 'NONE', *, *, #31001, .T. ) ;
#33145 = CARTESIAN_POINT ( 'NONE',  ( -0.8722640199205535794, -81.66406706422890238, -0.8949065950927366231 ) ) ;
#33146 = ADVANCED_FACE ( 'NONE', ( #12114 ), #29241, .F. ) ;
#33147 = CARTESIAN_POINT ( 'NONE',  ( -1.463640999337999959, -78.50544952233700258, -10.83301059047000159 ) ) ;
#33148 = DIRECTION ( 'NONE',  ( 0.000000000000000000, -1.000000000000000000, 0.000000000000000000 ) ) ;
#33149 = VERTEX_POINT ( 'NONE', #25395 ) ;
#33150 = ORIENTED_EDGE ( 'NONE', *, *, #11446, .F. ) ;
#33151 = CARTESIAN_POINT ( 'NONE',  ( 1.465624405047999845, -80.81793094364199703, 0.3884420286245000575 ) ) ;
#33152 = VERTEX_POINT ( 'NONE', #38107 ) ;
#33153 = DIRECTION ( 'NONE',  ( 0.000000000000000000, 1.000000000000000000, 0.000000000000000000 ) ) ;
#33154 = VERTEX_POINT ( 'NONE', #38974 ) ;
#33155 = AXIS2_PLACEMENT_3D ( 'NONE', #14412, #10008, #40711 ) ;
#33156 = CARTESIAN_POINT ( 'NONE',  ( 1.056237665594999875, -16.95133986302000295, 12.77256098197999989 ) ) ;
#33157 = CYLINDRICAL_SURFACE ( 'NONE', #21617, 9.250000000000000000 ) ;
#33158 = APPLICATION_PROTOCOL_DEFINITION ( 'draft international standard', 'automotive_design', 1998, #28888 ) ;
#33159 = CARTESIAN_POINT ( 'NONE',  ( 2.964513727003363019, -82.32291664973151057, -1.751382667063024590 ) ) ;
#33160 = CARTESIAN_POINT ( 'NONE',  ( 6.321504634335313177, -78.28489978996086052, -6.754501521448134760 ) ) ;
#33161 = DIRECTION ( 'NONE',  ( -1.674928520677000026E-10, 1.000000000000000000, 2.004066721390000047E-09 ) ) ;
#33162 = ADVANCED_FACE ( 'NONE', ( #20401 ), #7681, .F. ) ;
#33163 = VERTEX_POINT ( 'NONE', #56417 ) ;
#33164 = VERTEX_POINT ( 'NONE', #3264 ) ;
#33165 = LINE ( 'NONE', #15472, #7515 ) ;
#33166 = CARTESIAN_POINT ( 'NONE',  ( 8.343860018000999190, -55.64999999967000122, -8.343860018000999190 ) ) ;
#33167 = CARTESIAN_POINT ( 'NONE',  ( -0.9995835529977281642, -81.44791666666662877, 0.7681833999686391579 ) ) ;
#33168 = CARTESIAN_POINT ( 'NONE',  ( -1.208267226910347603, -61.62590682120529806, -12.70228502427989881 ) ) ;
#33169 = CARTESIAN_POINT ( 'NONE',  ( 4.746041175454999816, -77.43551473549599962, -8.464384343845999581 ) ) ;
#33170 = DIRECTION ( 'NONE',  ( 0.000000000000000000, 1.000000000000000000, 0.000000000000000000 ) ) ;
#33171 = CARTESIAN_POINT ( 'NONE',  ( -0.4631402796970099933, -85.97511617271671014, 3.956885520969557479 ) ) ;
#33172 = CARTESIAN_POINT ( 'NONE',  ( 1.924380748938630393E-07, -79.75000000000001421, -9.249538042332323684 ) ) ;
#33173 = CARTESIAN_POINT ( 'NONE',  ( 0.6904535216592000424, -79.91234740900999611, 1.161570125514999940 ) ) ;
#33174 = CARTESIAN_POINT ( 'NONE',  ( 0.6553672983243258310, -77.18037193750340919, -9.424189266312801294 ) ) ;
#33175 = CARTESIAN_POINT ( 'NONE',  ( 9.708203932502000200, -79.25000000000000000, -7.053423027506000587 ) ) ;
#33176 = CARTESIAN_POINT ( 'NONE',  ( -0.2201363562291999698, -79.36327907013999550, -1.483758735329000045 ) ) ;
#33177 = CARTESIAN_POINT ( 'NONE',  ( -5.743104117080999771, -78.99616001420199041, 7.801152530868000312 ) ) ;
#33178 = CARTESIAN_POINT ( 'NONE',  ( -10.77593383617251277, -80.24166666668229198, -2.296997422106781706 ) ) ;
#33179 = EDGE_CURVE ( 'NONE', #48919, #54320, #11260, .T. ) ;
#33180 = LINE ( 'NONE', #25206, #20275 ) ;
#33182 = CARTESIAN_POINT ( 'NONE',  ( -0.006333666751268000016, -16.66737355700000123, -12.77652491955999992 ) ) ;
#33181 = LINE ( 'NONE', #6628, #23092 ) ;
#33183 = CARTESIAN_POINT ( 'NONE',  ( -9.248871138250700952, -79.58998423164975122, 1.210936878181855691 ) ) ;
#33184 = CARTESIAN_POINT ( 'NONE',  ( 0.000000000000000000, -80.49999999999998579, 0.000000000000000000 ) ) ;
#33185 = LINE ( 'NONE', #20786, #2594 ) ;
#33186 = CARTESIAN_POINT ( 'NONE',  ( 2.444312764923342485, -1.435907104546281898, -2.543885789726834545 ) ) ;
#33187 = CARTESIAN_POINT ( 'NONE',  ( -9.611650271896834852, -78.24166666666666003, -5.539808784079895965 ) ) ;
#33188 = CARTESIAN_POINT ( 'NONE',  ( -0.5999663639301134888, -18.81035107904876469, -10.98362601162690844 ) ) ;
#33189 = CARTESIAN_POINT ( 'NONE',  ( 7.216788504278100369, -77.52047868913132334, 9.394654730084591066 ) ) ;
#33190 = CARTESIAN_POINT ( 'NONE',  ( -4.628649168153988747, -77.18975860091060781, -8.076984658556984442 ) ) ;
#33191 = CARTESIAN_POINT ( 'NONE',  ( -3.507257632973999950, -79.86191712038298363, 8.865074537405000399 ) ) ;
#33192 = AXIS2_PLACEMENT_3D ( 'NONE', #27580, #33170, #1332 ) ;
#33193 = CARTESIAN_POINT ( 'NONE',  ( 12.50679926050277047, -17.69581646371715422, -1.424414840275272542 ) ) ;
#33194 = CARTESIAN_POINT ( 'NONE',  ( 0.6195125560301592005, -79.47047398390786555, 10.74289813788460002 ) ) ;
#33195 = EDGE_CURVE ( 'NONE', #38791, #47867, #12663, .T. ) ;
#33196 = LINE ( 'NONE', #15502, #15003 ) ;
#33197 = CARTESIAN_POINT ( 'NONE',  ( 0.000000000000000000, -76.75499999999999545, 0.000000000000000000 ) ) ;
#33198 = VECTOR ( 'NONE', #24827, 1000.000000000000114 ) ;
#33199 = CARTESIAN_POINT ( 'NONE',  ( 11.17006500217999942, -77.44000681347299064, 1.528262659639999965 ) ) ;
#33200 = CARTESIAN_POINT ( 'NONE',  ( -1.600123231380999878, -81.40245127004399706, 0.1129161299330000007 ) ) ;
#33201 = CARTESIAN_POINT ( 'NONE',  ( -0.1437401157479178682, -81.98469811677230723, 1.242173127013889378 ) ) ;
#33202 = DIRECTION ( 'NONE',  ( 0.000000000000000000, 0.000000000000000000, -1.000000000000000000 ) ) ;
#33204 = CARTESIAN_POINT ( 'NONE',  ( -12.90000000000000036, -3.000000000000000000, 0.000000000000000000 ) ) ;
#33203 = CARTESIAN_POINT ( 'NONE',  ( 3.126063113129000204, -82.02128429901999596, -1.787420609967999896 ) ) ;
#33205 = CARTESIAN_POINT ( 'NONE',  ( 8.150225256662000817, -79.90095584965399667, -4.374508917085999649 ) ) ;
#33206 = CARTESIAN_POINT ( 'NONE',  ( -3.500000000146000101, -0.7499999998540000101, 2.054632350152999929E-08 ) ) ;
#33207 = CARTESIAN_POINT ( 'NONE',  ( 1.500000000000000000, -81.26041666666668561, 0.1963495408493652339 ) ) ;
#33208 = CARTESIAN_POINT ( 'NONE',  ( -1.750000000000000000, -55.55000000209000177, 12.50000000000000000 ) ) ;
#33209 = CARTESIAN_POINT ( 'NONE',  ( -7.954951288349001004, -18.75000000000000000, -9.722718241315000398 ) ) ;
#33210 = AXIS2_PLACEMENT_3D ( 'NONE', #3809, #4400, #17096 ) ;
#33211 = EDGE_LOOP ( 'NONE', ( #23264, #45905, #1553, #23801 ) ) ;
#33212 = EDGE_LOOP ( 'NONE', ( #12491, #42679, #54525, #50198 ) ) ;
#33213 = CIRCLE ( 'NONE', #32281, 3.799999999999999822 ) ;
#33214 = CARTESIAN_POINT ( 'NONE',  ( -10.65106809510000119, -79.16321472370599110, 5.591232889670999739 ) ) ;
#33215 = ADVANCED_FACE ( 'NONE', ( #39261 ), #57274, .F. ) ;
#33216 = CARTESIAN_POINT ( 'NONE',  ( 0.000000000000000000, -76.00000000000000000, 0.000000000000000000 ) ) ;
#33217 = FACE_OUTER_BOUND ( 'NONE', #49150, .T. ) ;
#33218 = ORIENTED_EDGE ( 'NONE', *, *, #33569, .F. ) ;
#33219 = EDGE_CURVE ( 'NONE', #52418, #29475, #20234, .T. ) ;
#33220 = CARTESIAN_POINT ( 'NONE',  ( 2.220279159302000149, -77.98351832560599917, 11.72628939184999908 ) ) ;
#33221 = ORIENTED_EDGE ( 'NONE', *, *, #1068, .T. ) ;
#33222 = VERTEX_POINT ( 'NONE', #29527 ) ;
#33223 = CARTESIAN_POINT ( 'NONE',  ( 8.190859204290999784, -59.94999999967000548, 7.342331066867000544 ) ) ;
#33224 = ORIENTED_EDGE ( 'NONE', *, *, #54901, .F. ) ;
#33225 = CARTESIAN_POINT ( 'NONE',  ( 0.4738570603385999780, -79.09443340893348307, -3.515258366932000111 ) ) ;
#33226 = CARTESIAN_POINT ( 'NONE',  ( 4.403238962115728405, -79.23630107778137699, 8.417739988564747478 ) ) ;
#33227 = ORIENTED_EDGE ( 'NONE', *, *, #27610, .F. ) ;
#33229 = EDGE_CURVE ( 'NONE', #32066, #3688, #7109, .T. ) ;
#33228 = CARTESIAN_POINT ( 'NONE',  ( 0.03738295792059419254, -82.72804728612686631, -1.249190724913706640 ) ) ;
#33230 = VERTEX_POINT ( 'NONE', #30099 ) ;
#33231 = CARTESIAN_POINT ( 'NONE',  ( 1.767510878348000247, -2.887137290291999836, 2.906076978666999988 ) ) ;
#33232 = EDGE_LOOP ( 'NONE', ( #49201, #44571, #43332, #55602, #28552, #12120 ) ) ;
#33233 = CARTESIAN_POINT ( 'NONE',  ( -1.210723843908615871, -79.21478203666787010, -9.248604757515597186 ) ) ;
#33234 = CARTESIAN_POINT ( 'NONE',  ( -0.6025044293664234551, -78.84232437041447383, -1.382994520336419342 ) ) ;
#33235 = AXIS2_PLACEMENT_3D ( 'NONE', #13199, #53076, #43934 ) ;
#33236 = CARTESIAN_POINT ( 'NONE',  ( -4.331976239377192783, -79.80000000000002558, -11.03186125555349228 ) ) ;
#33237 = CARTESIAN_POINT ( 'NONE',  ( 1.250000000000000000, -82.74999999999998579, 0.000000000000000000 ) ) ;
#33238 = CARTESIAN_POINT ( 'NONE',  ( 1.021160424422173252, -0.9687499998052564454, 3.160415270357120221 ) ) ;
#33239 = CARTESIAN_POINT ( 'NONE',  ( 6.240531904507999883, -78.06941474361464373, 7.431451467605000083 ) ) ;
#33240 = CARTESIAN_POINT ( 'NONE',  ( 1.849737152796000039, -76.62788311584399992, 11.02961253862999946 ) ) ;
#33241 = CARTESIAN_POINT ( 'NONE',  ( -9.396085398178650294, -77.24791666666668277, 7.220923959705211281 ) ) ;
#33242 = AXIS2_PLACEMENT_3D ( 'NONE', #26755, #40046, #35612 ) ;
#33243 = CARTESIAN_POINT ( 'NONE',  ( 9.925898951148999672, -76.53469514392799056, -5.249786549701999760 ) ) ;
#33244 = CARTESIAN_POINT ( 'NONE',  ( -6.733423791686919735, -78.66015289143886946, -6.348039707728767134 ) ) ;
#33245 = CARTESIAN_POINT ( 'NONE',  ( 2.448098496330775919, -76.55784816645272883, 11.49200783961538797 ) ) ;
#33246 = B_SPLINE_CURVE_WITH_KNOTS ( 'NONE', 3,
 ( #19461, #56068, #15612, #10317, #55476, #33016, #46348, #42777, #28594, #2340, #5872, #23881, #20334, #16773, #34754, #11769 ),
 .UNSPECIFIED., .F., .F.,
 ( 4, 2, 2, 2, 2, 2, 2, 4 ),
 ( 0.000000000000000000, 0.2499999999999964473, 0.3749999999999946709, 0.4374999999999952816, 0.4999999999999958922, 0.6249999999999968914, 0.7499999999999978906, 1.000000000000000000 ),
 .UNSPECIFIED. ) ;
#33247 = CARTESIAN_POINT ( 'NONE',  ( -8.742972704348000335, -77.54048501420199102, 3.483847966513999861 ) ) ;
#33248 = DIRECTION ( 'NONE',  ( -0.9999999929803531362, 0.000000000000000000, -0.0001184875252605944247 ) ) ;
#33249 = CARTESIAN_POINT ( 'NONE',  ( 0.000000000000000000, -76.75499999999999545, 0.000000000000000000 ) ) ;
#33250 = CARTESIAN_POINT ( 'NONE',  ( -1.243547092045992564, -77.18541666666664014, 9.499999999999994671 ) ) ;
#33251 = CARTESIAN_POINT ( 'NONE',  ( 3.415553852041999683, -79.04278455456849883, -1.563762801788000090 ) ) ;
#33252 = DIRECTION ( 'NONE',  ( 0.000000000000000000, 0.7071067811866525998, -0.7071067811864425456 ) ) ;
#33253 = CIRCLE ( 'NONE', #7816, 3.249999999999999556 ) ;
#33254 = CARTESIAN_POINT ( 'NONE',  ( -9.936194076909385942, -78.06890473706415889, 4.102870334978085509 ) ) ;
#33255 = CARTESIAN_POINT ( 'NONE',  ( 0.2897521468641586773, -82.95649998723895635, 1.216791426940023513 ) ) ;
#33256 = CARTESIAN_POINT ( 'NONE',  ( 0.000000000000000000, -75.67500000000001137, 0.000000000000000000 ) ) ;
#33257 = CARTESIAN_POINT ( 'NONE',  ( -7.474083310498281563, -76.26977652102928573, -9.069810220831756808 ) ) ;
#33258 = CARTESIAN_POINT ( 'NONE',  ( 4.907702572637520078, -79.99999999999997158, 7.984394256099379916 ) ) ;
#33259 = CIRCLE ( 'NONE', #43687, 11.70000000000000107 ) ;
#33260 = CARTESIAN_POINT ( 'NONE',  ( -10.19019669288000074, -59.99643762534999780, -7.646965578510999784 ) ) ;
#33261 = DIRECTION ( 'NONE',  ( 0.000000000000000000, 0.000000000000000000, -1.000000000000000000 ) ) ;
#33262 = CARTESIAN_POINT ( 'NONE',  ( -1.297058042903999953, -81.15301887804400849, -0.3101879797029999941 ) ) ;
#33263 = CARTESIAN_POINT ( 'NONE',  ( 3.973905474789803716, -79.36013131668573806, -8.444981681530821405 ) ) ;
#33264 = CARTESIAN_POINT ( 'NONE',  ( 1.500000000000001110, -80.63958333333333428, -0.1963495408493590721 ) ) ;
#33265 = CARTESIAN_POINT ( 'NONE',  ( 12.43646124688000043, -24.91751819622000141, -0.05236837568997999848 ) ) ;
#33266 = ADVANCED_FACE ( 'NONE', ( #33673 ), #52276, .F. ) ;
#33267 = CARTESIAN_POINT ( 'NONE',  ( 5.663577320046584873, -77.78160512761387224, 9.213540343163701962 ) ) ;
#33268 = CARTESIAN_POINT ( 'NONE',  ( 9.981840466370998755, -78.63412405397946259, 4.563647388395000171 ) ) ;
#33269 = CARTESIAN_POINT ( 'NONE',  ( -1.705971691335000040, -75.78238836370000797, -12.09219208115999855 ) ) ;
#33270 = EDGE_LOOP ( 'NONE', ( #53285, #52422, #14064, #28433 ) ) ;
#33271 = CARTESIAN_POINT ( 'NONE',  ( 1.972823595576999933, -85.99771544543098400, 3.196770659314999818 ) ) ;
#33272 = CARTESIAN_POINT ( 'NONE',  ( 11.24487063635999995, -80.46590415106278726, 0.9974943187964001590 ) ) ;
#33274 = CARTESIAN_POINT ( 'NONE',  ( -4.842945234633629248, -76.29082827606781336, -10.70557031532286274 ) ) ;
#33273 = CARTESIAN_POINT ( 'NONE',  ( 8.342888411232321388, -78.31448426059630208, -3.994830225491370790 ) ) ;
#33275 = CARTESIAN_POINT ( 'NONE',  ( 12.43646124691999866, -61.71751819588999410, -0.05236837569004999804 ) ) ;
#33276 = CARTESIAN_POINT ( 'NONE',  ( 8.282307197233999219, -78.09278501627599667, -7.564489280985000619 ) ) ;
#33277 = DIRECTION ( 'NONE',  ( 1.000000000000000000, 0.000000000000000000, 0.000000000000000000 ) ) ;
#33278 = CARTESIAN_POINT ( 'NONE',  ( 2.878019135186999922, -77.97805768234898949, -9.304660206797001010 ) ) ;
#33279 = AXIS2_PLACEMENT_3D ( 'NONE', #7633, #15921, #55793 ) ;
#33280 = CARTESIAN_POINT ( 'NONE',  ( -1.510823314100999903, -83.40663862339900447, -0.3534059060544000319 ) ) ;
#33281 = CARTESIAN_POINT ( 'NONE',  ( 1.437851432728850520, -80.22213541715329654, -10.97786456746221084 ) ) ;
#33282 = CARTESIAN_POINT ( 'NONE',  ( -1.211530263941000163, -79.43446749155899056, 1.067430724879000037 ) ) ;
#33283 = ORIENTED_EDGE ( 'NONE', *, *, #51247, .T. ) ;
#33284 = DIRECTION ( 'NONE',  ( 0.000000000000000000, 0.000000000000000000, -1.000000000000000000 ) ) ;
#33285 = CARTESIAN_POINT ( 'NONE',  ( -10.58783149161999937, -80.72605733498191682, -3.847989116766000084 ) ) ;
#33286 = CARTESIAN_POINT ( 'NONE',  ( 2.589532191826647622, -78.97650882476808931, -2.803207326140070510 ) ) ;
#33287 = ORIENTED_EDGE ( 'NONE', *, *, #2589, .F. ) ;
#33288 = CARTESIAN_POINT ( 'NONE',  ( 0.5704417986824000808, -78.79451108962000205, -1.205475954488999912 ) ) ;
#33289 = CARTESIAN_POINT ( 'NONE',  ( -3.697742159549999741, -79.20909416798998848, 10.41175280961999938 ) ) ;
#33290 = CIRCLE ( 'NONE', #47492, 0.8000000000000011546 ) ;
#33291 = CARTESIAN_POINT ( 'NONE',  ( 12.49168433582000226, -60.09849137196000157, 1.667916687244999974 ) ) ;
#33292 = CARTESIAN_POINT ( 'NONE',  ( 10.80657406421999944, -79.95794665545098212, 4.085057409123999506 ) ) ;
#33293 = ORIENTED_EDGE ( 'NONE', *, *, #27149, .T. ) ;
#33294 = ADVANCED_FACE ( 'NONE', ( #47583 ), #11830, .F. ) ;
#33295 = CARTESIAN_POINT ( 'NONE',  ( -5.775534476593000122, -78.17323108527999409, 10.70634074252000012 ) ) ;
#33296 = CARTESIAN_POINT ( 'NONE',  ( 10.89779338388999896, -77.89524787048398480, 3.455448588212000072 ) ) ;
#33297 = CARTESIAN_POINT ( 'NONE',  ( 7.921549804313935184, -78.69040357935692498, -7.357602076918057676 ) ) ;
#33298 = ORIENTED_EDGE ( 'NONE', *, *, #40025, .F. ) ;
#33299 = ORIENTED_EDGE ( 'NONE', *, *, #43573, .F. ) ;
#33300 = CARTESIAN_POINT ( 'NONE',  ( 0.02072621771690125181, -80.47431364731653503, 1.249620385757917118 ) ) ;
#33301 = VECTOR ( 'NONE', #41138, 1000.000000000000000 ) ;
#33302 = CARTESIAN_POINT ( 'NONE',  ( -10.75000000000000000, -77.60000000000000853, 2.252154972635999871E-14 ) ) ;
#33303 = CARTESIAN_POINT ( 'NONE',  ( -5.726462542197000793, -80.08545445672149299, -7.912542777261000637 ) ) ;
#33304 = ORIENTED_EDGE ( 'NONE', *, *, #7844, .F. ) ;
#33306 = ADVANCED_FACE ( 'NONE', ( #2969 ), #34528, .F. ) ;
#33305 = CARTESIAN_POINT ( 'NONE',  ( 12.49830607526000037, -55.59028586401999661, 1.666977523254999927 ) ) ;
#33307 = CARTESIAN_POINT ( 'NONE',  ( -10.06651861793999991, -78.54179491694800674, 4.223809761943999597 ) ) ;
#33308 = ORIENTED_EDGE ( 'NONE', *, *, #35686, .F. ) ;
#33309 = CARTESIAN_POINT ( 'NONE',  ( -12.55486071735000131, -24.15393633008000407, -1.580832792524999864 ) ) ;
#33310 = EDGE_CURVE ( 'NONE', #3300, #3351, #28955, .T. ) ;
#33311 = CARTESIAN_POINT ( 'NONE',  ( -3.399395987256165430, -78.69999999999998863, 0.06408526995191232700 ) ) ;
#33312 = LINE ( 'NONE', #10608, #22556 ) ;
#33313 = CARTESIAN_POINT ( 'NONE',  ( -1.231052532977768843, -80.11508864318425083, -0.2330927567282044255 ) ) ;
#33314 = DIRECTION ( 'NONE',  ( -0.9999999924279686647, 0.000000000000000000, -0.0001230612157847738313 ) ) ;
#33315 = CARTESIAN_POINT ( 'NONE',  ( -9.603246065258371544, -79.06172913613842468, -1.533382312990622998 ) ) ;
#33316 = CARTESIAN_POINT ( 'NONE',  ( 13.86363625866555438, -46.43897132165000130, 0.001706075946107717383 ) ) ;
#33317 = CARTESIAN_POINT ( 'NONE',  ( 0.1356080529126781065, -78.48133048614386098, -1.532370771129643483 ) ) ;
#33318 = CARTESIAN_POINT ( 'NONE',  ( 3.461210433975990597, -80.81979166925117397, -2.107082871561129611 ) ) ;
#33319 = CARTESIAN_POINT ( 'NONE',  ( -3.151328970204000157, -76.08706565608000005, -11.89977497056000111 ) ) ;
#33320 = CARTESIAN_POINT ( 'NONE',  ( -1.419761472987663975, -2.442049273140185939, -3.284178234334656832 ) ) ;
#33321 = ADVANCED_FACE ( 'NONE', ( #46997, #38685, #47863, #7392 ), #43640, .T. ) ;
#33322 = CARTESIAN_POINT ( 'NONE',  ( 1.250000000000000000, -18.75000000000000000, -12.00000000000000000 ) ) ;
#33323 = CARTESIAN_POINT ( 'NONE',  ( 10.82405698390000026, -79.27161254432999726, 5.765268246940999930 ) ) ;
#33324 = CARTESIAN_POINT ( 'NONE',  ( 8.135116633385999663, -76.95127711100199974, 9.200136113044999675 ) ) ;
#33325 = B_SPLINE_CURVE_WITH_KNOTS ( 'NONE', 3,
 ( #6231, #45532, #45827, #5647, #19825, #14210, #36940, #46123, #679, #51128, #27782, #14503, #15088, #28364, #18662, #28662, #41961, #37520, #37229, #41669, #32787, #50540, #9504, #54951, #5940, #10094, #14792, #23073, #50834, #37816, #50248, #55538, #28073, #27491, #10380 ),
 .UNSPECIFIED., .F., .F.,
 ( 4, 1, 1, 1, 1, 1, 1, 1, 1, 1, 1, 1, 1, 1, 1, 1, 1, 1, 1, 1, 1, 1, 1, 1, 1, 1, 1, 1, 1, 1, 1, 1, 4 ),
 ( 0.000000000000000000, 0.01250201779797715899, 0.04500188491171358551, 0.07750175202545862840, 0.1100016191391893078, 0.1425014862529343229, 0.1750013533666937848, 0.2075012204804100591, 0.2400010875941263333, 0.2725009547078425798, 0.3050008218215588540, 0.3375006889354190132, 0.3700005560491352874, 0.4025004231628515616, 0.4350002902765678359, 0.4675001573902841101, 0.5000000245040003843, 0.5324998916178604880, 0.5649997587315768177, 0.5974996258452930364, 0.6299994929590093662, 0.6624993600727255849, 0.6949992271864419147, 0.7274990943001582444, 0.7599989614140183480, 0.7924988285277345668, 0.8249986956414508965, 0.8574985627551672263, 0.8899984298688834450, 0.9224982969825997747, 0.9549981640964599894, 0.9874980312101760971, 1.000000000000000000 ),
 .UNSPECIFIED. ) ;
#33326 = CARTESIAN_POINT ( 'NONE',  ( 8.300970689365442468, -78.69166666666666288, 4.784380313523563188 ) ) ;
#33327 = CARTESIAN_POINT ( 'NONE',  ( 2.800996926600495041, -2.807707601517177132, -1.662906485826789016 ) ) ;
#33328 = CARTESIAN_POINT ( 'NONE',  ( 12.01270605470693731, -77.80744209907201991, 1.121883719411586267 ) ) ;
#33329 = CARTESIAN_POINT ( 'NONE',  ( -12.49999990534960226, -13.07071424677999971, -0.001538265197309672755 ) ) ;
#33330 = CIRCLE ( 'NONE', #7882, 2.000000000000000000 ) ;
#33331 = B_SPLINE_SURFACE_WITH_KNOTS ( 'NONE', 3, 3, ( 
 ( #50722, #46592, #5822, #23254 ),
 ( #23829, #28243, #4957, #27954 ),
 ( #18832, #14099, #18542, #1424 ),
 ( #32967, #22963, #54558, #36824 ),
 ( #46296, #54839, #14382, #41846 ),
 ( #19413, #37403, #55424, #32382 ),
 ( #50426, #40583, #58296, #31408 ),
 ( #49747, #27279, #57703, #31106 ),
 ( #53279, #54163, #22269, #45315 ),
 ( #12825, #54461, #44419, #13997 ),
 ( #22864, #44719, #31995, #35248 ),
 ( #8401, #49451, #57998, #50036 ),
 ( #9583, #30825, #53575, #26983 ),
 ( #21973, #4273, #53876, #26398 ),
 ( #35546, #40285, #40873, #13705 ),
 ( #27567, #4865, #45611, #45017 ),
 ( #180, #4571, #31700, #22571 ) ),
 .UNSPECIFIED., .F., .F., .F.,
 ( 4, 1, 1, 1, 1, 1, 1, 1, 1, 1, 1, 1, 1, 1, 4 ),
 ( 4, 4 ),
 ( -0.01011408452870000106, 0.000000000000000000, 0.08333333333333001192, 0.1666666666667000196, 0.2500000000000000000, 0.3333333333333000081, 0.4166666666666999919, 0.5000000000000000000, 0.5833333333333000637, 0.6666666666667000474, 0.7500000000000000000, 0.8333333333333000637, 0.9166666666667000474, 1.000000000000000000, 1.010362559107000013 ),
 ( -0.3559705546267999954, 1.357612419602000076 ),
 .UNSPECIFIED. ) ;
#33332 = ORIENTED_EDGE ( 'NONE', *, *, #43702, .F. ) ;
#33333 = CARTESIAN_POINT ( 'NONE',  ( -1.115197308773999918, -81.55880043062998652, -0.5833774300368999022 ) ) ;
#33334 = CARTESIAN_POINT ( 'NONE',  ( 2.613075649634000186, -77.24612214791498843, 9.236390685206998796 ) ) ;
#33335 = DIRECTION ( 'NONE',  ( 0.000000000000000000, -1.000000000000000000, 0.000000000000000000 ) ) ;
#33336 = CARTESIAN_POINT ( 'NONE',  ( 0.3271848554490964789, -78.85416666666665719, 1.217465845835395521 ) ) ;
#33337 = CARTESIAN_POINT ( 'NONE',  ( -1.309998969828999993, -2.891902036004999843, -3.642009152241000081 ) ) ;
#33338 = EDGE_CURVE ( 'NONE', #43980, #54533, #25859, .T. ) ;
#33339 = VECTOR ( 'NONE', #49917, 1000.000000000000000 ) ;
#33340 = CARTESIAN_POINT ( 'NONE',  ( 11.95316821454999889, -78.24878287036499103, -1.522347302216999987 ) ) ;
#33341 = CARTESIAN_POINT ( 'NONE',  ( 8.475813183550998886, -78.06180405034399428, 4.797946079729999092 ) ) ;
#33343 = CARTESIAN_POINT ( 'NONE',  ( 8.250583882568891525, -77.00729166667787240, 4.756314485391412994 ) ) ;
#33342 = CARTESIAN_POINT ( 'NONE',  ( -9.525237058298714032, -76.14974714360452879, 6.880006712239788769 ) ) ;
#33344 = CARTESIAN_POINT ( 'NONE',  ( -9.475123589965999571, -79.48523028421899994, 5.421936826000999687 ) ) ;
#33345 = CARTESIAN_POINT ( 'NONE',  ( -10.54404894584495800, -79.58452146335964983, 2.093743504281901480 ) ) ;
#33346 = ORIENTED_EDGE ( 'NONE', *, *, #39681, .F. ) ;
#33347 = EDGE_CURVE ( 'NONE', #24905, #22759, #54152, .T. ) ;
#33348 = CARTESIAN_POINT ( 'NONE',  ( 0.7681833999686451531, -82.17708333333331439, -0.9995835529977240563 ) ) ;
#33349 = CARTESIAN_POINT ( 'NONE',  ( 3.399999999999980371, -78.70000000000000284, -1.260385025514398905E-15 ) ) ;
#33350 = CARTESIAN_POINT ( 'NONE',  ( 3.075537641221555596, -76.94583333333332575, -11.44417895085270587 ) ) ;
#33351 = CARTESIAN_POINT ( 'NONE',  ( -9.038948602551000633, -62.13262223832000331, 9.029786144045999663 ) ) ;
#33352 = CARTESIAN_POINT ( 'NONE',  ( -0.4021068579646576713, -79.19911756258647983, -1.186049746191630172 ) ) ;
#33353 = CARTESIAN_POINT ( 'NONE',  ( -8.909545442949999838, -59.94999999967000548, -8.061017305527000687 ) ) ;
#33354 = CARTESIAN_POINT ( 'NONE',  ( 8.584472847271999996, -79.43113511353598710, 4.452153601206999767 ) ) ;
#33355 = CARTESIAN_POINT ( 'NONE',  ( 10.07615509326000058, -17.27367739700000016, -7.986954869189998973 ) ) ;
#33356 = CARTESIAN_POINT ( 'NONE',  ( 13.13047446164998711, -56.01421830981000483, 0.8260994316375004365 ) ) ;
#33357 = ORIENTED_EDGE ( 'NONE', *, *, #50535, .F. ) ;
#33358 = CARTESIAN_POINT ( 'NONE',  ( 11.26184072110999779, -78.52708536617198831, 0.07002095171033999310 ) ) ;
#33359 = DIRECTION ( 'NONE',  ( 0.7071067811865475727, 0.000000000000000000, -0.7071067811865475727 ) ) ;
#33360 = CARTESIAN_POINT ( 'NONE',  ( 5.802455652062412206, -79.21544088115599891, -10.31381048005165013 ) ) ;
#33361 = CARTESIAN_POINT ( 'NONE',  ( -2.677643855409316043, -77.34575811142462953, 11.78110567705964762 ) ) ;
#33362 = LINE ( 'NONE', #51691, #7249 ) ;
#33363 = B_SPLINE_CURVE_WITH_KNOTS ( 'NONE', 3,
 ( #47966, #44096, #39080, #48529, #30207, #37401, #55421, #32964 ),
 .UNSPECIFIED., .F., .F.,
 ( 4, 2, 2, 4 ),
 ( 0.000000000000000000, 0.4999999999999998890, 0.7499999999999998890, 1.000000000000000000 ),
 .UNSPECIFIED. ) ;
#33364 = CARTESIAN_POINT ( 'NONE',  ( -1.127487306198333927, -78.11114297373420357, 0.5952175666624754946 ) ) ;
#33365 = DIRECTION ( 'NONE',  ( 0.000000000000000000, 1.000000000000000000, 0.000000000000000000 ) ) ;
#33366 = CARTESIAN_POINT ( 'NONE',  ( 1.799490225533999732, -59.57152778012000027, -12.64500484464999808 ) ) ;
#33367 = PRODUCT_DEFINITION_SHAPE ( 'NONE', 'NONE',  #518 ) ;
#33368 = CARTESIAN_POINT ( 'NONE',  ( 0.9904172874407001226, -78.38666450191999502, 0.8543161689128000447 ) ) ;
#33369 = CARTESIAN_POINT ( 'NONE',  ( -12.82904091336000008, -55.47547470607999998, 2.062673488738000049 ) ) ;
#33370 = CARTESIAN_POINT ( 'NONE',  ( -10.79343819383525016, -79.46462750683407705, -1.992363124314718181 ) ) ;
#33371 = VECTOR ( 'NONE', #2880, 1000.000000000000000 ) ;
#33372 = CARTESIAN_POINT ( 'NONE',  ( -12.00000000000000000, -77.29999999999999716, 0.000000000000000000 ) ) ;
#33373 = ORIENTED_EDGE ( 'NONE', *, *, #3399, .F. ) ;
#33374 = EDGE_LOOP ( 'NONE', ( #520, #16987, #11478, #49557 ) ) ;
#33375 = CARTESIAN_POINT ( 'NONE',  ( -7.762343146465000565, -77.93383998579800220, -6.339840787406999745 ) ) ;
#33376 = CARTESIAN_POINT ( 'NONE',  ( 9.472593219588741675, -78.81085708764649667, -5.088232997904594157 ) ) ;
#33377 = EDGE_CURVE ( 'NONE', #36154, #33872, #26768, .T. ) ;
#33378 = ORIENTED_EDGE ( 'NONE', *, *, #56263, .T. ) ;
#33379 = CARTESIAN_POINT ( 'NONE',  ( 7.760941378066999796, -17.76914109191999813, 10.15321372496999963 ) ) ;
#33380 = CARTESIAN_POINT ( 'NONE',  ( -9.018298289885381180, -79.37428396167247513, 2.986588901158017784 ) ) ;
#33381 = CARTESIAN_POINT ( 'NONE',  ( 4.614376373661000841, -78.40102880538998420, -10.98357556630999987 ) ) ;
#33382 = PLANE ( 'NONE',  #18375 ) ;
#33383 = CARTESIAN_POINT ( 'NONE',  ( 0.000000000000000000, -74.64999999999999147, 0.000000000000000000 ) ) ;
#33384 = CARTESIAN_POINT ( 'NONE',  ( 3.194290819684984850, -86.12609999968211127, 2.320109443757182088 ) ) ;
#33385 = CARTESIAN_POINT ( 'NONE',  ( 9.376438147752001129, -79.53766105125399122, -6.156339679782000474 ) ) ;
#33386 = VERTEX_POINT ( 'NONE', #31254 ) ;
#33387 = CARTESIAN_POINT ( 'NONE',  ( 4.112279070415571169, -78.14664095760667806, 11.05398264717377188 ) ) ;
#33388 = ORIENTED_EDGE ( 'NONE', *, *, #26459, .T. ) ;
#33389 = CARTESIAN_POINT ( 'NONE',  ( 7.465779029155634738, -77.40036112842625471, 5.461091003694943602 ) ) ;
#33390 = CARTESIAN_POINT ( 'NONE',  ( -17.50000000000000000, -21.00000000000000000, 0.000000000000000000 ) ) ;
#33391 = CARTESIAN_POINT ( 'NONE',  ( 9.070820421759657748, -78.14995580251232354, 6.598623026053274110 ) ) ;
#33392 = CARTESIAN_POINT ( 'NONE',  ( 1.079065815471999867, -77.80869998691809997, 1.201179019145000026 ) ) ;
#33393 = CARTESIAN_POINT ( 'NONE',  ( 9.596002108778174389, -77.59791666666664867, -7.374560639698961140 ) ) ;
#33394 = EDGE_CURVE ( 'NONE', #12948, #11806, #41529, .T. ) ;
#33395 = CARTESIAN_POINT ( 'NONE',  ( -0.7812014261399538029, -81.57275290714748905, -1.008111165206596160 ) ) ;
#33396 = CARTESIAN_POINT ( 'NONE',  ( 0.1429208184976999974, -78.75682716043000653, 1.621183732314999792 ) ) ;
#33397 = CARTESIAN_POINT ( 'NONE',  ( 4.065750953757999220, -79.64804961620099277, -10.27363435345999854 ) ) ;
#33398 = EDGE_CURVE ( 'NONE', #41458, #43521, #4481, .T. ) ;
#33399 = CARTESIAN_POINT ( 'NONE',  ( -5.246265831776000255, -79.73908801482100728, -10.82514862071000117 ) ) ;
#33400 = AXIS2_PLACEMENT_3D ( 'NONE', #4120, #23519, #22121 ) ;
#33401 = CARTESIAN_POINT ( 'NONE',  ( -7.648026768036999989, -60.04999998387000204, -10.12290050219000115 ) ) ;
#33402 = CARTESIAN_POINT ( 'NONE',  ( 2.951756723799000337, -82.33855471126298653, -1.687755689119000202 ) ) ;
#33403 = EDGE_LOOP ( 'NONE', ( #39641, #53396, #19976, #32825, #40197 ) ) ;
#33404 = CARTESIAN_POINT ( 'NONE',  ( -7.374560639698973574, -79.47291666666666288, -9.596002108778167283 ) ) ;
#33405 = CARTESIAN_POINT ( 'NONE',  ( -0.4334656432294999862, -80.22550662411998701, 1.646792182271999971 ) ) ;
#33406 = CARTESIAN_POINT ( 'NONE',  ( 4.675525028857307142, -77.93936046386056660, 9.679868625465889664 ) ) ;
#33407 = CARTESIAN_POINT ( 'NONE',  ( 1.634596122093999959, -78.92999931626700061, 11.63574645295999943 ) ) ;
#33408 = CARTESIAN_POINT ( 'NONE',  ( -9.502921958796708424, -54.05907999824894716, 8.179400290910178839 ) ) ;
#33409 = CARTESIAN_POINT ( 'NONE',  ( -0.9112835142866211324, -78.68838743923397772, 0.8908661252871045155 ) ) ;
#33410 = CARTESIAN_POINT ( 'NONE',  ( 3.164729434338774183, -3.463813167320636932, -1.543632381241692109 ) ) ;
#33411 = CARTESIAN_POINT ( 'NONE',  ( 9.576401669510142156, -80.88767897940253704, 4.883949131846009095 ) ) ;
#33412 = CARTESIAN_POINT ( 'NONE',  ( -8.866000417715000026, -77.05536039296339368, 2.742227037787000388 ) ) ;
#33413 = FACE_OUTER_BOUND ( 'NONE', #54303, .T. ) ;
#33414 = CARTESIAN_POINT ( 'NONE',  ( 9.706674989537999565, -77.16945737050299670, -5.242346328414999590 ) ) ;
#33415 = CARTESIAN_POINT ( 'NONE',  ( -6.620362748380999918, -76.22968996195905333, -10.34376132320999986 ) ) ;
#33416 = CARTESIAN_POINT ( 'NONE',  ( -3.140974612311351777, -78.40416666666665435, -11.68767212001978884 ) ) ;
#33417 = VERTEX_POINT ( 'NONE', #11130 ) ;
#33418 = EDGE_CURVE ( 'NONE', #1462, #33666, #26941, .T. ) ;
#33419 = CARTESIAN_POINT ( 'NONE',  ( -0.8218343019581000330, -80.83782732035000151, -1.050237832603999832 ) ) ;
#33420 = CIRCLE ( 'NONE', #43846, 1.750000000000001332 ) ;
#33421 = CARTESIAN_POINT ( 'NONE',  ( 1.056237665594999875, -61.84866013665000395, -12.77256098201999990 ) ) ;
#33422 = CARTESIAN_POINT ( 'NONE',  ( -7.429974109827198525, -55.28385402668402548, 8.111636311575601610 ) ) ;
#33423 = CARTESIAN_POINT ( 'NONE',  ( 8.196653188619999142, -77.57589910769799246, 7.657217973713000170 ) ) ;
#33424 = CARTESIAN_POINT ( 'NONE',  ( 6.083963560182000130, -78.48130069644298601, -9.135064530700001129 ) ) ;
#33425 = CARTESIAN_POINT ( 'NONE',  ( 7.636246406686000299, -23.76323123101999713, -10.30460653225000023 ) ) ;
#33426 = CARTESIAN_POINT ( 'NONE',  ( 2.702538634015742680, -83.74895832765501780, -3.019410798344609681 ) ) ;
#33427 = CARTESIAN_POINT ( 'NONE',  ( -9.713032445802920023, -61.32293762623282163, 7.970418356084342904 ) ) ;
#33428 = CARTESIAN_POINT ( 'NONE',  ( 9.716210726936424180, -78.49548457799500056, 6.605226190989496260 ) ) ;
#33429 = CARTESIAN_POINT ( 'NONE',  ( -1.223703478834903713, -81.11953203607674823, -0.2972330812242202080 ) ) ;
#33430 = EDGE_LOOP ( 'NONE', ( #44789, #55060, #43198, #27847 ) ) ;
#33431 = FACE_OUTER_BOUND ( 'NONE', #34948, .T. ) ;
#33432 = CARTESIAN_POINT ( 'NONE',  ( 1.199500263597271799, -79.69791666666667140, -0.9218200799623701425 ) ) ;
#33434 = EDGE_CURVE ( 'NONE', #23500, #23213, #13593, .T. ) ;
#33433 = CARTESIAN_POINT ( 'NONE',  ( 7.753900686106000251, -54.51068035512000165, -10.31980286347000053 ) ) ;
#33435 = B_SPLINE_CURVE_WITH_KNOTS ( 'NONE', 3,
 ( #47008, #33096, #14515, #28671, #5374, #55255, #6538, #19537 ),
 .UNSPECIFIED., .F., .F.,
 ( 4, 2, 2, 4 ),
 ( 0.000000000000000000, 0.4999999999999977796, 0.7499999999999988898, 1.000000000000000000 ),
 .UNSPECIFIED. ) ;
#33436 = CARTESIAN_POINT ( 'NONE',  ( 10.55330385607999943, -77.95764851311697896, 3.944190366796999303 ) ) ;
#33437 = CARTESIAN_POINT ( 'NONE',  ( 0.1463366571038000052, -78.32352689100000021, 1.427117860474999889 ) ) ;
#33438 = CARTESIAN_POINT ( 'NONE',  ( -11.00000000000000000, -79.69999999999998863, 0.000000000000000000 ) ) ;
#33439 = CARTESIAN_POINT ( 'NONE',  ( 1.541569372070112909, -81.99491303306574252, -0.1072605994430432114 ) ) ;
#33440 = CARTESIAN_POINT ( 'NONE',  ( -0.7946115520685833600, -83.26841143953370761, 1.288064595800165524 ) ) ;
#33441 = CARTESIAN_POINT ( 'NONE',  ( 0.8868842948722143182, -79.78821287788076688, -0.8805106682841317145 ) ) ;
#33442 = CARTESIAN_POINT ( 'NONE',  ( 0.7678017030685237998, -80.92358540104676479, 0.9995472151052681165 ) ) ;
#33443 = ORIENTED_EDGE ( 'NONE', *, *, #5295, .F. ) ;
#33444 = CARTESIAN_POINT ( 'NONE',  ( -1.107453414133191094, -81.63871445155162121, -0.5797266078115248522 ) ) ;
#33445 = CARTESIAN_POINT ( 'NONE',  ( -0.2277317800897999955, -78.51452830333799682, -10.99999347944999961 ) ) ;
#33446 = DIRECTION ( 'NONE',  ( 0.7071067811864980568, -0.7071067811865969777, -4.786443936370980024E-09 ) ) ;
#33447 = EDGE_LOOP ( 'NONE', ( #6726, #51621, #37428 ) ) ;
#33448 = ORIENTED_EDGE ( 'NONE', *, *, #50667, .F. ) ;
#33449 = CARTESIAN_POINT ( 'NONE',  ( -1.198617868132000108, -80.64177705559200149, -0.6367414467165999348 ) ) ;
#33450 = AXIS2_PLACEMENT_3D ( 'NONE', #49324, #26866, #40461 ) ;
#33451 = ORIENTED_EDGE ( 'NONE', *, *, #27793, .F. ) ;
#33452 = CARTESIAN_POINT ( 'NONE',  ( 9.499693205731109202, -80.00008708754018016, -1.997583897032410100E-06 ) ) ;
#33453 = EDGE_LOOP ( 'NONE', ( #13695, #4075, #20261, #16051 ) ) ;
#33454 = CARTESIAN_POINT ( 'NONE',  ( 1.669724228656999987, -18.63102323466000243, 12.48434610067999984 ) ) ;
#33455 = APPLICATION_PROTOCOL_DEFINITION ( 'draft international standard', 'automotive_design', 1998, #52268 ) ;
#33456 = CARTESIAN_POINT ( 'NONE',  ( 0.7554284705563509839, -78.16666666666668561, -1.310679582531385945 ) ) ;
#33457 = CARTESIAN_POINT ( 'NONE',  ( 4.739769873023999658, -78.98486001420198477, -8.830749431300999319 ) ) ;
#33458 = AXIS2_PLACEMENT_3D ( 'NONE', #2495, #37331, #37913 ) ;
#33459 = CARTESIAN_POINT ( 'NONE',  ( 4.687722617765969879, -78.26731946421421071, -7.992545327129488619 ) ) ;
#33460 = FACE_OUTER_BOUND ( 'NONE', #48418, .T. ) ;
#33461 = EDGE_LOOP ( 'NONE', ( #52072, #19736, #6304, #39168 ) ) ;
#33462 = ORIENTED_EDGE ( 'NONE', *, *, #2676, .T. ) ;
#33463 = CARTESIAN_POINT ( 'NONE',  ( -9.250000000000000000, -77.59999999999999432, 0.000000000000000000 ) ) ;
#33464 = CARTESIAN_POINT ( 'NONE',  ( 6.055527902613000002, -77.71999999999999886, 7.319875806370000682 ) ) ;
#33465 = FILL_AREA_STYLE_COLOUR ( '', #8309 ) ;
#33466 = CARTESIAN_POINT ( 'NONE',  ( 9.576266942516207692, -76.04999999999998295, -5.533717098459915995 ) ) ;
#33467 = CARTESIAN_POINT ( 'NONE',  ( -9.446433787353997857, -78.28822960936498987, -2.221620594898999990 ) ) ;
#33468 = CARTESIAN_POINT ( 'NONE',  ( 0.000000000000000000, 4.040000000000000036, 0.000000000000000000 ) ) ;
#33469 = DIRECTION ( 'NONE',  ( 0.000000000000000000, 0.000000000000000000, -1.000000000000000000 ) ) ;
#33470 = CARTESIAN_POINT ( 'NONE',  ( -4.582365512893317394, -77.39392094393495825, -11.13666644834475861 ) ) ;
#33471 = CARTESIAN_POINT ( 'NONE',  ( 0.2675321060165000153, -79.40754610911000100, -1.681415376183999832 ) ) ;
#33472 = CARTESIAN_POINT ( 'NONE',  ( -8.307389487175075971, -76.63738348406045020, 8.309511392601589108 ) ) ;
#33473 = CARTESIAN_POINT ( 'NONE',  ( 0.9272340829244000160, -81.25267555511598516, 4.067774877469999772 ) ) ;
#33474 = CARTESIAN_POINT ( 'NONE',  ( -1.064988270483648414, -79.68717248096253059, 1.072152466623225386 ) ) ;
#33475 = CARTESIAN_POINT ( 'NONE',  ( -5.611728806388999402, -78.52021332859899871, -8.168780722191000265 ) ) ;
#33476 = FACE_OUTER_BOUND ( 'NONE', #7780, .T. ) ;
#33477 = CARTESIAN_POINT ( 'NONE',  ( 1.667936697358999965, -19.23537109840999904, -12.53241208775999915 ) ) ;
#33479 = CARTESIAN_POINT ( 'NONE',  ( 1.382886570147999983, -17.36901780168000187, -12.65982054476000052 ) ) ;
#33478 = CARTESIAN_POINT ( 'NONE',  ( -7.919595949288999570, -57.79999999967000690, -8.909545442949999838 ) ) ;
#33480 = CARTESIAN_POINT ( 'NONE',  ( 1.980584515752000119, -23.26485146623999967, -12.76303204602000108 ) ) ;
#33481 = CARTESIAN_POINT ( 'NONE',  ( 0.000000000000000000, -81.79999999999998295, -10.70000000000298179 ) ) ;
#33482 = DIRECTION ( 'NONE',  ( 0.000000000000000000, -1.000000000000000000, 0.000000000000000000 ) ) ;
#33483 = CARTESIAN_POINT ( 'NONE',  ( 0.3644735108981210225, -1.383145019569959056, -3.562971877919846264 ) ) ;
#33484 = EDGE_LOOP ( 'NONE', ( #46335, #10174, #49459, #31764, #38178 ) ) ;
#33485 = CARTESIAN_POINT ( 'NONE',  ( -5.539808784079887083, -78.28333333333333144, -9.611650271896841957 ) ) ;
#33486 = ADVANCED_FACE ( 'NONE', ( #24402 ), #42820, .F. ) ;
#33487 = DIRECTION ( 'NONE',  ( 0.7071067811865475727, 0.000000000000000000, -0.7071067811865475727 ) ) ;
#33488 = CARTESIAN_POINT ( 'NONE',  ( -1.929975092519000013, -55.59892743702999240, 12.72537404207999856 ) ) ;
#33489 = AXIS2_PLACEMENT_3D ( 'NONE', #3094, #56824, #16670 ) ;
#33490 = CARTESIAN_POINT ( 'NONE',  ( 0.9905026783004660107, -78.40226506858486744, 0.7633233902531472159 ) ) ;
#33491 = B_SPLINE_CURVE_WITH_KNOTS ( 'NONE', 3,
 ( #58310, #16995, #8414, #53005, #12556, #21988, #45032, #57434, #13717, #3986, #39708, #39997, #44153, #49762, #36160, #53587, #31121, #48586, #30554, #58010, #35561, #8712, #22282, #26703, #8131, #44734, #26996, #31712, #25842, #22584, #3700, #40300, #21703, #39427, #57715, #17272, #35262, #53292, #35862, #40597, #53890, #13421, #19614, #5450, #37612, #55042, #18455, #54752, #36445, #37319, #4878, #50337, #42051, #28455, #46210, #5164, #23453, #55335, #18743, #55627, #9888, #37028, #27867, #45914, #14297, #41465, #14591, #15178, #14880, #14010, #32876, #50920, #50631, #33171, #1051, #24037, #32007, #54475, #27291, #10469, #9595, #46503 ),
 .UNSPECIFIED., .F., .F.,
 ( 4, 2, 2, 2, 2, 2, 2, 2, 1, 1, 1, 2, 2, 2, 2, 2, 1, 1, 1, 2, 2, 2, 2, 2, 2, 2, 1, 1, 1, 1, 2, 2, 2, 2, 2, 1, 1, 1, 1, 2, 2, 2, 2, 2, 2, 2, 2, 4 ),
 ( 0.000000000000000000, 0.01562499999999791833, 0.03124999999999583666, 0.04687499999999375500, 0.06249999999999167333, 0.09374999999998750999, 0.1093749999999854006, 0.1171874999999843320, 0.1210937499999838463, 0.1230468749999836242, 0.1240234374999835132, 0.1245117187499834299, 0.1249999999999833328, 0.1874999999999746314, 0.2187499999999702460, 0.2343749999999679978, 0.2421874999999668876, 0.2460937499999663325, 0.2480468749999660827, 0.2490234374999659994, 0.2499999999999658884, 0.3749999999999674705, 0.4999999999999690248, 0.6249999999999705791, 0.6874999999999713562, 0.7187499999999715783, 0.7343749999999715783, 0.7421874999999714673, 0.7460937499999714673, 0.7480468749999713562, 0.7490234374999714673, 0.7499999999999715783, 0.8124999999999781286, 0.8437499999999813483, 0.8593749999999830136, 0.8671874999999837907, 0.8710937499999842348, 0.8730468749999843459, 0.8740234374999844569, 0.8745117187499845679, 0.8749999999999845679, 0.9062499999999884537, 0.9218749999999904521, 0.9374999999999923395, 0.9531249999999942268, 0.9687499999999961142, 0.9843749999999981126, 1.000000000000000000 ),
 .UNSPECIFIED. ) ;
#33492 = TOROIDAL_SURFACE ( 'NONE', #6150, 1.250000000000000000, 0.5000000000000000000 ) ;
#33493 = CARTESIAN_POINT ( 'NONE',  ( 9.314328882329000692, -79.06204449888298313, -2.038033000261999739 ) ) ;
#33494 = CARTESIAN_POINT ( 'NONE',  ( -12.77651047528000028, -53.49104280904999342, -0.04320343284637000181 ) ) ;
#33495 = CARTESIAN_POINT ( 'NONE',  ( -9.050966799188000067, -55.64999999964999233, -7.919595949288999570 ) ) ;
#33496 = CARTESIAN_POINT ( 'NONE',  ( -1.485504995112404858, -79.48613549087271224, 10.64710564121015679 ) ) ;
#33497 = CIRCLE ( 'NONE', #24062, 10.69999999999999929 ) ;
#33498 = CARTESIAN_POINT ( 'NONE',  ( -6.169975633831000117, -79.51351332859900367, -7.535017646125999669 ) ) ;
#33499 = CARTESIAN_POINT ( 'NONE',  ( 0.000000000000000000, -75.15999999999999659, 0.000000000000000000 ) ) ;
#33500 = CARTESIAN_POINT ( 'NONE',  ( -4.728196578006000017, -77.46027578382999934, -9.874152122658001574 ) ) ;
#33501 = EDGE_CURVE ( 'NONE', #53336, #44757, #30259, .T. ) ;
#33502 = CARTESIAN_POINT ( 'NONE',  ( -1.391687965710999952, -81.44947602328198855, -0.7977148706058000416 ) ) ;
#33503 = CARTESIAN_POINT ( 'NONE',  ( 5.395043866960259393, -77.97557524174651178, 7.539927916798925267 ) ) ;
#33504 = CARTESIAN_POINT ( 'NONE',  ( -9.066428667704000688, -77.99914192992498840, 2.532008238717000204 ) ) ;
#33506 = DIRECTION ( 'NONE',  ( -0.9859154929577472748, 0.1672442547470080754, 0.000000000000000000 ) ) ;
#33505 = CARTESIAN_POINT ( 'NONE',  ( -1.577929596948000057, -84.66679343488898724, -3.409033368874000214 ) ) ;
#33507 = DIRECTION ( 'NONE',  ( -1.000000000000000000, 0.000000000000000000, 0.000000000000000000 ) ) ;
#33508 = CARTESIAN_POINT ( 'NONE',  ( 1.250000000000000000, -78.85000000000000853, 0.000000000000000000 ) ) ;
#33509 = CARTESIAN_POINT ( 'NONE',  ( 4.415872262643816271, -80.25885311859400417, -9.801209063010123401 ) ) ;
#33510 = LINE ( 'NONE', #14629, #27717 ) ;
#33511 = LINE ( 'NONE', #32622, #23784 ) ;
#33512 = CARTESIAN_POINT ( 'NONE',  ( -1.818468715484000065E-14, -79.29999999999999716, -12.04999999999996874 ) ) ;
#33513 = ORIENTED_EDGE ( 'NONE', *, *, #55235, .T. ) ;
#33514 = ORIENTED_EDGE ( 'NONE', *, *, #30211, .F. ) ;
#33515 = CARTESIAN_POINT ( 'NONE',  ( 11.90415444617999974, -79.80461201918980407, -1.731350929957999885 ) ) ;
#33516 = CYLINDRICAL_SURFACE ( 'NONE', #30266, 1.250000000000000000 ) ;
#33517 = FACE_OUTER_BOUND ( 'NONE', #30477, .T. ) ;
#33518 = ORIENTED_EDGE ( 'NONE', *, *, #32479, .F. ) ;
#33519 = CARTESIAN_POINT ( 'NONE',  ( 11.75393452337000078, -77.35954407085999662, -2.068948229565000130 ) ) ;
#33520 = ADVANCED_FACE ( 'NONE', ( #20555 ), #52145, .T. ) ;
#33521 = VERTEX_POINT ( 'NONE', #52430 ) ;
#33522 = VERTEX_POINT ( 'NONE', #43570 ) ;
#33523 = ORIENTED_EDGE ( 'NONE', *, *, #30754, .F. ) ;
#33524 = CARTESIAN_POINT ( 'NONE',  ( -1.281863394863000050, -78.96791748997289062, -3.307769143335999917 ) ) ;
#33525 = CARTESIAN_POINT ( 'NONE',  ( 9.036425267681602591, -79.17454650634799407, 2.930576671598891014 ) ) ;
#33526 = AXIS2_PLACEMENT_3D ( 'NONE', #43662, #44819, #34776 ) ;
#33527 = VERTEX_POINT ( 'NONE', #3134 ) ;
#33528 = CARTESIAN_POINT ( 'NONE',  ( -10.45205659047999980, -59.56232685193999998, -7.651160337235999975 ) ) ;
#33529 = FACE_OUTER_BOUND ( 'NONE', #39974, .T. ) ;
#33530 = VERTEX_POINT ( 'NONE', #21124 ) ;
#33531 = CARTESIAN_POINT ( 'NONE',  ( 5.413904038987179312, -80.66666666666664298, -9.393203674808262349 ) ) ;
#33532 = CARTESIAN_POINT ( 'NONE',  ( -0.4522900895953318456, -78.85072686557104760, -1.438476364793949802 ) ) ;
#33533 = CARTESIAN_POINT ( 'NONE',  ( -10.78228907302829320, -79.80000000000002558, -5.154748993316502492 ) ) ;
#33534 = VECTOR ( 'NONE', #4521, 1000.000000000000000 ) ;
#33535 = CYLINDRICAL_SURFACE ( 'NONE', #27425, 10.69999999999999929 ) ;
#33536 = CARTESIAN_POINT ( 'NONE',  ( 3.335937506701805777, -0.9140624994645799584, 0.5252349859688600908 ) ) ;
#33537 = CARTESIAN_POINT ( 'NONE',  ( 9.690463944985998168, -78.49577218054876937, -0.5153813127049999832 ) ) ;
#33538 = CARTESIAN_POINT ( 'NONE',  ( -8.075725583014000009, -76.46247691852698836, -7.736700848913999451 ) ) ;
#33539 = CARTESIAN_POINT ( 'NONE',  ( -1.876049203459514203, -79.95935840993698207, -9.533404770284985119 ) ) ;
#33540 = CARTESIAN_POINT ( 'NONE',  ( 5.212769757709797780, -77.02020172621061533, -8.147222165250761705 ) ) ;
#33541 = CARTESIAN_POINT ( 'NONE',  ( 10.99909880189000155, -76.65258609231899811, 1.593564419259000164 ) ) ;
#33542 = CARTESIAN_POINT ( 'NONE',  ( -7.252642920492362144, -78.65334380994336527, -5.741174788834818798 ) ) ;
#33543 = CARTESIAN_POINT ( 'NONE',  ( 8.138070855479238475, -76.51354002294402790, 8.478431565815370163 ) ) ;
#33544 = CARTESIAN_POINT ( 'NONE',  ( -1.261445002938999860, -79.19066194505900569, -0.1968185027220000216 ) ) ;
#33545 = CARTESIAN_POINT ( 'NONE',  ( -7.720906625823901415, -80.16344810211410277, -7.835007712627920284 ) ) ;
#33546 = CARTESIAN_POINT ( 'NONE',  ( -2.373398577992831271, -3.040439981628704214, 2.220387636506996554 ) ) ;
#33547 = CARTESIAN_POINT ( 'NONE',  ( -0.3751936674244999992, -80.36167549782599906, -3.569729292793000219 ) ) ;
#33548 = CARTESIAN_POINT ( 'NONE',  ( 4.687352340516000027, -79.23329064464900284, -11.13768991102999983 ) ) ;
#33549 = CARTESIAN_POINT ( 'NONE',  ( -9.933930371580135699, -78.06886005323073618, 4.108349863449450190 ) ) ;
#33550 = CARTESIAN_POINT ( 'NONE',  ( 0.9737724313953866062, -82.90436024173828855, 0.7837087735941486999 ) ) ;
#33551 = DIRECTION ( 'NONE',  ( 0.000000000000000000, 0.000000000000000000, -1.000000000000000000 ) ) ;
#33552 = CARTESIAN_POINT ( 'NONE',  ( -2.098469896607999926E-14, 0.000000000000000000, 0.000000000000000000 ) ) ;
#33553 = CARTESIAN_POINT ( 'NONE',  ( -1.250000000000001332, -80.48958333333332860, 0.1636246173744632659 ) ) ;
#33554 = CARTESIAN_POINT ( 'NONE',  ( 10.07722254365999959, -21.74800977511999989, 7.718368845776000242 ) ) ;
#33555 = DIRECTION ( 'NONE',  ( 0.7071067811865474617, 0.000000000000000000, 0.7071067811865474617 ) ) ;
#33556 = ADVANCED_FACE ( 'NONE', ( #56858 ), #57889, .F. ) ;
#33557 = CARTESIAN_POINT ( 'NONE',  ( 10.01235002625000092, -60.09848884406000025, 7.653559626114000203 ) ) ;
#33558 = EDGE_CURVE ( 'NONE', #409, #31439, #34688, .T. ) ;
#33559 = CARTESIAN_POINT ( 'NONE',  ( 1.460959015002474493, -80.62916666666664867, -0.3926218265389176953 ) ) ;
#33560 = DIRECTION ( 'NONE',  ( 0.000000000000000000, -1.000000000000000000, 0.000000000000000000 ) ) ;
#33561 = CARTESIAN_POINT ( 'NONE',  ( 8.660058625535635102, -77.64905087922392113, -6.518498288151249653 ) ) ;
#33562 = CARTESIAN_POINT ( 'NONE',  ( 8.140362823347702559, -78.29063355552166570, -7.514683589434230093 ) ) ;
#33563 = CARTESIAN_POINT ( 'NONE',  ( -3.548303639236000340, -79.44880232962658795, -10.38621961377000247 ) ) ;
#33564 = CARTESIAN_POINT ( 'NONE',  ( 9.938819120173999266, -76.55355739169999651, 6.834338467449999399 ) ) ;
#33565 = ORIENTED_EDGE ( 'NONE', *, *, #49269, .T. ) ;
#33566 = B_SPLINE_SURFACE_WITH_KNOTS ( 'NONE', 3, 3, ( 
 ( #37726, #42167, #46321, #1735, #28270, #19728, #37429, #55746, #15291, #33285, #37141, #55150, #14696, #55449, #32698, #50746, #14992, #10288, #5846, #23852, #32989, #51035, #10583, #27299, #40892, #36454, #23751, #9894, #772, #14016, #32014, #18463, #50056, #18749, #19333 ),
 ( #49768, #1056, #37034, #483, #13725, #41764, #9602, #55049, #5171, #32591, #50641, #19044, #14597, #27876, #9309, #41471, #46216, #31430, #45334, #27587, #55343, #32297, #14304, #23459, #50344, #41182, #5457, #9019, #23174, #45630, #10188, #28166, #45924, #5743, #1342 ),
 ( #36168, #37327, #49470, #27006, #4884, #45040, #4594, #18175, #22590, #40603, #200, #54481, #54187, #31722, #22881, #36743, #54761, #35273, #35572, #22888, #18181, #36460, #17285, #17585, #35874, #32021, #44445, #8724, #17885, #30849, #40900, #58024, #44745, #45340, #207 ),
 ( #49475, #3997, #48886, #53903, #26717, #49171, #22296, #39720, #4296, #36176, #40313, #45047, #53306, #22599, #50063, #22001, #9316, #58322, #57728, #40610, #54193, #54487, #27309, #18469, #13731, #31728, #14023, #49773, #53599, #4891, #8428, #13434, #9609, #489, #27595 ) ),
 .UNSPECIFIED., .F., .F., .F.,
 ( 4, 4 ),
 ( 4, 1, 1, 1, 1, 1, 1, 1, 1, 1, 1, 1, 1, 1, 1, 1, 1, 1, 1, 1, 1, 1, 1, 1, 1, 1, 1, 1, 1, 1, 1, 1, 4 ),
 ( -0.5168282991433000850, 1.516828299142999992 ),
 ( 0.4364214072047999937, 0.4543785682496999656, 0.4723357292945999930, 0.4902928903395999960, 0.5082500513844999679, 0.5262072124294999709, 0.5441643734743999428, 0.5621215345193999458, 0.5800786955643000287, 0.5980358566093000316, 0.6159930176542000035, 0.6339501786992000065, 0.6519073397440999784, 0.6698645007890999814, 0.6878216618339999533, 0.7057788228789999563, 0.7237359839238999282, 0.7416931449688000111, 0.7596503060138000141, 0.7776074670587000970, 0.7955646281037001000, 0.8135217891486000719, 0.8314789501936000748, 0.8494361112385000467, 0.8673932722835000497, 0.8853504333284000216, 0.9033075943734000246, 0.9212647554182999965, 0.9392219164632999995, 0.9571790775082000824, 0.9751362385532000854, 0.9930933995981000573, 1.011050560643000029 ),
 .UNSPECIFIED. ) ;
#33567 = CARTESIAN_POINT ( 'NONE',  ( -1.645978843960999916, -83.23196544543098696, 3.605098035829000125 ) ) ;
#33568 = CARTESIAN_POINT ( 'NONE',  ( 9.751903312417001146, -80.50087683706640007, 5.687046010848999522 ) ) ;
#33569 = EDGE_CURVE ( 'NONE', #14133, #52412, #22050, .T. ) ;
#33570 = CARTESIAN_POINT ( 'NONE',  ( 8.916672120480782837, -78.32869008935927013, -2.465681892806660169 ) ) ;
#33571 = CARTESIAN_POINT ( 'NONE',  ( 10.25203062048420399, -54.67822876341044491, 7.730397977249435115 ) ) ;
#33572 = CARTESIAN_POINT ( 'NONE',  ( 0.1392748842281999744, -77.27569472622099056, 11.21600254538999941 ) ) ;
#33573 = DIRECTION ( 'NONE',  ( 0.000000000000000000, 1.000000000000000000, 0.000000000000000000 ) ) ;
#33574 = CARTESIAN_POINT ( 'NONE',  ( -6.496683922195000349, -78.26229597363898449, 7.256224481198000120 ) ) ;
#33575 = CARTESIAN_POINT ( 'NONE',  ( -0.7803569495551999635, -81.97502974756999095, -1.471836271561000054 ) ) ;
#33576 = DIRECTION ( 'NONE',  ( 1.000000000000000000, 0.000000000000000000, 0.000000000000000000 ) ) ;
#33577 = CARTESIAN_POINT ( 'NONE',  ( -1.102025757167999886, -80.42671995918099981, 1.180137589876000037 ) ) ;
#33578 = ORIENTED_EDGE ( 'NONE', *, *, #38191, .T. ) ;
#33579 = VECTOR ( 'NONE', #21209, 999.9999999999998863 ) ;
#33580 = DIRECTION ( 'NONE',  ( 0.000000000000000000, 1.000000000000000000, 0.000000000000000000 ) ) ;
#33581 = CARTESIAN_POINT ( 'NONE',  ( 1.250000000000000000, -23.25000000000000000, 12.00000000000000000 ) ) ;
#33582 = ORIENTED_EDGE ( 'NONE', *, *, #22117, .F. ) ;
#33583 = AXIS2_PLACEMENT_3D ( 'NONE', #22136, #44581, #30694 ) ;
#33584 = CARTESIAN_POINT ( 'NONE',  ( 1.224162466603000210, -77.89564526295849589, -0.5291525010897000225 ) ) ;
#33585 = CARTESIAN_POINT ( 'NONE',  ( 0.000000000000000000, 4.040000000000000036, 0.000000000000000000 ) ) ;
#33586 = CYLINDRICAL_SURFACE ( 'NONE', #19995, 1.250000000000000000 ) ;
#33587 = VECTOR ( 'NONE', #23251, 1000.000000000000000 ) ;
#33588 = ORIENTED_EDGE ( 'NONE', *, *, #33712, .F. ) ;
#33589 = CARTESIAN_POINT ( 'NONE',  ( 4.484119338316999936, -77.48133731782699840, -11.43188768503999952 ) ) ;
#33590 = CARTESIAN_POINT ( 'NONE',  ( 5.551777116439001070, -77.39115562571699058, 9.867624315061000573 ) ) ;
#33591 = CARTESIAN_POINT ( 'NONE',  ( -10.74992925859148230, -77.58958685757916385, 1.407065223439301072 ) ) ;
#33592 = ORIENTED_EDGE ( 'NONE', *, *, #17943, .T. ) ;
#33593 = ORIENTED_EDGE ( 'NONE', *, *, #55900, .F. ) ;
#33594 = CARTESIAN_POINT ( 'NONE',  ( -0.4825602083052458746, -80.50662037162305751, 1.153044462113711033 ) ) ;
#33595 = DIRECTION ( 'NONE',  ( 0.000000000000000000, -1.000000000000000000, 0.000000000000000000 ) ) ;
#33596 = CARTESIAN_POINT ( 'NONE',  ( 1.739862777674999972, -79.49090881849700452, 9.611119481339999382 ) ) ;
#33597 = ORIENTED_EDGE ( 'NONE', *, *, #15132, .F. ) ;
#33598 = CARTESIAN_POINT ( 'NONE',  ( -12.70610460582424750, -24.45512899796313633, -1.580683094053911830 ) ) ;
#33599 = CARTESIAN_POINT ( 'NONE',  ( -8.157922760392999351, -79.63124863701999345, -7.254216858269000312 ) ) ;
#33600 = ORIENTED_EDGE ( 'NONE', *, *, #29794, .T. ) ;
#33601 = CARTESIAN_POINT ( 'NONE',  ( -12.43571054526000097, -24.87980566418999828, -0.4385525234354999968 ) ) ;
#33602 = CARTESIAN_POINT ( 'NONE',  ( 8.979348251287998295, -77.78619415034600593, 3.086914251890999772 ) ) ;
#33603 = EDGE_CURVE ( 'NONE', #20388, #11813, #28677, .T. ) ;
#33604 = CARTESIAN_POINT ( 'NONE',  ( 1.250000000000000000, -55.54999999966999980, 12.00000000000000000 ) ) ;
#33605 = CARTESIAN_POINT ( 'NONE',  ( -8.485281374238999419, -55.54999999966999980, 8.485281374238999419 ) ) ;
#33606 = CARTESIAN_POINT ( 'NONE',  ( 4.316728918958533612, -78.88752913613843987, 8.714317166737037823 ) ) ;
#33607 = CARTESIAN_POINT ( 'NONE',  ( 2.887802510467000427, -76.96689670991779053, 9.218216609984001053 ) ) ;
#33608 = CARTESIAN_POINT ( 'NONE',  ( -1.530868492697737393, -78.85611562010234366, -0.1310416657043483035 ) ) ;
#33609 = CARTESIAN_POINT ( 'NONE',  ( -6.760013919724058518, -79.67291666666666572, -8.796335266379987416 ) ) ;
#33610 = B_SPLINE_CURVE_WITH_KNOTS ( 'NONE', 3,
 ( #55653, #19637, #41782, #5759, #15202, #14319 ),
 .UNSPECIFIED., .F., .F.,
 ( 4, 1, 1, 4 ),
 ( 0.000000000000000000, 0.3333333333333000081, 0.6666666666667000474, 1.000000000000000000 ),
 .UNSPECIFIED. ) ;
#33611 = CARTESIAN_POINT ( 'NONE',  ( 11.05577208806000122, -76.66461526165998919, -4.921212746988999243 ) ) ;
#33612 = CARTESIAN_POINT ( 'NONE',  ( 0.7680438806649999561, -80.74360977560299091, 1.420324776730000238 ) ) ;
#33613 = CARTESIAN_POINT ( 'NONE',  ( -2.486604901413153268, -78.00416666666664867, -9.252740428348998236 ) ) ;
#33614 = CARTESIAN_POINT ( 'NONE',  ( 0.000000000000000000, -82.00000000000000000, 0.000000000000000000 ) ) ;
#33615 = CARTESIAN_POINT ( 'NONE',  ( 10.82405698390000026, -79.23694587766000552, 5.765268246940999930 ) ) ;
#33616 = CARTESIAN_POINT ( 'NONE',  ( 0.03250568004163000707, -76.00867412998898942, 11.74995503739000036 ) ) ;
#33617 = DIRECTION ( 'NONE',  ( 0.000000000000000000, -1.000000000000000000, 0.000000000000000000 ) ) ;
#33618 = CARTESIAN_POINT ( 'NONE',  ( -12.01171088695212852, -78.04760641092620688, 0.3579334955698593168 ) ) ;
#33619 = CARTESIAN_POINT ( 'NONE',  ( 6.879576957522999692, -79.07245835675909973, 8.859431780707000215 ) ) ;
#33620 = CIRCLE ( 'NONE', #35506, 14.00000000000000000 ) ;
#33621 = ORIENTED_EDGE ( 'NONE', *, *, #57139, .F. ) ;
#33623 = EDGE_CURVE ( 'NONE', #24388, #51092, #40341, .T. ) ;
#33622 = CARTESIAN_POINT ( 'NONE',  ( 1.237362355298573968, -80.05155256813580422, 0.9256756271965481675 ) ) ;
#33624 = CARTESIAN_POINT ( 'NONE',  ( 7.587587806099000076, -77.02559020532309830, -6.054761558390000076 ) ) ;
#33625 = DIRECTION ( 'NONE',  ( 0.000000000000000000, -1.000000000000000000, 0.000000000000000000 ) ) ;
#33626 = CIRCLE ( 'NONE', #31721, 2.299999999999999822 ) ;
#33627 = CARTESIAN_POINT ( 'NONE',  ( 0.1963495408493638184, -78.63541666666668561, -1.499999999999999778 ) ) ;
#33628 = CARTESIAN_POINT ( 'NONE',  ( -3.690989959373000229, -2.872579967774000487, 0.4135749490274999718 ) ) ;
#33629 = CARTESIAN_POINT ( 'NONE',  ( -11.66523904145000046, -77.96402128256200115, -3.450322983582000180 ) ) ;
#33630 = CARTESIAN_POINT ( 'NONE',  ( -5.177883096403999907, -77.35120832211899256, -8.249196342081999589 ) ) ;
#33632 = CARTESIAN_POINT ( 'NONE',  ( 10.18499221077999906, -20.25022860214999909, -7.710118476625000383 ) ) ;
#33631 = CARTESIAN_POINT ( 'NONE',  ( -11.39055364300875262, -76.18003226433557984, 2.885907805895131961 ) ) ;
#33633 = CARTESIAN_POINT ( 'NONE',  ( 5.592013246121999792, -78.85879439517700007, 9.375753510130000024 ) ) ;
#33634 = CARTESIAN_POINT ( 'NONE',  ( -10.65756401913684215, -79.58963493226011110, 1.416508826642955521 ) ) ;
#33635 = ORIENTED_EDGE ( 'NONE', *, *, #756, .T. ) ;
#33636 = DIRECTION ( 'NONE',  ( 0.000000000000000000, -1.000000000000000000, 0.000000000000000000 ) ) ;
#33637 = CARTESIAN_POINT ( 'NONE',  ( -4.658421459997613923, -78.01682404241935842, 8.082575534271919437 ) ) ;
#33638 = ADVANCED_FACE ( 'NONE', ( #35260, #30552 ), #34973, .F. ) ;
#33639 = CARTESIAN_POINT ( 'NONE',  ( 6.606377239730313988, -77.32291666666665719, 8.596418555780454440 ) ) ;
#33640 = CARTESIAN_POINT ( 'NONE',  ( -7.619389973917000347, -60.20786254198000620, 10.35398617735999949 ) ) ;
#33641 = CARTESIAN_POINT ( 'NONE',  ( -0.5925039872731914237, -79.18577407509000921, -1.100617820668964741 ) ) ;
#33642 = CARTESIAN_POINT ( 'NONE',  ( -10.99162204853783109, -80.09707396476217411, 0.4707213547353387151 ) ) ;
#33643 = FACE_OUTER_BOUND ( 'NONE', #35019, .T. ) ;
#33644 = LINE ( 'NONE', #51684, #375 ) ;
#33645 = CARTESIAN_POINT ( 'NONE',  ( -12.70455814331304190, -54.23992875941976877, -1.489882837218519773 ) ) ;
#33646 = ORIENTED_EDGE ( 'NONE', *, *, #19243, .T. ) ;
#33647 = CARTESIAN_POINT ( 'NONE',  ( -8.320158381697998706, -78.71773976718499455, 7.590054615178000397 ) ) ;
#33648 = CARTESIAN_POINT ( 'NONE',  ( 7.648026766735999793, -23.25000000582000226, -10.12290050089000104 ) ) ;
#33649 = CARTESIAN_POINT ( 'NONE',  ( 1.199999999999999956, -80.99999999999998579, -7.000000000000000000 ) ) ;
#33650 = CARTESIAN_POINT ( 'NONE',  ( -3.399395994687518296, -78.67390000031814168, -0.06408487577575498750 ) ) ;
#33651 = CARTESIAN_POINT ( 'NONE',  ( 1.152279072913166447, -81.38189058625292205, 0.4841459733426476952 ) ) ;
#33652 = CARTESIAN_POINT ( 'NONE',  ( 0.8118302357295669180, -78.96982299379136805, 0.9819661897715911136 ) ) ;
#33653 = CARTESIAN_POINT ( 'NONE',  ( -9.126674389914770202, -76.99999999999998579, 1.824525243212377523 ) ) ;
#33654 = CARTESIAN_POINT ( 'NONE',  ( 3.365090863054962966, -82.21166587810114379, -0.7152718134427592522 ) ) ;
#33655 = CIRCLE ( 'NONE', #38379, 3.799999999999999822 ) ;
#33656 = CARTESIAN_POINT ( 'NONE',  ( 0.6875379384163999852, -78.91098019970999644, 1.112687622202999771 ) ) ;
#33657 = FACE_BOUND ( 'NONE', #40721, .T. ) ;
#33658 = CARTESIAN_POINT ( 'NONE',  ( 1.217465845835393967, -78.27083333333332860, 0.3271848554491025851 ) ) ;
#33659 = FACE_OUTER_BOUND ( 'NONE', #25825, .T. ) ;
#33660 = ORIENTED_EDGE ( 'NONE', *, *, #23091, .F. ) ;
#33661 = VECTOR ( 'NONE', #51579, 1000.000000000000000 ) ;
#33662 = ORIENTED_EDGE ( 'NONE', *, *, #30051, .F. ) ;
#33663 = CARTESIAN_POINT ( 'NONE',  ( 8.338887569536000299, -77.14397343098400484, 9.430583988958000319 ) ) ;
#33664 = CARTESIAN_POINT ( 'NONE',  ( 2.285767309104500988, -78.74219246598565292, -10.50419463615617488 ) ) ;
#33665 = AXIS2_PLACEMENT_3D ( 'NONE', #29343, #47683, #16077 ) ;
#33666 = VERTEX_POINT ( 'NONE', #8129 ) ;
#33667 = CARTESIAN_POINT ( 'NONE',  ( 10.31988039474999930, -17.71085245535000396, 7.753829094184000681 ) ) ;
#33668 = ADVANCED_FACE ( 'NONE', ( #43283 ), #3415, .F. ) ;
#33669 = CARTESIAN_POINT ( 'NONE',  ( 1.499999999999999778, -80.16041666666669130, 0.1963495408493654004 ) ) ;
#33670 = CARTESIAN_POINT ( 'NONE',  ( -10.22174476410000032, -78.28692462859000045, 6.403415649647000052 ) ) ;
#33671 = EDGE_CURVE ( 'NONE', #8523, #56093, #48299, .T. ) ;
#33672 = CARTESIAN_POINT ( 'NONE',  ( 7.660411271065999728, -59.99173735459000056, 10.01752031416000044 ) ) ;
#33673 = FACE_OUTER_BOUND ( 'NONE', #46564, .T. ) ;
#33674 = CARTESIAN_POINT ( 'NONE',  ( -1.199500263597274685, -79.94791666666668561, 0.9218200799623673669 ) ) ;
#33675 = CARTESIAN_POINT ( 'NONE',  ( -11.19989528650999944, -78.82951613320700801, 0.6168112860373000661 ) ) ;
#33676 = EDGE_LOOP ( 'NONE', ( #53337, #32146, #56406, #38708 ) ) ;
#33677 = CARTESIAN_POINT ( 'NONE',  ( 2.147427714508652663, -78.16044680869335082, 11.59697916390112837 ) ) ;
#33678 = ORIENTED_EDGE ( 'NONE', *, *, #31831, .F. ) ;
#33679 = CARTESIAN_POINT ( 'NONE',  ( 7.482987909259383841, -77.40011310578455550, 5.437463058363716684 ) ) ;
#33680 = CARTESIAN_POINT ( 'NONE',  ( 1.160587285869999929, -77.85707335648099559, 10.97894289003999901 ) ) ;
#33681 = CARTESIAN_POINT ( 'NONE',  ( 3.895551333537116800, -77.19668379744932452, 10.51885396664144423 ) ) ;
#33682 = UNCERTAINTY_MEASURE_WITH_UNIT (LENGTH_MEASURE( 1.000000000000000082E-05 ), #11401, 'distance_accuracy_value', 'NONE');
#33683 = CARTESIAN_POINT ( 'NONE',  ( -0.6374375075192000306, -78.51479484294699773, 1.266385724874999896 ) ) ;
#33684 = CARTESIAN_POINT ( 'NONE',  ( 0.000000000000000000, -75.15999999999999659, 0.000000000000000000 ) ) ;
#33685 = CARTESIAN_POINT ( 'NONE',  ( 8.596418555780418913, -80.80208333333334281, 6.606377239730356621 ) ) ;
#33686 = CARTESIAN_POINT ( 'NONE',  ( 0.1198033158700999995, -79.25796128845000510, 1.623056241665000066 ) ) ;
#33687 = CARTESIAN_POINT ( 'NONE',  ( -7.613962827179999948, -23.30639625649999758, 10.53101998747000145 ) ) ;
#33688 = CARTESIAN_POINT ( 'NONE',  ( -1.306188688584000168, -78.60863250589198969, -10.97140668998000024 ) ) ;
#33689 = SURFACE_SIDE_STYLE ('',( #15986 ) ) ;
#33690 = DIRECTION ( 'NONE',  ( 0.000000000000000000, 0.000000000000000000, -1.000000000000000000 ) ) ;
#33691 = CARTESIAN_POINT ( 'NONE',  ( -0.6679575896827999459, -84.31375945333499544, 3.481207230722999757 ) ) ;
#33692 = ORIENTED_EDGE ( 'NONE', *, *, #26215, .F. ) ;
#33693 = CARTESIAN_POINT ( 'NONE',  ( 8.871207433088001082, -78.68252314293499694, 8.146610743062000282 ) ) ;
#33694 = CARTESIAN_POINT ( 'NONE',  ( -0.8692139286044998636, -81.46779532827999049, -1.194008811194000153 ) ) ;
#33695 = CARTESIAN_POINT ( 'NONE',  ( 1.407066150998827370, -79.23556352264608904, -10.74982909488969973 ) ) ;
#33696 = CARTESIAN_POINT ( 'NONE',  ( 8.770451247185000909, -78.87574068541999850, 8.160602927202999624 ) ) ;
#33697 = CARTESIAN_POINT ( 'NONE',  ( -7.753900686131000697, -17.71068035545000185, 10.31980286348999876 ) ) ;
#33698 = CIRCLE ( 'NONE', #17688, 1.000000000000000000 ) ;
#33699 = CARTESIAN_POINT ( 'NONE',  ( 1.073843316271627879, -78.54527281979174802, 0.6870350484321460227 ) ) ;
#33700 = DIRECTION ( 'NONE',  ( 0.000000000000000000, 0.000000000000000000, -1.000000000000000000 ) ) ;
#33701 = CARTESIAN_POINT ( 'NONE',  ( 8.164054339978811470, -80.90669609449903987, 6.993313037839142154 ) ) ;
#33702 = CARTESIAN_POINT ( 'NONE',  ( -9.395661821092000210, -77.07430961238269163, 0.5765637145115000139 ) ) ;
#33703 = CARTESIAN_POINT ( 'NONE',  ( 1.667260628947000001, -55.59057987493000041, -12.49858003893000102 ) ) ;
#33704 = CARTESIAN_POINT ( 'NONE',  ( -10.94146508061000134, -77.46905714352298844, -1.409282183016999923 ) ) ;
#33705 = CARTESIAN_POINT ( 'NONE',  ( -10.06605292056000067, -80.49507241345030195, 4.209295221118999564 ) ) ;
#33706 = CARTESIAN_POINT ( 'NONE',  ( -1.068511653377071102, -81.19603045319907153, -0.6936404097926303081 ) ) ;
#33707 = EDGE_LOOP ( 'NONE', ( #56390, #30084 ) ) ;
#33708 = CARTESIAN_POINT ( 'NONE',  ( -6.650956564739962218, -78.62112206211111243, 9.738045520853518155 ) ) ;
#33709 = CARTESIAN_POINT ( 'NONE',  ( 1.801614160555000010, -60.18652261871999798, -12.59687422890000086 ) ) ;
#33710 = AXIS2_PLACEMENT_3D ( 'NONE', #31689, #45003, #4560 ) ;
#33711 = CARTESIAN_POINT ( 'NONE',  ( 0.000000000000000000, -75.00000000000000000, 7.200000000000000178 ) ) ;
#33712 = EDGE_CURVE ( 'NONE', #16171, #9567, #19255, .T. ) ;
#33713 = CARTESIAN_POINT ( 'NONE',  ( -11.21668965365999959, -77.76655350871099870, -0.06311738993059998193 ) ) ;
#33714 = CARTESIAN_POINT ( 'NONE',  ( 4.038786804788999873, -79.52483602375698979, -10.20549938643999965 ) ) ;
#33715 = AXIS2_PLACEMENT_3D ( 'NONE', #36175, #54192, #31131 ) ;
#33716 = CARTESIAN_POINT ( 'NONE',  ( 10.18127202938000053, -23.38645218951999993, -7.633406483298000644 ) ) ;
#33717 = EDGE_CURVE ( 'NONE', #40044, #39806, #1360, .T. ) ;
#33718 = CARTESIAN_POINT ( 'NONE',  ( -1.046437039839534400, -85.88802085068084580, 3.873386318261602401 ) ) ;
#33719 = CARTESIAN_POINT ( 'NONE',  ( 11.65000000000000036, -76.00000000000000000, 0.000000000000000000 ) ) ;
#33720 = CARTESIAN_POINT ( 'NONE',  ( 5.954976958736712511, -78.53219957205278945, 10.12882962619908866 ) ) ;
#33721 = CARTESIAN_POINT ( 'NONE',  ( -7.624341766639000539, -23.26485146254000114, -10.42531125024000005 ) ) ;
#33722 = ORIENTED_EDGE ( 'NONE', *, *, #53604, .T. ) ;
#33723 = CARTESIAN_POINT ( 'NONE',  ( -7.000000000000000000, -80.99999999999998579, 0.000000000000000000 ) ) ;
#33724 = CIRCLE ( 'NONE', #14840, 11.05000000000000071 ) ;
#33725 = CARTESIAN_POINT ( 'NONE',  ( -9.009247259181924150, -78.02083333333332860, -2.421167930323337991 ) ) ;
#33726 = CARTESIAN_POINT ( 'NONE',  ( 10.24618685648000138, -78.46331089110499590, 4.684505231889000143 ) ) ;
#33727 = CARTESIAN_POINT ( 'NONE',  ( -3.140974612311351777, -76.90416666666665435, -11.68767212001978884 ) ) ;
#33728 = DIRECTION ( 'NONE',  ( 0.000000000000000000, -1.000000000000000000, 0.000000000000000000 ) ) ;
#33729 = CARTESIAN_POINT ( 'NONE',  ( -7.686941364987999847, -57.04527982297999955, -10.48774103564000093 ) ) ;
#33730 = CARTESIAN_POINT ( 'NONE',  ( 1.546414444450387116, -82.60036552312749336, 0.02810878433797979817 ) ) ;
#33731 = CARTESIAN_POINT ( 'NONE',  ( -0.7497356048005754392, -79.67399901261697437, -1.001289280827892370 ) ) ;
#33732 = ADVANCED_FACE ( 'NONE', ( #44151 ), #29679, .F. ) ;
#33733 = CARTESIAN_POINT ( 'NONE',  ( -1.250000000000000000, -81.09999999999999432, 0.000000000000000000 ) ) ;
#33734 = ORIENTED_EDGE ( 'NONE', *, *, #4570, .F. ) ;
#33735 = CARTESIAN_POINT ( 'NONE',  ( 1.667917367010000040, -18.71943307332999851, 12.49306752634999995 ) ) ;
#33736 =( LENGTH_UNIT ( ) NAMED_UNIT ( * ) SI_UNIT ( .MILLI., .METRE. ) );
#33737 = CARTESIAN_POINT ( 'NONE',  ( -12.61271904360000029, -23.19692351046000311, 1.798332623270999964 ) ) ;
#33738 = ORIENTED_EDGE ( 'NONE', *, *, #10077, .F. ) ;
#33739 = VERTEX_POINT ( 'NONE', #47729 ) ;
#33740 = CARTESIAN_POINT ( 'NONE',  ( -12.54977952612999914, -53.75167110003000204, 0.03756586072996999370 ) ) ;
#33741 = VERTEX_POINT ( 'NONE', #35859 ) ;
#33742 = CARTESIAN_POINT ( 'NONE',  ( 3.089230661516983556, -79.90117923447624548, -9.040938033382255767 ) ) ;
#33743 = ORIENTED_EDGE ( 'NONE', *, *, #29620, .F. ) ;
#33744 = CARTESIAN_POINT ( 'NONE',  ( 0.005523896503811000225, -16.93036543774000080, 12.55021156880999911 ) ) ;
#33745 = CARTESIAN_POINT ( 'NONE',  ( -6.700596268546000545, -78.14582039176799810, -8.618433365121999756 ) ) ;
#33746 = CARTESIAN_POINT ( 'NONE',  ( 1.750000000001000089, -60.05000000958000328, 12.56594317859000043 ) ) ;
#33747 = ADVANCED_FACE ( 'NONE', ( #27579 ), #16406, .F. ) ;
#33748 = CARTESIAN_POINT ( 'NONE',  ( -9.067070616629999691, -79.16216332859900717, 3.715721191563000403 ) ) ;
#33749 = CARTESIAN_POINT ( 'NONE',  ( -1.780884232981000181, -79.81062908972909042, -11.07459082487999957 ) ) ;
#33750 = EDGE_LOOP ( 'NONE', ( #30006, #23606, #14871, #32421, #6819 ) ) ;
#33751 = EDGE_LOOP ( 'NONE', ( #19017, #37156, #50098, #27860 ) ) ;
#33752 = CARTESIAN_POINT ( 'NONE',  ( -8.796452690798227891, -77.57500652429015986, 2.860862753174310491 ) ) ;
#33753 = CARTESIAN_POINT ( 'NONE',  ( -10.07627163191000008, -18.75000000240999753, 7.601397897754999633 ) ) ;
#33754 = CARTESIAN_POINT ( 'NONE',  ( -12.54980660771999901, -61.84777352133000505, 0.05651102257804999779 ) ) ;
#33755 = CARTESIAN_POINT ( 'NONE',  ( 9.512131559252001267, -78.00399131807598962, -1.920953556448999899 ) ) ;
#33756 = AXIS2_PLACEMENT_3D ( 'NONE', #5395, #18691, #36684 ) ;
#33757 = CARTESIAN_POINT ( 'NONE',  ( 9.164385193176935118, -62.01567483104246037, 8.803702037067671071 ) ) ;
#33758 = CARTESIAN_POINT ( 'NONE',  ( 1.750000000000000000, -21.74977139337000054, 12.65375411739000100 ) ) ;
#33759 = CARTESIAN_POINT ( 'NONE',  ( 1.387435826181647514, -77.43417277704999435, -11.96237581351085844 ) ) ;
#33760 = CARTESIAN_POINT ( 'NONE',  ( -0.9181250412607999678, -79.84966061487999411, -1.434176897702999831 ) ) ;
#33761 = CARTESIAN_POINT ( 'NONE',  ( -0.6295237254636235624, -81.08333333333332860, -1.092232985442822990 ) ) ;
#33762 = CARTESIAN_POINT ( 'NONE',  ( -4.005222689013000270, -81.61342682855999442, 1.168223800990999983 ) ) ;
#33763 = CARTESIAN_POINT ( 'NONE',  ( -9.770419344647999438, -53.74469452534000169, 8.292776877908002220 ) ) ;
#33764 = CARTESIAN_POINT ( 'NONE',  ( 5.381001269034999979, -79.11539666193300491, -7.930497238065998822 ) ) ;
#33765 = CARTESIAN_POINT ( 'NONE',  ( 2.813981643250826004, -76.74597719254359163, -10.47041296866918891 ) ) ;
#33766 = CARTESIAN_POINT ( 'NONE',  ( -7.658900723009000266, -18.79059707833999937, -10.01676258974000078 ) ) ;
#33768 = CARTESIAN_POINT ( 'NONE',  ( 2.062312494845999655, -18.77284340107000205, -12.83634740209000036 ) ) ;
#33767 = DIRECTION ( 'NONE',  ( -1.000000000000000000, 0.000000000000000000, 0.000000000000000000 ) ) ;
#33769 = CARTESIAN_POINT ( 'NONE',  ( 0.4254080272216657077, -1.236984628861461655, -3.253004618393738223 ) ) ;
#33770 = CARTESIAN_POINT ( 'NONE',  ( 5.442928436726999664, -80.32760589224999137, 9.767578386100000287 ) ) ;
#33771 = DIRECTION ( 'NONE',  ( 0.000000000000000000, -1.000000000000000000, 0.000000000000000000 ) ) ;
#33772 = CYLINDRICAL_SURFACE ( 'NONE', #33665, 9.500000000000000000 ) ;
#33773 = CARTESIAN_POINT ( 'NONE',  ( 0.9972398994228051095, -0.8977338377876618036, -3.382366038698053412 ) ) ;
#33774 = ORIENTED_EDGE ( 'NONE', *, *, #16691, .T. ) ;
#33775 = CARTESIAN_POINT ( 'NONE',  ( 1.750000000000000000, -55.55000000278000272, 12.50000000000000000 ) ) ;
#33776 = CARTESIAN_POINT ( 'NONE',  ( 9.837774000986101441, -17.68535604389086657, -7.850041800329745634 ) ) ;
#33777 = CARTESIAN_POINT ( 'NONE',  ( 1.235246655398537730, -78.36231938546748665, 0.1914569952463864855 ) ) ;
#33778 = CARTESIAN_POINT ( 'NONE',  ( -0.09167600787266001749, -79.76881872134099183, 9.642089308184999652 ) ) ;
#33779 = CARTESIAN_POINT ( 'NONE',  ( 2.600000000000000089, -77.49999999999998579, 0.000000000000000000 ) ) ;
#33780 = EDGE_CURVE ( 'NONE', #22759, #46129, #6057, .T. ) ;
#33781 = CARTESIAN_POINT ( 'NONE',  ( 1.288488638071999981, -61.33564939335000332, 12.54709296486000092 ) ) ;
#33782 = CARTESIAN_POINT ( 'NONE',  ( 1.571200994964738085, -79.46334789937733944, 10.64531129885916094 ) ) ;
#33783 = AXIS2_PLACEMENT_3D ( 'NONE', #57718, #48876, #13424 ) ;
#33784 = CARTESIAN_POINT ( 'NONE',  ( 0.000000000000000000, -76.75499999999999545, 0.000000000000000000 ) ) ;
#33785 = CARTESIAN_POINT ( 'NONE',  ( 3.999999999999605649, -78.67389998729011324, 2.360693471584012659 ) ) ;
#33786 = CARTESIAN_POINT ( 'NONE',  ( 10.75070227408000001, -78.04375343946199450, -1.791407170491000178 ) ) ;
#33787 = CARTESIAN_POINT ( 'NONE',  ( 9.724363994122649402, -76.40209226852219615, -6.594912342232487568 ) ) ;
#33788 = CARTESIAN_POINT ( 'NONE',  ( 10.69210609810000001, -77.98167474757299544, 3.151740433137000252 ) ) ;
#33789 = CARTESIAN_POINT ( 'NONE',  ( -5.764562846862999912, -79.07549514476063734, 7.830301022820999712 ) ) ;
#33790 = CARTESIAN_POINT ( 'NONE',  ( 0.08523424779968000187, -79.45900909512999988, -1.572136285807000045 ) ) ;
#33791 = CARTESIAN_POINT ( 'NONE',  ( 7.958763982157000427, -54.32301960771999916, 9.723170657500999070 ) ) ;
#33792 = CARTESIAN_POINT ( 'NONE',  ( -8.650571159592999493, -79.47494415034599058, 4.057379972786000266 ) ) ;
#33793 = CARTESIAN_POINT ( 'NONE',  ( 0.000000000000000000, -23.15000000000000213, 12.00000000000000000 ) ) ;
#33794 = CARTESIAN_POINT ( 'NONE',  ( 1.199500263597268246, -81.30208333333334281, 0.9218200799623752495 ) ) ;
#33795 = CARTESIAN_POINT ( 'NONE',  ( -10.35486996921426517, -76.19583333330172081, 5.986144667812050457 ) ) ;
#33796 = CARTESIAN_POINT ( 'NONE',  ( -3.708203932498999933, -79.79999999999999716, 11.41267819554000162 ) ) ;
#33797 = AXIS2_PLACEMENT_3D ( 'NONE', #846, #5247, #37110 ) ;
#33798 = EDGE_CURVE ( 'NONE', #57837, #5962, #47007, .T. ) ;
#33799 = CARTESIAN_POINT ( 'NONE',  ( 9.785129497364000173, -79.40228377048700281, -6.997026981537000090 ) ) ;
#33800 = LINE ( 'NONE', #1096, #5757 ) ;
#33801 = CARTESIAN_POINT ( 'NONE',  ( 0.000000000000000000, -75.19999999999998863, 0.000000000000000000 ) ) ;
#33802 = ORIENTED_EDGE ( 'NONE', *, *, #30941, .T. ) ;
#33803 = CARTESIAN_POINT ( 'NONE',  ( -11.57073820100000106, -77.60370790967400012, 2.924640136927000089 ) ) ;
#33804 = ORIENTED_EDGE ( 'NONE', *, *, #16020, .F. ) ;
#33805 = ORIENTED_EDGE ( 'NONE', *, *, #50522, .F. ) ;
#33806 = CARTESIAN_POINT ( 'NONE',  ( 10.75000000000000000, -78.75000000000000000, 0.000000000000000000 ) ) ;
#33807 = CARTESIAN_POINT ( 'NONE',  ( -7.220923959705244144, -77.37291666666664014, -9.396085398178621872 ) ) ;
#33808 = ADVANCED_FACE ( 'NONE', ( #46133 ), #7916, .F. ) ;
#33809 = CARTESIAN_POINT ( 'NONE',  ( 3.383036022311000313, -82.46144529440799431, 0.3412540027450999824 ) ) ;
#33810 = CARTESIAN_POINT ( 'NONE',  ( 8.810121547015370425, -79.18024560760937902, 3.560590676149650413 ) ) ;
#33811 = EDGE_LOOP ( 'NONE', ( #50546, #10173, #24687, #18782, #25030 ) ) ;
#33812 = DIRECTION ( 'NONE',  ( 0.000000000000000000, 1.000000000000000000, 0.000000000000000000 ) ) ;
#33813 = ORIENTED_EDGE ( 'NONE', *, *, #58046, .F. ) ;
#33814 = CARTESIAN_POINT ( 'NONE',  ( -0.4143223953128999937, -2.940338749271000029, 3.376050216419999916 ) ) ;
#33815 = VERTEX_POINT ( 'NONE', #13570 ) ;
#33816 = LINE ( 'NONE', #47437, #30877 ) ;
#33817 = CARTESIAN_POINT ( 'NONE',  ( 0.02654131748702290294, -78.62385949634384019, 1.533359335126560863 ) ) ;
#33818 = CARTESIAN_POINT ( 'NONE',  ( -9.151116546556963272, -79.79999999999999716, -7.636046516761507696 ) ) ;
#33819 = CARTESIAN_POINT ( 'NONE',  ( -6.095795872867655341, -80.02337930389114717, 8.857137469015752274 ) ) ;
#33820 = AXIS2_PLACEMENT_3D ( 'NONE', #43432, #3847, #57293 ) ;
#33821 = CARTESIAN_POINT ( 'NONE',  ( -1.473730639944037524, -86.36264282632897960, -3.227832877233638431 ) ) ;
#33823 = EDGE_CURVE ( 'NONE', #58122, #15888, #38972, .T. ) ;
#33822 = CARTESIAN_POINT ( 'NONE',  ( 7.486068761172999686, -76.01845923541398520, -8.059700645992000645 ) ) ;
#33824 = DIRECTION ( 'NONE',  ( 0.000000000000000000, 1.000000000000000000, 0.000000000000000000 ) ) ;
#33825 = CARTESIAN_POINT ( 'NONE',  ( 9.208765611215513402, -77.12463919408332913, 2.957848825889281219 ) ) ;
#33826 = ADVANCED_FACE ( 'NONE', ( #39845 ), #17415, .F. ) ;
#33827 = CARTESIAN_POINT ( 'NONE',  ( 9.715343368859999273, -76.10078336855899295, -5.397362455191000663 ) ) ;
#33828 = CARTESIAN_POINT ( 'NONE',  ( -3.523190925713206578, -78.69400124385185791, -8.552690850126060340 ) ) ;
#33829 = CARTESIAN_POINT ( 'NONE',  ( -8.843810886990000952, -77.47671167140099158, 3.524029368129000250 ) ) ;
#33830 = CARTESIAN_POINT ( 'NONE',  ( 1.021809889922000059, -79.37257489745699957, -0.8570204080543000202 ) ) ;
#33831 = CARTESIAN_POINT ( 'NONE',  ( -10.87293685240500984, -80.11224519801238841, -1.667451285520860305 ) ) ;
#33832 = CARTESIAN_POINT ( 'NONE',  ( -12.60356226360999798, -56.04922971106000062, -1.750000000000000000 ) ) ;
#33833 = CARTESIAN_POINT ( 'NONE',  ( -3.522214246756000033, -78.55792549782628953, -0.6909427624360000575 ) ) ;
#33834 = CARTESIAN_POINT ( 'NONE',  ( -5.069472984156999651, -79.91866724859939097, 10.81386965974999903 ) ) ;
#33835 = CARTESIAN_POINT ( 'NONE',  ( -10.54437012725677647, -78.08449553974310220, 2.092245762801656639 ) ) ;
#33836 = AXIS2_PLACEMENT_3D ( 'NONE', #10023, #1179, #5291 ) ;
#33837 = CARTESIAN_POINT ( 'NONE',  ( 0.2140083157829042182, -82.96156039968620632, 1.231433140267152115 ) ) ;
#33838 = CARTESIAN_POINT ( 'NONE',  ( 1.939913477021999899, -82.74324735065199832, 2.966757473053999838 ) ) ;
#33839 = CARTESIAN_POINT ( 'NONE',  ( -7.046594079837121605, -76.27358058460355039, -9.403470532666203141 ) ) ;
#33840 = CARTESIAN_POINT ( 'NONE',  ( -7.601397897754999633, -23.24999999688999708, -10.07627163191000008 ) ) ;
#33841 = CARTESIAN_POINT ( 'NONE',  ( -7.943805570375999991, -61.23402324491999593, -9.641149735098998974 ) ) ;
#33842 = CARTESIAN_POINT ( 'NONE',  ( -2.486604901413195901, -78.29583333333336270, 9.252740428348989354 ) ) ;
#33843 = CARTESIAN_POINT ( 'NONE',  ( 0.9432352957733999288, -81.94682085214100198, 0.9428059748164999698 ) ) ;
#33844 = CARTESIAN_POINT ( 'NONE',  ( -12.72554264791999934, -18.79839278105999867, -1.930240062458999928 ) ) ;
#33845 = CARTESIAN_POINT ( 'NONE',  ( 12.66008999772000010, -24.62705329347999950, 1.387101471715999956 ) ) ;
#33846 = EDGE_CURVE ( 'NONE', #1255, #51686, #1413, .T. ) ;
#33847 = CARTESIAN_POINT ( 'NONE',  ( -9.745349999783975647, -77.98553474052145873, -4.591900818727150835 ) ) ;
#33848 = DIRECTION ( 'NONE',  ( -1.000000000000000000, 0.000000000000000000, 0.000000000000000000 ) ) ;
#33849 = CARTESIAN_POINT ( 'NONE',  ( 6.083963560182001018, -78.52175463664858057, -9.135064530700001129 ) ) ;
#33850 = CARTESIAN_POINT ( 'NONE',  ( 4.978310723272000082, -76.73944210185999282, -11.31553633254000069 ) ) ;
#33851 = ORIENTED_EDGE ( 'NONE', *, *, #32009, .T. ) ;
#33852 = LINE ( 'NONE', #48050, #32359 ) ;
#33853 = CARTESIAN_POINT ( 'NONE',  ( 10.42531125072000009, -55.53514854654000032, 7.624341767124000135 ) ) ;
#33854 = CARTESIAN_POINT ( 'NONE',  ( 9.444446661605001125, -78.97637553138000044, 8.397347097585999620 ) ) ;
#33855 = CARTESIAN_POINT ( 'NONE',  ( -2.062597299672999540, -19.21514526754999963, -12.87022657274000004 ) ) ;
#33856 = CARTESIAN_POINT ( 'NONE',  ( 7.282635111839001141, -77.63697173280098696, 6.467064367534000269 ) ) ;
#33857 = CARTESIAN_POINT ( 'NONE',  ( 4.171544725960999678, -82.46507062100899077, -0.06562968391973000859 ) ) ;
#33858 = DIRECTION ( 'NONE',  ( 0.000000000000000000, 0.000000000000000000, -1.000000000000000000 ) ) ;
#33859 = CARTESIAN_POINT ( 'NONE',  ( 0.000000000000000000, -75.67500000000001137, 0.000000000000000000 ) ) ;
#33860 = ORIENTED_EDGE ( 'NONE', *, *, #21693, .T. ) ;
#33861 = DIRECTION ( 'NONE',  ( -1.000000000000000000, 0.000000000000000000, 0.000000000000000000 ) ) ;
#33862 = DIRECTION ( 'NONE',  ( 0.000000000000000000, 1.000000000000000000, 0.000000000000000000 ) ) ;
#33863 = CARTESIAN_POINT ( 'NONE',  ( 7.601397897754999633, -23.24999999758999536, -10.07627163191000008 ) ) ;
#33864 = ORIENTED_EDGE ( 'NONE', *, *, #2842, .F. ) ;
#33865 = CARTESIAN_POINT ( 'NONE',  ( 0.1443438050804999873, -78.00070911552320752, 1.325798245762999983 ) ) ;
#33866 = CARTESIAN_POINT ( 'NONE',  ( 8.926269970182000080, -78.50678530967299196, -6.511497375149000177 ) ) ;
#33867 = CARTESIAN_POINT ( 'NONE',  ( 6.277107794117254613, -78.83005409785420170, 10.03091776325296891 ) ) ;
#33868 = ORIENTED_EDGE ( 'NONE', *, *, #37309, .F. ) ;
#33869 = CARTESIAN_POINT ( 'NONE',  ( 4.570427068259999892, -77.67124252579399979, 11.39767413300000065 ) ) ;
#33870 = CARTESIAN_POINT ( 'NONE',  ( -10.99954758021000067, -77.53789446037799848, 2.683689935402000071 ) ) ;
#33871 = AXIS2_PLACEMENT_3D ( 'NONE', #44111, #40254, #3661 ) ;
#33872 = VERTEX_POINT ( 'NONE', #13788 ) ;
#33873 = ORIENTED_EDGE ( 'NONE', *, *, #28413, .F. ) ;
#33874 = CIRCLE ( 'NONE', #27260, 1.000000000000000000 ) ;
#33875 = CARTESIAN_POINT ( 'NONE',  ( -0.8843139287876815580, -80.53818017118156547, 0.8829188658367019826 ) ) ;
#33876 = ADVANCED_FACE ( 'NONE', ( #32086 ), #45995, .F. ) ;
#33877 = CARTESIAN_POINT ( 'NONE',  ( 10.75040930116792204, -77.83963288239696965, -1.407121311787697948 ) ) ;
#33878 = CARTESIAN_POINT ( 'NONE',  ( 3.366547962069000199, -79.78316274281900178, -9.168809063548000182 ) ) ;
#33879 = ORIENTED_EDGE ( 'NONE', *, *, #18203, .F. ) ;
#33880 = CARTESIAN_POINT ( 'NONE',  ( -12.71759155191110757, -24.06493881575022087, -1.809604648260982662 ) ) ;
#33881 = CARTESIAN_POINT ( 'NONE',  ( -0.2230286467304000153, -78.19680123892500490, -10.77282081049999896 ) ) ;
#33882 = ADVANCED_FACE ( 'NONE', ( #50713 ), #50455, .T. ) ;
#33883 = ORIENTED_EDGE ( 'NONE', *, *, #54248, .T. ) ;
#33884 = CARTESIAN_POINT ( 'NONE',  ( -0.2976406553997369420, -79.25604966714371358, -1.238856423539541840 ) ) ;
#33885 = CARTESIAN_POINT ( 'NONE',  ( -6.013262726775999489, -77.43941915034599788, 7.348341287529000176 ) ) ;
#33886 = CARTESIAN_POINT ( 'NONE',  ( 9.346058021984571695, -16.83471832412213232, -8.620905970628376380 ) ) ;
#33887 = CARTESIAN_POINT ( 'NONE',  ( -0.1963495408493673156, -81.28541666666667709, 1.499999999999999556 ) ) ;
#33888 = CARTESIAN_POINT ( 'NONE',  ( 5.395886906468551736, -77.87470926922809156, 7.541113365569439786 ) ) ;
#33889 = CARTESIAN_POINT ( 'NONE',  ( -8.912837724143001239, -77.08455291172688817, 3.724768546731999752 ) ) ;
#33890 = EDGE_CURVE ( 'NONE', #42976, #35609, #27369, .T. ) ;
#33891 = CARTESIAN_POINT ( 'NONE',  ( -10.98362417419999915, -18.84999999999999787, 0.5999999999999999778 ) ) ;
#33892 = CARTESIAN_POINT ( 'NONE',  ( -3.942583242386946019, -81.74479167956226888, -0.7493896997992520737 ) ) ;
#33893 = CARTESIAN_POINT ( 'NONE',  ( -8.194866293440998817, -24.71043252651000088, 9.389192598794000588 ) ) ;
#33894 = CARTESIAN_POINT ( 'NONE',  ( 0.5575618792808999524, -79.12582046129089974, -4.134693037866999710 ) ) ;
#33895 = CARTESIAN_POINT ( 'NONE',  ( -9.250000000000000000, -77.99999999999998579, 0.000000000000000000 ) ) ;
#33896 = DIRECTION ( 'NONE',  ( 0.000000000000000000, -1.000000000000000000, 0.000000000000000000 ) ) ;
#33897 = DIRECTION ( 'NONE',  ( 0.000000000000000000, 1.000000000000000000, 1.740029764579000277E-14 ) ) ;
#33898 = CARTESIAN_POINT ( 'NONE',  ( 0.03250568004163000707, -75.94088557671300066, 11.74995503739000036 ) ) ;
#33899 = SHAPE_REPRESENTATION ( 'Push Button', ( #43526 ), #52000 ) ;
#33900 = FACE_OUTER_BOUND ( 'NONE', #28432, .T. ) ;
#33901 = CARTESIAN_POINT ( 'NONE',  ( -9.416161903791310905, -77.49611799111114863, 7.561431734142661121 ) ) ;
#33902 = CARTESIAN_POINT ( 'NONE',  ( 10.48543666025110710, -78.00833333333332575, -6.043427764450776785 ) ) ;
#33903 = EDGE_LOOP ( 'NONE', ( #37234, #42258, #17596, #25436, #9935, #29801 ) ) ;
#33904 = CARTESIAN_POINT ( 'NONE',  ( 0.9943715457052075823, -80.93213777880458792, -1.136342727594208402 ) ) ;
#33905 = FACE_OUTER_BOUND ( 'NONE', #16618, .T. ) ;
#33906 = LINE ( 'NONE', #15342, #11608 ) ;
#33907 = VECTOR ( 'NONE', #39102, 1000.000000000000000 ) ;
#33908 = CARTESIAN_POINT ( 'NONE',  ( 0.9218200799623742503, -78.67708333333332860, -1.199500263597268912 ) ) ;
#33909 = ADVANCED_FACE ( 'NONE', ( #53226 ), #57903, .F. ) ;
#33910 = CARTESIAN_POINT ( 'NONE',  ( 3.334892075843000292, -2.746854981583999766, 1.239339612286000092 ) ) ;
#33911 = TOROIDAL_SURFACE ( 'NONE', #5644, 8.500000000000000000, 2.000000000000000000 ) ;
#33912 = CARTESIAN_POINT ( 'NONE',  ( -11.68231536908000123, -77.48916203849999818, 2.952842578158000109 ) ) ;
#33913 = DIRECTION ( 'NONE',  ( 0.000000000000000000, 1.000000000000000000, 0.000000000000000000 ) ) ;
#33915 = CARTESIAN_POINT ( 'NONE',  ( 10.21045785712752796, -76.85731980684688835, -5.980552670349623234 ) ) ;
#33914 = CARTESIAN_POINT ( 'NONE',  ( -8.511625900046547955, -76.13945263819573483, 8.102560346989390538 ) ) ;
#33916 = CARTESIAN_POINT ( 'NONE',  ( -8.824204240651999598, -79.07668513919199427, -6.427191105727000142 ) ) ;
#33917 = CARTESIAN_POINT ( 'NONE',  ( -10.03645592992567792, -79.57090332437941527, 3.852638260147155602 ) ) ;
#33918 = ORIENTED_EDGE ( 'NONE', *, *, #54164, .T. ) ;
#33919 = DIRECTION ( 'NONE',  ( 1.000000000000000000, 0.000000000000000000, 0.000000000000000000 ) ) ;
#33920 = CARTESIAN_POINT ( 'NONE',  ( 9.438973017186889081, -79.48883391750764815, -1.335242394275343081 ) ) ;
#33921 = CARTESIAN_POINT ( 'NONE',  ( 1.636761686205415067, -2.333333333333333037, 2.839805762151342616 ) ) ;
#33922 = CARTESIAN_POINT ( 'NONE',  ( -7.646966600034999395, -59.99642081684000061, 10.19019745249000053 ) ) ;
#33923 = CARTESIAN_POINT ( 'NONE',  ( -0.5050702100269550687, -79.19199393167497192, -1.144170159917196727 ) ) ;
#33924 = CARTESIAN_POINT ( 'NONE',  ( 3.000000000000000000, -86.20000000000000284, 0.000000000000000000 ) ) ;
#33925 = CARTESIAN_POINT ( 'NONE',  ( 1.480558193255000043, -79.50583043005198647, 9.556295997439999468 ) ) ;
#33926 = DIRECTION ( 'NONE',  ( 0.000000000000000000, -1.000000000000000000, 0.000000000000000000 ) ) ;
#33927 = CARTESIAN_POINT ( 'NONE',  ( -2.879226727952072018, -78.70416666666666572, -10.71369944335147295 ) ) ;
#33928 = ORIENTED_EDGE ( 'NONE', *, *, #27766, .F. ) ;
#33929 = EDGE_CURVE ( 'NONE', #21876, #41938, #15034, .T. ) ;
#33930 = CARTESIAN_POINT ( 'NONE',  ( 10.97564558566000059, -79.04457588320700268, 2.523721168482999655 ) ) ;
#33931 = CARTESIAN_POINT ( 'NONE',  ( -4.800269761346773301, -76.26018993196245788, 10.10126516968071719 ) ) ;
#33932 = CARTESIAN_POINT ( 'NONE',  ( -3.161392481395000065, -1.783292672027000147, -1.501864700490999960 ) ) ;
#33933 = CARTESIAN_POINT ( 'NONE',  ( -1.499934128473817241, -81.90004407876089942, 2.109063419893342596E-06 ) ) ;
#33935 = CARTESIAN_POINT ( 'NONE',  ( 1.172672253443726609, -81.37839855359489150, 0.4351029964937788708 ) ) ;
#33934 = CARTESIAN_POINT ( 'NONE',  ( -0.1812720377017000006, -81.77208891657700462, -1.306792278262000062 ) ) ;
#33936 = B_SPLINE_CURVE_WITH_KNOTS ( 'NONE', 3,
 ( #16348, #34328, #52363, #25479 ),
 .UNSPECIFIED., .F., .F.,
 ( 4, 4 ),
 ( 0.000000000000000000, 1.000000000000000000 ),
 .UNSPECIFIED. ) ;
#33937 = AXIS2_PLACEMENT_3D ( 'NONE', #20343, #38338, #56362 ) ;
#33938 = DIRECTION ( 'NONE',  ( 1.000000000000000000, 0.000000000000000000, 0.000000000000000000 ) ) ;
#33939 = CARTESIAN_POINT ( 'NONE',  ( 10.18499221076999994, -57.05022860182000244, -7.710118476618999850 ) ) ;
#33940 = CARTESIAN_POINT ( 'NONE',  ( 1.667917367065999912, -55.51943464808999806, -12.49306764013999960 ) ) ;
#33941 = CARTESIAN_POINT ( 'NONE',  ( 10.73640186359711102, -76.13322000874006790, -2.284131902630157196 ) ) ;
#33942 = DIRECTION ( 'NONE',  ( 1.000000000000000000, 0.000000000000000000, 0.000000000000000000 ) ) ;
#33943 = EDGE_CURVE ( 'NONE', #41659, #37958, #15699, .T. ) ;
#33944 = CARTESIAN_POINT ( 'NONE',  ( 8.944729675425000082, -79.49243891193700051, 3.923329690209000908 ) ) ;
#33945 = ORIENTED_EDGE ( 'NONE', *, *, #51117, .T. ) ;
#33946 = ORIENTED_EDGE ( 'NONE', *, *, #17624, .F. ) ;
#33947 = CARTESIAN_POINT ( 'NONE',  ( 6.829512357978999582, -77.43143009854699699, -9.995615053322000065 ) ) ;
#33948 = CARTESIAN_POINT ( 'NONE',  ( -4.666033688610307983, -78.68943876540365068, -9.684451540703740591 ) ) ;
#33949 = ADVANCED_FACE ( 'NONE', ( #37543 ), #1554, .T. ) ;
#33950 = ORIENTED_EDGE ( 'NONE', *, *, #20193, .F. ) ;
#33951 = CARTESIAN_POINT ( 'NONE',  ( 8.958657468039000094, -16.79887336309000290, 8.950049500644999156 ) ) ;
#33952 = AXIS2_PLACEMENT_3D ( 'NONE', #49766, #36165, #54185 ) ;
#33953 = CARTESIAN_POINT ( 'NONE',  ( -9.157651701204139627, -78.82306796249194747, 3.211112441314760257 ) ) ;
#33954 = VECTOR ( 'NONE', #23545, 1000.000000000000000 ) ;
#33955 = CARTESIAN_POINT ( 'NONE',  ( -10.26699006316252749, -75.84166666666666856, -5.917523019358070790 ) ) ;
#33956 = CARTESIAN_POINT ( 'NONE',  ( -10.42426601462999969, -77.61928380272000538, 7.425889537758000536 ) ) ;
#33957 = CARTESIAN_POINT ( 'NONE',  ( -9.393200444579274944, -79.64169496360098321, -5.413760864891401070 ) ) ;
#33958 = CARTESIAN_POINT ( 'NONE',  ( -8.485281374238999419, -23.25000000000000000, -8.485281374238999419 ) ) ;
#33959 = CARTESIAN_POINT ( 'NONE',  ( 5.137083998358000336, -77.21100733245999947, -10.56753840748999984 ) ) ;
#33960 = CARTESIAN_POINT ( 'NONE',  ( 4.782478426736999744, -79.67384276626299311, 10.14623135401999932 ) ) ;
#33961 = EDGE_CURVE ( 'NONE', #1186, #41874, #7033, .T. ) ;
#33962 = ORIENTED_EDGE ( 'NONE', *, *, #280, .F. ) ;
#33963 = CARTESIAN_POINT ( 'NONE',  ( 0.000000000000000000, -75.00000000000000000, 0.000000000000000000 ) ) ;
#33964 = ORIENTED_EDGE ( 'NONE', *, *, #2345, .T. ) ;
#33965 = CARTESIAN_POINT ( 'NONE',  ( 5.783621287653671672, -77.27891537691782275, -7.219593957272368634 ) ) ;
#33966 = CARTESIAN_POINT ( 'NONE',  ( 12.50240681836000078, -61.48234730679999416, -1.005418944265000114 ) ) ;
#33967 = CARTESIAN_POINT ( 'NONE',  ( 0.7681833999686451531, -83.17708333333330017, -0.9995835529977240563 ) ) ;
#33968 = DIRECTION ( 'NONE',  ( 0.7071067811865474617, -0.7071067811865474617, 4.376097137204291133E-09 ) ) ;
#33969 = CARTESIAN_POINT ( 'NONE',  ( -0.2558648464975999959, -78.71324533647100452, -1.394486488214999875 ) ) ;
#33970 = FACE_OUTER_BOUND ( 'NONE', #20474, .T. ) ;
#33971 = CARTESIAN_POINT ( 'NONE',  ( -10.36597025940959327, -18.22476146848570977, 7.635927901519359295 ) ) ;
#33972 = CARTESIAN_POINT ( 'NONE',  ( -1.491326706514000122, -77.86238728987000002, -0.6515838025032999470 ) ) ;
#33973 = FACE_OUTER_BOUND ( 'NONE', #32576, .T. ) ;
#33974 = CARTESIAN_POINT ( 'NONE',  ( 10.94849663375999960, -79.73232667919899086, -1.486040076422999956 ) ) ;
#33975 = CARTESIAN_POINT ( 'NONE',  ( 7.090970028742000331, -77.75223832859899176, 6.513691531324999673 ) ) ;
#33976 = CARTESIAN_POINT ( 'NONE',  ( -7.919595949288999570, -55.65000000488999632, -8.768124086549999419 ) ) ;
#33977 = CARTESIAN_POINT ( 'NONE',  ( 2.575543530473000331, -83.78155969446399354, -2.438881961842000123 ) ) ;
#33978 = AXIS2_PLACEMENT_3D ( 'NONE', #16603, #34590, #24880 ) ;
#33979 = ORIENTED_EDGE ( 'NONE', *, *, #39957, .F. ) ;
#33980 = CARTESIAN_POINT ( 'NONE',  ( -1.354012292646000093, -83.36889217614600511, -0.7194680089321999761 ) ) ;
#33981 = CARTESIAN_POINT ( 'NONE',  ( 0.7712594847575999779, -80.66762112988999434, 1.518214662813999860 ) ) ;
#33982 = CARTESIAN_POINT ( 'NONE',  ( -8.596154512980129780, -79.15224688203926462, -6.606175269931966909 ) ) ;
#33983 = CARTESIAN_POINT ( 'NONE',  ( -1.360213228908000005, -77.68205080677400076, -11.90234785270000017 ) ) ;
#33984 = CARTESIAN_POINT ( 'NONE',  ( -9.414496040451998837, -16.73736394015000073, 8.652369398713998905 ) ) ;
#33985 = CARTESIAN_POINT ( 'NONE',  ( 5.413694191244308840, -78.93348499250215866, 9.392869764965404045 ) ) ;
#33986 = CARTESIAN_POINT ( 'NONE',  ( 3.449524682386059471, -2.016339860153205876, 0.7156992932775020355 ) ) ;
#33987 = CARTESIAN_POINT ( 'NONE',  ( 10.74987353692243452, -80.85518448745408193, 0.6718904260645724991 ) ) ;
#33988 = CARTESIAN_POINT ( 'NONE',  ( 9.508660861234000450, -78.38883383484099454, -0.5057122284909000287 ) ) ;
#33989 = CARTESIAN_POINT ( 'NONE',  ( 1.691611010928999903, -54.56917308736999672, -12.66722148965999928 ) ) ;
#33990 = CARTESIAN_POINT ( 'NONE',  ( -10.37098203719999923, -77.98654766055700804, -3.760912916518000415 ) ) ;
#33991 = CARTESIAN_POINT ( 'NONE',  ( -13.89999999928999941, -5.999999999291000030, -8.437402497311000243E-09 ) ) ;
#33992 = DIRECTION ( 'NONE',  ( 1.000000000000000000, 0.000000000000000000, 0.000000000000000000 ) ) ;
#33993 = CARTESIAN_POINT ( 'NONE',  ( 1.256367437124104258, -81.38684823543385960, -0.2130951737473960883 ) ) ;
#33994 = ORIENTED_EDGE ( 'NONE', *, *, #17890, .F. ) ;
#33995 = DIRECTION ( 'NONE',  ( 1.000000000000000000, 0.000000000000000000, 0.000000000000000000 ) ) ;
#33996 = CARTESIAN_POINT ( 'NONE',  ( 1.666727925310000025, -59.99174481743000342, -12.50018462905999961 ) ) ;
#33997 = B_SPLINE_CURVE_WITH_KNOTS ( 'NONE', 3,
 ( #46996, #51418, #20968, #47287, #52561, #7680, #30098, #43134, #42841, #24824, #43411, #38684, #6815, #56704, #2399, #56416, #15965, #38973, #33957, #10975, #16261, #11549 ),
 .UNSPECIFIED., .F., .F.,
 ( 4, 2, 2, 2, 2, 2, 2, 2, 2, 2, 4 ),
 ( 0.000000000000000000, 0.1250000000000000000, 0.2500000000000000000, 0.3750000000000000000, 0.4375000000000000000, 0.5000000000000000000, 0.5625000000000000000, 0.6250000000000000000, 0.7500000000000000000, 0.8750000000000000000, 1.000000000000000000 ),
 .UNSPECIFIED. ) ;
#33998 = CARTESIAN_POINT ( 'NONE',  ( -3.962108358898298821, -78.54828561723799396, 0.07469349987780400657 ) ) ;
#33999 = CIRCLE ( 'NONE', #8538, 0.5000000000000006661 ) ;
#34000 = CARTESIAN_POINT ( 'NONE',  ( 9.070694317316998934, -78.06615328173100465, 6.598531290616000078 ) ) ;
#34001 = CARTESIAN_POINT ( 'NONE',  ( 10.85730540529999999, -79.13154306309999697, 1.607151491820999922 ) ) ;
#34002 = FACE_OUTER_BOUND ( 'NONE', #5864, .T. ) ;
#34003 = CARTESIAN_POINT ( 'NONE',  ( 3.315849953455010990, -84.09583333138887440, 2.328886385603761155 ) ) ;
#34004 = CARTESIAN_POINT ( 'NONE',  ( 11.80177567542000006, -76.84575795437399393, 2.898902813627999731 ) ) ;
#34005 = CARTESIAN_POINT ( 'NONE',  ( 11.00358534011910017, -78.47804174058605042, 4.128363279570725908 ) ) ;
#34006 = ORIENTED_EDGE ( 'NONE', *, *, #32080, .T. ) ;
#34007 = EDGE_CURVE ( 'NONE', #32937, #13151, #3028, .T. ) ;
#34008 = CONICAL_SURFACE ( 'NONE', #42535, 12.74999999937999995, 0.7853981633972997312 ) ;
#34009 = CARTESIAN_POINT ( 'NONE',  ( -1.163537450530989892, -80.07049513950991582, 0.4564699256384350257 ) ) ;
#34010 = CARTESIAN_POINT ( 'NONE',  ( -8.082524092276891281, -78.04166666666668561, -4.658475568430815450 ) ) ;
#34011 = ADVANCED_FACE ( 'NONE', ( #39287 ), #53188, .F. ) ;
#34012 = CARTESIAN_POINT ( 'NONE',  ( 9.550909342165001092, -78.88469620609498634, -5.975706243058000133 ) ) ;
#34013 = CARTESIAN_POINT ( 'NONE',  ( 6.043427764450807871, -76.96666666666666856, -10.48543666025108934 ) ) ;
#34014 = CARTESIAN_POINT ( 'NONE',  ( -1.817320609109999873E-14, -79.15000000008998882, 0.000000000000000000 ) ) ;
#34015 = CARTESIAN_POINT ( 'NONE',  ( -10.14948852600999984, -59.55100835476999777, 7.674614791855999485 ) ) ;
#34016 = CARTESIAN_POINT ( 'NONE',  ( -1.455028237381281730, -81.87158815977416282, -0.4162487262828510892 ) ) ;
#34017 = DIRECTION ( 'NONE',  ( 1.000000000000000000, 0.000000000000000000, 0.000000000000000000 ) ) ;
#34018 = ORIENTED_EDGE ( 'NONE', *, *, #14827, .F. ) ;
#34019 = CARTESIAN_POINT ( 'NONE',  ( 1.799490225533999732, -19.22847221992000044, 12.64500484465999897 ) ) ;
#34020 = CARTESIAN_POINT ( 'NONE',  ( -10.26699006316255591, -76.25833333333333997, 5.917523019358029934 ) ) ;
#34021 = EDGE_LOOP ( 'NONE', ( #30746, #29674, #18727, #50544 ) ) ;
#34022 = VERTEX_POINT ( 'NONE', #32161 ) ;
#34023 = CARTESIAN_POINT ( 'NONE',  ( -12.77649795258999887, -53.49168567723999956, 0.06462540730615000395 ) ) ;
#34024 = ADVANCED_FACE ( 'NONE', ( #28312 ), #41929, .T. ) ;
#34025 = ORIENTED_EDGE ( 'NONE', *, *, #45387, .F. ) ;
#34026 = ORIENTED_EDGE ( 'NONE', *, *, #34300, .F. ) ;
#34027 = CARTESIAN_POINT ( 'NONE',  ( -1.323062013136505399, -80.99999999999998579, -10.86425420506007633 ) ) ;
#34028 = CARTESIAN_POINT ( 'NONE',  ( -10.91657421154000041, -77.57385718872899361, -0.06142861151470999787 ) ) ;
#34029 = FACE_BOUND ( 'NONE', #12959, .T. ) ;
#34030 = CARTESIAN_POINT ( 'NONE',  ( -5.809342935555999787, -79.11861332859899676, 7.891128111295000025 ) ) ;
#34031 = CARTESIAN_POINT ( 'NONE',  ( 2.365362167656198888, -79.35465741588306798, 9.023513813972275699 ) ) ;
#34032 = EDGE_CURVE ( 'NONE', #58285, #11409, #5888, .T. ) ;
#34033 = ORIENTED_EDGE ( 'NONE', *, *, #16238, .T. ) ;
#34034 = ORIENTED_EDGE ( 'NONE', *, *, #48052, .F. ) ;
#34035 = CARTESIAN_POINT ( 'NONE',  ( -5.567379522523680180, -77.52644555432438267, 7.387118996003618321 ) ) ;
#34036 = CARTESIAN_POINT ( 'NONE',  ( 9.499999999999998224, -77.66166666666666174, 1.392772743091435617 ) ) ;
#34037 = ADVANCED_FACE ( 'NONE', ( #37770 ), #55791, .F. ) ;
#34038 = CARTESIAN_POINT ( 'NONE',  ( -12.61277705616999967, -59.99666672496000075, -1.798399175679000095 ) ) ;
#34039 = VECTOR ( 'NONE', #6682, 999.9999999999998863 ) ;
#34040 = CARTESIAN_POINT ( 'NONE',  ( -7.707166124622999881, -77.32181941897998456, -5.896629607976000109 ) ) ;
#34041 = CARTESIAN_POINT ( 'NONE',  ( 7.653559502275999016, -23.29849137228000444, 10.01234990228999955 ) ) ;
#34042 = DIRECTION ( 'NONE',  ( 0.000000000000000000, -1.000000000000000000, 0.000000000000000000 ) ) ;
#34043 = CARTESIAN_POINT ( 'NONE',  ( -10.53003236233000095, -18.67547726287999765, 7.612971540274999782 ) ) ;
#34044 = FACE_OUTER_BOUND ( 'NONE', #7947, .T. ) ;
#34045 = CARTESIAN_POINT ( 'NONE',  ( 0.7181780477660000273, -80.54425450742999715, 1.413724517075999998 ) ) ;
#34046 = CARTESIAN_POINT ( 'NONE',  ( -1.342463812738999916E-14, -80.70000000000000284, -13.99999999999935874 ) ) ;
#34047 = CARTESIAN_POINT ( 'NONE',  ( -9.414496040419999545, -53.53736393982000408, 8.652369398681999613 ) ) ;
#34048 = CARTESIAN_POINT ( 'NONE',  ( -3.403932870613000095, -78.34601332859899969, 9.307723658127001087 ) ) ;
#34049 = FACE_OUTER_BOUND ( 'NONE', #33211, .T. ) ;
#34050 = CARTESIAN_POINT ( 'NONE',  ( 1.931087888049999979, -18.68415522710999710, -12.71658889741000031 ) ) ;
#34052 = CARTESIAN_POINT ( 'NONE',  ( 13.94241845804000057, -32.46002936525999871, 4.312607202007000224E-05 ) ) ;
#34051 = CARTESIAN_POINT ( 'NONE',  ( 0.1963495408493571848, -78.76458333333334849, 1.500000000000000666 ) ) ;
#34053 = ADVANCED_FACE ( 'NONE', ( #54903 ), #34363, .F. ) ;
#34054 = CARTESIAN_POINT ( 'NONE',  ( 8.300970689365456678, -79.00833333333333997, -4.784380313523530326 ) ) ;
#34055 = CARTESIAN_POINT ( 'NONE',  ( 9.015520653554002450, -80.22846898612900191, 6.426785087202000035 ) ) ;
#34056 = CARTESIAN_POINT ( 'NONE',  ( -0.3713770062794000126, -82.23533397128800004, -1.193557338046999927 ) ) ;
#34057 = DIRECTION ( 'NONE',  ( 0.000000000000000000, 1.000000000000000000, 0.000000000000000000 ) ) ;
#34058 = CARTESIAN_POINT ( 'NONE',  ( 3.236072848700317639, -1.467564355532075648, -1.392980727198947166 ) ) ;
#34059 = B_SPLINE_CURVE_WITH_KNOTS ( 'NONE', 3,
 ( #5027, #9461, #40155, #41917, #20351, #33035, #10333, #1201, #20070, #15042, #28313, #42792, #24487, #11214, #37472, #50789, #2073, #38061 ),
 .UNSPECIFIED., .F., .F.,
 ( 4, 2, 2, 2, 2, 2, 2, 2, 4 ),
 ( 0.000000000000000000, 0.1249999999999999722, 0.2499999999999999445, 0.3749999999999998890, 0.4999999999999998890, 0.6249999999999998890, 0.7499999999999997780, 0.8749999999999998890, 1.000000000000000000 ),
 .UNSPECIFIED. ) ;
#34060 = ORIENTED_EDGE ( 'NONE', *, *, #14479, .T. ) ;
#34061 = CARTESIAN_POINT ( 'NONE',  ( -3.167843140252689427, -1.581004088418222597, 0.8520282484494562381 ) ) ;
#34062 = CARTESIAN_POINT ( 'NONE',  ( -12.50485692589189490, -24.86593462704853863, 0.6924071800263524867 ) ) ;
#34063 = CARTESIAN_POINT ( 'NONE',  ( 0.8798274126591324462, -78.41291895153544544, 0.8879370300962265983 ) ) ;
#34064 =( GEOMETRIC_REPRESENTATION_CONTEXT ( 3 ) GLOBAL_UNCERTAINTY_ASSIGNED_CONTEXT ( ( #28965 ) ) GLOBAL_UNIT_ASSIGNED_CONTEXT ( ( #28722, #15454, #38168 ) ) REPRESENTATION_CONTEXT ( 'NONE', 'WORKASPACE' ) );
#34065 = CARTESIAN_POINT ( 'NONE',  ( -7.482909773998999370, -79.44736948050399405, -6.081476139641999623 ) ) ;
#34066 = LINE ( 'NONE', #33779, #21520 ) ;
#34067 = CARTESIAN_POINT ( 'NONE',  ( -6.863219652448105279, -79.28723744505849425, 6.877600145842833967 ) ) ;
#34068 = CARTESIAN_POINT ( 'NONE',  ( -1.500000000000000222, -80.01041666666669983, -0.1963495408493622085 ) ) ;
#34069 = DIRECTION ( 'NONE',  ( 1.894056205636980548E-11, 1.538483569415980182E-07, -0.9999999999999882316 ) ) ;
#34070 = EDGE_CURVE ( 'NONE', #23434, #38752, #950, .T. ) ;
#34071 = FACE_OUTER_BOUND ( 'NONE', #20320, .T. ) ;
#34072 = ADVANCED_FACE ( 'NONE', ( #24043 ), #33023, .F. ) ;
#34073 = CARTESIAN_POINT ( 'NONE',  ( 3.992904449609000039, -78.62148118236264338, 2.356505866712913289 ) ) ;
#34074 = CARTESIAN_POINT ( 'NONE',  ( 0.9750215749860999814, -78.00291024847199139, -10.90431470505999911 ) ) ;
#34075 = CARTESIAN_POINT ( 'NONE',  ( 8.269121427749986708, -76.38708047178403149, -8.347674621122058269 ) ) ;
#34076 = CARTESIAN_POINT ( 'NONE',  ( 9.014158510551999015, -78.00891109057499762, 6.557403976990999972 ) ) ;
#34077 = CARTESIAN_POINT ( 'NONE',  ( 0.000000000000000000, -87.15000000002500258, -10.09999999997999964 ) ) ;
#34078 = CARTESIAN_POINT ( 'NONE',  ( 7.648026766733999615, -18.74999999413999774, 10.12290050089000104 ) ) ;
#34079 = CARTESIAN_POINT ( 'NONE',  ( 5.212684961665999595, -76.94014298669428342, -8.147089634514999901 ) ) ;
#34080 = CARTESIAN_POINT ( 'NONE',  ( 1.861092857305999937, -79.65044415034600434, -9.371850619045000386 ) ) ;
#34081 = CARTESIAN_POINT ( 'NONE',  ( -2.122304942052989585, -0.7955729038712460177, -2.762992850480189055 ) ) ;
#34082 = CARTESIAN_POINT ( 'NONE',  ( 7.653722864265482428, -80.28804818156974932, -7.548741967642948580 ) ) ;
#34083 = DIRECTION ( 'NONE',  ( 1.000000000000000000, 0.000000000000000000, 0.000000000000000000 ) ) ;
#34084 = CARTESIAN_POINT ( 'NONE',  ( 7.359053403517531677, -80.16684166704409620, 8.232126067569696559 ) ) ;
#34085 = VECTOR ( 'NONE', #54802, 1000.000000000000000 ) ;
#34086 = CARTESIAN_POINT ( 'NONE',  ( -5.092641036025000290, -79.40810352659100602, 10.89826376711000044 ) ) ;
#34087 = CARTESIAN_POINT ( 'NONE',  ( -0.1636246173744726473, -81.88541666666664298, 1.249999999999999112 ) ) ;
#34088 = CARTESIAN_POINT ( 'NONE',  ( -8.415968974905998934, -79.88124863702039136, -7.483677623529000122 ) ) ;
#34089 = EDGE_LOOP ( 'NONE', ( #14186, #18553, #37367, #56343 ) ) ;
#34090 = FACE_OUTER_BOUND ( 'NONE', #41221, .T. ) ;
#34091 = ORIENTED_EDGE ( 'NONE', *, *, #28006, .F. ) ;
#34092 = ORIENTED_EDGE ( 'NONE', *, *, #9937, .F. ) ;
#34093 = VERTEX_POINT ( 'NONE', #52943 ) ;
#34094 = CARTESIAN_POINT ( 'NONE',  ( 3.438062876453999994, -82.49041413704399872, -0.2266124004514999957 ) ) ;
#34095 = CARTESIAN_POINT ( 'NONE',  ( 4.321906625261624946, -79.23704788471283678, 8.459721384812338485 ) ) ;
#34096 = EDGE_LOOP ( 'NONE', ( #51423, #33646, #1671, #16583 ) ) ;
#34097 = CARTESIAN_POINT ( 'NONE',  ( -10.48774103543000180, -58.55472018357999531, -7.686941364784000363 ) ) ;
#34098 = CARTESIAN_POINT ( 'NONE',  ( -1.750000000000000000, -55.55000000209000177, 12.50000000000000000 ) ) ;
#34099 = ORIENTED_EDGE ( 'NONE', *, *, #48543, .T. ) ;
#34100 = CARTESIAN_POINT ( 'NONE',  ( 0.08254163500371779205, -79.47024897342303973, 1.249696854227522635 ) ) ;
#34101 = CARTESIAN_POINT ( 'NONE',  ( -1.433418477799210056, -78.77510440916314849, -0.4689554305704703996 ) ) ;
#34102 = DIRECTION ( 'NONE',  ( 0.7071067811865475727, 0.000000000000000000, -0.7071067811865475727 ) ) ;
#34103 = CARTESIAN_POINT ( 'NONE',  ( -10.21591591617042205, -80.07484147801372387, 3.346207656172486722 ) ) ;
#34104 = DIRECTION ( 'NONE',  ( -1.000000000000000000, 0.000000000000000000, 0.000000000000000000 ) ) ;
#34105 = CARTESIAN_POINT ( 'NONE',  ( -3.244210320986640639, -86.17851879815596305, -2.264204901133591186 ) ) ;
#34106 = CARTESIAN_POINT ( 'NONE',  ( 1.849737152796000039, -76.69567166912000289, 11.02961253862999946 ) ) ;
#34107 = CARTESIAN_POINT ( 'NONE',  ( 8.079871975571242260, -76.40862220706031849, 7.134473887754699817 ) ) ;
#34108 = CARTESIAN_POINT ( 'NONE',  ( -0.3725602292220764333, -81.24407571201139433, 1.466352916892600167 ) ) ;
#34109 = CARTESIAN_POINT ( 'NONE',  ( 10.90992603612999901, -76.12586531054799366, -2.119726332427000148 ) ) ;
#34110 = CARTESIAN_POINT ( 'NONE',  ( -6.269511089439802731, -78.66582854956671156, -6.801662962640114607 ) ) ;
#34111 = AXIS2_PLACEMENT_3D ( 'NONE', #19613, #28454, #1050 ) ;
#34112 = CARTESIAN_POINT ( 'NONE',  ( 10.25000000000000000, -87.20000000000000284, 0.000000000000000000 ) ) ;
#34113 = CARTESIAN_POINT ( 'NONE',  ( -7.596835002782738933, -77.24791666666669698, 5.838193839761661508 ) ) ;
#34114 = CARTESIAN_POINT ( 'NONE',  ( 2.314806860876999828, -81.92878455456799713, -2.958581976489000009 ) ) ;
#34115 = AXIS2_PLACEMENT_3D ( 'NONE', #50742, #6724, #15581 ) ;
#34116 = CARTESIAN_POINT ( 'NONE',  ( -9.563733257752160100, -78.06231107666935998, 4.912333404894130950 ) ) ;
#34117 = EDGE_CURVE ( 'NONE', #29449, #185, #37196, .T. ) ;
#34118 = CARTESIAN_POINT ( 'NONE',  ( 0.000000000000000000, -0.09999999995300053179, 0.000000000000000000 ) ) ;
#34119 = CARTESIAN_POINT ( 'NONE',  ( -3.250000000000000000, -1.600000000000000089, 0.000000000000000000 ) ) ;
#34120 = CARTESIAN_POINT ( 'NONE',  ( -0.6865296035375000328, -83.51594503318798957, -3.479976932919000010 ) ) ;
#34121 = CARTESIAN_POINT ( 'NONE',  ( -11.16685539660449322, -76.22546096737708865, -3.732204631842894305 ) ) ;
#34122 = CARTESIAN_POINT ( 'NONE',  ( 10.04116292115999975, -22.76462890193000277, 7.682344222570999470 ) ) ;
#34123 = CARTESIAN_POINT ( 'NONE',  ( -8.790688707576000738, -61.73813493216999859, -8.797962936864001549 ) ) ;
#34124 = ADVANCED_FACE ( 'NONE', ( #4219, #17207 ), #13058, .T. ) ;
#34125 = CARTESIAN_POINT ( 'NONE',  ( -7.608356748847191042, -79.22937652759581795, 9.340614718761999669 ) ) ;
#34126 = FACE_OUTER_BOUND ( 'NONE', #48602, .T. ) ;
#34127 = CARTESIAN_POINT ( 'NONE',  ( -12.61112375831999977, -18.78433928967000099, -1.798929377342999736 ) ) ;
#34128 = CARTESIAN_POINT ( 'NONE',  ( 7.349802007153999561, -77.72476194169999530, -10.73869877321999944 ) ) ;
#34129 = CARTESIAN_POINT ( 'NONE',  ( -0.9755963328057704054, -77.83258753084055570, 10.79518899496484430 ) ) ;
#34131 = CARTESIAN_POINT ( 'NONE',  ( 9.392096872483362446, -78.39518815251655326, -7.218040555448557605 ) ) ;
#34130 = CIRCLE ( 'NONE', #15404, 10.05000000000000071 ) ;
#34132 = CARTESIAN_POINT ( 'NONE',  ( 1.811016405462519963, -24.06173555371950457, -12.71771640064136655 ) ) ;
#34133 = CARTESIAN_POINT ( 'NONE',  ( -0.4693628207621999837, -76.70343746089999115, -12.35326893399999904 ) ) ;
#34134 = VERTEX_POINT ( 'NONE', #52373 ) ;
#34135 = EDGE_CURVE ( 'NONE', #43690, #54597, #2368, .T. ) ;
#34136 = CARTESIAN_POINT ( 'NONE',  ( 11.22355342542000045, -80.50686022575678180, 0.9700744431168999427 ) ) ;
#34137 = CARTESIAN_POINT ( 'NONE',  ( 9.723199427898999048, -54.32306055827000080, -7.958735709912999390 ) ) ;
#34138 = APPLICATION_CONTEXT ( 'automotive_design' ) ;
#34139 = CARTESIAN_POINT ( 'NONE',  ( 12.72558241039000038, -60.00131830475000072, 1.930284820929999867 ) ) ;
#34140 = CARTESIAN_POINT ( 'NONE',  ( -3.351075299998999668, -78.68536893705000068, -12.34648790642000016 ) ) ;
#34141 = DIRECTION ( 'NONE',  ( -1.000000000000000000, 0.000000000000000000, 0.000000000000000000 ) ) ;
#34142 = CARTESIAN_POINT ( 'NONE',  ( -9.375068251199000002, -78.41144320180897864, -2.204836785425999590 ) ) ;
#34143 = CARTESIAN_POINT ( 'NONE',  ( -3.903163414993999769, -86.14648452804499357, 1.102130188697999946 ) ) ;
#34144 = CARTESIAN_POINT ( 'NONE',  ( 1.455635362263224986, -79.96447437086105481, 10.65250472726658693 ) ) ;
#34145 = CARTESIAN_POINT ( 'NONE',  ( 0.2446082660763000405, -80.12904421889498963, -1.596051606003999979 ) ) ;
#34146 = VERTEX_POINT ( 'NONE', #48519 ) ;
#34147 = FACE_OUTER_BOUND ( 'NONE', #2611, .T. ) ;
#34148 = CARTESIAN_POINT ( 'NONE',  ( 2.059442021937579081, -78.96127176157177985, -2.897349721442271431 ) ) ;
#34149 = ADVANCED_FACE ( 'NONE', ( #29903 ), #53227, .F. ) ;
#34150 = ORIENTED_EDGE ( 'NONE', *, *, #55315, .F. ) ;
#34151 = CARTESIAN_POINT ( 'NONE',  ( -2.919153588227000107, -78.76730753078498992, 10.54354582977000021 ) ) ;
#34152 = ADVANCED_FACE ( 'NONE', ( #47958 ), #50969, .F. ) ;
#34153 = FILL_AREA_STYLE_COLOUR ( '', #45390 ) ;
#34154 = CARTESIAN_POINT ( 'NONE',  ( 0.000000000000000000, -76.75499999999999545, 0.000000000000000000 ) ) ;
#34155 = ORIENTED_EDGE ( 'NONE', *, *, #42080, .F. ) ;
#34156 = CARTESIAN_POINT ( 'NONE',  ( 12.02223179210000126, -78.94651279900399743, 0.8134715296432000198 ) ) ;
#34157 = CARTESIAN_POINT ( 'NONE',  ( 10.92669092472000081, -78.30827334234999171, 0.1833893325657000029 ) ) ;
#34158 = AXIS2_PLACEMENT_3D ( 'NONE', #20063, #25337, #15332 ) ;
#34159 = ORIENTED_EDGE ( 'NONE', *, *, #11105, .T. ) ;
#34160 = ORIENTED_EDGE ( 'NONE', *, *, #12341, .F. ) ;
#34161 = CARTESIAN_POINT ( 'NONE',  ( -0.4115157024871364810, -80.50168328157944586, 1.181061143696242599 ) ) ;
#34162 = CIRCLE ( 'NONE', #10597, 10.50000000000000000 ) ;
#34163 = CARTESIAN_POINT ( 'NONE',  ( -3.140027178014999976, -86.25171435779598994, 1.398030083151000191 ) ) ;
#34164 = CARTESIAN_POINT ( 'NONE',  ( 9.202039358297998461, -80.40014324972001702, 2.360608321670000453 ) ) ;
#34165 = ORIENTED_EDGE ( 'NONE', *, *, #44536, .F. ) ;
#34166 = CARTESIAN_POINT ( 'NONE',  ( 0.8519719440434405655, -2.455349913743563040, 3.164316409633407989 ) ) ;
#34167 = ORIENTED_EDGE ( 'NONE', *, *, #48931, .F. ) ;
#34168 = CARTESIAN_POINT ( 'NONE',  ( -8.031111192612954142, -78.48262027226905957, 9.095921368955231401 ) ) ;
#34169 = CARTESIAN_POINT ( 'NONE',  ( 3.861138328465000047, -76.91105638344899376, 8.493887087553000370 ) ) ;
#34170 = CIRCLE ( 'NONE', #22860, 1.250000000000000444 ) ;
#34171 = CARTESIAN_POINT ( 'NONE',  ( 8.798041828522000785, -53.86186490677999927, 8.790609562984000647 ) ) ;
#34172 = CARTESIAN_POINT ( 'NONE',  ( 11.00000000000000000, -77.94999999999998863, 0.000000000000000000 ) ) ;
#34173 = CARTESIAN_POINT ( 'NONE',  ( 0.1963495408493571848, -81.26458333333333428, 1.500000000000000666 ) ) ;
#34174 = CARTESIAN_POINT ( 'NONE',  ( -1.247385798842000071, -54.32277743483000165, 12.50301438874000048 ) ) ;
#34175 = AXIS2_PLACEMENT_3D ( 'NONE', #21660, #6933, #25225 ) ;
#34176 = CARTESIAN_POINT ( 'NONE',  ( -6.489766492868402459, -80.42572473943350531, -9.141528674627377171 ) ) ;
#34177 = CARTESIAN_POINT ( 'NONE',  ( 11.53501176087999980, -78.87824739248154060, -3.234124663588000548 ) ) ;
#34178 = CARTESIAN_POINT ( 'NONE',  ( 2.632379610102243639, -82.24583335181431210, -3.029167836885550802 ) ) ;
#34179 = CARTESIAN_POINT ( 'NONE',  ( -7.660431276880000695, -23.19179487662999861, 10.01749742441000102 ) ) ;
#34180 = CARTESIAN_POINT ( 'NONE',  ( 0.5576182071907999083, -79.11955496681159161, -4.135110746870999776 ) ) ;
#34181 = CARTESIAN_POINT ( 'NONE',  ( 9.653543233641000754, -78.05386001420200159, -2.068833003092999778 ) ) ;
#34182 = CARTESIAN_POINT ( 'NONE',  ( 10.30767511324000019, -60.54763733864000130, -7.634418707071000121 ) ) ;
#34183 = LINE ( 'NONE', #29751, #7573 ) ;
#34184 = CARTESIAN_POINT ( 'NONE',  ( -11.80208112487999905, -77.02061369597500118, -3.396125071686999952 ) ) ;
#34185 = CARTESIAN_POINT ( 'NONE',  ( -1.500000000000000000, -81.00000000000000000, 0.000000000000000000 ) ) ;
#34186 = CARTESIAN_POINT ( 'NONE',  ( -9.549999999953000085, -76.40000000004698677, 5.125988344190999543E-10 ) ) ;
#34187 = CARTESIAN_POINT ( 'NONE',  ( 12.00000000000000000, -78.04999999999999716, 0.000000000000000000 ) ) ;
#34188 = CARTESIAN_POINT ( 'NONE',  ( 0.9648153198142549458, -79.93009253907807476, -1.161834974252261121 ) ) ;
#34189 = DIRECTION ( 'NONE',  ( 0.7071067811865475727, 0.000000000000000000, 0.7071067811865475727 ) ) ;
#34190 = CARTESIAN_POINT ( 'NONE',  ( -12.50000000000000000, -55.35321828636000419, 1.250000000000000000 ) ) ;
#34191 = VECTOR ( 'NONE', #43737, 1000.000000000000000 ) ;
#34192 = DIRECTION ( 'NONE',  ( 0.000000000000000000, -1.000000000000000000, 0.000000000000000000 ) ) ;
#34193 = CARTESIAN_POINT ( 'NONE',  ( 0.6621380763940999392, -2.108437473830000464, -3.495547994364999855 ) ) ;
#34194 = CARTESIAN_POINT ( 'NONE',  ( 12.06733228363000165, -78.18105580595199910, -1.536887159723000051 ) ) ;
#34195 = CARTESIAN_POINT ( 'NONE',  ( -2.581517684854000017, -78.37446617076199118, -9.391243908516001326 ) ) ;
#34197 = DIRECTION ( 'NONE',  ( 1.000000000000000000, 0.000000000000000000, 0.000000000000000000 ) ) ;
#34196 = CARTESIAN_POINT ( 'NONE',  ( -11.45922444272926732, -76.18195732767712514, 2.597715832044583451 ) ) ;
#34198 = CARTESIAN_POINT ( 'NONE',  ( -1.285835855790000037, -81.60322848715999555, 0.7092774996876000104 ) ) ;
#34199 = CARTESIAN_POINT ( 'NONE',  ( -7.624341764926000131, -23.26485149464000202, 10.42531124853000080 ) ) ;
#34200 = ORIENTED_EDGE ( 'NONE', *, *, #11708, .T. ) ;
#34201 = EDGE_CURVE ( 'NONE', #44710, #37950, #7990, .T. ) ;
#34202 = DIRECTION ( 'NONE',  ( 0.000000000000000000, 1.000000000000000000, 0.000000000000000000 ) ) ;
#34203 = VECTOR ( 'NONE', #31911, 1000.000000000000000 ) ;
#34204 = CARTESIAN_POINT ( 'NONE',  ( 7.234766560894000165, -79.01412808429699908, 9.437955368358000641 ) ) ;
#34205 = CARTESIAN_POINT ( 'NONE',  ( 8.787724721424778451, -79.46806983379561018, -3.732128204872922961 ) ) ;
#34206 = CARTESIAN_POINT ( 'NONE',  ( 0.009747935475830782001, -79.99999999999998579, -9.487720945728824518 ) ) ;
#34207 = CARTESIAN_POINT ( 'NONE',  ( -8.878335097444999491, -61.86963071710999884, 8.870344075662000449 ) ) ;
#34208 = DIRECTION ( 'NONE',  ( -3.552713678800000476E-14, -1.000000000000000000, 1.184237892933000067E-14 ) ) ;
#34209 = CARTESIAN_POINT ( 'NONE',  ( -9.237809349072998444, -79.23357724651299350, -3.213393753055000079 ) ) ;
#34210 = CARTESIAN_POINT ( 'NONE',  ( 9.596002108778174389, -78.09791666666666288, -7.374560639698961140 ) ) ;
#34211 = CARTESIAN_POINT ( 'NONE',  ( -12.70722357730239871, -54.38971352745738841, -1.610228312160249864 ) ) ;
#34212 = EDGE_LOOP ( 'NONE', ( #53270, #29435, #14857, #11407 ) ) ;
#34213 = AXIS2_PLACEMENT_3D ( 'NONE', #10787, #33487, #19931 ) ;
#34214 = CARTESIAN_POINT ( 'NONE',  ( 10.40000000000000036, 0.000000000000000000, 0.000000000000000000 ) ) ;
#34215 = CARTESIAN_POINT ( 'NONE',  ( -10.68477278295909372, -79.01421070604040153, 5.086768384352462036 ) ) ;
#34216 = CARTESIAN_POINT ( 'NONE',  ( 0.5999999998848000171, -23.14999999478999726, 11.79999999988000070 ) ) ;
#34217 = VECTOR ( 'NONE', #3723, 1000.000000000000227 ) ;
#34218 = CARTESIAN_POINT ( 'NONE',  ( -0.05495261879129516996, -81.47894154460885829, 1.248718060273657837 ) ) ;
#34219 = CARTESIAN_POINT ( 'NONE',  ( -1.630114970985000022, -79.84613452854999593, -0.3434887894992000312 ) ) ;
#34220 = EDGE_CURVE ( 'NONE', #45201, #21891, #20426, .T. ) ;
#34221 = ORIENTED_EDGE ( 'NONE', *, *, #45263, .T. ) ;
#34222 = B_SPLINE_CURVE_WITH_KNOTS ( 'NONE', 3,
 ( #5526, #15854, #1708, #56299, #51301, #2289, #55719, #51593, #20284, #46001 ),
 .UNSPECIFIED., .F., .F.,
 ( 4, 2, 2, 2, 4 ),
 ( 0.000000000000000000, 0.2500000000000000000, 0.5000000000000000000, 0.7500000000000000000, 1.000000000000000000 ),
 .UNSPECIFIED. ) ;
#34223 = CARTESIAN_POINT ( 'NONE',  ( 0.01019144981830593689, -78.52458150190987851, 1.274912689113979924 ) ) ;
#34224 = CARTESIAN_POINT ( 'NONE',  ( -8.216989605509789740, -77.00000000000000000, 4.339777185649433378 ) ) ;
#34225 = CARTESIAN_POINT ( 'NONE',  ( -7.970414252932341626, -24.52292089079958615, -9.713036876646134132 ) ) ;
#34226 = LINE ( 'NONE', #19512, #30199 ) ;
#34227 = CARTESIAN_POINT ( 'NONE',  ( -5.100000000000000533, -75.20000000000000284, 0.000000000000000000 ) ) ;
#34228 = CARTESIAN_POINT ( 'NONE',  ( 5.496668217546000434, -79.88211081103300160, -8.073860231047000013 ) ) ;
#34229 = ORIENTED_EDGE ( 'NONE', *, *, #51329, .T. ) ;
#34230 = ORIENTED_EDGE ( 'NONE', *, *, #38692, .T. ) ;
#34231 = CARTESIAN_POINT ( 'NONE',  ( -10.67341028599000019, -76.21560886216698805, 6.449573273694999997 ) ) ;
#34232 = CARTESIAN_POINT ( 'NONE',  ( -6.557449765169716116, -78.67302949370692033, -8.547667297717341128 ) ) ;
#34233 = CARTESIAN_POINT ( 'NONE',  ( -0.6293846543609998845, -78.55484433024999191, 1.274475086505999943 ) ) ;
#34234 = ORIENTED_EDGE ( 'NONE', *, *, #18570, .T. ) ;
#34235 = ADVANCED_FACE ( 'NONE', ( #1852 ), #19376, .F. ) ;
#34236 = DIRECTION ( 'NONE',  ( 0.000000000000000000, -1.000000000000000000, 0.000000000000000000 ) ) ;
#34237 = CARTESIAN_POINT ( 'NONE',  ( 7.890405061430818101, -79.05045859552323861, -5.649360742093826104 ) ) ;
#34238 = CARTESIAN_POINT ( 'NONE',  ( -1.495357591690006815, -54.24123662602505647, 12.70444646756156537 ) ) ;
#34239 = CARTESIAN_POINT ( 'NONE',  ( -10.59557217617999925, -77.03266118433998599, 7.456311996931999531 ) ) ;
#34240 = DIRECTION ( 'NONE',  ( 6.735242868878000753E-11, 1.000000000000000000, 0.000000000000000000 ) ) ;
#34241 = CARTESIAN_POINT ( 'NONE',  ( -0.4871519710308191420, -86.12609999968211127, 3.917790784211915955 ) ) ;
#34242 = CONICAL_SURFACE ( 'NONE', #29289, 9.099999999966000175, 0.7853981633972997312 ) ;
#34243 = CARTESIAN_POINT ( 'NONE',  ( 10.12058791103999944, -79.61937008025999774, 4.836508133599999759 ) ) ;
#34244 = CARTESIAN_POINT ( 'NONE',  ( -0.7262319456430645914, -79.98135051806083595, 9.221384681847585085 ) ) ;
#34245 = VERTEX_POINT ( 'NONE', #45783 ) ;
#34246 = CARTESIAN_POINT ( 'NONE',  ( 0.000000000000000000, 4.040000000000000036, 0.000000000000000000 ) ) ;
#34247 = EDGE_LOOP ( 'NONE', ( #5489, #3979, #6498, #7082, #47887 ) ) ;
#34248 = CARTESIAN_POINT ( 'NONE',  ( -7.103610810849999346, -79.69152403476999780, -8.744578195291998313 ) ) ;
#34249 = CARTESIAN_POINT ( 'NONE',  ( 5.439453896751886397, -77.27516157131327645, -7.481521277697023464 ) ) ;
#34250 = CARTESIAN_POINT ( 'NONE',  ( 0.2827145210274000231, -79.93828967281199027, -1.389291862697999980 ) ) ;
#34251 = DIRECTION ( 'NONE',  ( 0.000000000000000000, -1.000000000000000000, 0.000000000000000000 ) ) ;
#34252 = CARTESIAN_POINT ( 'NONE',  ( -3.633154385059917058, -77.25115648345233410, 10.61234178577903009 ) ) ;
#34253 = UNCERTAINTY_MEASURE_WITH_UNIT (LENGTH_MEASURE( 1.000000000000000082E-05 ), #26747, 'distance_accuracy_value', 'NONE');
#34254 = CARTESIAN_POINT ( 'NONE',  ( -0.5750548074078000171, -79.01092107675799525, 1.295897153995000162 ) ) ;
#34255 = AXIS2_PLACEMENT_3D ( 'NONE', #17358, #4370, #31205 ) ;
#34256 = DIRECTION ( 'NONE',  ( -1.000000000000000000, 0.000000000000000000, 0.000000000000000000 ) ) ;
#34257 = CARTESIAN_POINT ( 'NONE',  ( 5.413904038987143785, -80.83333333333331439, 9.393203674808290771 ) ) ;
#34258 = CARTESIAN_POINT ( 'NONE',  ( -0.9156221410628999635, -78.25215827833000048, 1.345473579290000110 ) ) ;
#34259 = CARTESIAN_POINT ( 'NONE',  ( -12.82904109062999964, -18.67547726287999765, -2.062673488410000200 ) ) ;
#34260 = CARTESIAN_POINT ( 'NONE',  ( -7.612971414716000140, -18.67547470641000018, 10.53003223724000037 ) ) ;
#34261 = VECTOR ( 'NONE', #48686, 1000.000000000000000 ) ;
#34262 = CARTESIAN_POINT ( 'NONE',  ( -5.793600105730999594, -78.41198602556298169, 9.408086495002001115 ) ) ;
#34263 = DIRECTION ( 'NONE',  ( 0.000000000000000000, -1.000000000000000000, 0.000000000000000000 ) ) ;
#34264 = CARTESIAN_POINT ( 'NONE',  ( 3.630949683904999947, -79.79999999999999716, -11.17491406647000041 ) ) ;
#34265 = CYLINDRICAL_SURFACE ( 'NONE', #47953, 9.000000000000000000 ) ;
#34266 = CARTESIAN_POINT ( 'NONE',  ( 0.1743543163984999922, -85.83208224847899714, 3.543178075967999607 ) ) ;
#34267 = VERTEX_POINT ( 'NONE', #22443 ) ;
#34268 = CARTESIAN_POINT ( 'NONE',  ( -6.266080380867400379, -77.20000000000001705, 8.932657602619032744 ) ) ;
#34269 = CARTESIAN_POINT ( 'NONE',  ( -0.5581707956298000983, -81.36268744342000048, 1.358247929972999701 ) ) ;
#34270 = CARTESIAN_POINT ( 'NONE',  ( -3.206516299415000049, -2.013032031398999777, -0.5298615117031000299 ) ) ;
#34271 = CARTESIAN_POINT ( 'NONE',  ( 2.228685126279000173, -77.92621464558799005, 11.77068507108999995 ) ) ;
#34272 = LINE ( 'NONE', #16575, #38175 ) ;
#34273 = CARTESIAN_POINT ( 'NONE',  ( -1.263074648639895603, -79.26084591700393389, -0.1732096211842467925 ) ) ;
#34274 = CARTESIAN_POINT ( 'NONE',  ( 1.183291175563982778, -2.097760233681444486, 3.314621515608663582 ) ) ;
#34275 = CARTESIAN_POINT ( 'NONE',  ( 1.899930039692999895, -78.48940194988499286, 9.535935523283001203 ) ) ;
#34276 = CARTESIAN_POINT ( 'NONE',  ( -1.535759092668000036, -78.53095298048599204, 9.397436897434999992 ) ) ;
#34277 = CARTESIAN_POINT ( 'NONE',  ( -10.59418153559903963, -76.58652079386806122, 1.823743049675861316 ) ) ;
#34278 = CARTESIAN_POINT ( 'NONE',  ( -4.522750724863999316, -78.43558352699498926, 9.935798501838000618 ) ) ;
#34279 = CARTESIAN_POINT ( 'NONE',  ( 10.76452101003999928, -80.76354927348663182, -1.780076958437000201 ) ) ;
#34280 = CARTESIAN_POINT ( 'NONE',  ( -0.6937200964320594521, -82.07061195510875962, 1.068798584389240691 ) ) ;
#34281 = VERTEX_POINT ( 'NONE', #13581 ) ;
#34282 = CARTESIAN_POINT ( 'NONE',  ( -5.684557159767995138, -78.92708333333335702, 7.396918292183145560 ) ) ;
#34283 = ADVANCED_FACE ( 'NONE', ( #27150 ), #44751, .F. ) ;
#34284 = CARTESIAN_POINT ( 'NONE',  ( -0.9816856958575284064, -80.73641784909243313, -0.7730884388065356605 ) ) ;
#34285 = CARTESIAN_POINT ( 'NONE',  ( 8.959429364845298949, -78.89329112012718781, -7.653857676387937126 ) ) ;
#34286 = CARTESIAN_POINT ( 'NONE',  ( -3.957350048490399175, -78.48547955770027329, -2.236040895654427985 ) ) ;
#34287 = EDGE_CURVE ( 'NONE', #26450, #52133, #53749, .T. ) ;
#34288 = CARTESIAN_POINT ( 'NONE',  ( -0.9512330062464999791, -78.21565086401200517, 11.17646036812999988 ) ) ;
#34289 = CARTESIAN_POINT ( 'NONE',  ( -7.022507694776999543, -79.30009718909599314, 8.434951230355999030 ) ) ;
#34290 = CARTESIAN_POINT ( 'NONE',  ( 10.35410175339000105, -23.40399325350999860, -7.619715687203000520 ) ) ;
#34291 = CARTESIAN_POINT ( 'NONE',  ( 5.465577009020043953, -80.34583333333198141, 9.484549217282665978 ) ) ;
#34292 = CARTESIAN_POINT ( 'NONE',  ( 10.10886165594999930, -76.27976687979999326, -6.745106749100000521 ) ) ;
#34293 = CARTESIAN_POINT ( 'NONE',  ( 11.30151105938903733, -78.47057225285870175, 3.216226699527826138 ) ) ;
#34294 = CARTESIAN_POINT ( 'NONE',  ( -10.04567131166087357, -61.35088387338642946, 7.921299640537585951 ) ) ;
#34295 = ORIENTED_EDGE ( 'NONE', *, *, #54826, .F. ) ;
#34296 = CARTESIAN_POINT ( 'NONE',  ( -1.612912635236000147, -78.52781295235500636, 10.91330597072999886 ) ) ;
#34297 = DIRECTION ( 'NONE',  ( 1.000000000000000000, 0.000000000000000000, 0.000000000000000000 ) ) ;
#34298 = DIRECTION ( 'NONE',  ( -0.7071067811865475727, 0.000000000000000000, -0.7071067811865475727 ) ) ;
#34299 = CONICAL_SURFACE ( 'NONE', #25793, 12.94999999994000106, 0.7853981633972997312 ) ;
#34300 = EDGE_CURVE ( 'NONE', #22489, #19275, #37507, .T. ) ;
#34301 = CARTESIAN_POINT ( 'NONE',  ( 3.260743090391000187, -79.53082035574698239, 10.78408470153000032 ) ) ;
#34302 = B_SPLINE_CURVE_WITH_KNOTS ( 'NONE', 3,
 ( #39945, #19486, #427, #2080, #56377, #20078, #1788, #28620, #29201, #37479, #42510, #55502, #47246, #42222, #19784, #6778, #25070, #10933 ),
 .UNSPECIFIED., .F., .F.,
 ( 4, 2, 2, 2, 2, 2, 2, 2, 4 ),
 ( 0.000000000000000000, 0.1250000000000000000, 0.2500000000000000000, 0.3750000000000000000, 0.5000000000000000000, 0.6250000000000000000, 0.7500000000000000000, 0.8750000000000000000, 1.000000000000000000 ),
 .UNSPECIFIED. ) ;
#34303 = CARTESIAN_POINT ( 'NONE',  ( -12.82904091341000097, -60.12452529330000317, -2.062673488738000049 ) ) ;
#34304 = FACE_OUTER_BOUND ( 'NONE', #27910, .T. ) ;
#34305 = DIRECTION ( 'NONE',  ( -2.250403632142151042E-08, -0.7071067811865473507, -0.7071067811865473507 ) ) ;
#34306 = CARTESIAN_POINT ( 'NONE',  ( -1.442836895039729894, -82.87365703438442210, -0.4541944958676946142 ) ) ;
#34307 = CARTESIAN_POINT ( 'NONE',  ( -0.8673235339713729619, -79.66431752189797066, -0.8999146696370381449 ) ) ;
#34308 = CARTESIAN_POINT ( 'NONE',  ( -13.99999999996999911, -5.900000000026950353, 3.874891027003000340E-10 ) ) ;
#34309 = PRESENTATION_STYLE_ASSIGNMENT (( #16613 ) ) ;
#34310 = CARTESIAN_POINT ( 'NONE',  ( -12.55458806505999902, -24.16283916848999880, 1.575041344316999936 ) ) ;
#34311 = ORIENTED_EDGE ( 'NONE', *, *, #14207, .T. ) ;
#34312 = VERTEX_POINT ( 'NONE', #40748 ) ;
#34313 = DIRECTION ( 'NONE',  ( -1.000000000000000000, 0.000000000000000000, 0.000000000000000000 ) ) ;
#34314 = ORIENTED_EDGE ( 'NONE', *, *, #48434, .F. ) ;
#34315 = EDGE_LOOP ( 'NONE', ( #2828, #21442, #19016, #32848, #20263 ) ) ;
#34316 = CARTESIAN_POINT ( 'NONE',  ( -10.43309661003928035, -81.00000000000001421, -2.732452926732640730 ) ) ;
#34317 = CARTESIAN_POINT ( 'NONE',  ( 6.963658808075999573, -78.25476576377499782, -8.131364605499999954 ) ) ;
#34318 = CARTESIAN_POINT ( 'NONE',  ( -0.3926218265389190276, -78.10416666666667140, -1.460959015002473826 ) ) ;
#34319 = CARTESIAN_POINT ( 'NONE',  ( 9.449971683680001178, -78.42181332859900067, -2.591602768458999950 ) ) ;
#34320 = CARTESIAN_POINT ( 'NONE',  ( -3.149542236319641475, -78.19745273510419281, -8.697855718134043457 ) ) ;
#34321 = CARTESIAN_POINT ( 'NONE',  ( 7.348709943010458545, -79.30274935012705839, 5.745885650500440534 ) ) ;
#34322 = AXIS2_PLACEMENT_3D ( 'NONE', #6525, #21255, #11550 ) ;
#34323 = VERTEX_POINT ( 'NONE', #343 ) ;
#34324 = ORIENTED_EDGE ( 'NONE', *, *, #48742, .T. ) ;
#34325 = CARTESIAN_POINT ( 'NONE',  ( -3.175871872419103070, -77.50302735801024312, 8.687844134873774493 ) ) ;
#34326 = LINE ( 'NONE', #21336, #47072 ) ;
#34327 = ADVANCED_FACE ( 'NONE', ( #18322 ), #36314, .F. ) ;
#34328 = CARTESIAN_POINT ( 'NONE',  ( 10.86862532138017912, -78.33584017775066854, -1.957230818804968520 ) ) ;
#34329 = CARTESIAN_POINT ( 'NONE',  ( -8.592320330817999618, -78.29168487677797827, 4.510292750937000328 ) ) ;
#34330 = CARTESIAN_POINT ( 'NONE',  ( 7.705142895619999877, -20.24916621771999914, 10.24998526317999925 ) ) ;
#34331 = CARTESIAN_POINT ( 'NONE',  ( 8.114920487424473805, -61.62884529302247216, 9.847900218122900284 ) ) ;
#34332 = CARTESIAN_POINT ( 'NONE',  ( -10.75000000000000000, -76.50000000000000000, 0.000000000000000000 ) ) ;
#34333 = CARTESIAN_POINT ( 'NONE',  ( -10.49924843836999955, -80.39917579582198925, -4.054558598941000014 ) ) ;
#34334 = FACE_OUTER_BOUND ( 'NONE', #48254, .T. ) ;
#34335 = AXIS2_PLACEMENT_3D ( 'NONE', #54082, #380, #18359 ) ;
#34336 = CARTESIAN_POINT ( 'NONE',  ( 1.980532734072999901, -59.56232686814000488, 12.80090744966000038 ) ) ;
#34337 = CARTESIAN_POINT ( 'NONE',  ( 0.000000000000000000, -75.00000000000001421, 0.000000000000000000 ) ) ;
#34338 = CARTESIAN_POINT ( 'NONE',  ( -9.170454433240001535, -78.91216332859900717, 3.758088286126999744 ) ) ;
#34339 = CARTESIAN_POINT ( 'NONE',  ( -6.777984382448000389, -78.27882627552999395, -9.878005474088999094 ) ) ;
#34340 = CARTESIAN_POINT ( 'NONE',  ( -7.974020021247000933, -17.36898233693000293, -9.929669236791999865 ) ) ;
#34342 = CARTESIAN_POINT ( 'NONE',  ( 0.8445585116436000739, -17.28959556757000016, -12.43380736237000050 ) ) ;
#34341 = CARTESIAN_POINT ( 'NONE',  ( 7.613962745625999062, -60.10639784916000394, 10.53101990622000095 ) ) ;
#34343 = CARTESIAN_POINT ( 'NONE',  ( 1.211018816713875124, -79.46477661281171834, 9.190900382934870549 ) ) ;
#34344 = CARTESIAN_POINT ( 'NONE',  ( -10.78747482502000032, -79.91111849808099521, 2.492395449116000083 ) ) ;
#34345 = CARTESIAN_POINT ( 'NONE',  ( -8.684735281668000795, -77.87832987473298374, -7.170030519161000093 ) ) ;
#34346 = CARTESIAN_POINT ( 'NONE',  ( 2.674705653217700263, -3.500000000000001332, 2.124395908964210822 ) ) ;
#34347 = CARTESIAN_POINT ( 'NONE',  ( -3.521517461832780693, -1.752479614403898323, -0.1112614230686466144 ) ) ;
#34348 = VERTEX_POINT ( 'NONE', #49914 ) ;
#34349 = LINE ( 'NONE', #51814, #26316 ) ;
#34350 = DIRECTION ( 'NONE',  ( -0.3090169943750110115, 0.000000000000000000, -0.9510565162951328810 ) ) ;
#34351 = CARTESIAN_POINT ( 'NONE',  ( -1.250000000000000000, -77.64999999999999147, 0.000000000000000000 ) ) ;
#34352 = CARTESIAN_POINT ( 'NONE',  ( 0.9185483849010980251, -78.40937492225079097, 0.8489402260638932995 ) ) ;
#34353 = CARTESIAN_POINT ( 'NONE',  ( -1.265915941616999829, -1.948956610291999736, 3.247563974725000246 ) ) ;
#34354 = EDGE_CURVE ( 'NONE', #19523, #54307, #34059, .T. ) ;
#34355 = CARTESIAN_POINT ( 'NONE',  ( -9.601393729781001696, -79.88570935437299170, 0.8896799134053999802 ) ) ;
#34356 = CARTESIAN_POINT ( 'NONE',  ( -8.547463563348092208, -77.04807323675491659, 6.557389287125792166 ) ) ;
#34357 = CYLINDRICAL_SURFACE ( 'NONE', #12022, 1.750000000000000000 ) ;
#34358 = CARTESIAN_POINT ( 'NONE',  ( 0.000000000000000000, -91.89999999999999147, 0.000000000000000000 ) ) ;
#34359 = CARTESIAN_POINT ( 'NONE',  ( 0.5999999999999999778, -5.000000000000000000, 0.5999999999999999778 ) ) ;
#34360 = CARTESIAN_POINT ( 'NONE',  ( 1.439896632895334649, -77.33541666666666003, -10.99999999999999822 ) ) ;
#34361 = DIRECTION ( 'NONE',  ( -1.000000000000000000, 0.000000000000000000, 0.000000000000000000 ) ) ;
#34362 = CARTESIAN_POINT ( 'NONE',  ( 9.237438452994998883, -77.51063887770899896, -6.076007254799000279 ) ) ;
#34363 = CONICAL_SURFACE ( 'NONE', #41002, 10.90000000000000036, 0.7853981633972997312 ) ;
#34364 = EDGE_CURVE ( 'NONE', #34267, #22190, #5183, .T. ) ;
#34365 = CARTESIAN_POINT ( 'NONE',  ( 1.105002574708906726, -76.33194444570602855, -11.71518713480698715 ) ) ;
#34366 = CARTESIAN_POINT ( 'NONE',  ( 1.499018853861999956, -77.57312960254600398, 11.04570246958999924 ) ) ;
#34367 = CARTESIAN_POINT ( 'NONE',  ( 0.9318330740823052016, -81.90881483467170199, 0.8363232822795773069 ) ) ;
#34368 = CARTESIAN_POINT ( 'NONE',  ( 1.371113636630000077, -79.03211706016000448, -0.9421181051954000685 ) ) ;
#34369 = ADVANCED_FACE ( 'NONE', ( #2355 ), #52297, .F. ) ;
#34370 = CARTESIAN_POINT ( 'NONE',  ( 10.18499221075000172, -58.54977139891999371, 7.710118476601000026 ) ) ;
#34371 = CARTESIAN_POINT ( 'NONE',  ( 1.500000000000000000, -78.75000000000000000, 0.000000000000000000 ) ) ;
#34372 = CARTESIAN_POINT ( 'NONE',  ( 10.75000000000000000, -77.85000000000000853, 0.000000000000000000 ) ) ;
#34373 = CARTESIAN_POINT ( 'NONE',  ( 5.978428684135045579, -80.27239524385058189, -8.933915976532038172 ) ) ;
#34374 = CARTESIAN_POINT ( 'NONE',  ( -8.859283645363305482, -76.15416666664359013, 7.973755076573407763 ) ) ;
#34375 = CARTESIAN_POINT ( 'NONE',  ( 6.586108526242999694, -80.17391735373439587, 8.810401493720998900 ) ) ;
#34376 = ORIENTED_EDGE ( 'NONE', *, *, #17899, .F. ) ;
#34377 = CARTESIAN_POINT ( 'NONE',  ( 2.377756013412999803, -79.20693940223900142, -11.79209151100000064 ) ) ;
#34378 = AXIS2_PLACEMENT_3D ( 'NONE', #34662, #24668, #16103 ) ;
#34379 = CARTESIAN_POINT ( 'NONE',  ( 8.300970689365438915, -78.59166666666666856, 4.784380313523563188 ) ) ;
#34380 = FACE_OUTER_BOUND ( 'NONE', #56049, .T. ) ;
#34381 = ORIENTED_EDGE ( 'NONE', *, *, #9038, .T. ) ;
#34382 = DIRECTION ( 'NONE',  ( 5.794542751510810980E-07, -1.853100651952265483E-20, -0.9999999999998322453 ) ) ;
#34383 = ORIENTED_EDGE ( 'NONE', *, *, #48486, .T. ) ;
#34384 = VERTEX_POINT ( 'NONE', #1780 ) ;
#34385 = CARTESIAN_POINT ( 'NONE',  ( -0.4254240051736287720, -1.385416666666666297, 3.249999999999998224 ) ) ;
#34386 = ADVANCED_FACE ( 'NONE', ( #14742 ), #10426, .F. ) ;
#34387 = VERTEX_POINT ( 'NONE', #11784 ) ;
#34388 = CARTESIAN_POINT ( 'NONE',  ( -2.656488545785999911, -81.92924548946498930, -2.346920921671000304 ) ) ;
#34389 = CARTESIAN_POINT ( 'NONE',  ( 3.858042142442956735, -79.24129547567945053, 8.682305691183742624 ) ) ;
#34390 = VERTEX_POINT ( 'NONE', #25345 ) ;
#34391 = CARTESIAN_POINT ( 'NONE',  ( -1.249311940503775809, -82.61097515347459819, -0.1638495906064939833 ) ) ;
#34392 = ORIENTED_EDGE ( 'NONE', *, *, #37434, .F. ) ;
#34393 = CARTESIAN_POINT ( 'NONE',  ( 1.199999995295999877, -81.00000000470399186, 7.000000027760000521 ) ) ;
#34394 = EDGE_LOOP ( 'NONE', ( #48643, #10923, #48849, #41735, #39346, #40477, #29437, #32695, #15529, #29170, #39182 ) ) ;
#34395 = CARTESIAN_POINT ( 'NONE',  ( -9.555308244098332793, -79.54990282387937839, -0.02401532431606494614 ) ) ;
#34396 = CARTESIAN_POINT ( 'NONE',  ( -1.405018988616864251, -79.22043665247308297, 0.5474336264918724382 ) ) ;
#34397 = CARTESIAN_POINT ( 'NONE',  ( -10.99609774599787215, -18.31447404869839701, 0.3135602106493823316 ) ) ;
#34398 = ADVANCED_FACE ( 'NONE', ( #33905 ), #52511, .F. ) ;
#34399 = DIRECTION ( 'NONE',  ( 0.000000000000000000, -1.000000000000000000, 0.000000000000000000 ) ) ;
#34400 = CARTESIAN_POINT ( 'NONE',  ( -3.237453996416379542, -86.12609999968209706, -2.259489515355698419 ) ) ;
#34401 = CARTESIAN_POINT ( 'NONE',  ( -7.860507001410999450, -76.77091749508699081, 7.955276143908999842 ) ) ;
#34402 = CARTESIAN_POINT ( 'NONE',  ( 9.246161438659999732, -76.69780122596999661, -8.285323839175999794 ) ) ;
#34403 = EDGE_CURVE ( 'NONE', #35472, #12675, #16788, .T. ) ;
#34404 = CARTESIAN_POINT ( 'NONE',  ( 2.633009914059649681, -77.20296729498775790, 9.306851964919491849 ) ) ;
#34405 = AXIS2_PLACEMENT_3D ( 'NONE', #55069, #41787, #42378 ) ;
#34406 = CARTESIAN_POINT ( 'NONE',  ( -7.730852068515999598, -76.89588675065598977, 7.824058043802000206 ) ) ;
#34407 = CARTESIAN_POINT ( 'NONE',  ( -10.14950121162999963, -19.24922972541000021, 7.674627477474999182 ) ) ;
#34408 = CIRCLE ( 'NONE', #16516, 1.750000000000000000 ) ;
#34409 = CARTESIAN_POINT ( 'NONE',  ( -0.5999999999999999778, -5.000000000000000000, -0.5999999999999999778 ) ) ;
#34410 = CARTESIAN_POINT ( 'NONE',  ( 2.294724576751220990, -2.913169622022151906, 2.300959236491029181 ) ) ;
#34411 = CARTESIAN_POINT ( 'NONE',  ( 3.645312643188000301, -82.04903455456799577, -1.554753716817999898 ) ) ;
#34412 = CARTESIAN_POINT ( 'NONE',  ( -4.175974021636958078, -78.00676210295078761, 9.905762318292611113 ) ) ;
#34413 = CARTESIAN_POINT ( 'NONE',  ( -3.250000000000000000, -2.500000000000000000, 0.000000000000000000 ) ) ;
#34414 = CARTESIAN_POINT ( 'NONE',  ( -13.13047446164998711, -56.01421830981000483, -0.8260994316375004365 ) ) ;
#34415 = CARTESIAN_POINT ( 'NONE',  ( 1.078420410906000049, -83.63619503318798820, -3.379137726269000108 ) ) ;
#34416 = CARTESIAN_POINT ( 'NONE',  ( 0.3271848554490964789, -80.35416666666665719, 1.217465845835395521 ) ) ;
#34417 = CARTESIAN_POINT ( 'NONE',  ( 10.48543666025108045, -79.19166666666664867, 6.043427764450817641 ) ) ;
#34418 = CARTESIAN_POINT ( 'NONE',  ( -8.188293269190999979, -61.50494400535999517, -9.395718629102999486 ) ) ;
#34419 = AXIS2_PLACEMENT_3D ( 'NONE', #33478, #51805, #10480 ) ;
#34420 = CARTESIAN_POINT ( 'NONE',  ( -5.838193839761721016, -78.32708333333332007, 7.596835002782687418 ) ) ;
#34421 = CARTESIAN_POINT ( 'NONE',  ( -0.9218200799623716968, -77.57291666666667140, -1.199500263597270910 ) ) ;
#34422 = CARTESIAN_POINT ( 'NONE',  ( 1.500000000000000000, -80.65000000000000568, 0.000000000000000000 ) ) ;
#34423 = CARTESIAN_POINT ( 'NONE',  ( 12.72397319114999981, -23.22144180305999939, 1.930910316632999946 ) ) ;
#34424 = CARTESIAN_POINT ( 'NONE',  ( 8.318585563179999198, -78.11610009011799605, 7.159970128962999780 ) ) ;
#34425 = CARTESIAN_POINT ( 'NONE',  ( 1.668607604570599312, -23.79381631241117390, -12.52787843850908978 ) ) ;
#34426 = CARTESIAN_POINT ( 'NONE',  ( -12.41568479072999942, -76.00427771482000594, -1.552457108973999800 ) ) ;
#34427 = EDGE_LOOP ( 'NONE', ( #34383, #19731, #20025, #27343, #38469, #26333 ) ) ;
#34428 = CARTESIAN_POINT ( 'NONE',  ( 3.862060628231000159, -80.59715328376763921, 10.58270681924999934 ) ) ;
#34429 = CARTESIAN_POINT ( 'NONE',  ( -11.27112434177000111, -80.28882241345029058, -1.746253588004999857 ) ) ;
#34430 = CARTESIAN_POINT ( 'NONE',  ( 12.77301895554999867, -61.85186686341000240, 1.052127376138000114 ) ) ;
#34431 = CARTESIAN_POINT ( 'NONE',  ( -6.116358872417999137, -78.49843700449001460, 10.57564232554000050 ) ) ;
#34432 = CARTESIAN_POINT ( 'NONE',  ( 12.61277494327999982, -55.60332099621999902, -1.798398135845999946 ) ) ;
#34433 = CARTESIAN_POINT ( 'NONE',  ( 5.883202309618000392, -78.07035725226099032, -7.625033806424000637 ) ) ;
#34434 = ADVANCED_FACE ( 'NONE', ( #43942 ), #1477, .F. ) ;
#34435 = CARTESIAN_POINT ( 'NONE',  ( 3.632931406222999815, -85.58531592346599837, 2.052286280999000123 ) ) ;
#34436 = CARTESIAN_POINT ( 'NONE',  ( 4.234904783647084336, -79.94291063207141690, 9.880592056022285519 ) ) ;
#34437 = CARTESIAN_POINT ( 'NONE',  ( -1.435212230719999926, -80.02981897213200568, -0.7398511866349000154 ) ) ;
#34438 = ORIENTED_EDGE ( 'NONE', *, *, #36087, .T. ) ;
#34439 = CARTESIAN_POINT ( 'NONE',  ( 9.611650271896824194, -78.90833333333333144, -5.539808784079917281 ) ) ;
#34440 = CARTESIAN_POINT ( 'NONE',  ( -3.548349909811000291, -78.96264282632948550, -1.488874400533411246E-14 ) ) ;
#34441 = ORIENTED_EDGE ( 'NONE', *, *, #25087, .T. ) ;
#34442 = CARTESIAN_POINT ( 'NONE',  ( -10.10513987668000091, -78.40210692446099472, -4.192131248929999998 ) ) ;
#34443 = DIRECTION ( 'NONE',  ( 0.000000000000000000, 1.000000000000000000, 0.000000000000000000 ) ) ;
#34444 = CARTESIAN_POINT ( 'NONE',  ( -1.678309891182000024, -80.29203597816000126, -10.90631216329999909 ) ) ;
#34445 = ORIENTED_EDGE ( 'NONE', *, *, #7435, .T. ) ;
#34446 = CARTESIAN_POINT ( 'NONE',  ( 11.05834404496999923, -78.97364211442699400, 4.786306364259000468 ) ) ;
#34447 = ORIENTED_EDGE ( 'NONE', *, *, #52799, .F. ) ;
#34448 = B_SPLINE_CURVE_WITH_KNOTS ( 'NONE', 3,
 ( #12128, #7695, #11563, #24549, #25696, #56720, #1843, #20701, #33395, #51433 ),
 .UNSPECIFIED., .F., .F.,
 ( 4, 2, 2, 2, 4 ),
 ( 0.000000000000000000, 0.2500000000000000000, 0.5000000000000000000, 0.7500000000000000000, 1.000000000000000000 ),
 .UNSPECIFIED. ) ;
#34449 = ORIENTED_EDGE ( 'NONE', *, *, #17014, .T. ) ;
#34450 = EDGE_CURVE ( 'NONE', #51480, #56774, #35343, .T. ) ;
#34451 = CARTESIAN_POINT ( 'NONE',  ( 0.4497712132741803481, -80.44584343092967060, 1.166231044311930365 ) ) ;
#34452 = EDGE_CURVE ( 'NONE', #19275, #39544, #31213, .T. ) ;
#34453 = CARTESIAN_POINT ( 'NONE',  ( 11.44598977081988345, -77.96780392635157853, 3.079303880734496790 ) ) ;
#34454 = CARTESIAN_POINT ( 'NONE',  ( -2.217000330786000450, -79.52338147675502000, 9.512392227823999846 ) ) ;
#34455 = EDGE_LOOP ( 'NONE', ( #26044, #55307, #11121, #44363 ) ) ;
#34456 = CARTESIAN_POINT ( 'NONE',  ( 3.250000000000000000, -2.350000000000000089, 0.000000000000000000 ) ) ;
#34457 = ORIENTED_EDGE ( 'NONE', *, *, #2994, .T. ) ;
#34458 = CARTESIAN_POINT ( 'NONE',  ( -1.777672186646999997, -78.93657643206628904, 12.13420648597999829 ) ) ;
#34459 = CARTESIAN_POINT ( 'NONE',  ( 3.699999999670000594, -79.00321104920828930, -1.355252715606880543E-15 ) ) ;
#34460 = CARTESIAN_POINT ( 'NONE',  ( 10.31988039472999930, -54.51085245502000021, 7.753829094159000235 ) ) ;
#34461 = CARTESIAN_POINT ( 'NONE',  ( 8.114915067892086498, -17.17115967855345104, -9.847905526149444810 ) ) ;
#34462 = DIRECTION ( 'NONE',  ( 1.000000000000000000, 0.000000000000000000, 0.000000000000000000 ) ) ;
#34463 = CARTESIAN_POINT ( 'NONE',  ( 6.670495747569742839, -78.23427913613843998, -7.076578245536430778 ) ) ;
#34464 = EDGE_CURVE ( 'NONE', #51092, #41582, #34675, .T. ) ;
#34465 = FACE_OUTER_BOUND ( 'NONE', #21524, .T. ) ;
#34466 = DIRECTION ( 'NONE',  ( 0.000000000000000000, -1.000000000000000000, 0.000000000000000000 ) ) ;
#34467 = CARTESIAN_POINT ( 'NONE',  ( 9.249909156602798888, -78.84782921127370514, -0.2699301895770213067 ) ) ;
#34468 = CARTESIAN_POINT ( 'NONE',  ( -11.91862232004000077, -75.92788042555999084, 3.079279237876999531 ) ) ;
#34469 = CARTESIAN_POINT ( 'NONE',  ( -6.380837375266275480, -79.36735876298251924, -7.083146235777555866 ) ) ;
#34470 = CARTESIAN_POINT ( 'NONE',  ( 7.527250314086999516, -78.12666001420200246, 6.388289016235000339 ) ) ;
#34471 = CARTESIAN_POINT ( 'NONE',  ( 10.18127202940000053, -60.18645218919000683, -7.633406483317000557 ) ) ;
#34472 = CARTESIAN_POINT ( 'NONE',  ( -1.777672186646999997, -78.86924249125999609, 12.13420648597999829 ) ) ;
#34473 = CARTESIAN_POINT ( 'NONE',  ( -1.925872869407999843, -76.61078631292498642, -12.12904120624999926 ) ) ;
#34474 = CARTESIAN_POINT ( 'NONE',  ( 9.500000000000000000, -78.64999999999999147, 0.000000000000000000 ) ) ;
#34475 = DIRECTION ( 'NONE',  ( 0.000000000000000000, -1.000000000000000000, 0.000000000000000000 ) ) ;
#34476 = CARTESIAN_POINT ( 'NONE',  ( 8.485281374238999419, -60.74999999967048581, -8.485281374238999419 ) ) ;
#34477 = EDGE_CURVE ( 'NONE', #25833, #4267, #11757, .T. ) ;
#34478 = AXIS2_PLACEMENT_3D ( 'NONE', #40979, #22969, #32675 ) ;
#34479 = CARTESIAN_POINT ( 'NONE',  ( 1.447876981061720691, -81.02323280059788146, 0.4369728999075917497 ) ) ;
#34480 = CARTESIAN_POINT ( 'NONE',  ( 7.531584214675000055, -77.32165489554499516, 5.594615735256000200 ) ) ;
#34481 = CARTESIAN_POINT ( 'NONE',  ( 11.89999999977000122, -18.84999999999999787, 0.000000000000000000 ) ) ;
#34482 = FACE_BOUND ( 'NONE', #20327, .T. ) ;
#34483 = CARTESIAN_POINT ( 'NONE',  ( 0.4885402653841000031, -3.419151880086999995, 3.366111076004999703 ) ) ;
#34484 = VECTOR ( 'NONE', #44520, 1000.000000000000114 ) ;
#34485 = CARTESIAN_POINT ( 'NONE',  ( 9.289757862025998847, -77.74698675917198898, 7.853848066408001038 ) ) ;
#34486 = CARTESIAN_POINT ( 'NONE',  ( 5.110488341091000031, -78.60185680379399287, 8.291116005822999568 ) ) ;
#34488 = CARTESIAN_POINT ( 'NONE',  ( 0.2696047275149000555, -79.10056507792100433, 1.291465103089999955 ) ) ;
#34487 = CARTESIAN_POINT ( 'NONE',  ( -11.51771691073675186, -76.18376931278361042, 2.323585216717103386 ) ) ;
#34489 = CARTESIAN_POINT ( 'NONE',  ( -1.331776743724000234, -83.16115579321099460, -0.3115240295706999674 ) ) ;
#34490 = CARTESIAN_POINT ( 'NONE',  ( -10.63482758102835746, -79.58845129605020929, 1.575059985258391526 ) ) ;
#34491 = VECTOR ( 'NONE', #57329, 1000.000000000000114 ) ;
#34492 = ORIENTED_EDGE ( 'NONE', *, *, #45175, .T. ) ;
#34493 = CARTESIAN_POINT ( 'NONE',  ( -10.35845608625999859, -18.70221245812999911, -7.627487525417000036 ) ) ;
#34494 = CARTESIAN_POINT ( 'NONE',  ( 5.873650711053000073, -79.85752639446890555, -10.25566215449000040 ) ) ;
#34495 = CARTESIAN_POINT ( 'NONE',  ( -9.324131985855107274, -79.26576877103842378, -1.871943872962896105 ) ) ;
#34496 = CARTESIAN_POINT ( 'NONE',  ( -6.215025413931507536, -80.00000000000000000, -7.018981048385420252 ) ) ;
#34497 = CARTESIAN_POINT ( 'NONE',  ( -0.6747260877994001316, -82.25000000000000000, -1.052256958371999840 ) ) ;
#34498 = CARTESIAN_POINT ( 'NONE',  ( -2.884990931743999898, -1.577671397434999845, -1.282714777154000174 ) ) ;
#34499 = CARTESIAN_POINT ( 'NONE',  ( 9.459667290369997872, -80.04440615245599133, 2.889698063178000265 ) ) ;
#34500 = FACE_OUTER_BOUND ( 'NONE', #16266, .T. ) ;
#34501 = CARTESIAN_POINT ( 'NONE',  ( 9.611650271896847286, -78.80833333333333712, -5.539808784079878201 ) ) ;
#34502 = EDGE_LOOP ( 'NONE', ( #52270, #47916, #19311, #40510 ) ) ;
#34503 = DIRECTION ( 'NONE',  ( 0.7071067811865475727, 0.000000000000000000, 0.7071067811865475727 ) ) ;
#34504 = CARTESIAN_POINT ( 'NONE',  ( -11.32256795663581883, -79.07170504178779424, -3.221356905262933168 ) ) ;
#34505 = CARTESIAN_POINT ( 'NONE',  ( -1.927595379902999895, -79.92946001420199309, -9.337547616506999049 ) ) ;
#34506 = CARTESIAN_POINT ( 'NONE',  ( 3.962812355711000212, -78.54828561723799396, 0.000000000000000000 ) ) ;
#34507 = CARTESIAN_POINT ( 'NONE',  ( 1.587978134902999994, -80.66326143374000424, 0.5035716945827000135 ) ) ;
#34508 = ORIENTED_EDGE ( 'NONE', *, *, #27593, .F. ) ;
#34509 = CARTESIAN_POINT ( 'NONE',  ( -1.140137907013035523, -79.11293633046733476, 0.5694093068792435153 ) ) ;
#34510 = CARTESIAN_POINT ( 'NONE',  ( -9.131943537062705119, -77.00000000000000000, 1.799860230811830997 ) ) ;
#34511 = CARTESIAN_POINT ( 'NONE',  ( -9.722718241315000398, -55.54999999966999980, -7.954951288349001004 ) ) ;
#34512 = B_SPLINE_CURVE_WITH_KNOTS ( 'NONE', 3,
 ( #15378, #51408, #14199, #10961, #51983, #38097, #20956, #7097, #12102, #38383, #56117, #39244, #29227, #57259, #52833, #7668 ),
 .UNSPECIFIED., .F., .F.,
 ( 4, 2, 2, 2, 2, 2, 2, 4 ),
 ( 0.000000000000000000, 0.2500000000000002220, 0.3749999999999991118, 0.4999999999999980016, 0.6249999999999968914, 0.6874999999999963363, 0.7499999999999958922, 1.000000000000000000 ),
 .UNSPECIFIED. ) ;
#34513 = EDGE_CURVE ( 'NONE', #16536, #55676, #43801, .T. ) ;
#34514 = CARTESIAN_POINT ( 'NONE',  ( -5.414043966650280204, -78.51670080977129373, 9.393383066539517046 ) ) ;
#34515 = CARTESIAN_POINT ( 'NONE',  ( -2.217000330786000450, -79.10276701284199419, 9.512392227823999846 ) ) ;
#34516 = ORIENTED_EDGE ( 'NONE', *, *, #43234, .F. ) ;
#34517 = ORIENTED_EDGE ( 'NONE', *, *, #25889, .T. ) ;
#34518 = CARTESIAN_POINT ( 'NONE',  ( -1.974112733099000039, -76.93905973945899746, -12.43285320951000017 ) ) ;
#34519 = CARTESIAN_POINT ( 'NONE',  ( 2.133450394463557664, -78.74103176239034951, -10.53608711097416162 ) ) ;
#34520 = CARTESIAN_POINT ( 'NONE',  ( -0.2168337308465000113, -78.03052863245000026, 1.404775742570000041 ) ) ;
#34521 = ORIENTED_EDGE ( 'NONE', *, *, #35748, .T. ) ;
#34522 = CARTESIAN_POINT ( 'NONE',  ( 3.861138328465000047, -77.03126418298700173, 8.493887087553000370 ) ) ;
#34523 = CARTESIAN_POINT ( 'NONE',  ( -8.796335266380014062, -77.64791666666667425, 6.760013919724027431 ) ) ;
#34524 = LINE ( 'NONE', #16834, #6290 ) ;
#34525 = CARTESIAN_POINT ( 'NONE',  ( -10.25367346088999909, -78.20590642111000079, 7.393739220494000008 ) ) ;
#34526 = AXIS2_PLACEMENT_3D ( 'NONE', #22755, #36329, #18045 ) ;
#34527 = CARTESIAN_POINT ( 'NONE',  ( -9.050966798898000931, -59.94999999040999938, -7.919595949288999570 ) ) ;
#34529 = EDGE_CURVE ( 'NONE', #10810, #58355, #26815, .T. ) ;
#34528 = CYLINDRICAL_SURFACE ( 'NONE', #50369, 1.000000000000000000 ) ;
#34530 = DIRECTION ( 'NONE',  ( -1.000000000000000000, 0.000000000000000000, 0.000000000000000000 ) ) ;
#34531 = CARTESIAN_POINT ( 'NONE',  ( 0.9578316561262000262, -79.03348640149199866, -11.17589679220000143 ) ) ;
#34532 = DIRECTION ( 'NONE',  ( 0.000000000000000000, -1.000000000000000000, 0.000000000000000000 ) ) ;
#34533 = VECTOR ( 'NONE', #9315, 1000.000000000000000 ) ;
#34534 = ORIENTED_EDGE ( 'NONE', *, *, #53369, .F. ) ;
#34535 = CARTESIAN_POINT ( 'NONE',  ( -4.858114519317477509, -78.20876728749668416, 10.74709704218741813 ) ) ;
#34536 = ORIENTED_EDGE ( 'NONE', *, *, #32809, .T. ) ;
#34537 = CARTESIAN_POINT ( 'NONE',  ( 10.83613785003000096, -78.84875340478899375, -3.083350589994000135 ) ) ;
#34538 = CARTESIAN_POINT ( 'NONE',  ( 4.461117935985351224, -77.26506148592295631, -8.103638615493796493 ) ) ;
#34539 = CARTESIAN_POINT ( 'NONE',  ( 0.5703284788033999853, -80.08136847860799890, 1.189660050829999927 ) ) ;
#34540 = FACE_OUTER_BOUND ( 'NONE', #10224, .T. ) ;
#34541 = CARTESIAN_POINT ( 'NONE',  ( 9.762347760324658452, -76.49685047353065670, 6.553835441005383622 ) ) ;
#34542 = CARTESIAN_POINT ( 'NONE',  ( 0.7281259072094999896, -77.77060549223068620, -1.216509659635999885 ) ) ;
#34543 = DIRECTION ( 'NONE',  ( -1.411442051944999995E-10, 6.386283326366000088E-09, -1.000000000000000000 ) ) ;
#34544 = DIRECTION ( 'NONE',  ( 0.000000000000000000, -1.000000000000000000, 0.000000000000000000 ) ) ;
#34545 = CARTESIAN_POINT ( 'NONE',  ( -5.539808784079933268, -78.51666666666667993, 9.611650271896811759 ) ) ;
#34546 = EDGE_CURVE ( 'NONE', #43155, #4192, #38170, .T. ) ;
#34547 = PLANE ( 'NONE',  #1748 ) ;
#34548 = CARTESIAN_POINT ( 'NONE',  ( -7.668949790003000366, -22.77129148951999937, 10.21381326472000062 ) ) ;
#34549 = CARTESIAN_POINT ( 'NONE',  ( 9.014082483815000657, -78.75678530967299196, -6.575554473347999362 ) ) ;
#34550 = CARTESIAN_POINT ( 'NONE',  ( 10.01332852689000141, -18.71943464842000182, -7.654537165467999671 ) ) ;
#34551 = DIRECTION ( 'NONE',  ( -0.7071067811865475727, 0.000000000000000000, 0.7071067811865475727 ) ) ;
#34552 = EDGE_CURVE ( 'NONE', #26739, #26014, #14566, .T. ) ;
#34553 = CARTESIAN_POINT ( 'NONE',  ( -9.312500000004000356, -79.68749999999599254, 6.570867420027000168E-10 ) ) ;
#34554 = DIRECTION ( 'NONE',  ( 0.000000000000000000, 0.000000000000000000, -1.000000000000000000 ) ) ;
#34555 = ORIENTED_EDGE ( 'NONE', *, *, #45187, .F. ) ;
#34556 = CARTESIAN_POINT ( 'NONE',  ( -1.260823269212999920, -83.43220886491398858, -0.6699510868867000202 ) ) ;
#34557 = CARTESIAN_POINT ( 'NONE',  ( -0.7850755733694999572, -79.53107020522999449, -1.063938263677999929 ) ) ;
#34558 = DIRECTION ( 'NONE',  ( 0.000000000000000000, -1.000000000000000000, 0.000000000000000000 ) ) ;
#34559 = CARTESIAN_POINT ( 'NONE',  ( 9.450487096927000508, -77.76343875304499420, -7.362360902974999455 ) ) ;
#34560 = CARTESIAN_POINT ( 'NONE',  ( 0.000000000000000000, -81.00000000000000000, 0.000000000000000000 ) ) ;
#34561 = CARTESIAN_POINT ( 'NONE',  ( 1.541440768196999933, -82.49213214217199663, 0.6318380856084999664 ) ) ;
#34562 = CARTESIAN_POINT ( 'NONE',  ( -1.042351935971276067, -2.351068062435671902, -3.365055153995229809 ) ) ;
#34563 = CARTESIAN_POINT ( 'NONE',  ( -0.6471704932797999188, -78.01035194988499200, 9.701898969124000516 ) ) ;
#34564 = CARTESIAN_POINT ( 'NONE',  ( -9.269208960685000775, -78.16144320180897864, -2.179940704506999616 ) ) ;
#34565 = CARTESIAN_POINT ( 'NONE',  ( 0.6812374851801442643, -81.27140723383548959, -1.049688098706359041 ) ) ;
#34566 = CARTESIAN_POINT ( 'NONE',  ( -9.500000000000000000, -78.89999999999999147, 0.000000000000000000 ) ) ;
#34567 = CARTESIAN_POINT ( 'NONE',  ( 10.95939905454414109, -75.97881982022552450, 4.237625572471915625 ) ) ;
#34568 = CARTESIAN_POINT ( 'NONE',  ( 0.2886757222754123275, -82.00700602769721570, 1.241303401317177979 ) ) ;
#34569 = EDGE_LOOP ( 'NONE', ( #51618, #8450, #34954, #53182 ) ) ;
#34570 = CARTESIAN_POINT ( 'NONE',  ( 0.000000000000000000, -76.79999999999999716, 0.000000000000000000 ) ) ;
#34571 = CARTESIAN_POINT ( 'NONE',  ( 0.3926218265389159745, -79.25416666666666288, 1.460959015002474493 ) ) ;
#34572 = CARTESIAN_POINT ( 'NONE',  ( 7.372964296364999726, -79.14958221312299713, 9.618238180306001084 ) ) ;
#34573 = CARTESIAN_POINT ( 'NONE',  ( 0.000000000000000000, -87.70000000000000284, 0.000000000000000000 ) ) ;
#34574 = CARTESIAN_POINT ( 'NONE',  ( -0.7572724432162000197, -83.24215694101300755, 1.483977110291999857 ) ) ;
#34575 = CARTESIAN_POINT ( 'NONE',  ( -10.13785388426000011, -78.40114185044998862, -4.205702700205000255 ) ) ;
#34576 = CARTESIAN_POINT ( 'NONE',  ( 10.01676948373000009, -23.20938276584000093, -7.658894993369000481 ) ) ;
#34577 = CARTESIAN_POINT ( 'NONE',  ( -1.718598679952006991, -17.75037066954035225, 12.71111582768095438 ) ) ;
#34578 = EDGE_CURVE ( 'NONE', #53199, #27284, #6099, .T. ) ;
#34579 = CARTESIAN_POINT ( 'NONE',  ( -5.227273583242999067, -76.09884160047198520, -11.10057349953000028 ) ) ;
#34580 = CYLINDRICAL_SURFACE ( 'NONE', #39643, 2.500000000000000000 ) ;
#34581 = CARTESIAN_POINT ( 'NONE',  ( 1.250000000000000000, -78.75000000000000000, 0.000000000000000000 ) ) ;
#34582 = ORIENTED_EDGE ( 'NONE', *, *, #25263, .F. ) ;
#34583 = AXIS2_PLACEMENT_3D ( 'NONE', #10019, #32133, #50174 ) ;
#34584 = CARTESIAN_POINT ( 'NONE',  ( -5.182070223403000497, -78.55504929535699432, 9.738987759633999985 ) ) ;
#34585 = CARTESIAN_POINT ( 'NONE',  ( -0.9789787176784884304, -80.04688031827949146, 0.7776048570041739216 ) ) ;
#34586 = CARTESIAN_POINT ( 'NONE',  ( 12.56594317819999951, -55.54999998572999687, 1.750000000000000000 ) ) ;
#34587 = VECTOR ( 'NONE', #50162, 1000.000000000000000 ) ;
#34588 = VECTOR ( 'NONE', #56971, 1000.000000000000000 ) ;
#34589 = CARTESIAN_POINT ( 'NONE',  ( -3.642272407944000090, -79.27798916675298813, -10.66127506782999923 ) ) ;
#34590 = DIRECTION ( 'NONE',  ( 0.000000000000000000, 1.000000000000000000, 0.000000000000000000 ) ) ;
#34591 = CARTESIAN_POINT ( 'NONE',  ( 11.68767212001979594, -79.52916666666665435, -3.140974612311341563 ) ) ;
#34592 = LINE ( 'NONE', #52621, #53871 ) ;
#34593 = AXIS2_PLACEMENT_3D ( 'NONE', #55080, #50671, #50377 ) ;
#34594 = CARTESIAN_POINT ( 'NONE',  ( 1.291202636478971044, -83.05585137522281514, -0.7864065562573873125 ) ) ;
#34595 = CARTESIAN_POINT ( 'NONE',  ( 0.8323279321850197698, -79.78345157011268896, -0.9349414125349536642 ) ) ;
#34596 = DIRECTION ( 'NONE',  ( -1.000000000000000000, 0.000000000000000000, 0.000000000000000000 ) ) ;
#34597 = CARTESIAN_POINT ( 'NONE',  ( 1.667936697358999965, -22.76462890193000277, 12.53241208773999915 ) ) ;
#34598 = CARTESIAN_POINT ( 'NONE',  ( -9.396085398178650294, -76.24791666666668277, 7.220923959705211281 ) ) ;
#34599 = EDGE_LOOP ( 'NONE', ( #55387, #43703, #41915, #26389 ) ) ;
#34600 = ORIENTED_EDGE ( 'NONE', *, *, #45523, .T. ) ;
#34601 = B_SPLINE_CURVE_WITH_KNOTS ( 'NONE', 3,
 ( #22690, #53992, #40702, #18274, #17975, #12935 ),
 .UNSPECIFIED., .F., .F.,
 ( 4, 2, 4 ),
 ( 0.000000000000000000, 0.5000000000000000000, 1.000000000000000000 ),
 .UNSPECIFIED. ) ;
#34602 = CARTESIAN_POINT ( 'NONE',  ( -12.43356773662999970, -54.08739070985000552, -0.8411682846950000458 ) ) ;
#34603 = ORIENTED_EDGE ( 'NONE', *, *, #10602, .F. ) ;
#34604 = ORIENTED_EDGE ( 'NONE', *, *, #19989, .F. ) ;
#34605 = FACE_OUTER_BOUND ( 'NONE', #36419, .T. ) ;
#34606 = CARTESIAN_POINT ( 'NONE',  ( -8.496131438301000927, -77.51938450272599823, 6.855006679309999740 ) ) ;
#34608 = EDGE_CURVE ( 'NONE', #43155, #16765, #52958, .T. ) ;
#34607 = CARTESIAN_POINT ( 'NONE',  ( -9.090572324265000503, -78.22428667140098923, 3.947417077667999763 ) ) ;
#34609 = CARTESIAN_POINT ( 'NONE',  ( -1.020496043806678133, -78.21636009095580278, -9.194640008617911420 ) ) ;
#34610 = CARTESIAN_POINT ( 'NONE',  ( -10.71602610194999805, -79.67444737472000327, 3.314346869870000489 ) ) ;
#34611 = VERTEX_POINT ( 'NONE', #35505 ) ;
#34613 = ORIENTED_EDGE ( 'NONE', *, *, #13444, .T. ) ;
#34612 = ADVANCED_FACE ( 'NONE', ( #40244 ), #42009, .F. ) ;
#34614 = CARTESIAN_POINT ( 'NONE',  ( -1.980088454537020981, -77.49218653272571089, 9.036431384186325744 ) ) ;
#34615 = CARTESIAN_POINT ( 'NONE',  ( -9.177034484502000211, -77.26263836681899022, 6.137278520473000043 ) ) ;
#34616 = CIRCLE ( 'NONE', #16729, 0.5000000000000001110 ) ;
#34617 = CARTESIAN_POINT ( 'NONE',  ( -12.43646124691999866, -61.71751819588999410, 0.05236837569004999804 ) ) ;
#34618 = CARTESIAN_POINT ( 'NONE',  ( -6.766389538252999714, -77.89375126897199664, -6.956053621355001049 ) ) ;
#34619 = CARTESIAN_POINT ( 'NONE',  ( 9.346069275303429791, -61.96527745656915442, 8.620894635631328740 ) ) ;
#34620 = CARTESIAN_POINT ( 'NONE',  ( 9.073547343405500953, -53.57191135162067752, -8.894853367357773877 ) ) ;
#34621 = CARTESIAN_POINT ( 'NONE',  ( 3.942135768300999654, -80.08362823344599235, -10.54187931140000067 ) ) ;
#34622 = CARTESIAN_POINT ( 'NONE',  ( -9.722718241315000398, -60.04999999966999980, -7.247844507162001015 ) ) ;
#34623 = CARTESIAN_POINT ( 'NONE',  ( -7.648026768008000076, -55.55000001556999933, 10.12290050216000026 ) ) ;
#34624 = ADVANCED_FACE ( 'NONE', ( #30788 ), #39096, .T. ) ;
#34625 = VECTOR ( 'NONE', #30531, 1000.000000000000000 ) ;
#34626 = EDGE_LOOP ( 'NONE', ( #47294, #46890, #8432, #30785 ) ) ;
#34627 = AXIS2_PLACEMENT_3D ( 'NONE', #11034, #55597, #55895 ) ;
#34628 = CARTESIAN_POINT ( 'NONE',  ( -9.029856014839001688, -53.46737842902999915, 9.038878718651000455 ) ) ;
#34629 = CARTESIAN_POINT ( 'NONE',  ( 3.925078296951999501, -78.55011942976800299, 11.31856107452000160 ) ) ;
#34630 = CARTESIAN_POINT ( 'NONE',  ( -7.659225706236999720, -18.31732796024000010, -9.963487823496000928 ) ) ;
#34632 = CARTESIAN_POINT ( 'NONE',  ( -1.933504092460000212, -18.59593152724999854, -12.70940235707999832 ) ) ;
#34631 = CARTESIAN_POINT ( 'NONE',  ( 1.210855936474563910, -78.46461170675218000, 9.190418661073644913 ) ) ;
#34633 = CIRCLE ( 'NONE', #31808, 3.799999999999999822 ) ;
#34634 = CARTESIAN_POINT ( 'NONE',  ( -9.252740428348994683, -78.82083333333329733, -2.486604901413163926 ) ) ;
#34635 = DIRECTION ( 'NONE',  ( 0.000000000000000000, -1.000000000000000000, 0.000000000000000000 ) ) ;
#34636 = CARTESIAN_POINT ( 'NONE',  ( -7.743768518152000624, -77.38807570069999997, -8.177286450628999503 ) ) ;
#34637 = CARTESIAN_POINT ( 'NONE',  ( 2.851043015753209176, -3.499999999999999112, 1.899452699823827029 ) ) ;
#34638 = CARTESIAN_POINT ( 'NONE',  ( -5.539808784079931492, -80.11666666668466519, 9.611650271896815312 ) ) ;
#34639 = VERTEX_POINT ( 'NONE', #57961 ) ;
#34640 = CARTESIAN_POINT ( 'NONE',  ( -2.941324361237704910, -3.499999999999999556, -1.526268571259735252 ) ) ;
#34641 = B_SPLINE_CURVE_WITH_KNOTS ( 'NONE', 3,
 ( #14920, #48842, #30526, #17243, #43543, #56834, #8103, #44124, #47993, #20809, #8384, #16681, #3673, #12245, #57686, #35231, #26099, #21674, #52979, #16390, #48557, #21102, #2816, #53261 ),
 .UNSPECIFIED., .F., .F.,
 ( 4, 2, 2, 2, 2, 2, 2, 2, 2, 2, 2, 4 ),
 ( 0.000000000000000000, 0.1249999999999996114, 0.2499999999999992228, 0.3749999999999988343, 0.4374999999999983347, 0.4999999999999977796, 0.6249999999999967804, 0.7499999999999956701, 0.8124999999999947820, 0.8437499999999948930, 0.8749999999999951150, 1.000000000000000000 ),
 .UNSPECIFIED. ) ;
#34642 = DIRECTION ( 'NONE',  ( 1.000000000000000000, 0.000000000000000000, 0.000000000000000000 ) ) ;
#34643 = CARTESIAN_POINT ( 'NONE',  ( 2.852847297332000043, -3.410973948317999938, -2.519339706139999802 ) ) ;
#34644 = CARTESIAN_POINT ( 'NONE',  ( 2.940699877186000233, -79.37056235426499029, 8.954246345182999889 ) ) ;
#34645 = DIRECTION ( 'NONE',  ( -7.074008051008000492E-10, -1.000000000000000000, -4.749370611643999689E-10 ) ) ;
#34646 = DIRECTION ( 'NONE',  ( 1.000000000000000000, 0.000000000000000000, 0.000000000000000000 ) ) ;
#34647 = DIRECTION ( 'NONE',  ( 0.9999873237594404385, 0.000000000000000000, 0.005035108780572202306 ) ) ;
#34648 = DIRECTION ( 'NONE',  ( 0.000000000000000000, -0.7071067811866525998, -0.7071067811864425456 ) ) ;
#34649 = CARTESIAN_POINT ( 'NONE',  ( 2.877569803687999972, -84.07371544543099162, -2.724990427310999941 ) ) ;
#34650 = CARTESIAN_POINT ( 'NONE',  ( -12.00000000000000000, -18.75000000000000000, 0.000000000000000000 ) ) ;
#34651 = DIRECTION ( 'NONE',  ( 0.000000000000000000, -1.000000000000000000, 0.000000000000000000 ) ) ;
#34652 = CARTESIAN_POINT ( 'NONE',  ( -10.52498723879999964, -77.28216120838598613, 3.387147871870999971 ) ) ;
#34653 = CARTESIAN_POINT ( 'NONE',  ( 10.67369879590530424, -76.41529813363538892, -4.913311340196373500 ) ) ;
#34654 = CARTESIAN_POINT ( 'NONE',  ( -10.52129323452999898, -77.68207497455300370, 3.681981700656000278 ) ) ;
#34655 = CARTESIAN_POINT ( 'NONE',  ( 0.4596630180541980693, -81.94513611944643117, 1.162390080072868592 ) ) ;
#34656 = FACE_OUTER_BOUND ( 'NONE', #19453, .T. ) ;
#34657 = CARTESIAN_POINT ( 'NONE',  ( -0.5065222552852000071, -77.14901792243969680, 9.658707080791000266 ) ) ;
#34658 = CARTESIAN_POINT ( 'NONE',  ( 7.507056363060000237, -79.70894415034599945, -5.572808305725000189 ) ) ;
#34659 = CARTESIAN_POINT ( 'NONE',  ( -0.4479237788617201899, -0.8216145633097318157, -3.428385239426285480 ) ) ;
#34660 = CARTESIAN_POINT ( 'NONE',  ( -2.486379155175535871, -80.20678445994957428, -10.46580476966082962 ) ) ;
#34661 = EDGE_CURVE ( 'NONE', #31891, #3607, #6458, .T. ) ;
#34662 = CARTESIAN_POINT ( 'NONE',  ( 0.000000000000000000, -73.00000000000001421, 0.000000000000000000 ) ) ;
#34663 = CARTESIAN_POINT ( 'NONE',  ( 3.708203932500000022, -75.80000000000001137, 11.41267819554000162 ) ) ;
#34664 = CARTESIAN_POINT ( 'NONE',  ( 8.060167321886254399, -54.17936585327868215, 9.621722524767893248 ) ) ;
#34665 = CARTESIAN_POINT ( 'NONE',  ( -1.243547092045992564, -78.68541666666664014, 9.499999999999994671 ) ) ;
#34666 = CARTESIAN_POINT ( 'NONE',  ( -6.349996674360999904, -78.90074028895499225, -9.301156207373001195 ) ) ;
#34667 = VECTOR ( 'NONE', #55528, 1000.000000000000000 ) ;
#34668 = CARTESIAN_POINT ( 'NONE',  ( 10.75041758345825649, -77.36048236442238135, 1.407139100108084406 ) ) ;
#34669 = VERTEX_POINT ( 'NONE', #14247 ) ;
#34670 = CARTESIAN_POINT ( 'NONE',  ( -1.217390015647338064, -24.81893024926236890, 12.70229597940998012 ) ) ;
#34671 = ORIENTED_EDGE ( 'NONE', *, *, #34661, .T. ) ;
#34672 = ORIENTED_EDGE ( 'NONE', *, *, #25374, .F. ) ;
#34673 = DIRECTION ( 'NONE',  ( 0.000000000000000000, 0.000000000000000000, -1.000000000000000000 ) ) ;
#34674 = ORIENTED_EDGE ( 'NONE', *, *, #9705, .T. ) ;
#34675 = B_SPLINE_CURVE_WITH_KNOTS ( 'NONE', 3,
 ( #25217, #43237, #24932, #2508, #2794, #37632, #55650, #33190, #46819, #26076 ),
 .UNSPECIFIED., .F., .F.,
 ( 4, 2, 2, 2, 4 ),
 ( 0.000000000000000000, 0.2500000000000000000, 0.5000000000000000000, 0.7500000000000000000, 1.000000000000000000 ),
 .UNSPECIFIED. ) ;
#34676 = CARTESIAN_POINT ( 'NONE',  ( 2.136931703850000197, -79.41556330239998829, -2.883967052643999995 ) ) ;
#34677 = CARTESIAN_POINT ( 'NONE',  ( -6.771338525271339392, -79.33792608965413251, 6.663214335040369640 ) ) ;
#34678 = ORIENTED_EDGE ( 'NONE', *, *, #10441, .F. ) ;
#34679 = CARTESIAN_POINT ( 'NONE',  ( 12.16119841297000015, -78.66141265907999980, -1.092202732365999962 ) ) ;
#34680 = ORIENTED_EDGE ( 'NONE', *, *, #2312, .F. ) ;
#34681 = CARTESIAN_POINT ( 'NONE',  ( -9.250000000000000000, -79.49999999999998579, 1.813240672189999963E-14 ) ) ;
#34683 = EDGE_CURVE ( 'NONE', #44715, #43667, #32243, .T. ) ;
#34682 = ORIENTED_EDGE ( 'NONE', *, *, #3432, .T. ) ;
#34684 = DIRECTION ( 'NONE',  ( 0.000000000000000000, 0.000000000000000000, -1.000000000000000000 ) ) ;
#34685 = CARTESIAN_POINT ( 'NONE',  ( 12.49999990534960226, -13.07071424677999971, 0.001538265197309672755 ) ) ;
#34686 = B_SPLINE_SURFACE_WITH_KNOTS ( 'NONE', 3, 3, ( 
 ( #45583, #32837, #18996, #45878 ),
 ( #1295, #5697, #727, #41430 ),
 ( #23706, #4838, #41718, #19289 ),
 ( #5989, #36700, #55295, #22834 ),
 ( #147, #14842, #440, #54137 ),
 ( #18416, #13676, #31675, #49720 ),
 ( #54437, #9263, #27249, #31968 ),
 ( #1015, #50011, #9557, #27541 ),
 ( #5129, #23127, #41135, #54716 ),
 ( #36989, #9850, #37869, #10733 ),
 ( #29011, #24299, #1583, #46761 ),
 ( #42605, #19573, #28710, #37573 ),
 ( #33433, #55589, #6283, #15139 ),
 ( #6578, #19875, #2168, #42312 ),
 ( #1880, #51177, #55889, #33134 ),
 ( #15441, #51470, #11027, #47050 ),
 ( #24590, #20169, #23996, #42013 ) ),
 .UNSPECIFIED., .F., .F., .F.,
 ( 4, 1, 1, 1, 1, 1, 1, 1, 1, 1, 1, 1, 1, 1, 4 ),
 ( 4, 4 ),
 ( -0.01011398171657000057, 0.000000000000000000, 0.08333333333333001192, 0.1666666666667000196, 0.2500000000000000000, 0.3333333333333000081, 0.4166666666666999919, 0.5000000000000000000, 0.5833333333333000637, 0.6666666666667000474, 0.7500000000000000000, 0.8333333333333000637, 0.9166666666667000474, 1.000000000000000000, 1.010365777941000021 ),
 ( -0.3559705546970000078, 1.357612346710000084 ),
 .UNSPECIFIED. ) ;
#34687 = CARTESIAN_POINT ( 'NONE',  ( -8.506113518985836564, -80.04778286667620080, 6.573857701660976716 ) ) ;
#34688 = LINE ( 'NONE', #48018, #31482 ) ;
#34689 = CARTESIAN_POINT ( 'NONE',  ( -3.938198560205464993, -86.17851879815596305, -0.3769834764405665672 ) ) ;
#34690 = CARTESIAN_POINT ( 'NONE',  ( 9.776276929627000456, -76.04354117740300012, -5.431214116490000521 ) ) ;
#34691 = CARTESIAN_POINT ( 'NONE',  ( -13.07317008567999927, -77.51186929341000109, -1.028553310913000063 ) ) ;
#34692 = CARTESIAN_POINT ( 'NONE',  ( 9.100870196628985553, -77.07242046014692960, -3.274811821655061017 ) ) ;
#34693 = CARTESIAN_POINT ( 'NONE',  ( 9.723003665007999174, -76.67014927275398861, -5.142475670412999911 ) ) ;
#34694 = ADVANCED_FACE ( 'NONE', ( #5399 ), #10131, .T. ) ;
#34695 = CARTESIAN_POINT ( 'NONE',  ( -8.513832829815155989, -78.63200474943408835, -3.619427496593546678 ) ) ;
#34696 = CARTESIAN_POINT ( 'NONE',  ( -0.5470841013496000604, -79.76947588450499893, -1.216254552179000026 ) ) ;
#34697 = CARTESIAN_POINT ( 'NONE',  ( -10.95040223189505468, -80.10793889166065185, -1.053133452593003838 ) ) ;
#34698 = CARTESIAN_POINT ( 'NONE',  ( 2.837645820808837982, -2.891962703774921373, 1.585247691945158577 ) ) ;
#34699 = CARTESIAN_POINT ( 'NONE',  ( 1.665232602310000143, -79.65175264934788402, 3.129211432048999875 ) ) ;
#34700 = CARTESIAN_POINT ( 'NONE',  ( -5.799999999999999822, -80.99999999999998579, 0.000000000000000000 ) ) ;
#34701 = CARTESIAN_POINT ( 'NONE',  ( 0.9986783041480190581, -80.96805384704971686, 10.70471205834406625 ) ) ;
#34702 = CARTESIAN_POINT ( 'NONE',  ( -1.473190823115000159, -82.91469503318799639, 3.226649821350000114 ) ) ;
#34703 = CARTESIAN_POINT ( 'NONE',  ( -3.370587613551000228, -1.726292672027000208, 0.9429417476038000068 ) ) ;
#34704 = CARTESIAN_POINT ( 'NONE',  ( 1.250000000000000000, -81.24999999999998579, 0.000000000000000000 ) ) ;
#34705 = CARTESIAN_POINT ( 'NONE',  ( -7.646944885454000307, -59.99635956511999524, -10.19022188675999985 ) ) ;
#34706 = CARTESIAN_POINT ( 'NONE',  ( -10.87922314793346423, -79.26468826379790755, 5.174618772388034138 ) ) ;
#34707 = CARTESIAN_POINT ( 'NONE',  ( -0.8218343019581000330, -80.79405330277099040, -1.050237832603999832 ) ) ;
#34708 = CARTESIAN_POINT ( 'NONE',  ( 1.931087888240000217, -55.48415267986000288, 12.71658872082999814 ) ) ;
#34709 = CARTESIAN_POINT ( 'NONE',  ( 12.56884868898000107, -76.74651637867998488, -3.366471670097000324 ) ) ;
#34710 = CARTESIAN_POINT ( 'NONE',  ( 1.250000000000000000, -81.84999999999999432, 0.000000000000000000 ) ) ;
#34711 = CIRCLE ( 'NONE', #33797, 12.09999999999999964 ) ;
#34712 = LINE ( 'NONE', #56596, #36707 ) ;
#34713 = CARTESIAN_POINT ( 'NONE',  ( -1.726950059272000182, -75.69530751397000756, -12.24089000852000098 ) ) ;
#34714 = VERTEX_POINT ( 'NONE', #37267 ) ;
#34715 = CARTESIAN_POINT ( 'NONE',  ( 6.985849709488999970, -80.92822782980758234, -8.837815942395002011 ) ) ;
#34716 = CARTESIAN_POINT ( 'NONE',  ( -3.250000000000000000, 4.040000000000000036, 0.000000000000000000 ) ) ;
#34717 = B_SPLINE_CURVE_WITH_KNOTS ( 'NONE', 3,
 ( #36956, #23089, #44953, #49085, #4508, #22209, #22510, #40520, #113, #34469, #52217, #10394, #11493, #2910, #23957, #3205, #15909 ),
 .UNSPECIFIED., .F., .F.,
 ( 4, 2, 1, 2, 2, 2, 2, 2, 4 ),
 ( 0.000000000000000000, 0.04878227772541878643, 0.09756455545083757286, 0.1463468331762563523, 0.1951291109016751457, 0.2439113886270939391, 0.2926936663525128157, 0.3414759440779315813, 0.3902582218033504580 ),
 .UNSPECIFIED. ) ;
#34718 = CARTESIAN_POINT ( 'NONE',  ( 12.78037829250999913, -61.09316779356999660, 1.812823010630000065 ) ) ;
#34719 = CARTESIAN_POINT ( 'NONE',  ( -12.00000000000000000, -78.89999999999999147, -1.868256502752000067E-14 ) ) ;
#34720 = CARTESIAN_POINT ( 'NONE',  ( 0.8456326333846000409, -78.58901425910798366, -9.484475825334998333 ) ) ;
#34721 = CARTESIAN_POINT ( 'NONE',  ( 3.474217323525000012, -82.26950239379898733, -1.986488251467000143 ) ) ;
#34722 = CARTESIAN_POINT ( 'NONE',  ( 4.235425280252315794, -79.94290626548179546, 9.880369340961230762 ) ) ;
#34723 = CARTESIAN_POINT ( 'NONE',  ( 0.7212099693301999848, -80.38286640014699458, 1.333715969168000059 ) ) ;
#34724 = VERTEX_POINT ( 'NONE', #50577 ) ;
#34725 = ADVANCED_FACE ( 'NONE', ( #49707, #28109 ), #50286, .F. ) ;
#34726 = CARTESIAN_POINT ( 'NONE',  ( 9.898965768568219303, -77.31804819846105659, -4.223239295616174616 ) ) ;
#34727 = CARTESIAN_POINT ( 'NONE',  ( 0.8355970340055913770, -82.13932291666422714, 1.088690951272730523 ) ) ;
#34728 = CARTESIAN_POINT ( 'NONE',  ( 3.621447497675001070, -78.99318692614360771, 7.242894995350030563 ) ) ;
#34729 = ORIENTED_EDGE ( 'NONE', *, *, #28413, .T. ) ;
#34730 = ADVANCED_FACE ( 'NONE', ( #23695 ), #28301, .F. ) ;
#34731 = CARTESIAN_POINT ( 'NONE',  ( 10.28297802758999957, -78.09309102680099102, -3.734674224488999883 ) ) ;
#34732 = CARTESIAN_POINT ( 'NONE',  ( -8.188331488387619927, -55.57158755757377122, -7.345153731672218633 ) ) ;
#34733 = CARTESIAN_POINT ( 'NONE',  ( 10.59805651207999944, -80.08569813701798523, 4.006234447635000251 ) ) ;
#34734 = ORIENTED_EDGE ( 'NONE', *, *, #33219, .T. ) ;
#34735 = CARTESIAN_POINT ( 'NONE',  ( -10.67791114319000023, -78.72947827561399947, -5.583725037239000599 ) ) ;
#34736 = EDGE_LOOP ( 'NONE', ( #27712, #40573, #13590, #210 ) ) ;
#34737 = ORIENTED_EDGE ( 'NONE', *, *, #23477, .T. ) ;
#34738 = CIRCLE ( 'NONE', #9314, 5.000000000000000888 ) ;
#34739 = CARTESIAN_POINT ( 'NONE',  ( 1.176455637918473185, -80.37807892517056985, 0.4310529391067065008 ) ) ;
#34740 = B_SPLINE_CURVE_WITH_KNOTS ( 'NONE', 3,
 ( #16231, #11232, #57243, #43105, #34210, #56388, #34792, #52247, #38366, #24797, #20939, #11804, #25365, #42811, #56102, #2663, #47554, #15938 ),
 .UNSPECIFIED., .F., .F.,
 ( 4, 2, 2, 2, 2, 2, 2, 2, 4 ),
 ( 0.000000000000000000, 0.1250000000000000000, 0.2500000000000000000, 0.3750000000000000000, 0.5000000000000000000, 0.6250000000000000000, 0.7500000000000000000, 0.8750000000000000000, 1.000000000000000000 ),
 .UNSPECIFIED. ) ;
#34741 = CARTESIAN_POINT ( 'NONE',  ( -3.620209226088999976, -86.25171438269200053, 1.611820996859000044 ) ) ;
#34742 = DIRECTION ( 'NONE',  ( 0.000000000000000000, 1.000000000000000000, 0.000000000000000000 ) ) ;
#34743 = ORIENTED_EDGE ( 'NONE', *, *, #7202, .T. ) ;
#34744 = CARTESIAN_POINT ( 'NONE',  ( 3.250377508590382991, -2.361707286923234950, 0.4258434008466360221 ) ) ;
#34746 = EDGE_CURVE ( 'NONE', #39067, #42771, #9290, .T. ) ;
#34745 = VERTEX_POINT ( 'NONE', #28403 ) ;
#34747 = CARTESIAN_POINT ( 'NONE',  ( -3.463460669170729478, -80.69899254569148184, -10.20046286209545983 ) ) ;
#34748 = CARTESIAN_POINT ( 'NONE',  ( 3.778552491321001128, -78.99318692756679638, -1.395910297075086959E-15 ) ) ;
#34749 = B_SPLINE_CURVE_WITH_KNOTS ( 'NONE', 3,
 ( #14083, #39563, #26269, #32078, #23238, #16558, #41244, #34541, #52574, #30111, #1406, #55113, #11139, #51288, #56000, #19397, #19105, #28819, #6395, #28230, #33543, #24111, #41535, #18815, #55704, #42128, #32367, #46868, #15253, #37097, #10843, #14953, #42426, #32950, #36806, #24410, #47161, #6691, #50994, #10543, #32655, #54825, #1694, #28527, #46576, #14657, #1995, #19988, #14367, #6102, #19687, #27940, #37688, #33245, #15547, #51582, #45988, #24700, #23524, #1118, #55630, #1922, #54759, #45920, #37325, #41762, #1339, #5455, #32880, #46214, #15184, #50925, #36741, #51220, #14302, #32295, #10773, #50638, #23457, #19916, #1627, #28751, #50342, #55931, #15482, #10473, #55047, #46507, #33472, #19040, #14595, #32589, #5741, #28164, #23748, #57368, #24630, #52371, #42641, #16062, #39065, #20208, #12207, #38199, #56219, #47674, #30193, #56507, #48242, #51799, #26627, #35483, #40523, #31643, #13350, #31349, #49686, #49390, #17204, #48515, #407, #4512, #30767, #30488, #27217, #22805, #12771, #22512, #17496, #21918, #45255, #12490 ),
 .UNSPECIFIED., .F., .F.,
 ( 4, 2, 2, 2, 2, 2, 1, 1, 1, 1, 1, 2, 2, 2, 2, 2, 1, 1, 1, 1, 2, 2, 2, 2, 2, 1, 1, 1, 2, 2, 2, 2, 1, 1, 1, 1, 1, 2, 2, 2, 2, 2, 1, 1, 1, 2, 2, 2, 2, 2, 1, 1, 1, 1, 1, 1, 2, 2, 2, 2, 2, 1, 1, 1, 1, 2, 2, 2, 2, 1, 1, 1, 2, 2, 2, 2, 1, 1, 1, 1, 1, 2, 2, 2, 4 ),
 ( 0.000000000000000000, 0.06250000000000682787, 0.1250000000000136557, 0.1875000000000204559, 0.2187500000000238420, 0.2343750000000255629, 0.2421875000000264511, 0.2460937500000268674, 0.2480468750000270617, 0.2490234375000272560, 0.2495117187500273392, 0.2497558593750273392, 0.2500000000000273670, 0.2812500000000348610, 0.2968750000000385247, 0.3046875000000404121, 0.3085937500000413003, 0.3105468750000417999, 0.3115234375000421330, 0.3120117187500422995, 0.3122558593750424105, 0.3125000000000424660, 0.3437500000000606182, 0.3593750000000696665, 0.3671875000000742739, 0.3710937500000765499, 0.3730468750000777156, 0.3740234375000782707, 0.3745117187500785483, 0.3750000000000788258, 0.4062500000000975331, 0.4218750000001068035, 0.4296875000001114664, 0.4335937500001137423, 0.4355468750001149081, 0.4365234375001154632, 0.4370117187501157408, 0.4372558593751158518, 0.4375000000001159073, 0.4687500000001304512, 0.4843750000001376677, 0.4921875000001413314, 0.4960937500001431077, 0.4980468750001439959, 0.4990234375001444400, 0.4995117187501446621, 0.5000000000001448841, 0.6250000000002021716, 0.6875000000002308154, 0.7187500000002450262, 0.7343750000002522427, 0.7421875000002557954, 0.7460937500002575717, 0.7480468750002584599, 0.7490234375002589040, 0.7495117187502592371, 0.7497558593752592371, 0.7500000000002592371, 0.7812500000002334799, 0.7968750000002204903, 0.8046875000002140510, 0.8085937500002108314, 0.8105468750002091660, 0.8115234375002082778, 0.8120117187502078338, 0.8122558593752075007, 0.8125000000002072786, 0.8437500000001729727, 0.8593750000001559863, 0.8671875000001473266, 0.8710937500001431077, 0.8730468750001408873, 0.8740234375001398881, 0.8750000000001388889, 0.9062500000001064704, 0.9218750000000902611, 0.9296875000000821565, 0.9335937500000780487, 0.9355468750000760503, 0.9365234375000750511, 0.9370117187500744960, 0.9372558593750741629, 0.9375000000000738298, 0.9687500000000369704, 1.000000000000000000 ),
 .UNSPECIFIED. ) ;
#34750 = CARTESIAN_POINT ( 'NONE',  ( 7.948094694382998426, -54.35965255578000210, 9.636752590464999102 ) ) ;
#34751 = AXIS2_PLACEMENT_3D ( 'NONE', #471, #9881, #14291 ) ;
#34752 = CARTESIAN_POINT ( 'NONE',  ( 0.3926218265389159745, -81.25416666666667709, 1.460959015002474493 ) ) ;
#34753 = CARTESIAN_POINT ( 'NONE',  ( -3.044681358458452003, -77.30245510314006196, -11.37321520970169431 ) ) ;
#34754 = CARTESIAN_POINT ( 'NONE',  ( -12.70556836324321281, -16.77227722580009939, -0.2598513551437900415 ) ) ;
#34755 = CARTESIAN_POINT ( 'NONE',  ( -10.26943924278000075, -78.60695423824412842, 6.168847710361000658 ) ) ;
#34756 = EDGE_CURVE ( 'NONE', #47867, #36570, #39591, .T. ) ;
#34757 = CARTESIAN_POINT ( 'NONE',  ( 5.246383657897999875, -77.46100733245999947, -10.79237965019999912 ) ) ;
#34758 = CARTESIAN_POINT ( 'NONE',  ( 1.328206530128999807, -76.58160288575999175, -12.23810562210000086 ) ) ;
#34759 = ADVANCED_FACE ( 'NONE', ( #8586 ), #37275, .F. ) ;
#34760 = CARTESIAN_POINT ( 'NONE',  ( -3.559953446648999709, -80.08155496681199281, 2.176417643061999918 ) ) ;
#34761 = CARTESIAN_POINT ( 'NONE',  ( 5.492755632425520673, -77.13749999994708162, -7.555491190735147633 ) ) ;
#34762 = CARTESIAN_POINT ( 'NONE',  ( -12.77301916226999978, -16.94808379552999966, 1.052060437765000023 ) ) ;
#34763 = CARTESIAN_POINT ( 'NONE',  ( 5.539808784079867543, -77.93333333333333712, 9.611650271896852615 ) ) ;
#34764 = CARTESIAN_POINT ( 'NONE',  ( -10.85634995915000012, -76.03702797665600599, -5.741293403527000017 ) ) ;
#34765 = CARTESIAN_POINT ( 'NONE',  ( 1.748323643227931434, -79.96240695551148292, 10.92574688943145844 ) ) ;
#34766 = CARTESIAN_POINT ( 'NONE',  ( -0.8031675853856999892, -1.684977233352999981, 4.044120181570000305 ) ) ;
#34767 = CARTESIAN_POINT ( 'NONE',  ( 1.250000000000000000, -78.75000000000000000, 0.000000000000000000 ) ) ;
#34768 = B_SPLINE_CURVE_WITH_KNOTS ( 'NONE', 3,
 ( #22667, #40678, #54263, #35340, #13796, #9386, #27375, #30628, #21777, #48947, #8491, #32094, #14096, #36822, #27665, #50134, #45709, #5246 ),
 .UNSPECIFIED., .F., .F.,
 ( 4, 2, 2, 2, 2, 2, 2, 2, 4 ),
 ( 0.000000000000000000, 0.1249999999999999722, 0.2500000000000000000, 0.3750000000000000000, 0.5000000000000001110, 0.6250000000000001110, 0.7500000000000000000, 0.8750000000000000000, 1.000000000000000000 ),
 .UNSPECIFIED. ) ;
#34769 = CARTESIAN_POINT ( 'NONE',  ( 1.906446389314999879, -1.641372700497000015, 3.546581172111999525 ) ) ;
#34770 = CARTESIAN_POINT ( 'NONE',  ( 1.479781043334260859, -80.47666266983802075, -0.4561458805849814557 ) ) ;
#34771 = DIRECTION ( 'NONE',  ( 8.423204520001998884E-11, 1.000000000000000000, -1.870146057550999887E-10 ) ) ;
#34772 = CARTESIAN_POINT ( 'NONE',  ( 1.577356090230000119, -78.17520242672080144, 0.3451975780249000314 ) ) ;
#34773 = DIRECTION ( 'NONE',  ( 0.000000000000000000, -1.000000000000000000, 0.000000000000000000 ) ) ;
#34774 = CARTESIAN_POINT ( 'NONE',  ( 2.891311992273000175, -2.268041850768999890, 2.073108726819999692 ) ) ;
#34775 = CARTESIAN_POINT ( 'NONE',  ( 10.96171043400000045, -78.08619942611500164, -5.535041421897999747 ) ) ;
#34776 = DIRECTION ( 'NONE',  ( -1.000000000000000000, 0.000000000000000000, 0.000000000000000000 ) ) ;
#34778 = EDGE_CURVE ( 'NONE', #11225, #37628, #21179, .T. ) ;
#34777 = AXIS2_PLACEMENT_3D ( 'NONE', #57090, #38505, #16657 ) ;
#34780 = CARTESIAN_POINT ( 'NONE',  ( 9.599999999999999645, -87.59999999999999432, 0.000000000000000000 ) ) ;
#34779 = CARTESIAN_POINT ( 'NONE',  ( -9.696018661907480407, -75.80000000000001137, 6.813282359576399827 ) ) ;
#34781 = CARTESIAN_POINT ( 'NONE',  ( 0.3210957952920999725, -81.22411572283999703, -1.312678830453999801 ) ) ;
#34782 = CARTESIAN_POINT ( 'NONE',  ( -4.927957436858316775, -79.51302443800736341, 9.553899519113622674 ) ) ;
#34783 = ORIENTED_EDGE ( 'NONE', *, *, #10734, .T. ) ;
#34784 = CARTESIAN_POINT ( 'NONE',  ( -10.53101990620000095, -18.69360215052999763, -7.613962745610000304 ) ) ;
#34785 = CARTESIAN_POINT ( 'NONE',  ( 8.459138740827000902, -79.37812103921298501, -8.569435492024000567 ) ) ;
#34786 = CARTESIAN_POINT ( 'NONE',  ( -3.141535938717197496, -79.15175190257748739, 8.986458492157693101 ) ) ;
#34787 = CARTESIAN_POINT ( 'NONE',  ( 11.44417895085271475, -77.02916666666666856, -3.075537641221520069 ) ) ;
#34788 = LINE ( 'NONE', #22082, #4993 ) ;
#34789 = CIRCLE ( 'NONE', #9364, 9.950000000000001066 ) ;
#34790 = CARTESIAN_POINT ( 'NONE',  ( 3.237649453555000001, -1.422597686686999818, -2.108892360458999971 ) ) ;
#34791 = CARTESIAN_POINT ( 'NONE',  ( -9.582886764941999758, -79.13235384747198964, 1.297353921085000028 ) ) ;
#34792 = CARTESIAN_POINT ( 'NONE',  ( 6.043427764450807871, -78.06666666666666288, -10.48543666025108756 ) ) ;
#34793 = CARTESIAN_POINT ( 'NONE',  ( 0.000000000000000000, -46.09579702914000165, 0.000000000000000000 ) ) ;
#34794 = VERTEX_POINT ( 'NONE', #44826 ) ;
#34795 = CARTESIAN_POINT ( 'NONE',  ( 3.042547531669000271, -78.64783470746900207, -10.31045122763999977 ) ) ;
#34796 = AXIS2_PLACEMENT_3D ( 'NONE', #14283, #39981, #8398 ) ;
#34797 = CARTESIAN_POINT ( 'NONE',  ( -14.00000000000000000, -72.70000000000000284, 0.000000000000000000 ) ) ;
#34798 = FACE_OUTER_BOUND ( 'NONE', #33751, .T. ) ;
#34799 = ADVANCED_FACE ( 'NONE', ( #4381 ), #22096, .T. ) ;
#34800 = CARTESIAN_POINT ( 'NONE',  ( 3.914500761937000028, -78.48547955770028750, 0.000000000000000000 ) ) ;
#34801 = CARTESIAN_POINT ( 'NONE',  ( -1.529754383668999962, -81.42117201505999446, -0.6588408878327000062 ) ) ;
#34802 = ORIENTED_EDGE ( 'NONE', *, *, #16639, .F. ) ;
#34803 = CARTESIAN_POINT ( 'NONE',  ( 7.985065670160999218, -77.74030535679999332, 7.712612023391999472 ) ) ;
#34804 = DIRECTION ( 'NONE',  ( 0.000000000000000000, 1.000000000000000000, 0.000000000000000000 ) ) ;
#34805 = CARTESIAN_POINT ( 'NONE',  ( 0.000000000000000000, -75.20000000000000284, 0.000000000000000000 ) ) ;
#34806 = CARTESIAN_POINT ( 'NONE',  ( -12.60413670423000099, -60.10716680829000325, 1.799502287691000069 ) ) ;
#34807 = CARTESIAN_POINT ( 'NONE',  ( 0.3271848554490964789, -78.35416666666665719, 1.217465845835395521 ) ) ;
#34808 = CARTESIAN_POINT ( 'NONE',  ( 1.739862777674999972, -79.07029435458399291, 9.611119481339999382 ) ) ;
#34809 = VERTEX_POINT ( 'NONE', #13521 ) ;
#34810 = ORIENTED_EDGE ( 'NONE', *, *, #9937, .T. ) ;
#34811 = CARTESIAN_POINT ( 'NONE',  ( -9.952602430950999945, -76.70740172182600247, 7.514132727938000578 ) ) ;
#34812 = CARTESIAN_POINT ( 'NONE',  ( 2.106029303673160324, -78.74082198396830279, -10.54159598279656329 ) ) ;
#34813 = ORIENTED_EDGE ( 'NONE', *, *, #41370, .T. ) ;
#34814 = CARTESIAN_POINT ( 'NONE',  ( 10.00844281758000065, -18.63109810616999695, 7.647097920691000361 ) ) ;
#34815 = CARTESIAN_POINT ( 'NONE',  ( 5.417173251955453850, -79.02203476639424196, -8.051588635942257710 ) ) ;
#34816 = AXIS2_PLACEMENT_3D ( 'NONE', #53527, #44674, #4227 ) ;
#34817 = LINE ( 'NONE', #7966, #22334 ) ;
#34818 = CARTESIAN_POINT ( 'NONE',  ( 7.228795249850000104, -77.84130236656999102, -10.56189739613000000 ) ) ;
#34819 = CARTESIAN_POINT ( 'NONE',  ( 6.433795189870999742, -77.42361205349585873, -9.188274595716000803 ) ) ;
#34820 = CARTESIAN_POINT ( 'NONE',  ( 7.714303428875997959, -26.30294702886003222, 12.53545825868000385 ) ) ;
#34821 = CARTESIAN_POINT ( 'NONE',  ( -0.5301359684276694129, -86.40321104920798234, 4.263478205968190160 ) ) ;
#34822 = CARTESIAN_POINT ( 'NONE',  ( -9.735611069857000643, -79.36032251751400679, 5.570995215215999607 ) ) ;
#34823 = CARTESIAN_POINT ( 'NONE',  ( -0.7835675759065233725, -79.98183763911107746, 9.216734333713379357 ) ) ;
#34824 = DIRECTION ( 'NONE',  ( -0.9999999999999693578, 2.479738203407925921E-07, -1.117914101428966396E-12 ) ) ;
#34825 = EDGE_LOOP ( 'NONE', ( #12039, #41446, #2027 ) ) ;
#34826 = CARTESIAN_POINT ( 'NONE',  ( -9.688835989853998854, -79.66343168043698597, -5.749381838710999837 ) ) ;
#34827 = CARTESIAN_POINT ( 'NONE',  ( 8.684857183346831988, -77.32189494946037200, -3.221164999357318592 ) ) ;
#34828 = CARTESIAN_POINT ( 'NONE',  ( -1.390602365772999782, -80.78170427028999256, 0.2763432473779000587 ) ) ;
#34829 = CARTESIAN_POINT ( 'NONE',  ( -0.9728543758959999899, -78.16750647927929663, -1.031316509929999903 ) ) ;
#34830 = LINE ( 'NONE', #48163, #42665 ) ;
#34831 = CIRCLE ( 'NONE', #48103, 9.599999999999999645 ) ;
#34832 = FACE_OUTER_BOUND ( 'NONE', #37082, .T. ) ;
#34833 = DIRECTION ( 'NONE',  ( 1.000000000000000000, 0.000000000000000000, 0.000000000000000000 ) ) ;
#34834 = CYLINDRICAL_SURFACE ( 'NONE', #27158, 3.600000000000000089 ) ;
#34835 = CARTESIAN_POINT ( 'NONE',  ( -7.654537085030999499, -18.71943307332999851, 10.01332844637000008 ) ) ;
#34836 = CARTESIAN_POINT ( 'NONE',  ( -9.595360835209000072, -79.59955593965399601, -5.693913425678999829 ) ) ;
#34837 = CARTESIAN_POINT ( 'NONE',  ( 10.21380041493000057, -22.77152778045000048, -7.668936932623999780 ) ) ;
#34838 = CARTESIAN_POINT ( 'NONE',  ( -0.9038093657317438634, -83.04000885484705918, 0.8629080614449039510 ) ) ;
#34839 = CARTESIAN_POINT ( 'NONE',  ( 4.115840777475000323, -80.89192428167199012, -0.6829423103135000561 ) ) ;
#34840 = CARTESIAN_POINT ( 'NONE',  ( 9.393203674808260573, -77.79166666666665719, 5.413904038987188194 ) ) ;
#34841 = EDGE_LOOP ( 'NONE', ( #5727, #24390, #17104, #18951, #22158, #44929 ) ) ;
#34842 = CARTESIAN_POINT ( 'NONE',  ( -3.820214278402727093, -77.19999999999998863, 10.15434263821451566 ) ) ;
#34843 = CARTESIAN_POINT ( 'NONE',  ( 1.298035947816999824, -80.66793607721000114, -0.6866955795318000488 ) ) ;
#34844 = CARTESIAN_POINT ( 'NONE',  ( -3.250000000000000000, -2.000000000000000000, 0.000000000000000000 ) ) ;
#34845 = CARTESIAN_POINT ( 'NONE',  ( -10.61596739836999959, -78.53665897790600070, -5.551333230057999835 ) ) ;
#34846 = CARTESIAN_POINT ( 'NONE',  ( -12.76303204294999993, -23.26485150694999859, 1.980584515756000030 ) ) ;
#34847 = CARTESIAN_POINT ( 'NONE',  ( -0.7803569495551999635, -81.79738077595999357, -1.471836271561000054 ) ) ;
#34848 = CARTESIAN_POINT ( 'NONE',  ( 8.219513559211000242, -78.92490194988499752, 5.194554602171000290 ) ) ;
#34849 = CARTESIAN_POINT ( 'NONE',  ( 9.589208240076997569, -78.96433849994599541, 0.8944121949827000817 ) ) ;
#34851 = EDGE_CURVE ( 'NONE', #54228, #29062, #49449, .T. ) ;
#34850 = CARTESIAN_POINT ( 'NONE',  ( -0.006333666751428999701, -53.46737355666999747, -12.77652491951000080 ) ) ;
#34852 = FACE_OUTER_BOUND ( 'NONE', #31214, .T. ) ;
#34853 = CARTESIAN_POINT ( 'NONE',  ( -0.5999999999999999778, -5.000000000000000000, 4.000000000000000000 ) ) ;
#34854 = CARTESIAN_POINT ( 'NONE',  ( 3.576074390005977488, -85.88547955769999476, -1.592170899228049441 ) ) ;
#34855 = VERTEX_POINT ( 'NONE', #12299 ) ;
#34856 = FACE_OUTER_BOUND ( 'NONE', #3813, .T. ) ;
#34857 = CARTESIAN_POINT ( 'NONE',  ( -2.841500632089049017, -2.143116487617794608, -1.636193441488569267 ) ) ;
#34858 = CARTESIAN_POINT ( 'NONE',  ( -6.516581675540000340, -79.40704064464900114, -10.39800818482999922 ) ) ;
#34859 = CARTESIAN_POINT ( 'NONE',  ( 3.914500761936999140, -78.48547955770027329, -2.310234204170795280 ) ) ;
#34860 = AXIS2_PLACEMENT_3D ( 'NONE', #53361, #44221, #35336 ) ;
#34861 = CARTESIAN_POINT ( 'NONE',  ( 1.531359430757999851, -82.54740557480100449, -0.6558942768039000004 ) ) ;
#34862 = CARTESIAN_POINT ( 'NONE',  ( 1.508420534579999917, -77.69816034697798557, 11.11497989572000122 ) ) ;
#34863 = CARTESIAN_POINT ( 'NONE',  ( 7.788493169598000421, -78.68206539377699471, 7.733265204867000087 ) ) ;
#34864 = CARTESIAN_POINT ( 'NONE',  ( 1.583004792647870307, -17.54790758843439491, 12.70616254411041801 ) ) ;
#34865 = CARTESIAN_POINT ( 'NONE',  ( 0.4178879169752000022, -76.13657433877699532, -12.26266848588000080 ) ) ;
#34866 = CARTESIAN_POINT ( 'NONE',  ( 0.000000000000000000, -76.75499999999999545, 0.000000000000000000 ) ) ;
#34867 = CARTESIAN_POINT ( 'NONE',  ( 0.000000000000000000, -6.000000000000000000, 0.000000000000000000 ) ) ;
#34868 = ORIENTED_EDGE ( 'NONE', *, *, #12944, .T. ) ;
#34869 = CARTESIAN_POINT ( 'NONE',  ( -10.64923527428000050, -79.68499373684099396, 3.293689214829000012 ) ) ;
#34870 = CARTESIAN_POINT ( 'NONE',  ( 5.452652381452083752, -77.32493831431021647, 7.507522693077579135 ) ) ;
#34871 = CARTESIAN_POINT ( 'NONE',  ( -10.71369944335148361, -78.17916666666667425, 2.879226727952040044 ) ) ;
#34872 = ADVANCED_FACE ( 'NONE', ( #47757 ), #38216, .F. ) ;
#34873 = CARTESIAN_POINT ( 'NONE',  ( -10.30593458266999995, -78.27435544289399161, -4.275431210322000020 ) ) ;
#34874 = DIRECTION ( 'NONE',  ( 0.000000000000000000, 0.000000000000000000, -1.000000000000000000 ) ) ;
#34875 = CARTESIAN_POINT ( 'NONE',  ( 0.3270994294228949939, -78.95440165101413754, 1.217085255381527009 ) ) ;
#34876 = CIRCLE ( 'NONE', #30160, 6.100000000000000533 ) ;
#34877 = CARTESIAN_POINT ( 'NONE',  ( -0.3126037839058401491, -82.45865881358655258, -1.517344252390254722 ) ) ;
#34878 = CARTESIAN_POINT ( 'NONE',  ( 11.61659281346613781, -76.93273162705501989, -2.077594685895145066 ) ) ;
#34879 = CIRCLE ( 'NONE', #29236, 0.8000000000000000444 ) ;
#34880 = ADVANCED_FACE ( 'NONE', ( #48049 ), #43897, .F. ) ;
#34881 = CARTESIAN_POINT ( 'NONE',  ( -1.001315002657000131, -61.48522411647999775, 12.50000000000000000 ) ) ;
#34882 = CARTESIAN_POINT ( 'NONE',  ( -12.70249480710866230, -61.76498603269881471, -0.9989402950384759228 ) ) ;
#34883 = EDGE_CURVE ( 'NONE', #46040, #57635, #26858, .T. ) ;
#34884 = CARTESIAN_POINT ( 'NONE',  ( 1.538071403319964281, -76.16458333333332575, 11.75000000000000711 ) ) ;
#34885 = VERTEX_POINT ( 'NONE', #52458 ) ;
#34886 = ORIENTED_EDGE ( 'NONE', *, *, #21888, .F. ) ;
#34887 = CARTESIAN_POINT ( 'NONE',  ( -12.77651065919999951, -53.49103388577999851, 0.04307580168117999125 ) ) ;
#34888 = ORIENTED_EDGE ( 'NONE', *, *, #52060, .F. ) ;
#34889 = FACE_OUTER_BOUND ( 'NONE', #13466, .T. ) ;
#34890 = ORIENTED_EDGE ( 'NONE', *, *, #17233, .F. ) ;
#34891 = CARTESIAN_POINT ( 'NONE',  ( -0.2440801457610911052, -81.00000000000000000, -10.96803368417560876 ) ) ;
#34892 = CARTESIAN_POINT ( 'NONE',  ( -10.30400671801000101, -77.54662084572800040, 3.605941145585999763 ) ) ;
#34893 = CARTESIAN_POINT ( 'NONE',  ( 8.546298008199000762, -78.96463667140099574, -5.018094164374000243 ) ) ;
#34894 = CARTESIAN_POINT ( 'NONE',  ( -9.805641529082999241, -79.23866588669099542, -5.446788484474000214 ) ) ;
#34895 = ORIENTED_EDGE ( 'NONE', *, *, #27890, .T. ) ;
#34896 = ORIENTED_EDGE ( 'NONE', *, *, #33394, .T. ) ;
#34897 = CARTESIAN_POINT ( 'NONE',  ( -5.437822718421641888, -77.52503815049138325, 7.482785194970384524 ) ) ;
#34898 = CARTESIAN_POINT ( 'NONE',  ( 10.94195044575999987, -77.54892574480697931, -1.468969119710000104 ) ) ;
#34899 = PRESENTATION_STYLE_ASSIGNMENT (( #35475 ) ) ;
#34900 = CARTESIAN_POINT ( 'NONE',  ( -12.55486071739000131, -60.95393632975000031, -1.580832792523999775 ) ) ;
#34901 = CARTESIAN_POINT ( 'NONE',  ( 8.444976262095000408, -78.12114190200398411, 4.780490068936999570 ) ) ;
#34902 = CARTESIAN_POINT ( 'NONE',  ( 7.678690995240000206, -20.24351820077000141, 10.59551070215999857 ) ) ;
#34903 = ADVANCED_BREP_SHAPE_REPRESENTATION ( '', ( #36811, #43526 ), #52000 ) ;
#34904 = CARTESIAN_POINT ( 'NONE',  ( -9.055506177563403369, -79.42412239826263942, -2.871540687672356373 ) ) ;
#34905 = DIRECTION ( 'NONE',  ( 0.4045837981834735086, 0.8201365133286462328, 0.4045837981834735086 ) ) ;
#34906 = CARTESIAN_POINT ( 'NONE',  ( -3.493617039247999934, -80.46877773805297807, -10.33892454317000187 ) ) ;
#34907 = FACE_OUTER_BOUND ( 'NONE', #51273, .T. ) ;
#34908 = CARTESIAN_POINT ( 'NONE',  ( 4.658475568430830549, -78.66666666666665719, -8.082524092276877070 ) ) ;
#34909 = ORIENTED_EDGE ( 'NONE', *, *, #11133, .T. ) ;
#34910 = CARTESIAN_POINT ( 'NONE',  ( -5.582142573279000430, -79.09604631854099921, -10.84844757254999870 ) ) ;
#34911 = CARTESIAN_POINT ( 'NONE',  ( -7.645391692591000599, -55.58469634128999814, 10.18949678826999872 ) ) ;
#34912 = CARTESIAN_POINT ( 'NONE',  ( -10.61596739836999959, -78.74002463773399541, -5.551333230057999835 ) ) ;
#34913 = CARTESIAN_POINT ( 'NONE',  ( -8.798041828550999810, -17.06186490710999948, -8.790609563012999672 ) ) ;
#34914 = CIRCLE ( 'NONE', #83, 1.199999999999999956 ) ;
#34916 = CARTESIAN_POINT ( 'NONE',  ( 12.76303204291999904, -55.53514849259999409, 1.980584515756000030 ) ) ;
#34915 = LINE ( 'NONE', #30494, #38184 ) ;
#34917 = LINE ( 'NONE', #21071, #52478 ) ;
#34918 = SURFACE_STYLE_USAGE ( .BOTH. , #57377 ) ;
#34919 = PLANE ( 'NONE',  #37073 ) ;
#34920 = CARTESIAN_POINT ( 'NONE',  ( -11.07095105964000048, -78.38183842717499772, 1.299477954992000139 ) ) ;
#34921 = FACE_OUTER_BOUND ( 'NONE', #46448, .T. ) ;
#34922 = CARTESIAN_POINT ( 'NONE',  ( 11.08684999561000062, -80.58721576625140415, 1.943057827011999805 ) ) ;
#34923 = ORIENTED_EDGE ( 'NONE', *, *, #26958, .F. ) ;
#34924 = CARTESIAN_POINT ( 'NONE',  ( 9.984017254981603529, -80.28079889738930319, 4.071156503779067570 ) ) ;
#34925 = CARTESIAN_POINT ( 'NONE',  ( 2.061649843245999758, -55.59438692379999480, 12.83797346712000120 ) ) ;
#34926 = CARTESIAN_POINT ( 'NONE',  ( 7.651147547633000201, -19.23743349724999874, -10.45204383579999963 ) ) ;
#34927 = CARTESIAN_POINT ( 'NONE',  ( 3.129541869639000051, -2.920362276481999864, -2.166049510376999887 ) ) ;
#34928 = CARTESIAN_POINT ( 'NONE',  ( 6.249458598087999306, -79.83812488639198079, 7.054820424332000073 ) ) ;
#34929 = CARTESIAN_POINT ( 'NONE',  ( 1.750000000001000089, -23.24999998674999802, -12.56594318051000059 ) ) ;
#34930 = DIRECTION ( 'NONE',  ( -1.194297873234000201E-10, 1.000000000000000000, -5.211291098350999982E-10 ) ) ;
#34931 = DIRECTION ( 'NONE',  ( -1.000000000000000000, 0.000000000000000000, 0.000000000000000000 ) ) ;
#34932 = CARTESIAN_POINT ( 'NONE',  ( 1.636761686205427058, -3.166666666666666519, -2.839805762151336399 ) ) ;
#34933 = CARTESIAN_POINT ( 'NONE',  ( 1.276300174619999783, -84.43832450217399810, 3.928048035916000380 ) ) ;
#34934 = CARTESIAN_POINT ( 'NONE',  ( -9.000000000000000000, -0.2000000000000000111, 0.000000000000000000 ) ) ;
#34935 = EDGE_CURVE ( 'NONE', #37820, #46551, #57972, .T. ) ;
#34936 = CARTESIAN_POINT ( 'NONE',  ( -1.873308010621101083, -77.06556246648871422, -11.87619401410840325 ) ) ;
#34937 = VECTOR ( 'NONE', #22329, 1000.000000000000000 ) ;
#34938 = CARTESIAN_POINT ( 'NONE',  ( -0.03884788386675075422, -76.32452440415889328, -11.74979495016792796 ) ) ;
#34939 = CARTESIAN_POINT ( 'NONE',  ( -3.573177736666999671, -77.04238470710198783, 10.43715168250999881 ) ) ;
#34940 = CARTESIAN_POINT ( 'NONE',  ( 0.4751859727251985799, -81.94403392660923657, 1.156120668747460334 ) ) ;
#34941 = CARTESIAN_POINT ( 'NONE',  ( 1.750000000001000089, -59.55100836327999758, -12.60354432391999957 ) ) ;
#34942 = CARTESIAN_POINT ( 'NONE',  ( 7.559982449049000408, -76.90594942799179989, -6.032732969207000195 ) ) ;
#34943 = CARTESIAN_POINT ( 'NONE',  ( 9.539544502573999551, -79.26434415034600534, 0.5400218831816999687 ) ) ;
#34944 = CARTESIAN_POINT ( 'NONE',  ( 3.251229025254284366, -3.362671771015649291, 0.5096591584606244840 ) ) ;
#34945 = CARTESIAN_POINT ( 'NONE',  ( -5.781545516559535081, -80.17986992905298393, -9.063146604324529676 ) ) ;
#34946 = CARTESIAN_POINT ( 'NONE',  ( 4.299999999999999822, -81.99999999999998579, 0.000000000000000000 ) ) ;
#34947 = CARTESIAN_POINT ( 'NONE',  ( -1.135826688880000157, -81.40663953506998496, -0.9797437077257000748 ) ) ;
#34948 = EDGE_LOOP ( 'NONE', ( #4775, #14147, #22272, #1238 ) ) ;
#34949 = CARTESIAN_POINT ( 'NONE',  ( 7.652056849482000267, -79.38624118732400348, 9.281873293285000770 ) ) ;
#34950 = DIRECTION ( 'NONE',  ( -3.675129103447999014E-09, -0.9999999999999997780, 2.168720876821999677E-08 ) ) ;
#34951 = EDGE_CURVE ( 'NONE', #35616, #9151, #29047, .T. ) ;
#34952 = CARTESIAN_POINT ( 'NONE',  ( -0.4163023988263999664, -79.44546714899098561, -11.25436168207999899 ) ) ;
#34953 = CARTESIAN_POINT ( 'NONE',  ( -12.00000000000000000, -18.84999999999999787, -0.5999999999999999778 ) ) ;
#34954 = ORIENTED_EDGE ( 'NONE', *, *, #12181, .F. ) ;
#34955 = B_SPLINE_CURVE_WITH_KNOTS ( 'NONE', 3,
 ( #12701, #40148, #52295, #29832, #47883, #7415 ),
 .UNSPECIFIED., .F., .F.,
 ( 4, 2, 4 ),
 ( 0.000000000000000000, 0.5000000000000000000, 1.000000000000000000 ),
 .UNSPECIFIED. ) ;
#34956 = CARTESIAN_POINT ( 'NONE',  ( 7.709155920934510853, -60.72747430363504151, 9.998700314201467876 ) ) ;
#34957 = CONICAL_SURFACE ( 'NONE', #52892, 0.6999999997695030007, 0.7853981633972997312 ) ;
#34958 = VERTEX_POINT ( 'NONE', #53918 ) ;
#34959 = VERTEX_POINT ( 'NONE', #22613 ) ;
#34960 = AXIS2_PLACEMENT_3D ( 'NONE', #24425, #38860, #28833 ) ;
#34961 = CYLINDRICAL_SURFACE ( 'NONE', #52730, 11.05000000000000071 ) ;
#34962 = CARTESIAN_POINT ( 'NONE',  ( -3.263865106102529889, -78.77708333023421972, -1.096753143766827643 ) ) ;
#34963 = CARTESIAN_POINT ( 'NONE',  ( 5.472379214682000281, -79.74019400902800214, -9.446080217779000421 ) ) ;
#34964 = CARTESIAN_POINT ( 'NONE',  ( -6.865937273109800287, -79.33902379046836018, 6.565646674124808513 ) ) ;
#34965 = ORIENTED_EDGE ( 'NONE', *, *, #37116, .T. ) ;
#34966 = CARTESIAN_POINT ( 'NONE',  ( 3.042547531669000271, -78.24783470746899638, -10.31045122763999977 ) ) ;
#34967 = CARTESIAN_POINT ( 'NONE',  ( 7.135759946468999360, -79.17960427995001282, -10.09022804928999939 ) ) ;
#34968 = VERTEX_POINT ( 'NONE', #53614 ) ;
#34969 = FACE_OUTER_BOUND ( 'NONE', #10655, .T. ) ;
#34970 = CARTESIAN_POINT ( 'NONE',  ( -2.807719666672398695, -79.80000000000001137, 11.69429938913882694 ) ) ;
#34971 = ADVANCED_FACE ( 'NONE', ( #22905 ), #50079, .F. ) ;
#34972 = CARTESIAN_POINT ( 'NONE',  ( -10.59627636761023339, -80.08682005774406321, 1.811415407155257729 ) ) ;
#34973 = PLANE ( 'NONE',  #37155 ) ;
#34974 = CARTESIAN_POINT ( 'NONE',  ( 3.241578942234940808, -86.36264282632899381, -1.443243930775132133 ) ) ;
#34975 = CARTESIAN_POINT ( 'NONE',  ( -10.19999999921000011, -0.2000000007865999907, 1.811583764860000079E-09 ) ) ;
#34976 = CARTESIAN_POINT ( 'NONE',  ( -10.31502378008536880, -79.09895833336493354, 5.961239727259085797 ) ) ;
#34977 = CARTESIAN_POINT ( 'NONE',  ( -1.300896064473999969, -80.10182505433999722, -0.3655689422679000433 ) ) ;
#34978 = CARTESIAN_POINT ( 'NONE',  ( 10.91568895729999866, -76.21867431695000050, 1.352609846672000016 ) ) ;
#34979 = CARTESIAN_POINT ( 'NONE',  ( -1.250000000000000000, -18.55321828668999729, -12.50000000000000000 ) ) ;
#34980 = CIRCLE ( 'NONE', #4839, 0.5000000000000004441 ) ;
#34981 = CARTESIAN_POINT ( 'NONE',  ( -1.334654685515000105, -82.29771400872598974, -3.731581711997999928 ) ) ;
#34982 = LINE ( 'NONE', #25561, #49694 ) ;
#34983 = CARTESIAN_POINT ( 'NONE',  ( -2.298892750299144083, -3.037928567523061396, 2.296935490278543490 ) ) ;
#34984 = CARTESIAN_POINT ( 'NONE',  ( -3.026296275368999922, -80.08155496681199281, 1.850160319665000053 ) ) ;
#34985 = EDGE_CURVE ( 'NONE', #26753, #7317, #5114, .T. ) ;
#34986 = FACE_OUTER_BOUND ( 'NONE', #13056, .T. ) ;
#34987 = CARTESIAN_POINT ( 'NONE',  ( 1.077708808469999946, -83.70524735065198740, -3.376907981158000283 ) ) ;
#34988 = CARTESIAN_POINT ( 'NONE',  ( -0.8385792221450999451, -2.889988518283999941, -3.712528424878000166 ) ) ;
#34989 = CARTESIAN_POINT ( 'NONE',  ( -0.04771467012325169427, -80.62837193105833933, 1.273752274804522244 ) ) ;
#34990 = ORIENTED_EDGE ( 'NONE', *, *, #35614, .F. ) ;
#34991 = CARTESIAN_POINT ( 'NONE',  ( 8.596418555780417137, -80.19791666666667140, -6.606377239730353956 ) ) ;
#34992 = CARTESIAN_POINT ( 'NONE',  ( -11.85739648576925909, -79.28587530551916984, 2.129864859879342820 ) ) ;
#34993 = CARTESIAN_POINT ( 'NONE',  ( -1.321095329625999959, -82.18904536324399146, -0.1826337427822999904 ) ) ;
#34994 = CARTESIAN_POINT ( 'NONE',  ( -9.500000000000001776, -78.90666666666666629, -0.7958701389094111622 ) ) ;
#34995 = CARTESIAN_POINT ( 'NONE',  ( 12.61117499582000079, -23.21550664553999965, 1.798980867984000032 ) ) ;
#34996 = CIRCLE ( 'NONE', #21816, 1.750000000000001332 ) ;
#34997 = CARTESIAN_POINT ( 'NONE',  ( -5.539808784079887083, -79.78333333333333144, -9.611650271896841957 ) ) ;
#34998 = CARTESIAN_POINT ( 'NONE',  ( 1.782734487911076027, -24.12245368561141490, -12.71547286926152864 ) ) ;
#34999 = CARTESIAN_POINT ( 'NONE',  ( -9.216780614190000165, -76.52341425608999259, 8.238619774073001167 ) ) ;
#35000 = VERTEX_POINT ( 'NONE', #40916 ) ;
#35001 = EDGE_CURVE ( 'NONE', #48492, #31399, #55156, .T. ) ;
#35002 = CARTESIAN_POINT ( 'NONE',  ( 10.99960575394902129, -80.99614106727162266, -0.5334183479100040870 ) ) ;
#35003 = DIRECTION ( 'NONE',  ( 0.000000000000000000, 0.000000000000000000, 1.000000000000000000 ) ) ;
#35004 = EDGE_CURVE ( 'NONE', #47059, #48866, #54363, .T. ) ;
#35005 = CARTESIAN_POINT ( 'NONE',  ( 12.61277705616999967, -59.99666672496000075, 1.798399175679000095 ) ) ;
#35006 = CARTESIAN_POINT ( 'NONE',  ( -2.062597265787999845, -22.78461666469000235, -12.87024489156999962 ) ) ;
#35007 = CARTESIAN_POINT ( 'NONE',  ( 2.217690073412000196, -79.10064318342999456, -9.260249588150999855 ) ) ;
#35008 = CARTESIAN_POINT ( 'NONE',  ( 4.174306380842000230, -82.38975280906599608, -0.06567313222218000568 ) ) ;
#35009 = CARTESIAN_POINT ( 'NONE',  ( 4.239312547723716129, -79.94287370176201080, 9.878703068895035244 ) ) ;
#35010 = CARTESIAN_POINT ( 'NONE',  ( -1.347695613438000040, -80.08519065986000385, -0.6947364142266000409 ) ) ;
#35011 = ORIENTED_EDGE ( 'NONE', *, *, #29687, .T. ) ;
#35012 = CARTESIAN_POINT ( 'NONE',  ( 2.365578933032910669, -78.95508126976140773, 9.023057518257136422 ) ) ;
#35013 = B_SPLINE_CURVE_WITH_KNOTS ( 'NONE', 3,
 ( #11496, #21773, #30908, #3770, #22360, #26482 ),
 .UNSPECIFIED., .F., .F.,
 ( 4, 1, 1, 4 ),
 ( 0.000000000000000000, 0.3333333333333000081, 0.6666666666667000474, 1.000000000000000000 ),
 .UNSPECIFIED. ) ;
#35014 = CARTESIAN_POINT ( 'NONE',  ( -1.242879273300786513, -78.85062977682864016, -3.768395784351273647 ) ) ;
#35015 = ORIENTED_EDGE ( 'NONE', *, *, #3364, .T. ) ;
#35016 = CARTESIAN_POINT ( 'NONE',  ( -8.178338515874335357, -55.49583131490307153, -7.356278612544859818 ) ) ;
#35017 = ADVANCED_FACE ( 'NONE', ( #13743 ), #29684, .F. ) ;
#35018 = CARTESIAN_POINT ( 'NONE',  ( -10.75000000000000000, -80.50000000000000000, -1.711887504597999906E-14 ) ) ;
#35019 = EDGE_LOOP ( 'NONE', ( #46925, #13465, #13328, #38615, #21323, #43049, #38465, #14138, #36488 ) ) ;
#35020 = MECHANICAL_DESIGN_GEOMETRIC_PRESENTATION_REPRESENTATION (  '', ( #48261 ), #34064 ) ;
#35021 = B_SPLINE_CURVE_WITH_KNOTS ( 'NONE', 3,
 ( #46382, #5906, #33352, #33923, #51099, #37200, #28922, #10650, #33641, #46679, #35866, #27002, #50849, #10395, #45037, #4590, #55259, #9306, #19252, #23958, #18172, #37535, #6244, #24261, #42277, #16854, #43728, #24842, #24551, #21272, #25416, #25699, #57290, #56723, #3280 ),
 .UNSPECIFIED., .F., .F.,
 ( 4, 2, 2, 2, 1, 1, 2, 2, 2, 2, 1, 1, 2, 2, 2, 2, 1, 2, 2, 4 ),
 ( 0.000000000000000000, 0.1250000000000194011, 0.1875000000000297817, 0.2187500000000348055, 0.2343750000000359990, 0.2421875000000349443, 0.2460937500000344447, 0.2500000000000339173, 0.3750000000000124900, 0.4375000000000017764, 0.4687499999999963918, 0.4843749999999936162, 0.4921874999999931721, 0.4999999999999927280, 0.6249999999999864553, 0.6874999999999840128, 0.7187499999999836797, 0.7343749999999844569, 0.7499999999999851230, 1.000000000000000000 ),
 .UNSPECIFIED. ) ;
#35022 = ORIENTED_EDGE ( 'NONE', *, *, #54521, .T. ) ;
#35023 = ORIENTED_EDGE ( 'NONE', *, *, #37434, .T. ) ;
#35024 = CYLINDRICAL_SURFACE ( 'NONE', #21035, 0.5000000000000000000 ) ;
#35025 = CARTESIAN_POINT ( 'NONE',  ( -3.453171399369999950, -1.863032031399000088, -0.5706200895263999762 ) ) ;
#35026 = ORIENTED_EDGE ( 'NONE', *, *, #27080, .T. ) ;
#35027 = CARTESIAN_POINT ( 'NONE',  ( 10.98449626305583671, -18.69382183571523726, 0.5845794248139535298 ) ) ;
#35028 = ORIENTED_EDGE ( 'NONE', *, *, #20538, .F. ) ;
#35029 = CARTESIAN_POINT ( 'NONE',  ( 9.708203932502000200, -79.25000000000000000, -7.053423027506000587 ) ) ;
#35030 = CARTESIAN_POINT ( 'NONE',  ( -3.913805347717917105, -78.91452044229970397, 0.07378289354579982418 ) ) ;
#35031 = CIRCLE ( 'NONE', #8632, 1.749999999999999334 ) ;
#35032 = CARTESIAN_POINT ( 'NONE',  ( 7.658900722992000532, -55.59059707800999917, 10.01676258972999989 ) ) ;
#35033 = CARTESIAN_POINT ( 'NONE',  ( -7.718346056094000041, -21.74888345808999901, -10.07719973192000040 ) ) ;
#35034 = CARTESIAN_POINT ( 'NONE',  ( 5.790379964274294800, -79.57682291666264973, 7.536004867747862157 ) ) ;
#35035 = CARTESIAN_POINT ( 'NONE',  ( -8.255731568163469092, -80.90898308749885359, -7.584690471252304889 ) ) ;
#35036 = CARTESIAN_POINT ( 'NONE',  ( -1.436413824931296546, -77.87453550735162366, -0.4659587443401291829 ) ) ;
#35037 = CARTESIAN_POINT ( 'NONE',  ( 8.545990964147081925, -78.81890182048778115, -3.539321513413446585 ) ) ;
#35038 = CARTESIAN_POINT ( 'NONE',  ( -9.934814764470999648, -24.62368287829000124, 7.968971842743999723 ) ) ;
#35039 = CARTESIAN_POINT ( 'NONE',  ( -0.4363934998635000118, -80.49350264934798815, -4.152006803154999481 ) ) ;
#35040 = ADVANCED_FACE ( 'NONE', ( #23196, #58037 ), #41201, .T. ) ;
#35041 = CARTESIAN_POINT ( 'NONE',  ( -2.575222906043999949, -77.21666001420199166, 9.530972118016000749 ) ) ;
#35042 = LINE ( 'NONE', #8486, #292 ) ;
#35043 = CARTESIAN_POINT ( 'NONE',  ( -10.71369944335148183, -78.07916666666665151, 2.879226727952040932 ) ) ;
#35044 = DIRECTION ( 'NONE',  ( -1.000000000000000000, 0.000000000000000000, 0.000000000000000000 ) ) ;
#35045 = CARTESIAN_POINT ( 'NONE',  ( -6.272971974831354380, -80.02293377770999427, 9.114735501174534349 ) ) ;
#35046 = PLANE ( 'NONE',  #53638 ) ;
#35047 = DIRECTION ( 'NONE',  ( 0.000000000000000000, 0.000000000000000000, -1.000000000000000000 ) ) ;
#35048 = CARTESIAN_POINT ( 'NONE',  ( -0.9492059026655267351, -80.77846795208610331, 1.175833850632304278 ) ) ;
#35049 = CARTESIAN_POINT ( 'NONE',  ( -6.176117940694000552, -77.38832598960298981, 7.205939610817000407 ) ) ;
#35050 = CARTESIAN_POINT ( 'NONE',  ( -1.347317391812999920, -79.44859309350199794, -0.7577098654840999092 ) ) ;
#35051 = CARTESIAN_POINT ( 'NONE',  ( -8.096452064242996016, -22.78578169018999944, -13.15643568217000769 ) ) ;
#35052 = CARTESIAN_POINT ( 'NONE',  ( 0.9838624519628998977, -2.321243309748000083, 3.418988675016000123 ) ) ;
#35053 = B_SPLINE_CURVE_WITH_KNOTS ( 'NONE', 3,
 ( #28614, #50201, #46659, #31873, #9462, #45483, #23030, #41045, #634, #18616, #9751, #45784, #41334, #29758, #16499, #42793, #56083, #7346 ),
 .UNSPECIFIED., .F., .F.,
 ( 4, 2, 2, 2, 2, 2, 2, 2, 4 ),
 ( 0.000000000000000000, 0.1249999999999999722, 0.2500000000000000000, 0.3750000000000000000, 0.5000000000000001110, 0.6250000000000001110, 0.7500000000000000000, 0.8750000000000000000, 1.000000000000000000 ),
 .UNSPECIFIED. ) ;
#35054 = CARTESIAN_POINT ( 'NONE',  ( -11.77559907170000031, -77.89629421814900923, -3.482965070681999897 ) ) ;
#35055 = LINE ( 'NONE', #43948, #25970 ) ;
#35057 = CARTESIAN_POINT ( 'NONE',  ( 1.154392285689999742, -78.95172720777699737, -0.6387050628028000387 ) ) ;
#35056 = DIRECTION ( 'NONE',  ( 1.000000000000000000, 1.534883903844000000E-11, -3.930229729684000008E-14 ) ) ;
#35058 = CARTESIAN_POINT ( 'NONE',  ( -1.211920851286000023, -81.18216705308998371, -0.6339750518301998650 ) ) ;
#35059 = CARTESIAN_POINT ( 'NONE',  ( -5.099192467852374122, -79.51443440021429865, 9.463776008281715946 ) ) ;
#35060 = VERTEX_POINT ( 'NONE', #53318 ) ;
#35061 = CARTESIAN_POINT ( 'NONE',  ( -12.00000000000000355, -78.89293765275958492, 1.064976873965742366 ) ) ;
#35062 = CARTESIAN_POINT ( 'NONE',  ( 8.263989999164000011, -79.07297727176099045, 8.606143803265000614 ) ) ;
#35063 = CARTESIAN_POINT ( 'NONE',  ( -2.546082409442600447, -79.14654788605089664, 9.173657452411669411 ) ) ;
#35064 = EDGE_CURVE ( 'NONE', #56422, #23208, #30374, .T. ) ;
#35065 = CARTESIAN_POINT ( 'NONE',  ( 11.75000000000000000, -77.04999999999999716, 0.000000000000000000 ) ) ;
#35066 = CARTESIAN_POINT ( 'NONE',  ( -10.71369944335148183, -79.07916666666666572, 2.879226727952040932 ) ) ;
#35067 = AXIS2_PLACEMENT_3D ( 'NONE', #21342, #15761, #11349 ) ;
#35068 = CARTESIAN_POINT ( 'NONE',  ( -10.75000000000000000, -77.00000000000000000, 0.000000000000000000 ) ) ;
#35069 = CARTESIAN_POINT ( 'NONE',  ( 1.673403667841999898, -79.34562022128699255, -9.636531604483000280 ) ) ;
#35070 = CARTESIAN_POINT ( 'NONE',  ( 12.54977961484000026, -25.04832888628999754, 0.03757501521676000211 ) ) ;
#35071 = DIRECTION ( 'NONE',  ( 0.000000000000000000, 1.000000000000000000, 0.000000000000000000 ) ) ;
#35072 = ORIENTED_EDGE ( 'NONE', *, *, #12669, .F. ) ;
#35073 = DIRECTION ( 'NONE',  ( -0.3090169943748909409, 0.000000000000000000, 0.9510565162951718499 ) ) ;
#35074 = CARTESIAN_POINT ( 'NONE',  ( 2.846957383478000203, -79.67206001420200323, 9.316630448266000286 ) ) ;
#35075 = DIRECTION ( 'NONE',  ( 0.000000000000000000, 1.000000000000000000, 0.000000000000000000 ) ) ;
#35076 = FACE_OUTER_BOUND ( 'NONE', #1378, .T. ) ;
#35077 = CARTESIAN_POINT ( 'NONE',  ( 1.356773869401999955, -79.58955477686998847, -0.9668579442890000708 ) ) ;
#35078 = AXIS2_PLACEMENT_3D ( 'NONE', #24839, #38988, #43724 ) ;
#35079 = EDGE_CURVE ( 'NONE', #42463, #9508, #14619, .T. ) ;
#35080 = VERTEX_POINT ( 'NONE', #28777 ) ;
#35081 = DIRECTION ( 'NONE',  ( -0.7071067811864976127, 0.7071067811865975328, 1.603636560452993712E-09 ) ) ;
#35082 = CARTESIAN_POINT ( 'NONE',  ( -9.500000000000000000, -78.38958333333334849, 1.243547092045920399 ) ) ;
#35083 = CARTESIAN_POINT ( 'NONE',  ( -1.232226823489766199, -54.27709088663590364, -12.50408896745906340 ) ) ;
#35084 = EDGE_CURVE ( 'NONE', #52197, #49440, #14325, .T. ) ;
#35085 = ORIENTED_EDGE ( 'NONE', *, *, #22404, .T. ) ;
#35086 = CIRCLE ( 'NONE', #33210, 1.000000000000000000 ) ;
#35087 = CARTESIAN_POINT ( 'NONE',  ( 1.001315001700999963, -54.11477588220000001, 12.50000000000000000 ) ) ;
#35088 = CARTESIAN_POINT ( 'NONE',  ( -9.038965287750000854, -53.46737759073999996, -9.029769469428000406 ) ) ;
#35089 = CIRCLE ( 'NONE', #11587, 12.80000000000000071 ) ;
#35090 = CARTESIAN_POINT ( 'NONE',  ( 9.647254834573999460, -80.00735905321899111, -1.526580663425000095 ) ) ;
#35091 = ORIENTED_EDGE ( 'NONE', *, *, #57860, .T. ) ;
#35092 = ORIENTED_EDGE ( 'NONE', *, *, #48052, .T. ) ;
#35093 = CARTESIAN_POINT ( 'NONE',  ( 4.323029931973999318, -76.84458834893798951, -11.57148487019000171 ) ) ;
#35094 = DIRECTION ( 'NONE',  ( -1.000000000000000000, 0.000000000000000000, 0.000000000000000000 ) ) ;
#35095 = ORIENTED_EDGE ( 'NONE', *, *, #32965, .T. ) ;
#35096 = CARTESIAN_POINT ( 'NONE',  ( 4.001451577097999923, -77.96945194988499850, 8.339717337904000161 ) ) ;
#35097 = DIRECTION ( 'NONE',  ( 0.7071067811865475727, 0.000000000000000000, -0.7071067811865475727 ) ) ;
#35098 = LINE ( 'NONE', #57552, #4678 ) ;
#35099 = EDGE_CURVE ( 'NONE', #57123, #23864, #20313, .T. ) ;
#35100 = CARTESIAN_POINT ( 'NONE',  ( -1.930860503447785925, -55.02582494032501614, 12.72930866328045418 ) ) ;
#35101 = CARTESIAN_POINT ( 'NONE',  ( -9.082935096011000908, -77.23075131599000542, -9.017176053435999705 ) ) ;
#35102 = CARTESIAN_POINT ( 'NONE',  ( 2.976864594307000011, -77.39637571049389919, -10.81463766284999828 ) ) ;
#35103 = CARTESIAN_POINT ( 'NONE',  ( 3.965107357241011155, -86.25171435493598437, 0.4551303408108293702 ) ) ;
#35104 = CARTESIAN_POINT ( 'NONE',  ( 6.766402264611000028, -79.57821326152900099, -8.946167390840999545 ) ) ;
#35105 = CARTESIAN_POINT ( 'NONE',  ( 1.403051294136565819, -79.96338502862796815, 9.142673906005519768 ) ) ;
#35106 = CARTESIAN_POINT ( 'NONE',  ( 8.620934061286547490, -16.83470696674769229, 9.346030177879564249 ) ) ;
#35107 = ORIENTED_EDGE ( 'NONE', *, *, #17154, .T. ) ;
#35108 = CARTESIAN_POINT ( 'NONE',  ( 4.209725253073815843, -77.26262135689660226, -8.236522718530926213 ) ) ;
#35109 = CARTESIAN_POINT ( 'NONE',  ( -1.327188084842999993, -79.29332556885799477, 0.06657717027841000834 ) ) ;
#35110 = LINE ( 'NONE', #39561, #11657 ) ;
#35111 = CONICAL_SURFACE ( 'NONE', #4973, 5.249999999862000166, 0.7853981633972997312 ) ;
#35112 = CARTESIAN_POINT ( 'NONE',  ( -10.31421052434999908, -76.82175206120300004, 3.823226550887000030 ) ) ;
#35114 = ADVANCED_FACE ( 'NONE', ( #5763 ), #37348, .T. ) ;
#35113 = CARTESIAN_POINT ( 'NONE',  ( -1.146672249030999957, -77.62752668643429388, 0.4628715253012000153 ) ) ;
#35115 = CARTESIAN_POINT ( 'NONE',  ( 12.64500484462999985, -22.77152778045000048, 1.799490225533999732 ) ) ;
#35116 = CARTESIAN_POINT ( 'NONE',  ( 11.44417895085270054, -76.57083333333333997, 3.075537641221564922 ) ) ;
#35117 = CARTESIAN_POINT ( 'NONE',  ( -1.750000000000000000, -23.24999999688999708, 12.50000000000000000 ) ) ;
#35118 = DIRECTION ( 'NONE',  ( 1.000000000000000000, 0.000000000000000000, 0.000000000000000000 ) ) ;
#35119 = EDGE_CURVE ( 'NONE', #23138, #46623, #32611, .T. ) ;
#35120 = CARTESIAN_POINT ( 'NONE',  ( 9.178372771442999678, -78.26048704979598369, -6.069379357596000446 ) ) ;
#35121 = DIRECTION ( 'NONE',  ( 0.000000000000000000, -1.000000000000000000, 0.000000000000000000 ) ) ;
#35122 = CARTESIAN_POINT ( 'NONE',  ( -8.596418555780431348, -79.55208333333332860, -6.606377239730338857 ) ) ;
#35123 = CARTESIAN_POINT ( 'NONE',  ( -0.06100561046413999905, -79.80967046134098553, 4.171670386524000129 ) ) ;
#35124 = CIRCLE ( 'NONE', #1251, 13.89999999999999858 ) ;
#35125 = B_SPLINE_SURFACE_WITH_KNOTS ( 'NONE', 3, 3, ( 
 ( #51172, #20448, #15721, #20735, #11881, #29573, #47630, #7445, #7153, #55883, #28704, #39023, #34004, #3020, #25154, #21017, #43180, #24583, #47042, #6274, #2735, #19868, #51464, #38732, #56751, #16311, #11019, #34292, #29285, #52326, #15133, #42307, #2162, #37863, #29003 ),
 ( #20162, #33130, #6572, #10726, #42599, #38151, #56173, #35437, #7730, #58187, #49046, #44614, #44318, #48756, #39881, #53179, #53466, #12728, #3308, #44037, #4169, #8888, #26883, #53769, #30148, #39597, #21302, #22462, #39310, #34865, #34579, #31299, #13008, #35738, #44907 ),
 ( #4463, #30721, #8593, #26011, #40175, #57600, #52611, #57320, #16884, #12162, #57035, #17451, #8303, #31008, #48198, #26303, #17161, #22167, #13305, #26580, #17750, #49342, #16594, #52895, #25730, #43756, #3873, #12445, #57894, #30441, #21873, #8014, #48471, #3587, #21591 ),
 ( #35147, #1219, #9183, #49637, #54643, #40766, #41639, #36910, #55213, #36038, #31595, #32178, #40474, #5333, #27463, #36624, #27169, #19209, #18339, #5048, #5616, #18916, #45206, #37201, #32465, #28044, #27754, #50218, #23340, #14182, #54921, #9766, #4754, #45501, #46090 ) ),
 .UNSPECIFIED., .F., .F., .F.,
 ( 4, 4 ),
 ( 4, 1, 1, 1, 1, 1, 1, 1, 1, 1, 1, 1, 1, 1, 1, 1, 1, 1, 1, 1, 1, 1, 1, 1, 1, 1, 1, 1, 1, 1, 1, 1, 4 ),
 ( -0.1772706441294000235, 1.177270644128999955 ),
 ( -0.01390847417841000085, 0.008692796361505999644, 0.03129406690142000347, 0.05389533744134000076, 0.07649660798125000605, 0.09909787852116999640, 0.1216991490611000065, 0.1443004196010000129, 0.1669016901409000053, 0.1895029606807999978, 0.2121042312206999902, 0.2347055017607000138, 0.2573067723006000063, 0.2799080428405000265, 0.3025093133803999912, 0.3251105839203000114, 0.3477118544601999761, 0.3703131250002000274, 0.3929143955401000476, 0.4155156660800000124, 0.4381169366199000326, 0.4607182071597999973, 0.4833194776997000175, 0.5059207482395999822, 0.5285220187796000335, 0.5511232893194999427, 0.5737245598593999629, 0.5963258303992999831, 0.6189271009392000034, 0.6415283714791000236, 0.6641296420191000749, 0.6867309125589999841, 0.7093321830989000043 ),
 .UNSPECIFIED. ) ;
#35126 = ORIENTED_EDGE ( 'NONE', *, *, #40364, .F. ) ;
#35127 = CARTESIAN_POINT ( 'NONE',  ( 0.6444261930239000291, -82.67414080993400205, 1.576239777183000124 ) ) ;
#35128 = CARTESIAN_POINT ( 'NONE',  ( -1.251342548660999920, -81.48916334729999278, 0.5102646838515999539 ) ) ;
#35129 = CARTESIAN_POINT ( 'NONE',  ( 12.80000000000000071, -2.900000000000000355, 0.000000000000000000 ) ) ;
#35130 = CARTESIAN_POINT ( 'NONE',  ( -8.885616033064000163, -78.00760259185899770, 8.035041515002001589 ) ) ;
#35131 = CARTESIAN_POINT ( 'NONE',  ( 4.056922300394875336, -77.00000000000000000, 8.335976438453148063 ) ) ;
#35132 = VECTOR ( 'NONE', #22672, 1000.000000000000000 ) ;
#35133 = CARTESIAN_POINT ( 'NONE',  ( -0.6811744818814000624, -82.30265449683999179, -1.520282978132999840 ) ) ;
#35134 = CARTESIAN_POINT ( 'NONE',  ( -12.00019890019965096, -76.39977373798492977, -1.177339121803222359E-06 ) ) ;
#35135 = CARTESIAN_POINT ( 'NONE',  ( -0.5312504855272001114, -78.75070194988499850, -9.708839960653000034 ) ) ;
#35136 = CARTESIAN_POINT ( 'NONE',  ( -2.061649843245999758, -55.59438692379999480, -12.83797346712000120 ) ) ;
#35137 = CARTESIAN_POINT ( 'NONE',  ( 12.00000000000000888, -78.53958333333332575, -1.570796326794872577 ) ) ;
#35138 = CARTESIAN_POINT ( 'NONE',  ( 3.620209227049977052, -85.94828561723799965, -1.611820994701049781 ) ) ;
#35139 = EDGE_LOOP ( 'NONE', ( #28726, #7929, #34392, #58001, #7252, #40342 ) ) ;
#35140 = CIRCLE ( 'NONE', #18236, 1.750000000000001332 ) ;
#35141 = CARTESIAN_POINT ( 'NONE',  ( -9.372585790538636275, -78.28499999999999659, 1.790612804732440555 ) ) ;
#35142 = CARTESIAN_POINT ( 'NONE',  ( 1.310679582531385501, -79.19166666666669130, 0.7554284705563518720 ) ) ;
#35143 = CARTESIAN_POINT ( 'NONE',  ( 11.73875605999435123, -78.93695179073836243, -1.874534623384944254 ) ) ;
#35144 = CARTESIAN_POINT ( 'NONE',  ( -2.375990957848951091, -78.54828561723799396, -3.940594315429740480 ) ) ;
#35145 = CARTESIAN_POINT ( 'NONE',  ( -4.399243655502999673, -79.83797013842199419, 10.05537673064999815 ) ) ;
#35146 = CARTESIAN_POINT ( 'NONE',  ( 0.3664097479239993849, -17.02809982499870856, -12.50575740043519346 ) ) ;
#35147 = CARTESIAN_POINT ( 'NONE',  ( 8.159281975656000441, -77.05763688248899257, -8.859554478729998905 ) ) ;
#35148 = CARTESIAN_POINT ( 'NONE',  ( -0.2201363562291999698, -79.46327907014000402, -1.483758735329000045 ) ) ;
#35149 = CARTESIAN_POINT ( 'NONE',  ( 9.415891442473027340, -79.15074836997709440, 0.09954902595250748887 ) ) ;
#35150 = ORIENTED_EDGE ( 'NONE', *, *, #2676, .F. ) ;
#35151 = CARTESIAN_POINT ( 'NONE',  ( -7.286644543156999276, -79.20872152740099637, -8.282906837769999697 ) ) ;
#35152 = CARTESIAN_POINT ( 'NONE',  ( 1.050086718088998339, -79.89624094074886784, 0.6784569047000227338 ) ) ;
#35153 = DIRECTION ( 'NONE',  ( 0.000000000000000000, -1.000000000000000000, 0.000000000000000000 ) ) ;
#35154 = CARTESIAN_POINT ( 'NONE',  ( 10.38514225167999960, -78.02921528601798684, -3.771779243421000238 ) ) ;
#35155 = CARTESIAN_POINT ( 'NONE',  ( -10.57172952794455156, -76.48333333333334849, 2.251292830498277109 ) ) ;
#35156 = CARTESIAN_POINT ( 'NONE',  ( 1.569236785184999737E-14, 0.000000000000000000, 0.000000000000000000 ) ) ;
#35157 = VECTOR ( 'NONE', #33335, 1000.000000000000000 ) ;
#35158 = DIRECTION ( 'NONE',  ( -0.7071067811864980568, 0.7071067811865969777, 2.302416782339995233E-09 ) ) ;
#35159 = CARTESIAN_POINT ( 'NONE',  ( 5.022587898441999599, -78.48512198850698951, -11.20577484976000093 ) ) ;
#35160 = CARTESIAN_POINT ( 'NONE',  ( -1.407171709420465211, -79.38541666666665719, 10.74999999999999467 ) ) ;
#35161 = CARTESIAN_POINT ( 'NONE',  ( 0.000000000000000000, 0.000000000000000000, 0.000000000000000000 ) ) ;
#35162 = AXIS2_PLACEMENT_3D ( 'NONE', #28452, #19609, #45911 ) ;
#35163 = CARTESIAN_POINT ( 'NONE',  ( -12.77306367228999839, -25.05881314456000197, 1.040970605966999862 ) ) ;
#35164 = ORIENTED_EDGE ( 'NONE', *, *, #6182, .T. ) ;
#35165 = EDGE_LOOP ( 'NONE', ( #25601, #17426, #44278, #12750, #17511, #57546, #4269 ) ) ;
#35166 = CARTESIAN_POINT ( 'NONE',  ( 10.40070879200345466, -78.82965153313729445, -2.740125206622860965 ) ) ;
#35167 = B_SPLINE_CURVE_WITH_KNOTS ( 'NONE', 3,
 ( #33463, #55327, #29040, #46497, #20197, #55621, #55036, #42632, #6899, #24907, #51210, #10762, #50914, #28741, #19905, #42345, #37898, #24619, #15757, #51501, #11058, #47080, #1327, #32577, #42925, #56209, #19029, #33752, #14584, #50624, #28152, #46204, #5728, #23738, #41752, #32869, #19321, #10462, #28448, #6021, #24031, #48505, #25769, #2479, #30478, #20483, #29607, #8050, #43495, #56784, #12760, #52927, #39630, #7479, #20767, #26046, #44070, #11913, #3057, #16052, #38479, #48231, #12197, #39054, #12477, #57636, #30757, #53213, #7766, #56497, #25477, #30181, #38766, #34035, #3340, #17192, #21335, #25189, #3619, #34897, #52074, #52642, #21052, #21625, #35181, #39347, #57355, #48790, #16918, #43209, #11632, #26334, #43791, #8335, #47663, #7189, #2768, #16346, #34325, #52361, #29890, #47947, #57068, #16628, #34614, #53502, #18081, #44650, #45540, #40802, #687, #39915, #35473, #36076, #44350, #9221, #18669, #5085, #21906, #18373, #22202, #4205, #9806, #54676, #13637, #31633, #8629, #13044, #54097, #49379, #13338, #44946, #3903, #31335, #396, #8926, #49675, #27206, #45245, #54393, #4793, #57931, #22793, #26615, #40213, #17486, #36658, #36367, #23081, #14218, #13930, #31925, #58224, #17787, #32215, #49970, #35776, #9513, #50257, #53804, #41095, #31042, #49079, #27499, #26915, #4502, #22501, #40512, #14799, #46417, #15095, #15683, #15395, #32502, #33389, #55844, #10688, #46130, #33092, #33679, #55544, #45835, #24254, #51134, #971, #51426, #42269, #5654, #37824, #55252, #10982, #28372, #5370, #28962, #51717, #56134, #5947, #1541, #1256, #23951, #28668, #41968, #19533, #23663, #19831, #47004, #27789, #19244, #37237, #23378, #6238, #50840, #6531, #41675, #41388, #24543, #18954, #32793, #42557, #10387, #37526, #46718, #1835, #2124, #20124, #28080, #38113, #36947, #54960, #14511, #50547, #10100, #20408, #38402, #7401, #30399, #47871, #39270, #21554, #29821, #25404, #34827, #48158, #56423, #12409, #3272, #57281, #56993, #2980, #52571, #43420, #7689, #20978, #15973, #56713, #16270, #11267, #38982, #43141, #16555, #43719, #16845, #57563, #30107, #12122, #44001, #52855, #25974, #33965, #52284, #24832, #52002, #48435, #25690, #7977, #11556, #34249, #29534, #3551, #6822, #11840, #34538, #47591, #21264, #7117, #39559, #17125, #35108, #42848, #25117, #29247, #47295, #2407, #2700, #20694, #38693, #53429, #23016, #40737, #44573, #40441, #22724, #48722, #35703, #27434, #13862, #31558, #49007, #49304, #328, #18010, #53144, #18306, #12692, #21837, #36299 ),
 .UNSPECIFIED., .F., .F.,
 ( 4, 2, 2, 1, 1, 1, 1, 1, 2, 2, 2, 2, 2, 1, 1, 1, 2, 2, 2, 2, 2, 2, 2, 1, 1, 1, 1, 1, 2, 2, 2, 2, 1, 1, 2, 2, 2, 1, 1, 1, 1, 2, 2, 2, 2, 2, 1, 1, 1, 1, 2, 2, 2, 2, 2, 1, 1, 1, 1, 2, 2, 2, 2, 2, 2, 2, 2, 1, 1, 1, 1, 2, 2, 2, 2, 1, 1, 1, 1, 1, 2, 2, 2, 2, 2, 1, 1, 2, 2, 2, 2, 2, 1, 1, 2, 2, 2, 2, 1, 1, 1, 1, 2, 2, 2, 2, 2, 2, 2, 1, 1, 1, 1, 1, 2, 2, 1, 1, 1, 1, 1, 1, 2, 2, 2, 2, 2, 1, 1, 1, 1, 2, 2, 2, 2, 1, 1, 2, 2, 2, 2, 1, 1, 2, 2, 2, 2, 1, 1, 1, 1, 2, 2, 2, 2, 2, 2, 2, 1, 1, 1, 1, 2, 2, 2, 2, 1, 2, 2, 2, 2, 1, 1, 1, 1, 1, 2, 2, 2, 2, 2, 1, 1, 1, 1, 2, 2, 2, 2, 2, 1, 1, 1, 1, 1, 2, 2, 2, 2, 2, 4 ),
 ( 0.000000000000000000, 0.01562500000005664219, 0.02343750000008496329, 0.02734375000009912904, 0.02929687500010621365, 0.03027343750010977330, 0.03076171875011152884, 0.03100585937511241008, 0.03112792968761284029, 0.03125000000011327050, 0.04687500000016913554, 0.05468750000019706459, 0.05859375000021103258, 0.06054687500021796454, 0.06152343750022142704, 0.06201171875022322422, 0.06225585937522412627, 0.06250000000022502833, 0.07812500000022287727, 0.09375000000022072622, 0.1093750000002185613, 0.1171875000002174511, 0.1210937500002169098, 0.1230468750002166461, 0.1240234375002165074, 0.1245117187502164519, 0.1247558593752164380, 0.1248779296877164380, 0.1249389648439664241, 0.1250000000002164102, 0.1328125000002231826, 0.1367187500002266520, 0.1386718750002283451, 0.1396484375002291778, 0.1401367187502295941, 0.1406250000002300105, 0.1484375000002361999, 0.1523437500002392531, 0.1542968750002407519, 0.1552734375002415568, 0.1557617187502419454, 0.1560058593752421396, 0.1562500000002423062, 0.1718750000002544354, 0.1796875000002605416, 0.1835937500002635669, 0.1855468750002650935, 0.1865234375002658429, 0.1870117187502662315, 0.1872558593752664258, 0.1873779296877665090, 0.1875000000002665923, 0.2031250000002769174, 0.2109375000002820522, 0.2148437500002845779, 0.2167968750002858824, 0.2177734375002865208, 0.2182617187502868539, 0.2185058593752870482, 0.2186279296877871314, 0.2187500000002871869, 0.2343750000002968459, 0.2421875000003016754, 0.2460937500003040623, 0.2500000000003064216, 0.2656250000003159140, 0.2734375000003206879, 0.2773437500003230749, 0.2792968750003242406, 0.2802734375003248513, 0.2807617187503251843, 0.2810058593753253509, 0.2812500000003255174, 0.2968750000003349543, 0.3046875000003396727, 0.3085937500003420042, 0.3105468750003432254, 0.3115234375003438361, 0.3120117187503441136, 0.3122558593753442802, 0.3123779296878443357, 0.3125000000003443357, 0.3281250000003541056, 0.3359375000003589351, 0.3398437500003613221, 0.3417968750003624878, 0.3427734375003629874, 0.3432617187503632650, 0.3437500000003635425, 0.3515625000003680389, 0.3554687500003703149, 0.3574218750003714251, 0.3583984375003719802, 0.3588867187503722578, 0.3591308593753724243, 0.3593750000003725908, 0.3671875000003768097, 0.3710937500003789191, 0.3730468750003799183, 0.3740234375003804179, 0.3745117187503806400, 0.3747558593753807510, 0.3748779296878808065, 0.3750000000003808620, 0.4062500000003944067, 0.4375000000004078959, 0.4687500000004214407, 0.4843750000004282685, 0.4921875000004316547, 0.4960937500004333200, 0.4980468750004342082, 0.4990234375004343748, 0.4995117187504344303, 0.4997558593754346523, 0.4998779296879345968, 0.5000000000004345413, 0.5156250000004241052, 0.5234375000004188871, 0.5273437500004162226, 0.5292968750004148903, 0.5302734375004141132, 0.5307617187504137801, 0.5310058593754136691, 0.5312500000004135581, 0.5468750000004045653, 0.5546875000004000134, 0.5585937500003976819, 0.5605468750003965717, 0.5615234375003960166, 0.5620117187503956835, 0.5622558593753955725, 0.5623779296878954614, 0.5625000000003953504, 0.5781250000003820277, 0.5859375000003753664, 0.5898437500003721468, 0.5917968750003703704, 0.5927734375003694822, 0.5937500000003685940, 0.6015625000003618217, 0.6054687500003584910, 0.6074218750003568257, 0.6083984375003558265, 0.6088867187503553824, 0.6093750000003549383, 0.6171875000003481659, 0.6210937500003448353, 0.6230468750003431699, 0.6240234375003422818, 0.6245117187503418377, 0.6247558593753416156, 0.6248779296878415046, 0.6250000000003412826, 0.6562500000003149703, 0.6875000000002885470, 0.7187500000002622347, 0.7343750000002490230, 0.7421875000002423617, 0.7460937500002389200, 0.7480468750002372547, 0.7490234375002363665, 0.7495117187502359224, 0.7497558593752357003, 0.7500000000002354783, 0.7656250000002193801, 0.7734375000002113865, 0.7773437500002073897, 0.7792968750002053913, 0.7812500000002032818, 0.7968750000001869616, 0.8046875000001787459, 0.8085937500001746381, 0.8105468750001726397, 0.8115234375001716405, 0.8120117187501710854, 0.8122558593751708633, 0.8123779296876707523, 0.8125000000001706413, 0.8281250000001512124, 0.8359375000001415534, 0.8398437500001367795, 0.8417968750001343370, 0.8427734375001331157, 0.8432617187501324496, 0.8435058593751321165, 0.8436279296876320055, 0.8437500000001318945, 0.8593750000001109113, 0.8671875000001003642, 0.8710937500000951461, 0.8730468750000924816, 0.8740234375000911493, 0.8745117187500904832, 0.8747558593750902611, 0.8748779296875901501, 0.8749389648438401501, 0.8750000000000900391, 0.9062500000000676126, 0.9375000000000450751, 0.9687500000000226485, 1.000000000000000000 ),
 .UNSPECIFIED. ) ;
#35168 = VERTEX_POINT ( 'NONE', #50660 ) ;
#35169 = CARTESIAN_POINT ( 'NONE',  ( 8.597946777922295780, -79.53556089611873858, 4.122091896699570768 ) ) ;
#35170 = ORIENTED_EDGE ( 'NONE', *, *, #8069, .T. ) ;
#35171 = CARTESIAN_POINT ( 'NONE',  ( -10.75986520424384274, -81.00000000000001421, -0.7996052922503522620 ) ) ;
#35172 = CONICAL_SURFACE ( 'NONE', #44642, 0.6999999997695030007, 0.7853981633972997312 ) ;
#35173 = ADVANCED_FACE ( 'NONE', ( #1947 ), #42951, .T. ) ;
#35174 = AXIS2_PLACEMENT_3D ( 'NONE', #12374, #17090, #53391 ) ;
#35175 = CARTESIAN_POINT ( 'NONE',  ( 1.892857502466999797, -78.48868998579800405, 9.500437764121999251 ) ) ;
#35176 = EDGE_CURVE ( 'NONE', #7317, #35168, #50490, .T. ) ;
#35177 = CARTESIAN_POINT ( 'NONE',  ( -6.528096133866698736, -78.16282450551233296, -6.553206690438871718 ) ) ;
#35178 = CARTESIAN_POINT ( 'NONE',  ( -10.71602610194999805, -79.74223592799599203, 3.314346869870000489 ) ) ;
#35179 = EDGE_LOOP ( 'NONE', ( #6305, #39627, #7834, #36495, #55533, #15425, #46758 ) ) ;
#35180 = ORIENTED_EDGE ( 'NONE', *, *, #51772, .F. ) ;
#35181 = CARTESIAN_POINT ( 'NONE',  ( -4.564206451014241495, -77.51613632694960643, 8.045838294816407554 ) ) ;
#35182 = DIRECTION ( 'NONE',  ( 0.000000000000000000, 0.000000000000000000, -1.000000000000000000 ) ) ;
#35183 = CARTESIAN_POINT ( 'NONE',  ( -0.1963495408493673433, -77.88541666666668561, 1.499999999999999334 ) ) ;
#35184 = CARTESIAN_POINT ( 'NONE',  ( 8.444976262095000408, -78.18144482767498005, 4.780490068936999570 ) ) ;
#35185 = CARTESIAN_POINT ( 'NONE',  ( -10.23621640724999793, -76.45181667362000155, 8.212304960288999922 ) ) ;
#35186 = CARTESIAN_POINT ( 'NONE',  ( -5.510565319487811031, -79.47559583644631687, -7.739628810976011408 ) ) ;
#35187 = CARTESIAN_POINT ( 'NONE',  ( 8.114915067887620737, -53.97115967817116200, -9.847905526091571105 ) ) ;
#35188 = CARTESIAN_POINT ( 'NONE',  ( -8.254612054926999676, -79.93512533242399343, 6.886499823760000361 ) ) ;
#35189 = EDGE_CURVE ( 'NONE', #33163, #33164, #45943, .T. ) ;
#35190 = CARTESIAN_POINT ( 'NONE',  ( 12.78037507862999966, -17.70670131430000183, -1.812742845510000089 ) ) ;
#35191 = CARTESIAN_POINT ( 'NONE',  ( -9.783241737786999792, -24.53564621530999901, -7.961026681561000018 ) ) ;
#35192 = CARTESIAN_POINT ( 'NONE',  ( -9.250000000000000000, -78.49999999999998579, 0.000000000000000000 ) ) ;
#35193 = VERTEX_POINT ( 'NONE', #50948 ) ;
#35194 = CARTESIAN_POINT ( 'NONE',  ( 2.784107197330000005, -79.65218441210198819, -11.87846276067000062 ) ) ;
#35195 = CARTESIAN_POINT ( 'NONE',  ( 0.000000000000000000, -76.79999999999999716, 0.000000000000000000 ) ) ;
#35196 = CARTESIAN_POINT ( 'NONE',  ( 5.537129384246000541, -79.03844710739599577, 10.62336504503000079 ) ) ;
#35197 = CARTESIAN_POINT ( 'NONE',  ( -9.422860735135998311, -16.74048607655000254, -8.643926020477998406 ) ) ;
#35199 = DIRECTION ( 'NONE',  ( 0.000000000000000000, 1.000000000000000000, 0.000000000000000000 ) ) ;
#35198 = CARTESIAN_POINT ( 'NONE',  ( 7.691893942725999800, -58.55453807205000061, 10.42272502862000039 ) ) ;
#35200 = DIRECTION ( 'NONE',  ( 0.7071067811865474617, 0.000000000000000000, -0.7071067811865474617 ) ) ;
#35201 = CARTESIAN_POINT ( 'NONE',  ( 10.07722254368999870, -57.05199022587000002, -7.718368845804999268 ) ) ;
#35202 = CARTESIAN_POINT ( 'NONE',  ( -1.243547092045951041, -78.41458333333332575, -9.500000000000000000 ) ) ;
#35203 = CARTESIAN_POINT ( 'NONE',  ( -0.9550654082404999023, -78.20516599075500608, 11.22148896650999816 ) ) ;
#35204 = CARTESIAN_POINT ( 'NONE',  ( 1.250000000000000000, -83.24999999999998579, 0.000000000000000000 ) ) ;
#35205 = CARTESIAN_POINT ( 'NONE',  ( -10.85082013035999893, -80.80199725428047941, 2.992226394595999928 ) ) ;
#35206 = VERTEX_POINT ( 'NONE', #19941 ) ;
#35207 = CARTESIAN_POINT ( 'NONE',  ( 4.000000000000000000, -74.80000000000001137, 0.5999999999999999778 ) ) ;
#35208 = AXIS2_PLACEMENT_3D ( 'NONE', #57896, #26885, #17453 ) ;
#35209 = EDGE_CURVE ( 'NONE', #6714, #48625, #24979, .T. ) ;
#35210 = CARTESIAN_POINT ( 'NONE',  ( 2.062323307449999810, -55.57286846775000555, 12.83634826441000065 ) ) ;
#35211 = CARTESIAN_POINT ( 'NONE',  ( -12.87024489156999962, -22.78461666469000235, 2.062597265787999845 ) ) ;
#35212 = CARTESIAN_POINT ( 'NONE',  ( 0.7054349844981000484, -2.771954967774000522, -3.576897754931000151 ) ) ;
#35213 = CARTESIAN_POINT ( 'NONE',  ( 8.183515395032999962, -79.31211703774899036, 4.675091623977000843 ) ) ;
#35214 = CARTESIAN_POINT ( 'NONE',  ( 2.486604901413172364, -77.44583333333332575, -9.252740428348998236 ) ) ;
#35215 = CARTESIAN_POINT ( 'NONE',  ( -0.001775305735512080086, -77.22499999999998010, -11.03387446371952940 ) ) ;
#35216 = CLOSED_SHELL ( 'NONE', ( #39444, #5306, #34799, #9788, #45973, #44762, #51066, #1016, #57746, #31934, #35674, #20356, #32476, #26147, #37896, #29070, #57109, #34235, #34011, #35669, #57866, #51435, #35279, #8052, #3316, #37159, #20923, #17983, #49839, #6435, #47898, #52208, #45048, #16202, #33826, #2342, #49581, #1651, #14943, #47789, #16587, #29304, #32347, #15289, #38475, #20748, #1791, #42642, #22976, #52482, #37564, #34624, #34694, #39216, #39646, #50757, #44829, #13761, #51985, #35040, #40090, #27501, #10228, #19593 ) ) ;
#35217 = CARTESIAN_POINT ( 'NONE',  ( -0.005928781627359999175, -62.00113050230000056, 12.66336824422999996 ) ) ;
#35218 = CARTESIAN_POINT ( 'NONE',  ( -2.839805762151337731, -3.041666666666666963, -1.636761686205423949 ) ) ;
#35219 = CARTESIAN_POINT ( 'NONE',  ( 0.3143049556117999965, -82.79444503318798354, 4.160684000108000546 ) ) ;
#35220 = CARTESIAN_POINT ( 'NONE',  ( 0.000000000000000000, -82.09999999999999432, 0.000000000000000000 ) ) ;
#35221 = CARTESIAN_POINT ( 'NONE',  ( 6.490606146300518908, -77.12338061544191703, -10.12186978042076646 ) ) ;
#35222 = CARTESIAN_POINT ( 'NONE',  ( 4.029831046159999985, -78.43071061401199984, -10.51637221458999960 ) ) ;
#35223 = DIRECTION ( 'NONE',  ( 0.7071067811865474617, 0.000000000000000000, 0.7071067811865474617 ) ) ;
#35224 = CARTESIAN_POINT ( 'NONE',  ( 0.1696949479679999984, -78.19689351345999739, 1.654914741598999983 ) ) ;
#35225 = CARTESIAN_POINT ( 'NONE',  ( 9.208615812369000508, -77.04458045456699722, 2.957800710608999850 ) ) ;
#35226 = CARTESIAN_POINT ( 'NONE',  ( -1.441818230322603700, -82.77428155285538480, -0.4538374300033769515 ) ) ;
#35227 = LINE ( 'NONE', #53258, #42161 ) ;
#35228 = CARTESIAN_POINT ( 'NONE',  ( -3.860146505116679005, -80.19620181100606260, -10.03328294032903578 ) ) ;
#35229 = ADVANCED_FACE ( 'NONE', ( #55657 ), #57051, .T. ) ;
#35230 = CARTESIAN_POINT ( 'NONE',  ( 6.606377239730347739, -77.17708333333330017, -8.596418555780422466 ) ) ;
#35231 = CARTESIAN_POINT ( 'NONE',  ( -10.04568514502024357, -17.44913840261576610, -7.921286339709529223 ) ) ;
#35232 = ORIENTED_EDGE ( 'NONE', *, *, #31153, .T. ) ;
#35233 = CARTESIAN_POINT ( 'NONE',  ( 8.179400488428159477, -54.05908162287557417, 9.502921777737899589 ) ) ;
#35234 = CARTESIAN_POINT ( 'NONE',  ( -1.092316917947570243, -78.14177812212517438, -0.6297690996598702684 ) ) ;
#35235 = CARTESIAN_POINT ( 'NONE',  ( -6.231249681807000229, -79.74506692201100577, 9.381124237602000093 ) ) ;
#35236 = CIRCLE ( 'NONE', #39139, 3.600000000000000089 ) ;
#35237 = CARTESIAN_POINT ( 'NONE',  ( 2.813637286836895068, -77.45420692980438560, 10.46962234225027366 ) ) ;
#35238 = ORIENTED_EDGE ( 'NONE', *, *, #1200, .F. ) ;
#35239 = CARTESIAN_POINT ( 'NONE',  ( -1.113896998616000111, -81.55636123001200133, -1.168951411329999912 ) ) ;
#35240 = B_SPLINE_CURVE_WITH_KNOTS ( 'NONE', 3,
 ( #55098, #37374, #10526, #9359, #32064, #50105, #9649, #45679, #5219, #23224, #41228, #18801, #6961, #11120, #33525, #51272, #20545, #46849, #19971, #11404, #33810, #10826, #15822, #1976, #2827, #56556, #16405, #55687, #28802, #51848, #1679, #24965, #47141, #56271, #6378, #20825, #37957, #24681, #25255, #38540, #24392, #29383, #42406, #55981, #47431, #6673, #29097, #2257, #19669, #42693, #16116, #20257, #42984, #33226, #2542, #29956, #34095, #51562, #29669, #48007, #52135, #37668, #34389, #11693, #38830, #11978, #47718, #56847, #7542, #7251, #52420, #43273, #38248, #25541, #15233, #15531, #40287, #58000, #3687, #30250, #8403, #39697, #31108, #52995, #31411, #44139, #21404, #12258, #49149, #26118, #39416, #53878, #35548, #22271, #48576, #3406, #13114, #8700, #12544, #17859, #25830, #26690, #52706, #3124, #44722, #43858, #58298, #13411, #35848, #30827, #21115, #8118, #12827, #57420, #17260, #49454, #16696, #48861, #7830, #4275, #17556, #26400, #35250, #21689, #9000, #43559, #21975, #30543, #44422, #39122, #57129, #48291, #34677, #16982, #34964, #57705, #53281, #3973, #39986, #53577, #50832, #28362, #4573, #49749, #9292, #40585, #26985, #1531, #1246, #46409, #10678, #19525, #5937, #33380, #24534, #6228, #24244, #42546, #42260, #28071, #182, #10377, #55834, #23654, #22573, #2114, #13707, #20113, #38104, #51416, #14790, #56124, #18156, #46994, #54167, #36150, #41959, #46119, #28952 ),
 .UNSPECIFIED., .F., .F.,
 ( 4, 2, 2, 2, 2, 2, 1, 2, 2, 1, 1, 2, 2, 2, 2, 2, 2, 2, 1, 1, 2, 2, 2, 1, 1, 2, 2, 1, 2, 2, 2, 1, 2, 2, 1, 1, 2, 1, 2, 2, 2, 1, 2, 2, 2, 2, 2, 1, 1, 1, 2, 2, 2, 2, 2, 2, 2, 1, 2, 2, 2, 2, 2, 2, 1, 2, 2, 2, 1, 2, 2, 1, 2, 2, 2, 2, 2, 2, 2, 2, 1, 2, 2, 2, 2, 2, 2, 2, 2, 2, 1, 1, 1, 2, 2, 2, 1, 1, 2, 2, 1, 2, 4 ),
 ( 0.000000000000000000, 0.02254148184236093658, 0.03381222276354139966, 0.03944759322413162600, 0.04508296368472185234, 0.06762444552708282708, 0.07044213075737798535, 0.07114655206495175410, 0.07149876271873865929, 0.07185097337252556449, 0.07325981598767324077, 0.07889518644826387650, 0.09016592736944517572, 0.1127074092118077603, 0.1352488910541703448, 0.1408842615147609667, 0.1422931041299086152, 0.1429975254374824534, 0.1437019467450562915, 0.1465196319753516718, 0.1577903728965331376, 0.1803318547388961246, 0.1916025956600775904, 0.1944202808903729707, 0.1958291235055207025, 0.1961813341593076354, 0.1965335448130945684, 0.1972379661206684898, 0.2028733365812608325, 0.2254148184236299257, 0.2479563002659990467, 0.2493651428811471116, 0.2497173535349341555, 0.2500695641887212273, 0.2507739854962953152, 0.2535916707265916670, 0.2592270411871845370, 0.2704977821083701661, 0.2817685230295557952, 0.2845862082598522025, 0.2859950508750004339, 0.2874038934901486653, 0.2930392639507415908, 0.3155807457931132376, 0.3212161162537061077, 0.3213922215805997129, 0.3215683269074932626, 0.3219205375612803621, 0.3226249588688546166, 0.3240338014840031811, 0.3268514867143001990, 0.3381222276354884371, 0.3606637094778649688, 0.3832051913202414450, 0.3888405617808354808, 0.3916582470111326097, 0.3930670896262811187, 0.3944759322414296276, 0.4057466731626182543, 0.4282881550049952857, 0.4395588959261836903, 0.4451942663867780037, 0.4458986876943522581, 0.4466031090019265126, 0.4480119516170751881, 0.4508296368473724836, 0.4733711186897506251, 0.4959126005321287667, 0.4987302857624259511, 0.4994347070700003166, 0.5001391283775746821, 0.5015479709927231911, 0.5071833414533171158, 0.5184540823745051874, 0.5297248232956932590, 0.5353601937562872948, 0.5381778789865843127, 0.5409955642168814416, 0.5635370460592578068, 0.5691724165198518426, 0.5705812591350003515, 0.5712856804425746615, 0.5719901017501488605, 0.5748077869804457674, 0.5860785279016335059, 0.6086200097440088719, 0.6311614915863842379, 0.6424322325075718654, 0.6427844431613589649, 0.6431366538151460643, 0.6438410751227201523, 0.6452499177378684392, 0.6480676029681649020, 0.6537029734287579386, 0.6762444552711299739, 0.6875151961923159361, 0.6931505666529089726, 0.6959682518832054354, 0.6963204625369925349, 0.6966726731907795234, 0.6973770944983537223, 0.6987859371135020092, 0.7213274189558753768 ),
 .UNSPECIFIED. ) ;
#35241 = ORIENTED_EDGE ( 'NONE', *, *, #45471, .T. ) ;
#35242 = DIRECTION ( 'NONE',  ( 0.000000000000000000, -1.000000000000000000, 0.000000000000000000 ) ) ;
#35243 = VECTOR ( 'NONE', #9878, 1000.000000000000000 ) ;
#35244 = ORIENTED_EDGE ( 'NONE', *, *, #31016, .F. ) ;
#35245 = DIRECTION ( 'NONE',  ( 0.000000000000000000, -1.000000000000000000, 0.000000000000000000 ) ) ;
#35246 = CARTESIAN_POINT ( 'NONE',  ( -9.254388464354001087, -79.90752053325199711, 5.469807505829999528 ) ) ;
#35247 = CARTESIAN_POINT ( 'NONE',  ( 9.200987374210999548, -78.86863103297000066, 5.875133813785999415 ) ) ;
#35248 = CARTESIAN_POINT ( 'NONE',  ( 0.8537148449481999357, -24.70498145908999987, -12.43377424872999981 ) ) ;
#35249 = CARTESIAN_POINT ( 'NONE',  ( 2.498996544723999680, -81.45596103735698534, 2.804707967251000245 ) ) ;
#35250 = CARTESIAN_POINT ( 'NONE',  ( -5.602526181104785508, -79.32510020630215308, 7.672075667186650350 ) ) ;
#35251 = ORIENTED_EDGE ( 'NONE', *, *, #35515, .F. ) ;
#35252 = CARTESIAN_POINT ( 'NONE',  ( -10.84202097104999929, -77.33490313763715562, 2.082001701158999740 ) ) ;
#35253 = CARTESIAN_POINT ( 'NONE',  ( 11.90545625444000066, -78.77723422687999744, 3.315402164377000194 ) ) ;
#35254 = VERTEX_POINT ( 'NONE', #23771 ) ;
#35255 = ORIENTED_EDGE ( 'NONE', *, *, #44519, .T. ) ;
#35256 = CARTESIAN_POINT ( 'NONE',  ( 12.85140862679999962, -57.04439829966000275, -1.980464483675000054 ) ) ;
#35257 = CARTESIAN_POINT ( 'NONE',  ( -1.624989163556999772E-14, -74.69999999881999031, 0.000000000000000000 ) ) ;
#35258 = DIRECTION ( 'NONE',  ( -1.000000000000000000, 0.000000000000000000, 0.000000000000000000 ) ) ;
#35259 = CARTESIAN_POINT ( 'NONE',  ( -1.120379678216000041, -79.31128506247100063, -0.7232983489183999470 ) ) ;
#35260 = FACE_BOUND ( 'NONE', #49335, .T. ) ;
#35261 = CARTESIAN_POINT ( 'NONE',  ( 0.4816222532846568538, -86.25171438276197478, -4.576205428947634601 ) ) ;
#35262 = CARTESIAN_POINT ( 'NONE',  ( 3.471857344089170017, -85.80962377308421196, 1.038510158527778726 ) ) ;
#35263 = CARTESIAN_POINT ( 'NONE',  ( -13.06702859930000038, -77.01232752474999188, -1.103813699724999875 ) ) ;
#35264 = EDGE_CURVE ( 'NONE', #55898, #1255, #55363, .T. ) ;
#35265 = CARTESIAN_POINT ( 'NONE',  ( -0.4297501350614000293, -80.48078034499999944, 1.281126864269000132 ) ) ;
#35266 = CARTESIAN_POINT ( 'NONE',  ( 9.958655842330001562, -76.24375625893898700, 4.669801055666999545 ) ) ;
#35267 = CYLINDRICAL_SURFACE ( 'NONE', #41636, 0.5000000000000004441 ) ;
#35268 = CARTESIAN_POINT ( 'NONE',  ( 3.799029956959000032, -82.54207433891198775, -1.620318395421999957 ) ) ;
#35269 = DIRECTION ( 'NONE',  ( 0.7071067811865474617, 0.000000000000000000, 0.7071067811865474617 ) ) ;
#35270 = CARTESIAN_POINT ( 'NONE',  ( -1.305255771447972224, -3.009187556855974943, 2.975616621677583673 ) ) ;
#35271 = CARTESIAN_POINT ( 'NONE',  ( -3.480664168985999840, -78.75880496681158149, -0.6827920017205999503 ) ) ;
#35272 = CARTESIAN_POINT ( 'NONE',  ( -0.3664097479317053319, -24.97190017499968206, -12.50575740043507800 ) ) ;
#35273 = CARTESIAN_POINT ( 'NONE',  ( 10.07210119001000059, -80.62085295350529179, 5.045985883512999592 ) ) ;
#35274 = CARTESIAN_POINT ( 'NONE',  ( -3.750250575282000121, -2.269022469510000306, 0.6493866540274000343 ) ) ;
#35275 = CARTESIAN_POINT ( 'NONE',  ( 0.7969900020161251319, -79.92870045822861869, -0.9955794363004618619 ) ) ;
#35276 = EDGE_LOOP ( 'NONE', ( #54859, #22335, #28588, #3691 ) ) ;
#35277 = FACE_OUTER_BOUND ( 'NONE', #20957, .T. ) ;
#35278 = B_SPLINE_CURVE_WITH_KNOTS ( 'NONE', 3,
 ( #32123, #53191, #13541, #18861, #45149, #4701, #304, #49875, #54588, #9419 ),
 .UNSPECIFIED., .F., .F.,
 ( 4, 2, 2, 2, 4 ),
 ( 0.000000000000000000, 0.1249999999999971689, 0.2499999999999943379, 0.4999999999999988898, 1.000000000000000000 ),
 .UNSPECIFIED. ) ;
#35279 = ADVANCED_FACE ( 'NONE', ( #24655 ), #9916, .F. ) ;
#35280 = DIRECTION ( 'NONE',  ( 0.000000000000000000, 1.000000000000000000, 0.000000000000000000 ) ) ;
#35281 = VECTOR ( 'NONE', #34240, 1000.000000000000000 ) ;
#35282 = CARTESIAN_POINT ( 'NONE',  ( 0.6791306551168999617, -81.38940478334400552, -1.147762040996999966 ) ) ;
#35283 = CARTESIAN_POINT ( 'NONE',  ( 4.044903269867999640, -79.05999999999998806, -8.595856998426999240 ) ) ;
#35284 = CARTESIAN_POINT ( 'NONE',  ( 12.53073434187000146, -77.78026658266999505, -3.509976885708000260 ) ) ;
#35285 = CARTESIAN_POINT ( 'NONE',  ( -7.921335223431004380, -61.35094696582485341, -10.04563431751754621 ) ) ;
#35286 = CARTESIAN_POINT ( 'NONE',  ( 12.37198840876000006, -76.25631020154999362, 1.869025070383000031 ) ) ;
#35287 = ORIENTED_EDGE ( 'NONE', *, *, #8047, .F. ) ;
#35288 = DIRECTION ( 'NONE',  ( 1.000000000000000000, 0.000000000000000000, 0.000000000000000000 ) ) ;
#35289 = CARTESIAN_POINT ( 'NONE',  ( 7.685661446562000343, -76.94999999999998863, -5.583959896778000420 ) ) ;
#35290 = CARTESIAN_POINT ( 'NONE',  ( 1.309590324566999975, -81.98873225866600478, -0.05285834632500000657 ) ) ;
#35291 = CARTESIAN_POINT ( 'NONE',  ( 7.641012305223999768, -18.71082276572999703, -10.18589226631999978 ) ) ;
#35292 = CARTESIAN_POINT ( 'NONE',  ( -9.612747958823000261, -77.38818535316599423, 0.5898851805584999219 ) ) ;
#35293 = CARTESIAN_POINT ( 'NONE',  ( 3.632564424962000160, -85.59158141794600283, 2.052078968907000256 ) ) ;
#35294 = CARTESIAN_POINT ( 'NONE',  ( -3.135571036917709886, -79.99881628433968217, 10.28260097463162914 ) ) ;
#35295 = CARTESIAN_POINT ( 'NONE',  ( -1.487176594838000021, -80.53170427028999256, 0.2955346688291999868 ) ) ;
#35296 = EDGE_CURVE ( 'NONE', #2377, #48625, #21217, .T. ) ;
#35297 = ORIENTED_EDGE ( 'NONE', *, *, #42905, .F. ) ;
#35298 = CARTESIAN_POINT ( 'NONE',  ( -2.904718832244216564, -77.20339151522927068, -10.35162020224675139 ) ) ;
#35299 = CARTESIAN_POINT ( 'NONE',  ( 1.399739583348414529, -82.10026041666372976, 0.1840776944558860095 ) ) ;
#35300 = CARTESIAN_POINT ( 'NONE',  ( -3.699999999670000150, -79.00321104920828930, -1.552506213169860872E-14 ) ) ;
#35301 = ORIENTED_EDGE ( 'NONE', *, *, #2197, .T. ) ;
#35302 = VERTEX_POINT ( 'NONE', #10795 ) ;
#35303 = CARTESIAN_POINT ( 'NONE',  ( 7.195688986358000250, -79.18869284577598933, 8.240744890341000328 ) ) ;
#35304 = DIRECTION ( 'NONE',  ( 1.000000000000000000, 0.000000000000000000, 0.000000000000000000 ) ) ;
#35305 = CARTESIAN_POINT ( 'NONE',  ( -1.882622766709999951, -79.91865347566299249, -11.17249270816999918 ) ) ;
#35306 = ORIENTED_EDGE ( 'NONE', *, *, #5626, .T. ) ;
#35307 = CARTESIAN_POINT ( 'NONE',  ( 4.527593368978999777, -77.60351546138099366, 11.29085598690000047 ) ) ;
#35308 = VERTEX_POINT ( 'NONE', #1652 ) ;
#35309 = B_SPLINE_SURFACE_WITH_KNOTS ( 'NONE', 3, 3, ( 
 ( #38282, #29987, #6411, #48041, #20576, #47470, #6994, #24998, #24124, #51880, #43018, #33262, #1711, #37702, #55722, #42440, #15268, #51303, #10861, #2007, #15564, #11153, #47174, #6705, #24716, #56302, #15857, #33843, #48894, #31138, #57451, #48321, #43889, #43592, #40319 ),
 ( #7861, #22304, #58328, #25860, #44752, #7572, #4303, #53607, #49178, #21436, #12855, #3155, #48605, #17892, #26724, #25572, #44451, #3435, #16725, #17010, #53909, #8152, #39445, #26151, #35881, #13442, #8731, #31442, #58031, #21144, #12576, #34993, #35578, #13146, #53024 ),
 ( #39152, #12289, #34707, #57159, #52738, #30573, #30279, #44171, #3719, #22008, #21721, #39726, #57734, #17293, #35282, #53312, #30856, #8435, #26430, #4003, #40015, #17591, #28696, #37558, #9032, #11010, #19860, #9615, #55575, #38142, #37855, #54199, #55876, #15426, #33122 ),
 ( #2154, #27603, #33419, #23981, #51457, #28994, #47035, #6565, #40908, #24282, #13736, #31734, #15124, #24573, #49779, #42590, #20155, #54494, #51165, #56166, #19560, #36467, #15714, #10719, #49482, #27019, #45055, #46747, #6267, #4607, #42300, #45347, #1865, #18188, #45645 ) ),
 .UNSPECIFIED., .F., .F., .F.,
 ( 4, 4 ),
 ( 4, 1, 1, 1, 1, 1, 1, 1, 1, 1, 1, 1, 1, 1, 1, 1, 1, 1, 1, 1, 1, 1, 1, 1, 1, 1, 1, 1, 1, 1, 1, 1, 4 ),
 ( -0.1566102636784000024, 1.156610263678000017 ),
 ( -0.02000000000000000042, 0.01250000000000000069, 0.04499999999999999833, 0.07749999999999999944, 0.1100000000000000006, 0.1424999999999999878, 0.1749999999999999889, 0.2074999999999999900, 0.2399999999999999911, 0.2725000000000000200, 0.3049999999999999933, 0.3375000000000000222, 0.3699999999999999956, 0.4025000000000000244, 0.4349999999999999978, 0.4675000000000000266, 0.5000000000000000000, 0.5324999999999999734, 0.5649999999999999467, 0.5975000000000000311, 0.6300000000000000044, 0.6624999999999999778, 0.6949999999999999512, 0.7275000000000000355, 0.7600000000000000089, 0.7924999999999999822, 0.8249999999999999556, 0.8575000000000000400, 0.8900000000000000133, 0.9224999999999999867, 0.9549999999999999600, 0.9875000000000000444, 1.020000000000000018 ),
 .UNSPECIFIED. ) ;
#35310 = EDGE_LOOP ( 'NONE', ( #42769, #45233, #24464, #9067, #5207, #45661 ) ) ;
#35311 = CARTESIAN_POINT ( 'NONE',  ( -1.539687499886083888, -78.08365330915714253, 11.67491192796933319 ) ) ;
#35312 = CARTESIAN_POINT ( 'NONE',  ( 6.728605944993000243, -79.93548824452055612, -7.080011783993000130 ) ) ;
#35313 = AXIS2_PLACEMENT_3D ( 'NONE', #34337, #30771, #31057 ) ;
#35314 = ORIENTED_EDGE ( 'NONE', *, *, #1809, .F. ) ;
#35315 = CARTESIAN_POINT ( 'NONE',  ( 0.1943040786466343206, -82.02213541144035958, -1.477864610832026804 ) ) ;
#35316 = B_SPLINE_CURVE_WITH_KNOTS ( 'NONE', 3,
 ( #32579, #50626, #46499, #14586, #41754, #42347, #42046, #760, #1616, #24033, #37314, #1046, #32871, #19608, #37607, #1329, #5731, #28154 ),
 .UNSPECIFIED., .F., .F.,
 ( 4, 2, 2, 2, 2, 2, 2, 2, 4 ),
 ( 0.000000000000000000, 0.1250000000000000833, 0.2500000000000001665, 0.3750000000000001665, 0.5000000000000002220, 0.6250000000000002220, 0.7500000000000001110, 0.8750000000000001110, 1.000000000000000000 ),
 .UNSPECIFIED. ) ;
#35317 = ORIENTED_EDGE ( 'NONE', *, *, #481, .F. ) ;
#35318 = CARTESIAN_POINT ( 'NONE',  ( 0.4456039955205827185, -80.49636525167119316, 1.193634369761791492 ) ) ;
#35319 = AXIS2_PLACEMENT_3D ( 'NONE', #7257, #2831, #38835 ) ;
#35320 = CARTESIAN_POINT ( 'NONE',  ( -0.03239454126609288276, -78.85171435493609238, -3.437034970110011134 ) ) ;
#35321 = CARTESIAN_POINT ( 'NONE',  ( 9.317995624384998621, -53.66762134137999851, 8.588852713974999276 ) ) ;
#35322 = FACE_OUTER_BOUND ( 'NONE', #16176, .T. ) ;
#35323 = CARTESIAN_POINT ( 'NONE',  ( 0.000000000000000000, -65.72928575305999743, 0.000000000000000000 ) ) ;
#35324 = ADVANCED_FACE ( 'NONE', ( #6055 ), #23480, .F. ) ;
#35325 = CIRCLE ( 'NONE', #22161, 1.749999999999998668 ) ;
#35326 = DIRECTION ( 'NONE',  ( 0.000000000000000000, 1.000000000000000000, 0.000000000000000000 ) ) ;
#35327 = CARTESIAN_POINT ( 'NONE',  ( 6.035966914210000311, -77.98297998349713112, 10.34809972146999968 ) ) ;
#35328 = CARTESIAN_POINT ( 'NONE',  ( 9.195972239629917055, -78.84146734569272041, -1.008436867448839758 ) ) ;
#35329 = ADVANCED_FACE ( 'NONE', ( #42082 ), #51422, .F. ) ;
#35330 = CARTESIAN_POINT ( 'NONE',  ( 0.000000000000000000, -75.20000000000000284, 0.000000000000000000 ) ) ;
#35331 = CARTESIAN_POINT ( 'NONE',  ( 0.1963495408493637351, -80.03541666666670551, -1.499999999999999778 ) ) ;
#35332 = CARTESIAN_POINT ( 'NONE',  ( -4.052894509781999943, -78.55792549782628953, -0.7950448020103999536 ) ) ;
#35333 = CARTESIAN_POINT ( 'NONE',  ( -6.519655663280999214, -77.25306001420199209, 7.413858028194999505 ) ) ;
#35334 = CARTESIAN_POINT ( 'NONE',  ( -1.250000000000000000, -83.49999999999998579, 0.000000000000000000 ) ) ;
#35335 = AXIS2_PLACEMENT_3D ( 'NONE', #34793, #56103, #56959 ) ;
#35336 = DIRECTION ( 'NONE',  ( 1.000000000000000000, 0.000000000000000000, 0.000000000000000000 ) ) ;
#35337 = CARTESIAN_POINT ( 'NONE',  ( 2.015551294784000191, -23.80347704843999779, 12.79857978895000059 ) ) ;
#35338 = CARTESIAN_POINT ( 'NONE',  ( 10.80348683896753137, -79.86729337777099147, 2.390241153868426505 ) ) ;
#35339 = CARTESIAN_POINT ( 'NONE',  ( 0.5786309740341742947, -78.42119534047722595, 12.05093123062573213 ) ) ;
#35340 = CARTESIAN_POINT ( 'NONE',  ( -1.092232985442824100, -80.95833333333330017, 0.6295237254636200097 ) ) ;
#35341 = ADVANCED_FACE ( 'NONE', ( #19066 ), #37054, .F. ) ;
#35342 = CARTESIAN_POINT ( 'NONE',  ( -0.1550674183001617967, -80.23188492957339690, 1.542021311756852864 ) ) ;
#35343 = LINE ( 'NONE', #40076, #24942 ) ;
#35344 = CARTESIAN_POINT ( 'NONE',  ( 0.2526653223220000632, -78.77055390729400131, 1.594795962155999947 ) ) ;
#35345 = CARTESIAN_POINT ( 'NONE',  ( -10.53003236233000095, -23.32452273707999879, -7.612971540276999960 ) ) ;
#35346 = CARTESIAN_POINT ( 'NONE',  ( -9.904830252356999765, -76.99205734789899225, 4.590139709818999769 ) ) ;
#35347 = CARTESIAN_POINT ( 'NONE',  ( -7.278283919121999901, -77.36717634323900938, 9.747261860606000639 ) ) ;
#35348 = FACE_OUTER_BOUND ( 'NONE', #51119, .T. ) ;
#35350 = CARTESIAN_POINT ( 'NONE',  ( 0.8816674349947000167, -78.05869998691809997, 0.9814419191067000892 ) ) ;
#35349 = CARTESIAN_POINT ( 'NONE',  ( -11.52285712076000834, -76.18393803225121985, 2.297929651431338982 ) ) ;
#35351 = CARTESIAN_POINT ( 'NONE',  ( 0.7304821784857000733, -81.47691005693999955, 1.273910602969000161 ) ) ;
#35352 = CARTESIAN_POINT ( 'NONE',  ( -9.358528765448124176, -79.55917755226546717, 5.292934104458898226 ) ) ;
#35353 = ORIENTED_EDGE ( 'NONE', *, *, #13970, .T. ) ;
#35354 = CARTESIAN_POINT ( 'NONE',  ( -10.07719973196000041, -20.25111654322000021, -7.718346056127999510 ) ) ;
#35355 = CARTESIAN_POINT ( 'NONE',  ( 2.220113589157999723, -79.83089276362140652, -11.83482178057999867 ) ) ;
#35356 = AXIS2_PLACEMENT_3D ( 'NONE', #44760, #220, #27323 ) ;
#35357 = CARTESIAN_POINT ( 'NONE',  ( 1.822780608403999913, -80.50309514466069061, 11.02275947276000068 ) ) ;
#35358 = CARTESIAN_POINT ( 'NONE',  ( 11.75000000000000178, -77.03958333333331154, -1.538071403319980268 ) ) ;
#35359 = CARTESIAN_POINT ( 'NONE',  ( -9.996770077891000028, -60.95065455317000414, 7.758602204140999881 ) ) ;
#35360 = AXIS2_PLACEMENT_3D ( 'NONE', #544, #46278, #49526 ) ;
#35361 = CARTESIAN_POINT ( 'NONE',  ( 0.6384810558836999661, -1.356750604646000058, -3.810785800737999995 ) ) ;
#35362 = CARTESIAN_POINT ( 'NONE',  ( 7.050245828045000884, -80.01787806992999208, 6.779143932755000712 ) ) ;
#35363 = CARTESIAN_POINT ( 'NONE',  ( 12.54976804508999955, -25.04775476228000031, 0.05637402076006000490 ) ) ;
#35364 = CARTESIAN_POINT ( 'NONE',  ( -2.062670899148999926, -55.49360374314999689, 12.83044039271999992 ) ) ;
#35365 = ORIENTED_EDGE ( 'NONE', *, *, #25748, .T. ) ;
#35366 = LINE ( 'NONE', #7654, #4094 ) ;
#35367 = CARTESIAN_POINT ( 'NONE',  ( 0.000000000000000000, -76.75499999999999545, 0.000000000000000000 ) ) ;
#35368 = DIRECTION ( 'NONE',  ( 0.000000000000000000, -1.000000000000000000, 0.000000000000000000 ) ) ;
#35369 = CARTESIAN_POINT ( 'NONE',  ( -10.35747158364999976, -60.11584477251999203, -7.626500902235000545 ) ) ;
#35370 = CARTESIAN_POINT ( 'NONE',  ( 3.088780581828999949, -85.55392953870899930, 1.744701995914999859 ) ) ;
#35371 = EDGE_LOOP ( 'NONE', ( #32560, #28504, #48974, #30748, #36333 ) ) ;
#35372 = DIRECTION ( 'NONE',  ( 0.000000000000000000, -1.000000000000000000, 0.000000000000000000 ) ) ;
#35373 = CARTESIAN_POINT ( 'NONE',  ( 7.764818829621773943, -77.87976087924900526, -8.854276815225853525 ) ) ;
#35374 = CARTESIAN_POINT ( 'NONE',  ( 0.000000000000000000, -90.35000000009100063, 0.000000000000000000 ) ) ;
#35375 = EDGE_LOOP ( 'NONE', ( #9429, #28323, #15155 ) ) ;
#35376 = EDGE_CURVE ( 'NONE', #30078, #2252, #3323, .T. ) ;
#35377 = CARTESIAN_POINT ( 'NONE',  ( -8.878349648264999061, -53.73036913477000098, -8.870329531799001188 ) ) ;
#35378 = CARTESIAN_POINT ( 'NONE',  ( 9.226480760116999136, -78.94040372155198781, -2.263195259622999611 ) ) ;
#35379 = ORIENTED_EDGE ( 'NONE', *, *, #58202, .T. ) ;
#35380 = VERTEX_POINT ( 'NONE', #29357 ) ;
#35381 = CARTESIAN_POINT ( 'NONE',  ( -6.658992300009000331, -76.27083001266900908, -10.40411675648000056 ) ) ;
#35382 = DIRECTION ( 'NONE',  ( 0.000000000000000000, -1.000000000000000000, 0.000000000000000000 ) ) ;
#35383 = VERTEX_POINT ( 'NONE', #43532 ) ;
#35384 = CARTESIAN_POINT ( 'NONE',  ( 0.000000000000000000, -75.20000000000000284, 7.200000000000000178 ) ) ;
#35385 = CARTESIAN_POINT ( 'NONE',  ( 0.8618151749125838590, -78.48198201294394494, -9.665976535993026530 ) ) ;
#35386 = CARTESIAN_POINT ( 'NONE',  ( 0.9442298177897724409, -80.29360019353696032, -0.8189497213649101770 ) ) ;
#35387 = CARTESIAN_POINT ( 'NONE',  ( -3.116139353062999717, -78.47578184934000944, 12.57467468523999976 ) ) ;
#35388 = DIRECTION ( 'NONE',  ( -1.000000000000000000, 0.000000000000000000, 0.000000000000000000 ) ) ;
#35389 = CARTESIAN_POINT ( 'NONE',  ( 12.99510751537000353, -15.69705297113999443, 6.911973076623003642 ) ) ;
#35390 = CARTESIAN_POINT ( 'NONE',  ( 1.368374140978811271, -86.25171435493598437, 3.153063748541271583 ) ) ;
#35391 = CARTESIAN_POINT ( 'NONE',  ( -7.301194973305000779, -79.33308617451200462, 8.515319286630999684 ) ) ;
#35392 = AXIS2_PLACEMENT_3D ( 'NONE', #12355, #16794, #21784 ) ;
#35393 = DIRECTION ( 'NONE',  ( 0.000000000000000000, -1.000000000000000000, 0.000000000000000000 ) ) ;
#35394 = LINE ( 'NONE', #58148, #20896 ) ;
#35395 = ORIENTED_EDGE ( 'NONE', *, *, #28233, .F. ) ;
#35396 = CARTESIAN_POINT ( 'NONE',  ( -11.19646453606000058, -79.12967694811598562, -1.252244488204000028 ) ) ;
#35397 = ADVANCED_FACE ( 'NONE', ( #57102 ), #35745, .F. ) ;
#35398 = CARTESIAN_POINT ( 'NONE',  ( 3.007117222848000093, -75.87269519504999948, 11.93703523519999976 ) ) ;
#35399 = CARTESIAN_POINT ( 'NONE',  ( 0.2630806288481999933, -79.88291798508399211, -1.292808645144999824 ) ) ;
#35400 = AXIS2_PLACEMENT_3D ( 'NONE', #22523, #41114, #417 ) ;
#35401 = CARTESIAN_POINT ( 'NONE',  ( -1.001490227998000027, -79.15975894690099324, -0.8734289068823000157 ) ) ;
#35402 = CARTESIAN_POINT ( 'NONE',  ( -1.202166735308230372, -3.252017009982586249, 3.308099677556824769 ) ) ;
#35403 = CARTESIAN_POINT ( 'NONE',  ( 12.71798269385000069, -23.29778754190000001, 1.931086388578000079 ) ) ;
#35404 = CARTESIAN_POINT ( 'NONE',  ( -12.75763395699000036, -19.22204592323999961, -1.931043742978000077 ) ) ;
#35405 = AXIS2_PLACEMENT_3D ( 'NONE', #12098, #34804, #16820 ) ;
#35406 = CARTESIAN_POINT ( 'NONE',  ( 9.050966799188000067, -55.64999999964999233, 7.919595949288999570 ) ) ;
#35407 = CARTESIAN_POINT ( 'NONE',  ( -10.76843015134999959, -79.98515786819298512, 1.073136842994000029 ) ) ;
#35408 = CARTESIAN_POINT ( 'NONE',  ( -4.911790911253000047, -77.46226498579800079, -8.407543791226999019 ) ) ;
#35409 = CARTESIAN_POINT ( 'NONE',  ( 6.055527902613000002, -77.71999999999999886, 7.319875806370000682 ) ) ;
#35410 = CARTESIAN_POINT ( 'NONE',  ( 8.596418555780450887, -79.69791666666668561, -6.606377239730321982 ) ) ;
#35411 = CARTESIAN_POINT ( 'NONE',  ( -8.982117338527000783, -79.69889424580067327, 6.718606902359000266 ) ) ;
#35412 = CARTESIAN_POINT ( 'NONE',  ( -1.407171709420465211, -77.88541666666667140, 10.74999999999999467 ) ) ;
#35413 = EDGE_CURVE ( 'NONE', #10827, #8754, #17759, .T. ) ;
#35414 = EDGE_LOOP ( 'NONE', ( #20648, #24746, #14638, #44349 ) ) ;
#35415 = CARTESIAN_POINT ( 'NONE',  ( 1.385204701026000018, -83.17972947813200335, -0.4875042294149000144 ) ) ;
#35416 = CARTESIAN_POINT ( 'NONE',  ( -0.7646200840319000713, -80.47830095821998952, -1.389155443296000048 ) ) ;
#35417 = FACE_OUTER_BOUND ( 'NONE', #49785, .T. ) ;
#35418 = CARTESIAN_POINT ( 'NONE',  ( -10.75000000000000000, -79.10000000000000853, 0.000000000000000000 ) ) ;
#35419 = CARTESIAN_POINT ( 'NONE',  ( -9.254388464354001087, -79.90752053325199711, 5.469807505829999528 ) ) ;
#35420 = FACE_OUTER_BOUND ( 'NONE', #15005, .T. ) ;
#35421 = CARTESIAN_POINT ( 'NONE',  ( 11.32533557775999888, -77.80105294172599883, -3.764608412264000226 ) ) ;
#35422 = CARTESIAN_POINT ( 'NONE',  ( -9.646692012709999986, -78.62005194988499568, 1.218660606027000215 ) ) ;
#35423 = CARTESIAN_POINT ( 'NONE',  ( -5.250896469870999006, -77.56454279010098674, 7.943454065752000304 ) ) ;
#35424 = CARTESIAN_POINT ( 'NONE',  ( 1.044910384896000188, -53.74473505772000692, -12.77260826194999943 ) ) ;
#35425 = CARTESIAN_POINT ( 'NONE',  ( 11.43430539595883388, -75.96832016884428640, 2.742965560814985881 ) ) ;
#35426 = CARTESIAN_POINT ( 'NONE',  ( -0.5608696358179350305, -85.88547955769999476, 4.510645591149664568 ) ) ;
#35427 = VERTEX_POINT ( 'NONE', #47979 ) ;
#35428 = CARTESIAN_POINT ( 'NONE',  ( 5.365645860858371030, -78.12749999999998352, 7.890595865543487797 ) ) ;
#35429 = CARTESIAN_POINT ( 'NONE',  ( 12.00000000000000000, -60.04999999966999980, 1.250000000000000000 ) ) ;
#35430 = CARTESIAN_POINT ( 'NONE',  ( -6.967078475965290174, -78.77478358560729532, -9.587638151555635702 ) ) ;
#35431 = CARTESIAN_POINT ( 'NONE',  ( -3.523652525393907720, -78.48547957940618858, -1.990986658322625669 ) ) ;
#35432 = B_SPLINE_CURVE_WITH_KNOTS ( 'NONE', 3,
 ( #33401, #24846, #16286, #38416, #25128, #51439 ),
 .UNSPECIFIED., .F., .F.,
 ( 4, 1, 1, 4 ),
 ( 0.000000000000000000, 0.3333333333333000081, 0.6666666666667000474, 1.000000000000000000 ),
 .UNSPECIFIED. ) ;
#35433 = CARTESIAN_POINT ( 'NONE',  ( -0.8762103189736000219, -81.35132337894999921, -1.416501064863000092 ) ) ;
#35434 = CARTESIAN_POINT ( 'NONE',  ( 1.633411169670999863, -77.97052377699598935, -11.09730050697999992 ) ) ;
#35435 = CARTESIAN_POINT ( 'NONE',  ( -10.57157196544999955, -79.91288308330898360, 2.324769239444999691 ) ) ;
#35436 = CARTESIAN_POINT ( 'NONE',  ( -2.831617975195505288, -80.38489583333210931, 10.53328982651339629 ) ) ;
#35437 = CARTESIAN_POINT ( 'NONE',  ( -10.58700924204000060, -76.96669458148599574, 6.201838006055000463 ) ) ;
#35438 = CARTESIAN_POINT ( 'NONE',  ( 2.593824895836550404, -78.55428885352219481, 11.47171456603886419 ) ) ;
#35439 = FACE_OUTER_BOUND ( 'NONE', #6020, .T. ) ;
#35440 = ORIENTED_EDGE ( 'NONE', *, *, #25996, .F. ) ;
#35441 = CARTESIAN_POINT ( 'NONE',  ( 5.768362037549999322, -78.30992220834100692, -9.403610972502001175 ) ) ;
#35442 = CARTESIAN_POINT ( 'NONE',  ( 1.154033295362816514, -79.88162843165144977, 0.4798940756958068876 ) ) ;
#35443 = EDGE_CURVE ( 'NONE', #55458, #49604, #17467, .T. ) ;
#35444 = DIRECTION ( 'NONE',  ( -0.9936845293270585300, 0.1122098755727947705, 0.000000000000000000 ) ) ;
#35445 = B_SPLINE_CURVE_WITH_KNOTS ( 'NONE', 3,
 ( #55410, #1697, #5236, #14956, #46285, #10847, #24412, #6106, #42131, #42428, #19691, #9962, #41248, #51584, #32954, #15552, #28530, #37978, #50999, #46579, #1997, #23241, #10250, #19991, #6397, #37691, #23527, #41835, #15257, #37100, #33545, #55710, #41539, #54829, #56002, #27655, #1121, #45697, #836, #18818, #32658, #36810, #14370, #32370, #50412, #27943, #45991, #19109, #55116, #14660, #50709, #11423, #48310, #39434, #3425, #56867, #16137, #56577, #16715, #52438, #43292, #33831, #24702, #11142, #29976, #20845, #43581, #47162, #2848, #11713, #34697, #7849, #48029, #7561 ),
 .UNSPECIFIED., .F., .F.,
 ( 4, 2, 2, 2, 2, 2, 2, 1, 1, 1, 1, 2, 2, 2, 2, 2, 1, 1, 1, 2, 2, 2, 2, 2, 1, 1, 1, 2, 2, 2, 2, 2, 1, 1, 1, 1, 2, 2, 1, 2, 2, 1, 1, 1, 2, 4 ),
 ( 0.000000000000000000, 0.04346818531367174082, 0.08693637062734348164, 0.1086704632841794249, 0.1195375096125975006, 0.1249710327768065871, 0.1253106279745698770, 0.1256502231723332086, 0.1263294135678600105, 0.1276877943589138642, 0.1304045559410215438, 0.1738727412547442785, 0.2173409265684669855, 0.2390750192253283946, 0.2499420655537591407, 0.2506212559492860814, 0.2513004463448130776, 0.2526588271358671256, 0.2553755887179749995, 0.2608091118821907473, 0.3477454825096416569, 0.3694795751665044259, 0.3749130983307200626, 0.3755922887262470033, 0.3762714791217740551, 0.3776298599128280475, 0.3803466214949359214, 0.3912136678233673059, 0.4346818531370924554, 0.4781500384508176604, 0.4998841311076802629, 0.5005633215032072592, 0.5012425118987341444, 0.5026008926897881368, 0.5053176542718960107, 0.5107511774361116474, 0.5216182237645430320, 0.6085545943919933309, 0.6194216407204246044, 0.6248551638846403522, 0.6255343542801672374, 0.6262135446756940116, 0.6275719254667480040, 0.6302886870488556559, 0.6520227797057175367, 0.6954909650194412984 ),
 .UNSPECIFIED. ) ;
#35446 = CARTESIAN_POINT ( 'NONE',  ( -7.730500772889000061, -79.67897315952798465, 8.045567737375000306 ) ) ;
#35447 = CARTESIAN_POINT ( 'NONE',  ( -12.50728313511820922, -53.80024825451957327, 0.1773838729375966927 ) ) ;
#35448 = CARTESIAN_POINT ( 'NONE',  ( -1.339212577895066758, -81.81085671282828287, 0.7051202410463707215 ) ) ;
#35449 = CARTESIAN_POINT ( 'NONE',  ( -0.08732773870155000062, -78.70215651189698747, 12.27958277169999945 ) ) ;
#35450 = AXIS2_PLACEMENT_3D ( 'NONE', #31374, #49417, #40251 ) ;
#35451 = EDGE_CURVE ( 'NONE', #1173, #36999, #534, .T. ) ;
#35452 = CARTESIAN_POINT ( 'NONE',  ( -12.50000000000000000, -60.04999999966999980, -1.250000000000000000 ) ) ;
#35453 = AXIS2_PLACEMENT_3D ( 'NONE', #50653, #55649, #46818 ) ;
#35454 = CARTESIAN_POINT ( 'NONE',  ( 0.000000000000000000, -26.10094976978000147, 0.000000000000000000 ) ) ;
#35455 = ADVANCED_FACE ( 'NONE', ( #56246, #52109, #49349, #8896 ), #52397, .F. ) ;
#35456 = CARTESIAN_POINT ( 'NONE',  ( 2.813789756862229652, -78.35416666666665719, 10.47020627418440064 ) ) ;
#35457 = CARTESIAN_POINT ( 'NONE',  ( 7.483407197968000801, -79.75000000000000000, -5.437013583705000208 ) ) ;
#35458 = ORIENTED_EDGE ( 'NONE', *, *, #35189, .T. ) ;
#35459 = CONICAL_SURFACE ( 'NONE', #41265, 9.349999999968000353, 0.7853981633972997312 ) ;
#35460 = ORIENTED_EDGE ( 'NONE', *, *, #45850, .F. ) ;
#35461 = CARTESIAN_POINT ( 'NONE',  ( -10.75000000000000000, -78.00000000000000000, 2.252154972635999871E-14 ) ) ;
#35462 = CARTESIAN_POINT ( 'NONE',  ( -0.1199120982448000083, -77.75333998579800721, -9.541815775584998605 ) ) ;
#35463 = ORIENTED_EDGE ( 'NONE', *, *, #35758, .T. ) ;
#35464 = DIRECTION ( 'NONE',  ( -1.000000000000000000, 0.000000000000000000, 0.000000000000000000 ) ) ;
#35465 = ORIENTED_EDGE ( 'NONE', *, *, #19768, .F. ) ;
#35466 = CARTESIAN_POINT ( 'NONE',  ( 9.516272955293000990, -24.82538765621999843, 8.227498559427999680 ) ) ;
#35467 = CARTESIAN_POINT ( 'NONE',  ( -10.45205659049000069, -19.23767314807999895, 7.651160337241000420 ) ) ;
#35468 = CARTESIAN_POINT ( 'NONE',  ( -5.132841502757762520, -78.17821230117139919, -7.695201808387375664 ) ) ;
#35469 = CARTESIAN_POINT ( 'NONE',  ( 2.179295889402999897, -78.55775731164598596, 11.00312592022000047 ) ) ;
#35470 = CARTESIAN_POINT ( 'NONE',  ( 0.8568216711331626545, -79.41513557398620549, 0.9100032604084061783 ) ) ;
#35471 = VERTEX_POINT ( 'NONE', #38226 ) ;
#35472 = VERTEX_POINT ( 'NONE', #15796 ) ;
#35473 = CARTESIAN_POINT ( 'NONE',  ( -1.453085306447361003, -77.48762070070470998, 9.135110569084051946 ) ) ;
#35474 = CARTESIAN_POINT ( 'NONE',  ( 3.792698199283999649, -77.96245195745699164, -10.36819406884000117 ) ) ;
#35475 = SURFACE_STYLE_USAGE ( .BOTH. , #7768 ) ;
#35476 = CARTESIAN_POINT ( 'NONE',  ( 4.746041175454999816, -77.49581766116699555, -8.464384343845999581 ) ) ;
#35477 = CARTESIAN_POINT ( 'NONE',  ( 12.26635331368000159, -76.28453882784999962, 4.664607203767999977 ) ) ;
#35478 = CARTESIAN_POINT ( 'NONE',  ( -8.958921704583302059, -79.42676566002430150, -3.161023900737553127 ) ) ;
#35479 = CARTESIAN_POINT ( 'NONE',  ( 7.864797288573664780, -54.34877151149995456, -10.10445166985919840 ) ) ;
#35480 = CARTESIAN_POINT ( 'NONE',  ( 8.693423296916000353, -80.06508647311397908, -7.148151291522000683 ) ) ;
#35481 = CARTESIAN_POINT ( 'NONE',  ( 12.77651047532000028, -16.69104280938000073, 0.04320343284647000515 ) ) ;
#35482 = CARTESIAN_POINT ( 'NONE',  ( -10.07616267220999973, -24.72631139030000114, -7.986947465007999014 ) ) ;
#35483 = CARTESIAN_POINT ( 'NONE',  ( -10.83564775471081099, -76.66805056338695579, 4.543779009287320925 ) ) ;
#35484 = EDGE_CURVE ( 'NONE', #12549, #43416, #40182, .T. ) ;
#35485 = ORIENTED_EDGE ( 'NONE', *, *, #44213, .F. ) ;
#35486 = CARTESIAN_POINT ( 'NONE',  ( 12.19992621721999981, -79.20211240836600552, 1.693460693027999842 ) ) ;
#35487 = CARTESIAN_POINT ( 'NONE',  ( -8.533817832752999877, -53.79473856423000200, 9.213092693279001821 ) ) ;
#35488 = CARTESIAN_POINT ( 'NONE',  ( -5.786162884931686179, -78.02038376788627261, 9.061535599160601251 ) ) ;
#35489 = ADVANCED_FACE ( 'NONE', ( #39094 ), #52382, .T. ) ;
#35490 = CARTESIAN_POINT ( 'NONE',  ( 9.789819849890999848, -78.83501197700098828, -6.904744247936999813 ) ) ;
#35491 = CARTESIAN_POINT ( 'NONE',  ( -10.53562613913999968, -18.79442116269000351, -7.620013630324000253 ) ) ;
#35492 = CONICAL_SURFACE ( 'NONE', #10078, 13.94999999993999928, 0.7853981633972997312 ) ;
#35494 = CARTESIAN_POINT ( 'NONE',  ( 0.000000000000000000, -90.29999999999999716, 0.000000000000000000 ) ) ;
#35493 = CARTESIAN_POINT ( 'NONE',  ( 2.426647618366673645E-14, -5.899999999999999467, -12.90000000000000036 ) ) ;
#35495 = CARTESIAN_POINT ( 'NONE',  ( 0.2494208075035535266, -53.80711039216215852, 12.50614183109565047 ) ) ;
#35496 = CARTESIAN_POINT ( 'NONE',  ( -11.04620438670000127, -80.55603373794698996, 0.1137957503148000066 ) ) ;
#35497 = PLANE ( 'NONE',  #34816 ) ;
#35498 = CARTESIAN_POINT ( 'NONE',  ( -4.550163292746999488, -77.41531204370200214, -10.30194052436999996 ) ) ;
#35499 = CARTESIAN_POINT ( 'NONE',  ( 2.839805762151334179, -1.791666666666666519, 1.636761686205429056 ) ) ;
#35500 = CARTESIAN_POINT ( 'NONE',  ( -1.822066877594999967, -80.21134816220060770, 11.10737283064000103 ) ) ;
#35501 = AXIS2_PLACEMENT_3D ( 'NONE', #43651, #47808, #12063 ) ;
#35502 = ORIENTED_EDGE ( 'NONE', *, *, #28645, .T. ) ;
#35503 = CARTESIAN_POINT ( 'NONE',  ( 1.996848836733677857, -1.424485875898780618, 2.599776808039695908 ) ) ;
#35504 = CARTESIAN_POINT ( 'NONE',  ( -1.801750019967000016, -55.40992573246000319, 12.59656967650999881 ) ) ;
#35505 = CARTESIAN_POINT ( 'NONE',  ( 11.65000000000000036, -75.20000000000000284, 0.000000000000000000 ) ) ;
#35506 = AXIS2_PLACEMENT_3D ( 'NONE', #5107, #18104, #49101 ) ;
#35507 = CARTESIAN_POINT ( 'NONE',  ( 1.416261411028999939, -1.974711001041000280, 3.359468912789999706 ) ) ;
#35508 = CARTESIAN_POINT ( 'NONE',  ( 9.118072387854001093, -79.75045691161798800, -2.384738962471999901 ) ) ;
#35509 = AXIS2_PLACEMENT_3D ( 'NONE', #28210, #36216, #9944 ) ;
#35510 = CARTESIAN_POINT ( 'NONE',  ( 8.300970689365456678, -77.50833333333332575, -4.784380313523530326 ) ) ;
#35511 = LINE ( 'NONE', #57098, #9197 ) ;
#35512 = CARTESIAN_POINT ( 'NONE',  ( -1.466594960155999994, -60.88158199018999994, 12.44238958335999889 ) ) ;
#35513 = CARTESIAN_POINT ( 'NONE',  ( 12.43641395964999852, -17.08198970748000178, -0.03481089025434000450 ) ) ;
#35514 = CARTESIAN_POINT ( 'NONE',  ( -2.667898297452999667, -84.54699735065199206, 3.211217596898999993 ) ) ;
#35515 = EDGE_CURVE ( 'NONE', #41301, #9760, #41706, .T. ) ;
#35516 = FACE_OUTER_BOUND ( 'NONE', #1598, .T. ) ;
#35517 = B_SPLINE_CURVE_WITH_KNOTS ( 'NONE', 3,
 ( #43575, #3138, #56287, #2558, #20559, #19985, #15543, #25269, #38557, #56572, #16131, #34108, #29112, #6688, #42707, #2274, #20271, #49546, #4366, #49842, #40074, #58091, #27079, #53667, #22669, #40681, #9091, #45120, #17950, #57796, #31499, #36244, #21495, #17353, #17651, #45414, #22368, #40380, #13507, #58388, #31202, #35048, #35942, #22066, #273, #26488, #39782, #4670, #18252, #30913, #3774, #31800, #35639, #54265, #13207, #13798, #9389, #27377, #39501, #53969, #35342, #44512, #8492, #57505, #17067, #53365, #53082, #48949, #4062, #12916, #12637, #49241, #30629, #48662, #8792, #26784, #44813, #8207, #26209, #44226, #21778, #9679, #565, #6119, #23537, #28544, #55127, #51011, #19121, #848, #41263, #36534, #14672, #32097, #27667, #41550, #46004, #5528, #45713, #37112, #9976, #32669, #14970, #40973, #5249, #1133, #10561, #50136 ),
 .UNSPECIFIED., .F., .F.,
 ( 4, 2, 2, 2, 2, 2, 1, 2, 2, 2, 2, 2, 2, 2, 2, 2, 2, 2, 2, 2, 2, 2, 2, 2, 2, 2, 2, 2, 2, 2, 2, 2, 2, 2, 2, 2, 2, 2, 2, 2, 2, 2, 2, 2, 2, 2, 2, 2, 1, 2, 2, 2, 2, 2, 4 ),
 ( 0.000000000000000000, 0.01562500000000001041, 0.03125000000000001388, 0.04687500000000002082, 0.06250000000000002776, 0.07812500000000004163, 0.09375000000000004163, 0.1093750000000000416, 0.1250000000000000278, 0.1406250000000000278, 0.1562500000000000555, 0.1718750000000000555, 0.1875000000000000555, 0.2031250000000000833, 0.2187500000000000833, 0.2343750000000001110, 0.2500000000000001110, 0.2656250000000001110, 0.2812500000000001110, 0.2968750000000001665, 0.3125000000000001665, 0.3281250000000001665, 0.3437500000000001665, 0.3750000000000001110, 0.4062500000000001110, 0.4375000000000000555, 0.4687500000000000555, 0.5000000000000000000, 0.5312499999999998890, 0.5624999999999997780, 0.5937499999999998890, 0.6249999999999998890, 0.6562499999999998890, 0.6718749999999998890, 0.6874999999999998890, 0.7031249999999998890, 0.7187499999999998890, 0.7343749999999998890, 0.7499999999999998890, 0.7656250000000000000, 0.7812500000000000000, 0.7968750000000000000, 0.8125000000000000000, 0.8281250000000000000, 0.8437500000000000000, 0.8593750000000000000, 0.8750000000000000000, 0.8906250000000000000, 0.9062500000000000000, 0.9218750000000001110, 0.9375000000000001110, 0.9531250000000001110, 0.9687500000000001110, 0.9843750000000001110, 1.000000000000000000 ),
 .UNSPECIFIED. ) ;
#35518 = CARTESIAN_POINT ( 'NONE',  ( 12.03307672610699441, -76.69641582315870210, -1.008565388800895191 ) ) ;
#35519 = CARTESIAN_POINT ( 'NONE',  ( 10.74399384636999955, -78.87441265908000787, -6.654290843581000203 ) ) ;
#35520 = CARTESIAN_POINT ( 'NONE',  ( -8.684735281668000795, -77.83151106797200214, -7.170030519161000093 ) ) ;
#35521 = CARTESIAN_POINT ( 'NONE',  ( 0.8752045112715043373, -81.91385899954191530, 0.8919628724664445674 ) ) ;
#35522 = CARTESIAN_POINT ( 'NONE',  ( -0.6667013398134999935, -78.48293648134999501, -1.398288081058000065 ) ) ;
#35523 = CARTESIAN_POINT ( 'NONE',  ( 1.575772165441551964, -61.26154542760956900, 12.70597445621661059 ) ) ;
#35524 = CARTESIAN_POINT ( 'NONE',  ( 1.051432699053240105, -82.93622825826652445, -1.083844963264632977 ) ) ;
#35525 = CARTESIAN_POINT ( 'NONE',  ( -3.250000000000000000, -2.500000000000000000, 0.000000000000000000 ) ) ;
#35526 = CARTESIAN_POINT ( 'NONE',  ( 3.969016993814154848, -80.25512807981924368, -9.991659506732283091 ) ) ;
#35527 = LINE ( 'NONE', #40264, #28736 ) ;
#35528 = CARTESIAN_POINT ( 'NONE',  ( -1.172432707911829297, -77.68180296370584870, -0.4984351444782006424 ) ) ;
#35529 = ADVANCED_BREP_SHAPE_REPRESENTATION ( '', ( #56346, #43526 ), #49207 ) ;
#35530 = EDGE_CURVE ( 'NONE', #44472, #8017, #15589, .T. ) ;
#35531 = CARTESIAN_POINT ( 'NONE',  ( 0.9143116702203477608, -81.79083299997489576, -0.8519700409851096445 ) ) ;
#35532 = DIRECTION ( 'NONE',  ( 0.000000000000000000, 1.000000000000000000, 0.000000000000000000 ) ) ;
#35533 = CARTESIAN_POINT ( 'NONE',  ( 10.58513040395000004, -78.60114051593500051, 3.845644306921999878 ) ) ;
#35534 = CARTESIAN_POINT ( 'NONE',  ( 0.7681833999686451531, -80.17708333333334281, -0.9995835529977240563 ) ) ;
#35535 = ORIENTED_EDGE ( 'NONE', *, *, #8970, .F. ) ;
#35536 = VERTEX_POINT ( 'NONE', #24804 ) ;
#35537 = CARTESIAN_POINT ( 'NONE',  ( 0.000000000000000000, -77.70312499986998489, 0.000000000000000000 ) ) ;
#35538 = VERTEX_POINT ( 'NONE', #29216 ) ;
#35539 =( LENGTH_UNIT ( ) NAMED_UNIT ( * ) SI_UNIT ( .MILLI., .METRE. ) );
#35540 = VECTOR ( 'NONE', #26922, 1000.000000000000000 ) ;
#35541 = EDGE_LOOP ( 'NONE', ( #1599, #14493, #10460, #36673 ) ) ;
#35542 = CARTESIAN_POINT ( 'NONE',  ( 0.000000000000000000, -5.200000000000000178, 0.000000000000000000 ) ) ;
#35543 = CARTESIAN_POINT ( 'NONE',  ( 1.730605770088500472, -79.20104166191323714, -2.976826296013844075 ) ) ;
#35544 = AXIS2_PLACEMENT_3D ( 'NONE', #8286, #39292, #16576 ) ;
#35545 = CARTESIAN_POINT ( 'NONE',  ( -11.02198032011999906, -79.64450301542999000, -0.4665663988222000236 ) ) ;
#35546 = CARTESIAN_POINT ( 'NONE',  ( 2.065394024360999836, -23.42161432646000208, -12.82193048528000112 ) ) ;
#35547 = CARTESIAN_POINT ( 'NONE',  ( -1.963416759258999722, -80.25345679254499487, 3.442525934388999787 ) ) ;
#35548 = CARTESIAN_POINT ( 'NONE',  ( -1.341561494378749719, -79.28604399664807545, 9.404764964287370077 ) ) ;
#35549 = ORIENTED_EDGE ( 'NONE', *, *, #10925, .T. ) ;
#35550 = FACE_OUTER_BOUND ( 'NONE', #41079, .T. ) ;
#35551 = CARTESIAN_POINT ( 'NONE',  ( 11.76256880100000046, -78.69015337716000147, 3.275611217918000140 ) ) ;
#35552 = VECTOR ( 'NONE', #254, 1000.000000000000227 ) ;
#35553 = VERTEX_POINT ( 'NONE', #34216 ) ;
#35554 = ORIENTED_EDGE ( 'NONE', *, *, #31409, .F. ) ;
#35555 = DIRECTION ( 'NONE',  ( 0.7071067811865473507, -1.433669009702094715E-08, -0.7071067811865473507 ) ) ;
#35556 = CARTESIAN_POINT ( 'NONE',  ( -1.473982314889778600, -77.76680499034375771, -0.3169618534076995564 ) ) ;
#35557 = CIRCLE ( 'NONE', #30834, 2.000000000000001776 ) ;
#35558 = CARTESIAN_POINT ( 'NONE',  ( -1.185397549814999785, -80.30353753009200091, -0.6110718436566999756 ) ) ;
#35559 = CARTESIAN_POINT ( 'NONE',  ( 1.882180247600000245, -78.56901263324199647, 9.519879562373999349 ) ) ;
#35560 = CARTESIAN_POINT ( 'NONE',  ( -4.452050888846053489, -86.36264283715696877, -0.4261719148253248490 ) ) ;
#35561 = CARTESIAN_POINT ( 'NONE',  ( 2.133191202286643051, -85.88405207176444378, 2.764547849547144498 ) ) ;
#35562 = CARTESIAN_POINT ( 'NONE',  ( -3.372301964606999825, -76.90131824283000128, 12.67255275672000003 ) ) ;
#35563 = CARTESIAN_POINT ( 'NONE',  ( 12.20990109347999919, -76.47356177075999994, -3.270330254029999661 ) ) ;
#35564 = CARTESIAN_POINT ( 'NONE',  ( -10.81829297021999992, -76.44441179485198745, 1.986553170785000155 ) ) ;
#35565 = CARTESIAN_POINT ( 'NONE',  ( -9.250000000000000000, -78.59999999999999432, 0.000000000000000000 ) ) ;
#35566 = CARTESIAN_POINT ( 'NONE',  ( 5.256696614975999715, -77.33533667140099510, 7.937185564810000038 ) ) ;
#35567 = CARTESIAN_POINT ( 'NONE',  ( -10.18491068061999982, -60.10716934574000447, 7.640030139773000606 ) ) ;
#35568 = CARTESIAN_POINT ( 'NONE',  ( 1.034282562214086543, -2.950585576526748355, 3.080402021841319726 ) ) ;
#35569 = CARTESIAN_POINT ( 'NONE',  ( -3.412299873766000413, -78.67863830014491100, 0.4934769004953000193 ) ) ;
#35570 = FACE_OUTER_BOUND ( 'NONE', #27699, .T. ) ;
#35571 = CARTESIAN_POINT ( 'NONE',  ( -0.8455117474470024153, -80.98139262285351947, 10.71661036402546330 ) ) ;
#35572 = CARTESIAN_POINT ( 'NONE',  ( 11.22355342542000045, -80.59075526750170582, 0.9700744431168999427 ) ) ;
#35573 = CARTESIAN_POINT ( 'NONE',  ( 3.171758640500000226, -3.602072692704999746, 1.479846994257000059 ) ) ;
#35574 = CARTESIAN_POINT ( 'NONE',  ( 0.4728636598485260745, -79.59476634619571200, 1.184081205126365388 ) ) ;
#35575 = ORIENTED_EDGE ( 'NONE', *, *, #24696, .F. ) ;
#35576 = CARTESIAN_POINT ( 'NONE',  ( -4.000000000000000000, -5.000000000000000000, 0.5999999999999999778 ) ) ;
#35577 = DIRECTION ( 'NONE',  ( 1.000000000000000000, 0.000000000000000000, 0.000000000000000000 ) ) ;
#35578 = CARTESIAN_POINT ( 'NONE',  ( -0.9657971644277000278, -82.23865798662500026, -0.9195906491977999808 ) ) ;
#35579 = CARTESIAN_POINT ( 'NONE',  ( 2.062673488738000049, -55.47547470607999998, 12.82904091336000008 ) ) ;
#35580 = CARTESIAN_POINT ( 'NONE',  ( 7.411516475408999050, -77.15588683971000705, -10.69619859711000132 ) ) ;
#35581 = AXIS2_PLACEMENT_3D ( 'NONE', #403, #53811, #17796 ) ;
#35582 = EDGE_CURVE ( 'NONE', #35000, #24789, #6208, .T. ) ;
#35583 = CARTESIAN_POINT ( 'NONE',  ( -8.792818914796958651, -62.02696626408313563, -9.175540344859795638 ) ) ;
#35584 = CARTESIAN_POINT ( 'NONE',  ( 11.94419429569000002, -76.22030556059000617, -3.727676827021999983 ) ) ;
#35585 = ORIENTED_EDGE ( 'NONE', *, *, #28250, .T. ) ;
#35586 = LINE ( 'NONE', #53035, #13487 ) ;
#35587 = VECTOR ( 'NONE', #19588, 1000.000000000000000 ) ;
#35588 = CARTESIAN_POINT ( 'NONE',  ( -1.356221256960000066, -80.87683204993798824, -0.4246310591675999668 ) ) ;
#35589 = CARTESIAN_POINT ( 'NONE',  ( -2.062673488410000200, -23.32452273707999879, -12.82904109062999964 ) ) ;
#35590 = CARTESIAN_POINT ( 'NONE',  ( 8.085542028362999289, -78.16265682217398592, -5.029352477166999513 ) ) ;
#35592 = CARTESIAN_POINT ( 'NONE',  ( -3.249661007175000282, -0.7674197747463000763, 2.357191814219000037 ) ) ;
#35591 = CARTESIAN_POINT ( 'NONE',  ( -3.844964336665000371, -84.42243313234698121, 1.508231652767000108 ) ) ;
#35593 = CARTESIAN_POINT ( 'NONE',  ( -5.052420809101000088E-14, -80.79999999999999716, -13.89999999999999858 ) ) ;
#35594 = CARTESIAN_POINT ( 'NONE',  ( 1.413837046361000160, -79.34676037349100852, -0.1054710693050000120 ) ) ;
#35595 = ORIENTED_EDGE ( 'NONE', *, *, #2605, .F. ) ;
#35596 = CARTESIAN_POINT ( 'NONE',  ( -4.008563851605106976, -77.19461823621462315, -9.976209684486235574 ) ) ;
#35597 = CARTESIAN_POINT ( 'NONE',  ( 6.760013919724043419, -78.87708333333334565, -8.796335266379996298 ) ) ;
#35598 = VECTOR ( 'NONE', #57248, 1000.000000000000000 ) ;
#35599 = CARTESIAN_POINT ( 'NONE',  ( 3.407095545933001013, -78.77851879815550262, 6.814191091866031336 ) ) ;
#35600 = ORIENTED_EDGE ( 'NONE', *, *, #13607, .F. ) ;
#35602 = EDGE_CURVE ( 'NONE', #39760, #38477, #57901, .T. ) ;
#35601 = ORIENTED_EDGE ( 'NONE', *, *, #52437, .F. ) ;
#35603 = CARTESIAN_POINT ( 'NONE',  ( 0.000000000000000000, -77.00000000000000000, 0.000000000000000000 ) ) ;
#35604 = CARTESIAN_POINT ( 'NONE',  ( -11.75651041636212746, -76.05651041660414080, -1.538071389465395677 ) ) ;
#35605 = LINE ( 'NONE', #27913, #34085 ) ;
#35606 = ORIENTED_EDGE ( 'NONE', *, *, #8092, .F. ) ;
#35607 = CARTESIAN_POINT ( 'NONE',  ( -8.937463246932001226, -78.13263333629100771, 8.081925660605000061 ) ) ;
#35608 = ORIENTED_EDGE ( 'NONE', *, *, #54253, .T. ) ;
#35609 = VERTEX_POINT ( 'NONE', #25086 ) ;
#35610 = CARTESIAN_POINT ( 'NONE',  ( -12.00000000000000000, -18.84999999997999964, 0.7999999999999001243 ) ) ;
#35611 = EDGE_CURVE ( 'NONE', #4309, #13771, #4360, .T. ) ;
#35612 = DIRECTION ( 'NONE',  ( -0.7071067811865475727, 0.000000000000000000, 0.7071067811865475727 ) ) ;
#35613 = DIRECTION ( 'NONE',  ( 0.000000000000000000, 1.000000000000000000, -1.868195065453000187E-14 ) ) ;
#35614 = EDGE_CURVE ( 'NONE', #20674, #26795, #19502, .T. ) ;
#35615 = B_SPLINE_SURFACE_WITH_KNOTS ( 'NONE', 3, 3, ( 
 ( #55202, #1205, #10051, #15631, #50792, #29196, #20354, #42796, #37774, #55496, #37475, #56085, #33337, #46368, #51372, #19482, #1492, #5893, #51670, #10633, #5600, #10929, #51084, #24201, #28316, #42505, #2076, #50497, #23901, #15046, #46077, #28910, #33038, #20074, #41920 ),
 ( #55795, #28616, #46661, #41625, #46954, #37188, #10337, #1783, #42217, #19778, #6188, #6480, #24491, #38064, #33628, #19196, #11217, #14745, #32744, #47242, #6773, #23611, #38351, #24782, #2358, #56372, #15923, #28033, #39212, #38642, #29481, #53087, #12070, #17070, #25635 ),
 ( #2646, #43945, #57509, #30341, #25348, #21499, #51950, #7922, #43088, #7064, #16501, #56660, #48384, #21206, #3496, #11506, #25064, #52514, #33910, #57227, #20924, #30050, #20640, #39505, #29761, #56942, #35052, #34774, #16215, #47539, #34193, #52230, #25922, #11787, #47818 ),
 ( #43364, #16792, #7348, #52798, #2923, #48102, #38925, #34483, #7635, #43660, #3219, #12353, #47145, #29102, #2546, #56276, #33814, #33231, #46853, #20549, #38545, #24396, #56559, #15534, #37378, #15238, #55392, #15826, #23800, #10830, #16120, #47435, #6677, #24096, #42410 ) ),
 .UNSPECIFIED., .F., .F., .F.,
 ( 4, 4 ),
 ( 4, 1, 1, 1, 1, 1, 1, 1, 1, 1, 1, 1, 1, 1, 1, 1, 1, 1, 1, 1, 1, 1, 1, 1, 1, 1, 1, 1, 1, 1, 1, 1, 4 ),
 ( -0.3708084972812999980, 1.370808497280999960 ),
 ( 0.1624174856069000028, 0.1891051637615999981, 0.2157928419163000211, 0.2424805200710000164, 0.2691681982257000394, 0.2958558763803000313, 0.3225435545349999988, 0.3492312326897000219, 0.3759189108443999894, 0.4026065889991000124, 0.4292942671537000043, 0.4559819453084000274, 0.4826696234630999949, 0.5093573016178000179, 0.5360449797724999854, 0.5627326579270999218, 0.5894203360818000004, 0.6161080142365000789, 0.6427956923911999354, 0.6694833705459000139, 0.6961710487005999815, 0.7228587268552000289, 0.7495464050098999964, 0.7762340831645999639, 0.8029217613193000425, 0.8296094394739998990, 0.8562971176285999464, 0.8829847957833000249, 0.9096724739379999924, 0.9363601520926999600, 0.9630478302474000385, 0.9897355084019999749, 1.016423186556999925 ),
 .UNSPECIFIED. ) ;
#35616 = VERTEX_POINT ( 'NONE', #57247 ) ;
#35617 = VERTEX_POINT ( 'NONE', #17380 ) ;
#35618 = CARTESIAN_POINT ( 'NONE',  ( 9.249824691843906876, -79.33960135255351531, -1.210482662510009799 ) ) ;
#35619 = CARTESIAN_POINT ( 'NONE',  ( 1.974456364585914558, -78.72609999968184979, -3.418760544058739637 ) ) ;
#35620 = DIRECTION ( 'NONE',  ( -1.000000000000000000, 0.000000000000000000, 0.000000000000000000 ) ) ;
#35621 = CARTESIAN_POINT ( 'NONE',  ( -7.613962745608000127, -23.30639784948999704, -10.53101990620000095 ) ) ;
#35622 = CARTESIAN_POINT ( 'NONE',  ( -1.537891305778452233, -77.31276490156547254, -11.67737886329171815 ) ) ;
#35623 = CARTESIAN_POINT ( 'NONE',  ( -10.26699006316255591, -78.75833333333332575, 5.917523019358029934 ) ) ;
#35624 = CARTESIAN_POINT ( 'NONE',  ( 7.668936932630000314, -56.02847221959000024, -10.21380041493999968 ) ) ;
#35625 = CARTESIAN_POINT ( 'NONE',  ( -7.954951288349001004, -60.24678171298000251, -9.722718241315000398 ) ) ;
#35626 = CARTESIAN_POINT ( 'NONE',  ( 0.5999999999999999778, -23.15000000000000213, -10.98362417419999915 ) ) ;
#35627 = CARTESIAN_POINT ( 'NONE',  ( 1.310679582531388387, -80.10833333333333428, -0.7554284705563470981 ) ) ;
#35628 = EDGE_CURVE ( 'NONE', #9567, #35617, #3627, .T. ) ;
#35629 = CARTESIAN_POINT ( 'NONE',  ( 1.620950162628999935, -80.68280496681198599, -3.844812462229999728 ) ) ;
#35630 = CARTESIAN_POINT ( 'NONE',  ( 4.993566916646000386, -77.65346001420199684, 8.516776984568000586 ) ) ;
#35631 = DIRECTION ( 'NONE',  ( 0.7071067811864970576, -0.7071067811865969777, 3.680441427362984728E-08 ) ) ;
#35632 = CONICAL_SURFACE ( 'NONE', #38484, 12.74999999937999995, 0.7853981633972997312 ) ;
#35633 = DIRECTION ( 'NONE',  ( 0.000000000000000000, 0.000000000000000000, -1.000000000000000000 ) ) ;
#35634 = CARTESIAN_POINT ( 'NONE',  ( -1.056237665594999875, -25.04866013698000060, 12.77256098197999989 ) ) ;
#35635 = DIRECTION ( 'NONE',  ( -1.000000000000000000, 0.000000000000000000, 0.000000000000000000 ) ) ;
#35636 = FACE_OUTER_BOUND ( 'NONE', #24894, .T. ) ;
#35637 = CARTESIAN_POINT ( 'NONE',  ( 4.086558352703000274, -1.033853494985000010, -0.5436765409910000457 ) ) ;
#35638 = CARTESIAN_POINT ( 'NONE',  ( 2.244378098519284936, -78.24176656480896952, -10.54564492727542024 ) ) ;
#35639 = CARTESIAN_POINT ( 'NONE',  ( 0.01771975371708433070, -80.47481071735674618, -1.547929127693172147 ) ) ;
#35640 = CARTESIAN_POINT ( 'NONE',  ( -0.6573153308273406159, -78.51914022995057962, 1.070387359618083956 ) ) ;
#35641 = CARTESIAN_POINT ( 'NONE',  ( -1.598336519864000049, -78.91939177743699929, -0.2292036100155999956 ) ) ;
#35642 = DIRECTION ( 'NONE',  ( -0.7071067811814418791, 1.254535583516073644E-07, -0.7071067811916420531 ) ) ;
#35643 = CARTESIAN_POINT ( 'NONE',  ( -0.8033103333046999195, -77.64572957994299429, -10.88715107357000100 ) ) ;
#35644 = B_SPLINE_SURFACE_WITH_KNOTS ( 'NONE', 3, 3, ( 
 ( #44693, #26659, #58268, #52180, #47481, #52461, #17832, #20870, #53847, #38587, #35819, #16162, #7585, #25009, #51892, #4543, #11735, #13381, #13086 ),
 ( #4246, #22245, #31380, #29713, #7296, #2872, #49422, #35519, #43606, #33854, #8972, #40256, #16450, #3166, #22546, #26957, #2591, #56318, #11450 ),
 ( #29429, #34431, #43030, #20590, #56602, #34140, #47761, #43316, #38873, #56893, #12019, #31083, #30000, #48054, #25584, #21156, #39162, #57171, #16737 ),
 ( #53547, #49120, #8671, #23417, #14553, #40846, #10430, #28414, #32544, #50593, #40557, #13971, #10144, #45289, #55004, #28120, #46171, #36408, #36120 ) ),
 .UNSPECIFIED., .F., .F., .F.,
 ( 4, 4 ),
 ( 4, 1, 1, 1, 1, 1, 1, 1, 1, 1, 1, 1, 1, 1, 1, 1, 4 ),
 ( -0.3708084972814000291, 1.370808497280999960 ),
 ( -0.009185076287115999730, 0.02066642164601000323, 0.05051791957914000125, 0.08036941751227000275, 0.1102209154453999973, 0.1400724133785000158, 0.1699239113116000066, 0.1997754092448000007, 0.2296269071778999915, 0.2594784051110000100, 0.2893299030441999764, 0.3191814009773000227, 0.3490328989103999580, 0.3788843968435000042, 0.4087358947766999706, 0.4385873927098000169, 0.4684388906429000077 ),
 .UNSPECIFIED. ) ;
#35645 = CARTESIAN_POINT ( 'NONE',  ( -10.52667135666000142, -78.33036326492899093, 6.323366929881999887 ) ) ;
#35646 = DIRECTION ( 'NONE',  ( -0.7071067811865475727, 0.000000000000000000, -0.7071067811865475727 ) ) ;
#35647 = CARTESIAN_POINT ( 'NONE',  ( -10.75000000000000000, -79.01041666666667140, -1.407171709420429018 ) ) ;
#35649 = CARTESIAN_POINT ( 'NONE',  ( 1.384987510431000102, -78.06445905126490459, 0.3030985439221999811 ) ) ;
#35648 = CARTESIAN_POINT ( 'NONE',  ( -1.500000000000000444, -79.88958333333333428, 0.1963495408493560745 ) ) ;
#35650 = CARTESIAN_POINT ( 'NONE',  ( 0.7887820451556000201, -81.54022674571000096, 1.375581554690999964 ) ) ;
#35651 = ORIENTED_EDGE ( 'NONE', *, *, #56411, .T. ) ;
#35652 = CARTESIAN_POINT ( 'NONE',  ( -2.293752191199000201, -84.67882450217399537, 2.760876382108000016 ) ) ;
#35653 = CARTESIAN_POINT ( 'NONE',  ( -9.403529956545000346, -79.07069129717299916, 7.335493971768999977 ) ) ;
#35654 = CARTESIAN_POINT ( 'NONE',  ( 6.339406590914999917, -80.46812245865710622, 9.199765193516999062 ) ) ;
#35655 = CARTESIAN_POINT ( 'NONE',  ( -8.343860018000999190, -59.94999999967000548, 8.343860018000999190 ) ) ;
#35656 = DIRECTION ( 'NONE',  ( 1.000000000000000000, 0.000000000000000000, 0.000000000000000000 ) ) ;
#35657 = CARTESIAN_POINT ( 'NONE',  ( -11.16975252231999960, -76.82659737091999830, 1.027088271520000040 ) ) ;
#35658 = CARTESIAN_POINT ( 'NONE',  ( 0.000000000000000000, -74.70999999999999375, 0.000000000000000000 ) ) ;
#35659 = DIRECTION ( 'NONE',  ( 0.000000000000000000, 1.000000000000000000, 0.000000000000000000 ) ) ;
#35660 = CARTESIAN_POINT ( 'NONE',  ( 2.161125324972999806, -0.7216593309027000691, -2.801917336448000118 ) ) ;
#35661 = CARTESIAN_POINT ( 'NONE',  ( 7.601397897754999633, -23.25000000000000000, 9.369164850722000892 ) ) ;
#35662 = DIRECTION ( 'NONE',  ( -0.7071067811865475727, 0.000000000000000000, -0.7071067811865475727 ) ) ;
#35663 = CARTESIAN_POINT ( 'NONE',  ( 0.000000000000000000, -74.70999999999999375, 0.000000000000000000 ) ) ;
#35664 = EDGE_LOOP ( 'NONE', ( #56266, #55325, #44748, #35301 ) ) ;
#35665 = CARTESIAN_POINT ( 'NONE',  ( -12.71758670595631280, -54.73493368743210397, 1.809547514116643274 ) ) ;
#35666 = CARTESIAN_POINT ( 'NONE',  ( 9.555317380607998956, -79.58626001420199714, 1.897550461403999966 ) ) ;
#35667 = AXIS2_PLACEMENT_3D ( 'NONE', #40889, #10184, #23169 ) ;
#35668 = CARTESIAN_POINT ( 'NONE',  ( 0.000000000000000000, -80.99999999999998579, -7.000000000000000000 ) ) ;
#35669 = ADVANCED_FACE ( 'NONE', ( #7656 ), #22090, .F. ) ;
#35670 = CARTESIAN_POINT ( 'NONE',  ( 1.250000000000000000, -81.74999999999998579, 0.000000000000000000 ) ) ;
#35671 = CARTESIAN_POINT ( 'NONE',  ( 1.640574411872000038, -79.65271399197999358, 0.2893137654249999802 ) ) ;
#35672 = CARTESIAN_POINT ( 'NONE',  ( 3.140974612311377090, -76.94583333333332575, -11.68767212001978528 ) ) ;
#35673 = ORIENTED_EDGE ( 'NONE', *, *, #48516, .T. ) ;
#35674 = ADVANCED_FACE ( 'NONE', ( #48976 ), #41076, .F. ) ;
#35675 = CYLINDRICAL_SURFACE ( 'NONE', #29455, 11.75000000000000000 ) ;
#35676 = CARTESIAN_POINT ( 'NONE',  ( 8.872958366224914073, -61.81010144656845995, -8.813896669730688416 ) ) ;
#35677 = FACE_OUTER_BOUND ( 'NONE', #50688, .T. ) ;
#35678 = ORIENTED_EDGE ( 'NONE', *, *, #54774, .F. ) ;
#35679 = ORIENTED_EDGE ( 'NONE', *, *, #42096, .F. ) ;
#35680 = CONICAL_SURFACE ( 'NONE', #49834, 8.899999998586000771, 0.7853981633972997312 ) ;
#35681 = CARTESIAN_POINT ( 'NONE',  ( -12.60552522438000089, -60.08917565288000162, 1.799501877759999813 ) ) ;
#35682 = CARTESIAN_POINT ( 'NONE',  ( -7.658900722992000532, -55.59059707800999917, -10.01676258972999989 ) ) ;
#35683 =( NAMED_UNIT ( * ) SI_UNIT ( $, .STERADIAN. ) SOLID_ANGLE_UNIT ( ) );
#35684 = CARTESIAN_POINT ( 'NONE',  ( -9.687172913667000174, -79.78005044541399116, -1.248753675804000096 ) ) ;
#35685 = VERTEX_POINT ( 'NONE', #34797 ) ;
#35686 = EDGE_CURVE ( 'NONE', #11409, #56919, #38868, .T. ) ;
#35687 = ORIENTED_EDGE ( 'NONE', *, *, #38456, .T. ) ;
#35688 = CARTESIAN_POINT ( 'NONE',  ( -1.918609024215000014, -76.73587854621999327, -12.08329390949000093 ) ) ;
#35689 = CARTESIAN_POINT ( 'NONE',  ( -9.768056576080892839, -78.63443854277882394, -4.490846406839354543 ) ) ;
#35690 = CARTESIAN_POINT ( 'NONE',  ( 1.466105194966000003, -78.93275043768998955, -0.4542193573542999685 ) ) ;
#35691 = ORIENTED_EDGE ( 'NONE', *, *, #8018, .T. ) ;
#35692 = CARTESIAN_POINT ( 'NONE',  ( -8.123853732960998997, -77.14685584965400267, 4.915330883505999893 ) ) ;
#35693 = CARTESIAN_POINT ( 'NONE',  ( 9.512289053070713152, -78.08404840513796330, -1.920985361971307537 ) ) ;
#35694 = CARTESIAN_POINT ( 'NONE',  ( 0.8841121778318057345, -80.28811247499398007, -0.8831609924660611677 ) ) ;
#35695 = CARTESIAN_POINT ( 'NONE',  ( 0.1861230080285300181, -77.83463541685786424, -1.415364582351019918 ) ) ;
#35696 = CARTESIAN_POINT ( 'NONE',  ( 10.79417609527999922, -77.47808473949946517, -3.050225076229999832 ) ) ;
#35697 = CARTESIAN_POINT ( 'NONE',  ( 3.930393413736140928, -86.17851879815599148, 0.4511457402659648230 ) ) ;
#35698 = CARTESIAN_POINT ( 'NONE',  ( -11.19989528650999944, -78.89730468648299677, 0.6168112860373000661 ) ) ;
#35699 = CARTESIAN_POINT ( 'NONE',  ( 5.420624143929649641, -79.92565254368837202, 7.494935276742532793 ) ) ;
#35700 = LINE ( 'NONE', #30396, #19015 ) ;
#35701 = ORIENTED_EDGE ( 'NONE', *, *, #13836, .F. ) ;
#35702 = CARTESIAN_POINT ( 'NONE',  ( 9.126884531295068825, -76.97371192633831072, -3.132086699607132374 ) ) ;
#35703 = CARTESIAN_POINT ( 'NONE',  ( 2.860640696257633842, -77.25019150838288340, -8.796429361950103498 ) ) ;
#35704 = CARTESIAN_POINT ( 'NONE',  ( -1.434155062425999994, -79.36523479771300060, -0.2237658014421000097 ) ) ;
#35705 = EDGE_CURVE ( 'NONE', #36029, #49361, #58117, .T. ) ;
#35706 = CARTESIAN_POINT ( 'NONE',  ( 0.9283799206808001081, -78.47094128391260881, 0.9373773696604000838 ) ) ;
#35707 = CARTESIAN_POINT ( 'NONE',  ( -1.083132186409117459, -2.748984415522624403, 3.413444661446231265 ) ) ;
#35708 = AXIS2_PLACEMENT_3D ( 'NONE', #27439, #5307, #5017 ) ;
#35709 = CARTESIAN_POINT ( 'NONE',  ( -9.433537730491899254, -16.87202052679777253, 8.532653828096353976 ) ) ;
#35710 = CARTESIAN_POINT ( 'NONE',  ( 7.144724566336000393, -76.52727280461898829, 9.988770583665001368 ) ) ;
#35711 = CARTESIAN_POINT ( 'NONE',  ( -1.338465391571669771, -79.07632407938210406, -0.4637712603925426835 ) ) ;
#35712 = CARTESIAN_POINT ( 'NONE',  ( 1.712298698931000063, -78.41967705768098540, 11.02540857285000087 ) ) ;
#35713 = CARTESIAN_POINT ( 'NONE',  ( -2.715334531406999652, -77.04536332859899517, -9.237819267638000653 ) ) ;
#35714 = CARTESIAN_POINT ( 'NONE',  ( -1.629306394757588539, -76.93573459678474080, 11.96328544387188941 ) ) ;
#35715 = CARTESIAN_POINT ( 'NONE',  ( -10.75000000000000000, -79.50000000000000000, 0.000000000000000000 ) ) ;
#35716 = CARTESIAN_POINT ( 'NONE',  ( 8.554126827399000987, -79.94402133281720069, -7.255689219360999864 ) ) ;
#35717 = DIRECTION ( 'NONE',  ( -1.000000000000000000, 0.000000000000000000, 0.000000000000000000 ) ) ;
#35718 = ORIENTED_EDGE ( 'NONE', *, *, #18313, .F. ) ;
#35719 = CARTESIAN_POINT ( 'NONE',  ( 0.5557217581696000108, -82.80077418747099216, 1.359272403504999893 ) ) ;
#35720 = CARTESIAN_POINT ( 'NONE',  ( 1.312293141192999890, -80.28913826020999522, 0.3222699683723999620 ) ) ;
#35721 = CARTESIAN_POINT ( 'NONE',  ( 7.674614791499999811, -56.04899163905999870, -10.14948852566000070 ) ) ;
#35722 = AXIS2_PLACEMENT_3D ( 'NONE', #25940, #8514, #4392 ) ;
#35723 = FACE_OUTER_BOUND ( 'NONE', #54734, .T. ) ;
#35724 = DIRECTION ( 'NONE',  ( -1.000000000000000000, 0.000000000000000000, 0.000000000000000000 ) ) ;
#35725 = ADVANCED_FACE ( 'NONE', ( #44250 ), #6715, .F. ) ;
#35726 = CARTESIAN_POINT ( 'NONE',  ( -11.69669687464000063, -78.56067377359198645, 2.371241166392999755 ) ) ;
#35727 = CARTESIAN_POINT ( 'NONE',  ( 8.384816012895999648, -78.71759415034600238, -4.923277454554000343 ) ) ;
#35728 = CARTESIAN_POINT ( 'NONE',  ( 0.8445585116459000119, -54.08959556723999640, -12.43380736233000050 ) ) ;
#35729 = DIRECTION ( 'NONE',  ( 0.7071067811864963915, 0.000000000000000000, -0.7071067811865987540 ) ) ;
#35730 = CARTESIAN_POINT ( 'NONE',  ( -5.250095168255000111, -80.11166617326099981, -9.571408815458999797 ) ) ;
#35731 = CARTESIAN_POINT ( 'NONE',  ( 3.677662896325250674, -85.88547955769999476, 2.671197113343194651 ) ) ;
#35732 = ORIENTED_EDGE ( 'NONE', *, *, #19663, .F. ) ;
#35733 = CARTESIAN_POINT ( 'NONE',  ( -6.954077596906954817, -78.23999999999998067, 6.533946999607151973 ) ) ;
#35734 = CARTESIAN_POINT ( 'NONE',  ( 1.996052055574059514, -78.54828564506388489, -3.456153366506571789 ) ) ;
#35735 = CARTESIAN_POINT ( 'NONE',  ( 1.611423453808999984, -81.54080102427998611, 0.4225784326546000447 ) ) ;
#35736 = CARTESIAN_POINT ( 'NONE',  ( -7.022507694776999543, -79.36040011476698908, 8.434951230355999030 ) ) ;
#35737 = DIRECTION ( 'NONE',  ( 0.000000000000000000, -0.8191989533107670862, 0.5735094374938772832 ) ) ;
#35738 = CARTESIAN_POINT ( 'NONE',  ( -11.85634656288999977, -75.99822096499200086, 1.610826861118999975 ) ) ;
#35739 = CARTESIAN_POINT ( 'NONE',  ( 0.1409072282368034335, -78.57076637647936934, 11.74721378579847020 ) ) ;
#35740 = CARTESIAN_POINT ( 'NONE',  ( -10.75000000000000000, -77.60000000000000853, 2.252154972635999871E-14 ) ) ;
#35741 = ORIENTED_EDGE ( 'NONE', *, *, #12623, .F. ) ;
#35742 = CARTESIAN_POINT ( 'NONE',  ( 11.26004178396000199, -80.02508423127190440, -0.2131731071575000136 ) ) ;
#35743 = CARTESIAN_POINT ( 'NONE',  ( 7.483407197968000801, -77.19999999999998863, -5.437013583705000208 ) ) ;
#35744 = CARTESIAN_POINT ( 'NONE',  ( 8.750272118727675519, -75.80000000000002558, -8.070589281326626008 ) ) ;
#35745 = CYLINDRICAL_SURFACE ( 'NONE', #56130, 0.5000000000000000000 ) ;
#35746 = EDGE_CURVE ( 'NONE', #29444, #1603, #24761, .T. ) ;
#35747 = CARTESIAN_POINT ( 'NONE',  ( 0.2656919276500000482, -79.36995726186898992, -11.15441650005999996 ) ) ;
#35748 = EDGE_CURVE ( 'NONE', #19884, #26170, #9415, .T. ) ;
#35749 = DIRECTION ( 'NONE',  ( 1.000000000000000000, 0.000000000000000000, 0.000000000000000000 ) ) ;
#35750 = CARTESIAN_POINT ( 'NONE',  ( 0.2396844382371944027, -81.48695566245035593, -1.494320044138283565 ) ) ;
#35751 = CARTESIAN_POINT ( 'NONE',  ( -12.22643784615999962, -77.83401841833600088, -1.144550905343000080 ) ) ;
#35752 = VECTOR ( 'NONE', #57663, 1000.000000000000000 ) ;
#35753 = CARTESIAN_POINT ( 'NONE',  ( -1.513302041220051630E-14, -80.79999999999999716, 13.90000000000000036 ) ) ;
#35754 = CARTESIAN_POINT ( 'NONE',  ( -8.596418555780466875, -79.44791666666665719, 6.606377239730298001 ) ) ;
#35755 = CARTESIAN_POINT ( 'NONE',  ( -10.75000000000000000, -78.50000000000000000, 0.000000000000000000 ) ) ;
#35756 = CARTESIAN_POINT ( 'NONE',  ( -12.66313299633999812, -25.17803434852999800, -0.06050769725596999438 ) ) ;
#35757 = EDGE_LOOP ( 'NONE', ( #33121, #45311, #15379, #58221 ) ) ;
#35758 = EDGE_CURVE ( 'NONE', #11190, #5429, #27404, .T. ) ;
#35759 = ORIENTED_EDGE ( 'NONE', *, *, #20823, .F. ) ;
#35760 = CARTESIAN_POINT ( 'NONE',  ( 10.48060664564022737, -78.83212343620286333, -2.412640484422836185 ) ) ;
#35761 = CARTESIAN_POINT ( 'NONE',  ( 4.826563570534999847, -77.46213998579800375, 8.231944463396999367 ) ) ;
#35762 = AXIS2_PLACEMENT_3D ( 'NONE', #42960, #56531, #16090 ) ;
#35763 = VERTEX_POINT ( 'NONE', #27107 ) ;
#35764 = CARTESIAN_POINT ( 'NONE',  ( 1.870325714029711817, -79.60930526082691472, 9.346613135352017210 ) ) ;
#35765 = ORIENTED_EDGE ( 'NONE', *, *, #26606, .T. ) ;
#35766 = CARTESIAN_POINT ( 'NONE',  ( 9.770427757044000572, -25.05529868456000386, 8.292768371742001321 ) ) ;
#35767 = CARTESIAN_POINT ( 'NONE',  ( -9.301504212792000459, -78.18631111317900206, -5.931589059777999218 ) ) ;
#35768 = VECTOR ( 'NONE', #12624, 1000.000000000000000 ) ;
#35769 = DIRECTION ( 'NONE',  ( 0.000000000000000000, -1.000000000000000000, -1.213843840257000049E-13 ) ) ;
#35770 = CARTESIAN_POINT ( 'NONE',  ( -0.9465222407332000154, -81.15663953506998496, -0.8164530897714000757 ) ) ;
#35771 = CARTESIAN_POINT ( 'NONE',  ( 0.000000000000000000, -74.70999999999999375, 0.000000000000000000 ) ) ;
#35772 = CARTESIAN_POINT ( 'NONE',  ( 9.376438147752001129, -79.40208394470199949, -6.156339679782000474 ) ) ;
#35773 = CARTESIAN_POINT ( 'NONE',  ( 1.147151915388343157, -79.38294062387207362, 0.4959029880282930791 ) ) ;
#35774 = ORIENTED_EDGE ( 'NONE', *, *, #5199, .T. ) ;
#35775 = VERTEX_POINT ( 'NONE', #45144 ) ;
#35776 = CARTESIAN_POINT ( 'NONE',  ( 2.773106347243120329, -77.45094825236556346, 8.824487850178316606 ) ) ;
#35777 = CARTESIAN_POINT ( 'NONE',  ( -0.5413127449341000874, -78.05124810013299452, -11.02683867434999954 ) ) ;
#35778 = CARTESIAN_POINT ( 'NONE',  ( 5.091895231007000255, -78.72149758112600182, 8.260951054388000259 ) ) ;
#35779 = CARTESIAN_POINT ( 'NONE',  ( -9.657845603713999694, -75.80025915097000677, -8.171271387442999412 ) ) ;
#35780 = CARTESIAN_POINT ( 'NONE',  ( -9.041368304669726186, -79.42452246446772790, -2.915530444129728949 ) ) ;
#35781 = CARTESIAN_POINT ( 'NONE',  ( -0.9536002873971000104, -79.13599388661999967, 1.318830682536000110 ) ) ;
#35782 = PLANE ( 'NONE',  #39350 ) ;
#35783 = CARTESIAN_POINT ( 'NONE',  ( 12.70956139859000089, -18.59498835749000278, -1.933780970936999966 ) ) ;
#35784 = CARTESIAN_POINT ( 'NONE',  ( -10.36221643468999964, -23.22123873666000193, -7.631895748949999891 ) ) ;
#35785 = CARTESIAN_POINT ( 'NONE',  ( -3.357666099452000008, -85.94560505905998582, 0.9480989593101001311 ) ) ;
#35786 = VERTEX_POINT ( 'NONE', #54861 ) ;
#35787 = CARTESIAN_POINT ( 'NONE',  ( 11.31276370261999986, -79.72349187107899127, 4.871084483227000383 ) ) ;
#35788 = CARTESIAN_POINT ( 'NONE',  ( -11.35374465838000013, -76.14602084646099911, -0.6977592397238999711 ) ) ;
#35789 = CARTESIAN_POINT ( 'NONE',  ( -5.897312117113708396, -78.02137868188400205, 8.988332804861963510 ) ) ;
#35790 = CARTESIAN_POINT ( 'NONE',  ( -11.92766985523999956, -77.70911065163099352, -1.116582401450000095 ) ) ;
#35791 = CARTESIAN_POINT ( 'NONE',  ( -3.250000000000001776, -3.489583333333332593, 0.4254240051736045136 ) ) ;
#35792 = ADVANCED_FACE ( 'NONE', ( #18278 ), #17978, .F. ) ;
#35794 = CARTESIAN_POINT ( 'NONE',  ( -0.9212224518303999687, -17.18045898161000196, -12.54670315981999984 ) ) ;
#35793 = CARTESIAN_POINT ( 'NONE',  ( 0.000000000000000000, -49.87071424677999687, 0.000000000000000000 ) ) ;
#35795 = CARTESIAN_POINT ( 'NONE',  ( 3.140027144888999810, -86.25171435493598437, -1.398030157551999997 ) ) ;
#35796 = CARTESIAN_POINT ( 'NONE',  ( 10.18589234707000202, -55.51082434643999619, -7.641012386020999969 ) ) ;
#35797 = CARTESIAN_POINT ( 'NONE',  ( 9.500000000000000000, -78.54999999999999716, 0.000000000000000000 ) ) ;
#35798 = CARTESIAN_POINT ( 'NONE',  ( 2.837175473061999575, -78.24565671216601004, 10.77984396480000129 ) ) ;
#35800 = CARTESIAN_POINT ( 'NONE',  ( 0.4254240051736071226, -1.864583333333333259, 3.250000000000001776 ) ) ;
#35799 =( BOUNDED_SURFACE ( )  B_SPLINE_SURFACE ( 3, 3, ( 
 ( #39017, #52606, #26300, #44312, #39305, #39877, #57316 ),
 ( #17157, #2730, #16307, #47624, #16588, #8297, #53174 ),
 ( #26007, #29853, #43175, #43455, #57890, #12156, #11875 ),
 ( #33998, #52035, #35144, #7147, #3584, #12724, #57029 ),
 ( #30716, #34286, #21012, #47908, #7440, #34859, #25439 ),
 ( #18628, #36619, #5042, #45497, #13891, #53764, #27459 ),
 ( #9473, #50213, #44609, #23042, #54640, #22459, #18335 ),
 ( #27164, #49928, #53461, #41057, #4164, #9763, #14176 ),
 ( #17445, #49339, #644, #22163, #31885, #32173, #27750 ),
 ( #13004, #45795, #40169, #5330, #23337, #41348, #4457 ),
 ( #31003, #35431, #49042, #8587, #26575, #357, #58183 ),
 ( #17747, #40471, #8885, #45203, #35734, #13301, #13594 ),
 ( #44904, #31293, #4750, #26880, #63, #18040, #22751 ),
 ( #36034, #54058, #49633, #31590, #9180, #40762, #36327 ),
 ( #54352, #15641, #41930, #55804, #38075, #47252, #33349 ) ),
 .UNSPECIFIED., .F., .F., .F. ) 
 B_SPLINE_SURFACE_WITH_KNOTS ( ( 4, 1, 1, 1, 1, 1, 1, 1, 1, 1, 1, 1, 4 ),
 ( 4, 3, 4 ),
 ( 0.009836358966825000175, 0.09153389967814999639, 0.1732269073519000224, 0.2549246240467999969, 0.3366128957582000258, 0.4183102327763000283, 0.5000049915179999305, 0.5816997512343000665, 0.6633971206824998967, 0.7450853986059999823, 0.8267830947368000061, 0.9084761241232000017, 0.9901736240545999657 ),
 ( 0.000000000000000000, 0.5000000000000000000, 1.000000000000000000 ),
 .UNSPECIFIED. ) 
 GEOMETRIC_REPRESENTATION_ITEM ( )  RATIONAL_B_SPLINE_SURFACE ( (
 ( 1.000000000000000000, 0.8025111667134329219, 0.8025111667134329219, 1.000000000000000000, 0.8025111667134329219, 0.8025111667134329219, 1.000000000000000000),
 ( 1.000000000000000000, 0.8025111667134329219, 0.8025111667134329219, 1.000000000000000000, 0.8025111667134329219, 0.8025111667134329219, 1.000000000000000000),
 ( 1.000000000000000000, 0.8025111667134329219, 0.8025111667134329219, 1.000000000000000000, 0.8025111667134329219, 0.8025111667134329219, 1.000000000000000000),
 ( 1.000000000000000000, 0.8025111667134329219, 0.8025111667134329219, 1.000000000000000000, 0.8025111667134329219, 0.8025111667134329219, 1.000000000000000000),
 ( 1.000000000000000000, 0.8025111667134329219, 0.8025111667134329219, 1.000000000000000000, 0.8025111667134329219, 0.8025111667134329219, 1.000000000000000000),
 ( 1.000000000000000000, 0.8025111667134329219, 0.8025111667134329219, 1.000000000000000000, 0.8025111667134329219, 0.8025111667134329219, 1.000000000000000000),
 ( 1.000000000000000000, 0.8025111667134329219, 0.8025111667134329219, 1.000000000000000000, 0.8025111667134329219, 0.8025111667134329219, 1.000000000000000000),
 ( 1.000000000000000000, 0.8025111667134329219, 0.8025111667134329219, 1.000000000000000000, 0.8025111667134329219, 0.8025111667134329219, 1.000000000000000000),
 ( 1.000000000000000000, 0.8025111667134329219, 0.8025111667134329219, 1.000000000000000000, 0.8025111667134329219, 0.8025111667134329219, 1.000000000000000000),
 ( 1.000000000000000000, 0.8025111667134329219, 0.8025111667134329219, 1.000000000000000000, 0.8025111667134329219, 0.8025111667134329219, 1.000000000000000000),
 ( 1.000000000000000000, 0.8025111667134329219, 0.8025111667134329219, 1.000000000000000000, 0.8025111667134329219, 0.8025111667134329219, 1.000000000000000000),
 ( 1.000000000000000000, 0.8025111667134329219, 0.8025111667134329219, 1.000000000000000000, 0.8025111667134329219, 0.8025111667134329219, 1.000000000000000000),
 ( 1.000000000000000000, 0.8025111667134329219, 0.8025111667134329219, 1.000000000000000000, 0.8025111667134329219, 0.8025111667134329219, 1.000000000000000000),
 ( 1.000000000000000000, 0.8025111667134329219, 0.8025111667134329219, 1.000000000000000000, 0.8025111667134329219, 0.8025111667134329219, 1.000000000000000000),
 ( 1.000000000000000000, 0.8025111667134329219, 0.8025111667134329219, 1.000000000000000000, 0.8025111667134329219, 0.8025111667134329219, 1.000000000000000000) ) ) 
 REPRESENTATION_ITEM ( '' )  SURFACE ( )  );
#35801 = CARTESIAN_POINT ( 'NONE',  ( -9.611650271896857944, -80.15833333335581301, 5.539808784079855997 ) ) ;
#35802 = VERTEX_POINT ( 'NONE', #13534 ) ;
#35803 = FACE_OUTER_BOUND ( 'NONE', #37413, .T. ) ;
#35804 = CARTESIAN_POINT ( 'NONE',  ( 1.466594960164000039, -54.71841800914999965, 12.44238958329999889 ) ) ;
#35805 = DIRECTION ( 'NONE',  ( 0.000000000000000000, 1.000000000000000000, 0.000000000000000000 ) ) ;
#35806 = CARTESIAN_POINT ( 'NONE',  ( 3.654409531031999947, -2.491077063625000143, 1.063528925157000149 ) ) ;
#35807 = CARTESIAN_POINT ( 'NONE',  ( -1.819771783575000024, -80.13035146897098571, -9.247423239423000041 ) ) ;
#35808 = CIRCLE ( 'NONE', #47150, 5.000000000000000000 ) ;
#35809 = CARTESIAN_POINT ( 'NONE',  ( 7.596835002782722057, -77.49791666666669698, -5.838193839761678383 ) ) ;
#35810 = DIRECTION ( 'NONE',  ( 0.000000000000000000, 1.000000000000000000, 0.000000000000000000 ) ) ;
#35811 = CARTESIAN_POINT ( 'NONE',  ( -0.4802748259342999870, -61.80526907249000601, 12.54896097838000024 ) ) ;
#35812 = CARTESIAN_POINT ( 'NONE',  ( 12.77297374713000089, -17.27184670111999765, 1.476174539902000094 ) ) ;
#35813 = B_SPLINE_CURVE_WITH_KNOTS ( 'NONE', 3,
 ( #16871, #12716, #8289, #26000, #22154, #26293, #4155, #40161, #58175, #15271, #19707, #10865, #24127, #42730, #37115, #46596, #1137, #32971, #27957, #42145, #1427, #28836, #19416, #56016 ),
 .UNSPECIFIED., .F., .F.,
 ( 4, 2, 2, 2, 2, 2, 2, 2, 2, 2, 2, 4 ),
 ( 0.000000000000000000, 0.1250000000000006939, 0.2500000000000013878, 0.3750000000000016653, 0.4375000000000018319, 0.5000000000000018874, 0.6250000000000022204, 0.7500000000000025535, 0.8125000000000027756, 0.8437500000000022204, 0.8750000000000017764, 1.000000000000000000 ),
 .UNSPECIFIED. ) ;
#35814 = B_SPLINE_SURFACE_WITH_KNOTS ( 'NONE', 3, 3, ( 
 ( #7240, #16969, #48563, #26103, #11968, #56547, #57692, #47710, #17248, #8390, #44127, #57118, #34088, #7532, #11683, #26386, #20534, #35235, #43848, #3676, #57412, #53268, #16108, #29944, #16684, #38532, #25245, #52125, #34952, #48282, #25820, #21390, #52983, #30239, #7821, #29660, #21678, #12533, #39683, #20814, #43264, #2819, #38821, #47998, #25531, #43549, #3114, #21105, #34666, #52695, #12249, #23141, #27266, #9571, #35832, #26676, #22257, #21962, #18721, #35533, #40571, #5142, #8987, #41148, #44707, #740, #4261 ),
 ( #58283, #49734, #39972, #26970, #36715, #54728, #44407, #22850, #40272, #53561, #53862, #32270, #45002, #17846, #4559, #14273, #50315, #27555, #9862, #36423, #3959, #49436, #13395, #13986, #50025, #31396, #22560, #57986, #164, #45599, #18139, #17543, #13100, #31983, #31096, #36135, #18433, #49133, #8685, #9277, #54151, #13693, #31688, #45303, #4854, #40862, #452, #54450, #24312, #32850, #41444, #19304, #1028, #11041, #45890, #55902, #19587, #42326, #15152, #15456, #5422, #46187, #10443, #51483, #14565, #33445, #33147 ),
 ( #51192, #24011, #42028, #19010, #1894, #10747, #6299, #50608, #46775, #37003, #1596, #1311, #28723, #55020, #32558, #19886, #29023, #47062, #37880, #27845, #23432, #10157, #37587, #50897, #28430, #5712, #28134, #55309, #23720, #41732, #37294, #14855, #46478, #6004, #55605, #31881, #31288, #17742, #10055, #18034, #18907, #36614, #40757, #9758, #50208, #23333, #36027, #31583, #27160, #14465, #640, #9469, #40163, #41343, #27743, #351, #27454, #28037, #45790, #26872, #5326, #927, #5035, #50501, #18330, #36900, #44899 ),
 ( #54913, #32456, #46082, #13588, #54636, #4452, #22453, #45492, #22156, #40467, #58177, #35730, #45199, #23037, #53758, #49924, #9176, #13295, #41053, #49333, #8878, #59, #18623, #14172, #54053, #32169, #49628, #4746, #22747, #36323, #54347, #13886, #1497, #38071, #33344, #51377, #28321, #32749, #56091, #15051, #46373, #15637, #10342, #56378, #55503, #11511, #28915, #37192, #6486, #33916, #24497, #51955, #33043, #50797, #42511, #2081, #38356, #33633, #19487, #5897, #20361, #15929, #23907, #42802, #5607, #2364, #51675 ) ),
 .UNSPECIFIED., .F., .F., .F.,
 ( 4, 4 ),
 ( 4, 1, 1, 1, 1, 1, 1, 1, 1, 1, 1, 1, 1, 1, 1, 1, 1, 1, 1, 1, 1, 1, 1, 1, 1, 1, 1, 1, 1, 1, 1, 1, 1, 1, 1, 1, 1, 1, 1, 1, 1, 1, 1, 1, 1, 1, 1, 1, 1, 1, 1, 1, 1, 1, 1, 1, 1, 1, 1, 1, 1, 1, 1, 1, 4 ),
 ( -0.1772706441294000235, 1.177270644128999955 ),
 ( -0.02000000000000000042, -0.003749999999999999861, 0.01250000000000000069, 0.02875000000000000125, 0.04499999999999999833, 0.06124999999999999889, 0.07749999999999999944, 0.09375000000000000000, 0.1100000000000000006, 0.1262500000000000011, 0.1424999999999999878, 0.1587500000000000022, 0.1749999999999999889, 0.1912500000000000033, 0.2074999999999999900, 0.2237500000000000044, 0.2399999999999999911, 0.2562499999999999778, 0.2725000000000000200, 0.2887500000000000067, 0.3049999999999999933, 0.3212499999999999800, 0.3375000000000000222, 0.3537500000000000089, 0.3699999999999999956, 0.3862499999999999822, 0.4025000000000000244, 0.4187500000000000111, 0.4349999999999999978, 0.4512499999999999845, 0.4675000000000000266, 0.4837500000000000133, 0.5000000000000000000, 0.5162499999999999867, 0.5324999999999999734, 0.5487499999999999600, 0.5649999999999999467, 0.5812500000000000444, 0.5975000000000000311, 0.6137500000000000178, 0.6300000000000000044, 0.6462499999999999911, 0.6624999999999999778, 0.6787499999999999645, 0.6949999999999999512, 0.7112500000000000488, 0.7275000000000000355, 0.7437500000000000222, 0.7600000000000000089, 0.7762499999999999956, 0.7924999999999999822, 0.8087499999999999689, 0.8249999999999999556, 0.8412500000000000533, 0.8575000000000000400, 0.8737500000000000266, 0.8900000000000000133, 0.9062500000000000000, 0.9224999999999999867, 0.9387499999999999734, 0.9549999999999999600, 0.9712499999999999467, 0.9875000000000000444, 1.003749999999999920, 1.020000000000000018 ),
 .UNSPECIFIED. ) ;
#35815 = AXIS2_PLACEMENT_3D ( 'NONE', #35603, #5209, #18498 ) ;
#35816 = CARTESIAN_POINT ( 'NONE',  ( 3.472271713658000358, -82.31344503318798900, -1.985370858487000012 ) ) ;
#35817 = DIRECTION ( 'NONE',  ( -1.000000000000000000, 0.000000000000000000, 0.000000000000000000 ) ) ;
#35818 = CARTESIAN_POINT ( 'NONE',  ( 1.083751753440150623, -76.82094722090765515, 12.16865443235956512 ) ) ;
#35819 = CARTESIAN_POINT ( 'NONE',  ( 2.521041396662000000, -79.11443781726001134, 12.22511922822000052 ) ) ;
#35820 = CARTESIAN_POINT ( 'NONE',  ( -7.664623337597000763, -77.27352982952599803, -8.093710500358000104 ) ) ;
#35821 = EDGE_CURVE ( 'NONE', #51047, #5424, #22693, .T. ) ;
#35822 = CARTESIAN_POINT ( 'NONE',  ( -0.9131908197385000259, -81.34484551072999636, -1.254418330386999791 ) ) ;
#35823 = CARTESIAN_POINT ( 'NONE',  ( -0.8405898119991999096, -79.38147671680999906, 1.162537019067000132 ) ) ;
#35824 = CARTESIAN_POINT ( 'NONE',  ( 0.5135400120715946093, -61.97868533818393644, 12.70453250103551035 ) ) ;
#35825 = CARTESIAN_POINT ( 'NONE',  ( -0.5174486800468990344, -82.65282152379752745, 1.420763823235222212 ) ) ;
#35826 = CARTESIAN_POINT ( 'NONE',  ( 0.000000000000000000, -75.00000000000000000, -7.200000000000000178 ) ) ;
#35827 = CARTESIAN_POINT ( 'NONE',  ( 2.113904672446926813, -80.24111766284364933, -10.53987543967868312 ) ) ;
#35828 = CARTESIAN_POINT ( 'NONE',  ( 10.75000000000000355, -77.23958333333331439, -1.407171709420407035 ) ) ;
#35829 = CARTESIAN_POINT ( 'NONE',  ( 10.54280189716214267, -78.62763935669978821, 3.830266094756761941 ) ) ;
#35830 = CARTESIAN_POINT ( 'NONE',  ( 1.045316320065775351, -81.80395334762980042, -0.6852794371750267066 ) ) ;
#35831 = DIRECTION ( 'NONE',  ( 0.000000000000000000, 1.000000000000000000, 0.000000000000000000 ) ) ;
#35832 = CARTESIAN_POINT ( 'NONE',  ( -5.290207344092000774, -78.73732223094400240, 9.942216594703999988 ) ) ;
#35833 = CARTESIAN_POINT ( 'NONE',  ( 7.434020715870143903, -55.28308356097522847, 8.107762507646580019 ) ) ;
#35834 = EDGE_LOOP ( 'NONE', ( #31990, #4789, #22926, #37224, #55620 ) ) ;
#35835 = EDGE_CURVE ( 'NONE', #7896, #39052, #46614, .T. ) ;
#35836 = VERTEX_POINT ( 'NONE', #19437 ) ;
#35837 = VECTOR ( 'NONE', #45409, 1000.000000000000000 ) ;
#35838 = CARTESIAN_POINT ( 'NONE',  ( -0.7186842730350999631, -81.90364959367900610, 1.445929338514000184 ) ) ;
#35839 = ADVANCED_FACE ( 'NONE', ( #24149 ), #33566, .F. ) ;
#35840 = ORIENTED_EDGE ( 'NONE', *, *, #3, .F. ) ;
#35841 = DIRECTION ( 'NONE',  ( 0.000000000000000000, -0.8191989531316805628, 0.5735094377496839924 ) ) ;
#35842 = VERTEX_POINT ( 'NONE', #31436 ) ;
#35843 = CARTESIAN_POINT ( 'NONE',  ( -1.807051837523000026, -17.69921584757000232, 12.77977401834999860 ) ) ;
#35844 = CARTESIAN_POINT ( 'NONE',  ( 7.117135278674999732, -80.17052195727752917, 8.718833803912000135 ) ) ;
#35845 = CARTESIAN_POINT ( 'NONE',  ( 0.3926218265389159190, -78.35416666666667140, 1.460959015002474715 ) ) ;
#35846 = CARTESIAN_POINT ( 'NONE',  ( 7.779872909029999839, -79.45384861441699798, 7.821464818102998429 ) ) ;
#35847 = CARTESIAN_POINT ( 'NONE',  ( -2.815216471715999980, -82.17746358424498965, -2.487151863305999910 ) ) ;
#35848 = CARTESIAN_POINT ( 'NONE',  ( -3.621422511114219311, -79.30579764322290259, 8.782465238366681248 ) ) ;
#35849 = ORIENTED_EDGE ( 'NONE', *, *, #18652, .F. ) ;
#35850 = CARTESIAN_POINT ( 'NONE',  ( -5.876696946709999203, -77.43033226363316146, -9.346046374399000101 ) ) ;
#35851 = CARTESIAN_POINT ( 'NONE',  ( 10.11803007844999946, -79.12126414830001409, -6.834701957643000370 ) ) ;
#35852 = B_SPLINE_CURVE_WITH_KNOTS ( 'NONE', 3,
 ( #44697, #13977, #31972, #40260, #31385, #35523, #13091, #4252, #58273, #45293, #54141, #35824, #9561, #27545, #53853, #45589, #49426, #5134, #26962, #44992, #4548, #22550, #13682, #40561, #154, #31679, #32551, #37577, #55301, #28419 ),
 .UNSPECIFIED., .F., .F.,
 ( 4, 2, 2, 2, 2, 2, 2, 2, 2, 2, 2, 2, 2, 2, 4 ),
 ( 0.000000000000000000, 0.1250000000000012768, 0.1875000000000003608, 0.2499999999999994449, 0.3124999999999985012, 0.3749999999999976130, 0.4999999999999957256, 0.5624999999999947820, 0.6249999999999937828, 0.6874999999999928946, 0.7499999999999920064, 0.8124999999999911182, 0.8437499999999921174, 0.8749999999999930056, 1.000000000000000000 ),
 .UNSPECIFIED. ) ;
#35853 = VERTEX_POINT ( 'NONE', #12849 ) ;
#35854 = VERTEX_POINT ( 'NONE', #9026 ) ;
#35855 = DIRECTION ( 'NONE',  ( 0.000000000000000000, 1.000000000000000000, 0.000000000000000000 ) ) ;
#35856 = DIRECTION ( 'NONE',  ( 0.000000000000000000, -1.000000000000000000, 0.000000000000000000 ) ) ;
#35857 = CARTESIAN_POINT ( 'NONE',  ( -1.930860503577499721, -60.57417505875993413, -12.72930866334836253 ) ) ;
#35858 = CIRCLE ( 'NONE', #40594, 12.57042253521000141 ) ;
#35859 = CARTESIAN_POINT ( 'NONE',  ( 1.250000000000000000, -76.50000000000000000, 0.5000000000000000000 ) ) ;
#35860 = ADVANCED_FACE ( 'NONE', ( #45637 ), #43912, .F. ) ;
#35861 = CARTESIAN_POINT ( 'NONE',  ( -4.623525823812755675, -86.12610001270961391, -0.4425863276891007225 ) ) ;
#35862 = CARTESIAN_POINT ( 'NONE',  ( 3.604156498665337161, -85.79994401664013992, 0.7643492597376573272 ) ) ;
#35863 = CARTESIAN_POINT ( 'NONE',  ( -10.42426601462999969, -77.28220295299000497, 7.425889537758000536 ) ) ;
#35864 = CARTESIAN_POINT ( 'NONE',  ( 1.233662806718999860, -80.79657642056000100, -0.5514036435800000469 ) ) ;
#35865 = CARTESIAN_POINT ( 'NONE',  ( 9.621556021936999770, -76.73787633716699474, -5.088820230768000386 ) ) ;
#35866 = CARTESIAN_POINT ( 'NONE',  ( -0.6000517156062694646, -79.18523342396193243, -1.096500065134945912 ) ) ;
#35867 = DIRECTION ( 'NONE',  ( 1.000000000000000000, 0.000000000000000000, 0.000000000000000000 ) ) ;
#35868 = CARTESIAN_POINT ( 'NONE',  ( -1.093645373922000230, -81.69646188631999451, 3.809190202271000025 ) ) ;
#35869 = CARTESIAN_POINT ( 'NONE',  ( -10.04115011118999945, -59.56486430393999854, 7.682331425190000118 ) ) ;
#35870 = CARTESIAN_POINT ( 'NONE',  ( -7.611782534905008113, -76.76874987344496049, -9.041039793178395456 ) ) ;
#35871 = CARTESIAN_POINT ( 'NONE',  ( 3.222977620591999770, -79.29100264934788811, -1.475594510407999937 ) ) ;
#35872 = EDGE_CURVE ( 'NONE', #5115, #36325, #21715, .T. ) ;
#35873 = DIRECTION ( 'NONE',  ( 0.000000000000000000, -1.000000000000000000, 0.000000000000000000 ) ) ;
#35874 = CARTESIAN_POINT ( 'NONE',  ( -6.474781754604000739, -80.41016915147990574, -9.218806710208998112 ) ) ;
#35875 = CARTESIAN_POINT ( 'NONE',  ( 0.07399134906894000441, -2.121452884883999968, 3.805339572302000040 ) ) ;
#35876 = CARTESIAN_POINT ( 'NONE',  ( 1.117654118288571752, -79.96050370699357757, -0.6128475875778812698 ) ) ;
#35877 = EDGE_CURVE ( 'NONE', #42169, #35302, #4601, .T. ) ;
#35878 = VERTEX_POINT ( 'NONE', #46226 ) ;
#35879 = FACE_OUTER_BOUND ( 'NONE', #30169, .T. ) ;
#35880 = CARTESIAN_POINT ( 'NONE',  ( -7.601397897754999633, -23.24999999688999708, -10.07627163191000008 ) ) ;
#35881 = CARTESIAN_POINT ( 'NONE',  ( 0.6224761083686999319, -81.84175699957599193, -1.179448874982999884 ) ) ;
#35882 = CARTESIAN_POINT ( 'NONE',  ( -12.77649795263000065, -16.69168567756999977, 0.06462540730615000395 ) ) ;
#35884 = CARTESIAN_POINT ( 'NONE',  ( -1.264141272797000060, -77.59992396741000675, -12.95149364859999963 ) ) ;
#35883 = B_SPLINE_CURVE_WITH_KNOTS ( 'NONE', 3,
 ( #13375, #52673, #12227, #35215, #30217, #48826, #30510, #39664, #48264, #44687, #3375, #48539, #22237, #3938, #7799, #31372, #13079, #31076 ),
 .UNSPECIFIED., .F., .F.,
 ( 4, 2, 2, 2, 2, 2, 2, 2, 4 ),
 ( 0.000000000000000000, 0.1250000000000000555, 0.2500000000000001110, 0.3750000000000001665, 0.5000000000000001110, 0.6250000000000001110, 0.7500000000000001110, 0.8750000000000000000, 1.000000000000000000 ),
 .UNSPECIFIED. ) ;
#35885 = CARTESIAN_POINT ( 'NONE',  ( 4.099012831087000208, -79.16778667140098946, -8.483720866318000375 ) ) ;
#35886 = CARTESIAN_POINT ( 'NONE',  ( 12.75763395695999947, -22.77795407709999864, -1.931043742978000077 ) ) ;
#35887 = ORIENTED_EDGE ( 'NONE', *, *, #2068, .F. ) ;
#35888 = CARTESIAN_POINT ( 'NONE',  ( 9.473958333542425336, -76.97604166667584025, -0.9915651795498008347 ) ) ;
#35889 = CARTESIAN_POINT ( 'NONE',  ( -1.276921705536999907, -82.22385602485501011, 0.2952546641816000128 ) ) ;
#35890 = CARTESIAN_POINT ( 'NONE',  ( 9.546819346760999636, -61.48527546573999558, -8.130850182902999990 ) ) ;
#35891 = AXIS2_PLACEMENT_3D ( 'NONE', #52041, #6864, #52327 ) ;
#35892 = CARTESIAN_POINT ( 'NONE',  ( 8.297164401012999235, -79.30663806985799624, 4.009864491784999707 ) ) ;
#35894 = CARTESIAN_POINT ( 'NONE',  ( -3.587712099295000012, -1.745612256652999905, 1.801380527025000067 ) ) ;
#35893 = CARTESIAN_POINT ( 'NONE',  ( 2.192371239512000525, -85.63651402127000267, 3.552905146332000275 ) ) ;
#35895 = CARTESIAN_POINT ( 'NONE',  ( -1.930989179114000143, -57.04546192861999998, -12.80896991328000034 ) ) ;
#35896 = CARTESIAN_POINT ( 'NONE',  ( 0.6128924939060999000, -79.94211185406399522, 1.278445216313999877 ) ) ;
#35897 = ORIENTED_EDGE ( 'NONE', *, *, #21984, .T. ) ;
#35898 = CARTESIAN_POINT ( 'NONE',  ( -5.075520895105466224, -77.18593687418551497, -9.477339433974600880 ) ) ;
#35899 = DIRECTION ( 'NONE',  ( 0.000000000000000000, -1.000000000000000000, -6.032211767129999953E-14 ) ) ;
#35900 = CIRCLE ( 'NONE', #33068, 0.5000000000000004441 ) ;
#35901 = ORIENTED_EDGE ( 'NONE', *, *, #32666, .F. ) ;
#35902 = EDGE_LOOP ( 'NONE', ( #18985, #14861, #29244, #32703, #27702, #54237, #16620, #18291, #37291, #24599, #38312 ) ) ;
#35903 = CARTESIAN_POINT ( 'NONE',  ( -0.7623087083147439547, -77.75000000000001421, 1.329504222413994574 ) ) ;
#35904 = FACE_OUTER_BOUND ( 'NONE', #38014, .T. ) ;
#35905 = CARTESIAN_POINT ( 'NONE',  ( 11.70000000000000107, -80.79999999999999716, 0.000000000000000000 ) ) ;
#35906 = ORIENTED_EDGE ( 'NONE', *, *, #34354, .T. ) ;
#35907 = CARTESIAN_POINT ( 'NONE',  ( 10.95272639356999989, -78.90591505001499684, 4.740592608656999829 ) ) ;
#35908 = VERTEX_POINT ( 'NONE', #10194 ) ;
#35909 = ORIENTED_EDGE ( 'NONE', *, *, #31613, .F. ) ;
#35910 = CARTESIAN_POINT ( 'NONE',  ( -10.07627163191000008, -60.04999999657000131, 7.601397897754999633 ) ) ;
#35911 = CARTESIAN_POINT ( 'NONE',  ( -1.500000000000000000, -83.24999999999998579, 0.000000000000000000 ) ) ;
#35912 = DIRECTION ( 'NONE',  ( 0.000000000000000000, 1.000000000000000000, 0.000000000000000000 ) ) ;
#35913 = ORIENTED_EDGE ( 'NONE', *, *, #18169, .T. ) ;
#35914 = DIRECTION ( 'NONE',  ( 0.000000000000000000, 1.000000000000000000, 0.000000000000000000 ) ) ;
#35915 = AXIS2_PLACEMENT_3D ( 'NONE', #29372, #6367, #55378 ) ;
#35917 = VERTEX_POINT ( 'NONE', #33481 ) ;
#35916 = B_SPLINE_CURVE_WITH_KNOTS ( 'NONE', 3,
 ( #1614, #51791, #38189, #55922, #14872, #15170 ),
 .UNSPECIFIED., .F., .F.,
 ( 4, 1, 1, 4 ),
 ( 0.000000000000000000, 0.3333333333333000081, 0.6666666666667000474, 1.000000000000000000 ),
 .UNSPECIFIED. ) ;
#35918 = CARTESIAN_POINT ( 'NONE',  ( 1.117363022987682308, -79.86030597755448923, -0.6126732938519671157 ) ) ;
#35919 = CARTESIAN_POINT ( 'NONE',  ( -2.394033331947576837, -78.77851881763733388, -3.970517693957353877 ) ) ;
#35920 = CARTESIAN_POINT ( 'NONE',  ( 1.250000000000000000, -60.04999999966999980, 12.50000000000000000 ) ) ;
#35921 = EDGE_CURVE ( 'NONE', #42976, #3055, #38249, .T. ) ;
#35922 = CARTESIAN_POINT ( 'NONE',  ( -7.626500902215000544, -18.68415522710999710, -10.35747158362999976 ) ) ;
#35923 = CARTESIAN_POINT ( 'NONE',  ( 9.209295719246959777, -79.54427083332929271, 2.475804444607904831 ) ) ;
#35924 = EDGE_CURVE ( 'NONE', #38791, #11586, #37335, .T. ) ;
#35925 = CARTESIAN_POINT ( 'NONE',  ( 10.13881649148000008, -76.50783510652000530, -5.938594122520999719 ) ) ;
#35926 = CARTESIAN_POINT ( 'NONE',  ( -11.96278216175999987, -78.14575587604012696, 0.6386762756999999624 ) ) ;
#35927 = CARTESIAN_POINT ( 'NONE',  ( 7.699327770571627205, -78.80327297366488892, -5.126656867452202171 ) ) ;
#35928 = CARTESIAN_POINT ( 'NONE',  ( -10.52693147740000157, -23.42153431750000436, 7.606024891108000396 ) ) ;
#35929 = AXIS2_PLACEMENT_3D ( 'NONE', #35384, #53411, #13257 ) ;
#35930 = DIRECTION ( 'NONE',  ( -1.000000000000000000, 0.000000000000000000, 0.000000000000000000 ) ) ;
#35931 = CARTESIAN_POINT ( 'NONE',  ( -2.386247763912000330, -80.37325264934800373, -3.425700131269000082 ) ) ;
#35932 = CARTESIAN_POINT ( 'NONE',  ( 7.661108911051000447, -77.95368667140100172, -6.051246682538999444 ) ) ;
#35933 = CARTESIAN_POINT ( 'NONE',  ( -12.79971535686000017, -18.20965922269000004, 2.019101350716999921 ) ) ;
#35934 = CARTESIAN_POINT ( 'NONE',  ( 12.85144117163000033, -21.75472017028999971, -1.980464439859999981 ) ) ;
#35935 = CARTESIAN_POINT ( 'NONE',  ( -0.005523896503821000906, -25.06963456225999920, 12.55021156880999911 ) ) ;
#35936 = CARTESIAN_POINT ( 'NONE',  ( 1.007188805101713047, -81.05645702792023144, 0.8611998455131303354 ) ) ;
#35937 = FACE_OUTER_BOUND ( 'NONE', #33104, .T. ) ;
#35938 = EDGE_CURVE ( 'NONE', #43521, #13888, #26100, .T. ) ;
#35939 = CARTESIAN_POINT ( 'NONE',  ( -3.379948544607000116, -1.337975590836000039, 2.055725249092000162 ) ) ;
#35940 = CARTESIAN_POINT ( 'NONE',  ( -8.630067035710000667, -79.68530095943377489, -4.100810385846999750 ) ) ;
#35941 = CARTESIAN_POINT ( 'NONE',  ( 0.000000000000000000, -77.04999999999999716, -9.400000000000000355 ) ) ;
#35942 = CARTESIAN_POINT ( 'NONE',  ( -0.6250699663053016497, -80.75822413643739139, 1.377587401609168705 ) ) ;
#35943 = CARTESIAN_POINT ( 'NONE',  ( 12.43646324850000084, -61.72048514535000407, -0.1256879863178999857 ) ) ;
#35944 = CARTESIAN_POINT ( 'NONE',  ( 1.079065815471999867, -78.22481505010179603, 1.201179019145000026 ) ) ;
#35945 = CARTESIAN_POINT ( 'NONE',  ( 7.714303428875997959, -26.30294702886003222, -12.53545825868000385 ) ) ;
#35946 = CARTESIAN_POINT ( 'NONE',  ( 7.007185918478000097, -77.34612980692300255, 8.371063940391000102 ) ) ;
#35947 = CARTESIAN_POINT ( 'NONE',  ( 11.82394432951000063, -78.60165641916699997, -3.315134025842000121 ) ) ;
#35948 = DIRECTION ( 'NONE',  ( 1.000000000000000000, 0.000000000000000000, 0.000000000000000000 ) ) ;
#35949 = EDGE_CURVE ( 'NONE', #34348, #17562, #23758, .T. ) ;
#35951 = CARTESIAN_POINT ( 'NONE',  ( 0.7786926255480000059, -78.02060549223070041, -1.300993539011999989 ) ) ;
#35950 = CARTESIAN_POINT ( 'NONE',  ( -13.94827576517086065, -33.10361340872000113, -0.001644113314415235816 ) ) ;
#35952 = CARTESIAN_POINT ( 'NONE',  ( -1.491081270832000039, -81.72986186469999836, 0.8224925373206000145 ) ) ;
#35953 = VERTEX_POINT ( 'NONE', #41771 ) ;
#35954 = CARTESIAN_POINT ( 'NONE',  ( -3.497041162369999956, -84.91546544543099628, 1.371883813336999935 ) ) ;
#35955 = DIRECTION ( 'NONE',  ( 0.000000000000000000, 0.000000000000000000, -1.000000000000000000 ) ) ;
#35956 = EDGE_CURVE ( 'NONE', #24318, #23895, #51230, .T. ) ;
#35957 = CARTESIAN_POINT ( 'NONE',  ( -9.263776019951999174, -80.18834097062810429, -6.245495121194999832 ) ) ;
#35958 = AXIS2_PLACEMENT_3D ( 'NONE', #13099, #45001, #40861 ) ;
#35959 = DIRECTION ( 'NONE',  ( -0.9135454518431509463, 0.000000000000000000, 0.4067366561015779980 ) ) ;
#35960 = DIRECTION ( 'NONE',  ( 1.000000000000000000, 0.000000000000000000, 0.000000000000000000 ) ) ;
#35961 = CARTESIAN_POINT ( 'NONE',  ( -6.984027423104000043, -77.26237885894900614, 8.777327129872999123 ) ) ;
#35962 = CARTESIAN_POINT ( 'NONE',  ( -12.76303204291999904, -55.53514849259999409, -1.980584515756000030 ) ) ;
#35963 = CARTESIAN_POINT ( 'NONE',  ( -1.570837462060999945, -78.71707723970298787, 9.612084340777000691 ) ) ;
#35964 = CARTESIAN_POINT ( 'NONE',  ( 0.000000000000000000, -74.64999999999999147, 0.000000000000000000 ) ) ;
#35965 = CARTESIAN_POINT ( 'NONE',  ( 9.500000000000000000, -78.06166666666669585, 1.392772743091435839 ) ) ;
#35966 = CARTESIAN_POINT ( 'NONE',  ( 12.54902678210999944, -25.00971938212000012, -0.4616712539285000028 ) ) ;
#35967 = FACE_OUTER_BOUND ( 'NONE', #27984, .T. ) ;
#35968 = ORIENTED_EDGE ( 'NONE', *, *, #29217, .F. ) ;
#35969 = CARTESIAN_POINT ( 'NONE',  ( -1.980610890453999851, -55.27926110487717182, -12.74374574604606281 ) ) ;
#35970 = DIRECTION ( 'NONE',  ( -1.000000000000000000, 0.000000000000000000, 0.000000000000000000 ) ) ;
#35971 = CARTESIAN_POINT ( 'NONE',  ( 0.000000000000000000, -77.50000000000000000, -1.749999999999931166 ) ) ;
#35972 = CARTESIAN_POINT ( 'NONE',  ( -0.6866111826235999915, -83.50967953870899407, -3.480390452359999998 ) ) ;
#35973 = CARTESIAN_POINT ( 'NONE',  ( -12.92177931905999877, -58.55736537918999574, -2.062503053667999797 ) ) ;
#35974 = ORIENTED_EDGE ( 'NONE', *, *, #15009, .T. ) ;
#35975 = DIRECTION ( 'NONE',  ( -1.000000000000000000, 0.000000000000000000, 0.000000000000000000 ) ) ;
#35976 = AXIS2_PLACEMENT_3D ( 'NONE', #13268, #40136, #8552 ) ;
#35977 = CARTESIAN_POINT ( 'NONE',  ( 10.75000000000000000, -78.85000000000000853, 0.000000000000000000 ) ) ;
#35978 = CARTESIAN_POINT ( 'NONE',  ( 3.165411199172027512, -1.229166666666666741, -0.8506806241676553304 ) ) ;
#35979 = ADVANCED_FACE ( 'NONE', ( #28760 ), #13720, .F. ) ;
#35980 = ORIENTED_EDGE ( 'NONE', *, *, #47517, .T. ) ;
#35981 = VECTOR ( 'NONE', #32921, 1000.000000000000114 ) ;
#35982 = ORIENTED_EDGE ( 'NONE', *, *, #53777, .T. ) ;
#35983 = FACE_OUTER_BOUND ( 'NONE', #27024, .T. ) ;
#35984 = CARTESIAN_POINT ( 'NONE',  ( 6.653382217586999658, -79.64551742153697944, 7.150748904218000135 ) ) ;
#35985 = ORIENTED_EDGE ( 'NONE', *, *, #48048, .F. ) ;
#35986 = CARTESIAN_POINT ( 'NONE',  ( 12.19542156202999905, -76.36703390147599180, -0.9791554825414000574 ) ) ;
#35987 = DIRECTION ( 'NONE',  ( 0.000000000000000000, 0.000000000000000000, -1.000000000000000000 ) ) ;
#35988 = CARTESIAN_POINT ( 'NONE',  ( -1.437605742302000111, -79.31065654513999164, -0.8064262874623000510 ) ) ;
#35989 = ORIENTED_EDGE ( 'NONE', *, *, #38556, .F. ) ;
#35990 = CARTESIAN_POINT ( 'NONE',  ( -9.454379850511999805, -77.56257305011499170, 0.8787206290761000460 ) ) ;
#35991 = FACE_OUTER_BOUND ( 'NONE', #13929, .T. ) ;
#35992 = CARTESIAN_POINT ( 'NONE',  ( -1.198731353186000215, -77.11209425748999990, -13.05866524906999970 ) ) ;
#35993 = CARTESIAN_POINT ( 'NONE',  ( -8.649885944100999424, -77.80492085552104697, -7.141259254888000285 ) ) ;
#35994 = B_SPLINE_CURVE_WITH_KNOTS ( 'NONE', 3,
 ( #11590, #38436, #56453, #16008, #47621, #20726, #47905, #7437, #37560, #55576, #15125, #33123, #58181, #8295, #16585, #44310, #13299, #43750, #31002, #8008, #21010 ),
 .UNSPECIFIED., .F., .F.,
 ( 4, 2, 2, 2, 2, 2, 2, 2, 2, 1, 4 ),
 ( 0.000000000000000000, 0.1249999999999998612, 0.2499999999999998335, 0.3749999999999997780, 0.4999999999999997780, 0.5624999999999997780, 0.6249999999999997780, 0.7499999999999997780, 0.8124999999999998890, 0.8749999999999998890, 1.000000000000000000 ),
 .UNSPECIFIED. ) ;
#35995 = CARTESIAN_POINT ( 'NONE',  ( -0.4994022981156016061, -86.31452042059399332, 4.016310797290853607 ) ) ;
#35996 = CARTESIAN_POINT ( 'NONE',  ( -3.907230163516999699, -77.84202411058264204, -8.882807090995999744 ) ) ;
#35997 = CARTESIAN_POINT ( 'NONE',  ( 7.620730594883017517, -79.89843349061651168, 5.254643287462647194 ) ) ;
#35998 = CARTESIAN_POINT ( 'NONE',  ( 5.407125718259508496, -80.28489556119939152, 9.703328807378895249 ) ) ;
#35999 = PRESENTATION_LAYER_ASSIGNMENT (  '', '', ( #20917 ) ) ;
#36000 = EDGE_LOOP ( 'NONE', ( #21894, #37020, #40799, #14780 ) ) ;
#36001 = CARTESIAN_POINT ( 'NONE',  ( -2.486604901413195456, -77.69583333333333997, 9.252740428348991131 ) ) ;
#36002 = CARTESIAN_POINT ( 'NONE',  ( -6.024415200221000077, -76.46769539903000634, 10.73507988388000101 ) ) ;
#36003 = CARTESIAN_POINT ( 'NONE',  ( 0.2446082660763000405, -80.54515928207800357, -1.596051606003999979 ) ) ;
#36004 = CARTESIAN_POINT ( 'NONE',  ( -1.313442439244999926, -79.16551801124799681, -0.1235842678404999867 ) ) ;
#36005 = CARTESIAN_POINT ( 'NONE',  ( -0.3992292757334167108, -3.465166414414809992, -3.497470143203500026 ) ) ;
#36006 = CARTESIAN_POINT ( 'NONE',  ( -9.164374456839587069, -16.78432317405038532, 8.803712804485032350 ) ) ;
#36007 = CARTESIAN_POINT ( 'NONE',  ( -10.51110168222999874, -76.15842815987500103, 6.351495789100000344 ) ) ;
#36008 = DIRECTION ( 'NONE',  ( -1.000000000000000000, 0.000000000000000000, 0.000000000000000000 ) ) ;
#36009 = CARTESIAN_POINT ( 'NONE',  ( -10.03539896543000154, -80.02094125464398644, 4.876675511606999969 ) ) ;
#36010 = ADVANCED_FACE ( 'NONE', ( #1347, #6337 ), #5463, .T. ) ;
#36011 = CARTESIAN_POINT ( 'NONE',  ( -8.944649069631999794, -77.41293832859899737, 3.564210769743999752 ) ) ;
#36012 = PLANE ( 'NONE',  #46118 ) ;
#36013 = CARTESIAN_POINT ( 'NONE',  ( 10.12058791103999944, -79.53547618779010975, 4.836508133599999759 ) ) ;
#36014 = CARTESIAN_POINT ( 'NONE',  ( 6.606377239730313988, -77.82291666666665719, 8.596418555780454440 ) ) ;
#36015 = ORIENTED_EDGE ( 'NONE', *, *, #14140, .T. ) ;
#36016 = CARTESIAN_POINT ( 'NONE',  ( -0.4887637738901999818, -82.35865968170000428, 1.384759226041999858 ) ) ;
#36017 = CARTESIAN_POINT ( 'NONE',  ( 1.233662806718999860, -81.23652648686000077, -0.5514036435800000469 ) ) ;
#36018 = CARTESIAN_POINT ( 'NONE',  ( 0.000000000000000000, -90.39999999999999147, -9.599999999999999645 ) ) ;
#36019 = CARTESIAN_POINT ( 'NONE',  ( 9.450487096927000508, -77.69565019976899123, -7.362360902974999455 ) ) ;
#36020 = LINE ( 'NONE', #54047, #7994 ) ;
#36021 = CARTESIAN_POINT ( 'NONE',  ( 1.579899301681999990, -82.04607474515999854, 0.5283722218587000308 ) ) ;
#36022 = CARTESIAN_POINT ( 'NONE',  ( 9.414842545117998895, -77.77392362630298805, -7.334592169791999794 ) ) ;
#36023 = CARTESIAN_POINT ( 'NONE',  ( 7.048436826466999428, -77.81756081701298911, 6.223291978577000449 ) ) ;
#36024 = CARTESIAN_POINT ( 'NONE',  ( -5.062255795481000575, -77.22345684055298420, -8.064983548927001422 ) ) ;
#36025 = CARTESIAN_POINT ( 'NONE',  ( 1.750000000000000000, -23.24999999688999708, -12.50000000000000000 ) ) ;
#36026 = CARTESIAN_POINT ( 'NONE',  ( 3.900131474043036839, -76.04750243334697757, 11.09005429771401197 ) ) ;
#36027 = CARTESIAN_POINT ( 'NONE',  ( 0.9420327262254000189, -79.09066710378499465, -10.99155624668999920 ) ) ;
#36028 = CARTESIAN_POINT ( 'NONE',  ( 1.558396630253658044, -85.88547955769999476, 3.590921352246429610 ) ) ;
#36029 = VERTEX_POINT ( 'NONE', #37625 ) ;
#36030 = CARTESIAN_POINT ( 'NONE',  ( -0.6017968039497370025, -78.18000000000000682, 9.523103445003336276 ) ) ;
#36031 = CARTESIAN_POINT ( 'NONE',  ( -7.000000000000000000, -81.10000000285099020, 0.000000000000000000 ) ) ;
#36032 = CIRCLE ( 'NONE', #12473, 2.000000000000000000 ) ;
#36033 = EDGE_CURVE ( 'NONE', #35308, #22854, #58056, .T. ) ;
#36034 = CARTESIAN_POINT ( 'NONE',  ( -3.399395987256549567, -78.67390000031814168, 0.06408526995191954345 ) ) ;
#36035 = B_SPLINE_CURVE_WITH_KNOTS ( 'NONE', 3,
 ( #33464, #42346, #47664, #50915, #34036, #24032 ),
 .UNSPECIFIED., .F., .F.,
 ( 4, 2, 4 ),
 ( 0.000000000000000000, 0.5000000000000000000, 1.000000000000000000 ),
 .UNSPECIFIED. ) ;
#36036 = CARTESIAN_POINT ( 'NONE',  ( 10.74341457190999982, -79.16375363443799529, -2.245675826504000216 ) ) ;
#36037 = CARTESIAN_POINT ( 'NONE',  ( 1.980584515756000030, -55.53514849873000259, -12.76303204337999908 ) ) ;
#36038 = CARTESIAN_POINT ( 'NONE',  ( -1.155714523305999997, -76.75577497604999166, 12.45063448816000040 ) ) ;
#36039 = DIRECTION ( 'NONE',  ( -0.7071067811865475727, 0.000000000000000000, 0.7071067811865475727 ) ) ;
#36040 = DIRECTION ( 'NONE',  ( -0.7071067811865474617, 0.000000000000000000, 0.7071067811865474617 ) ) ;
#36041 = VERTEX_POINT ( 'NONE', #19340 ) ;
#36043 = CONICAL_SURFACE ( 'NONE', #27564, 10.09999999997999964, 0.7853981633972997312 ) ;
#36042 = CARTESIAN_POINT ( 'NONE',  ( 8.679422240859999249, -78.40488561575499205, -6.994438423095999724 ) ) ;
#36044 = CARTESIAN_POINT ( 'NONE',  ( 9.249645746724414863, -77.24371006452764732, -0.7293945652191456963 ) ) ;
#36045 = CARTESIAN_POINT ( 'NONE',  ( 0.000000000000000000, -76.00000000000000000, -2.799999999999999822 ) ) ;
#36046 = CARTESIAN_POINT ( 'NONE',  ( -3.740501050291150431, -78.39678895079168797, 2.113514116493498296 ) ) ;
#36047 = CARTESIAN_POINT ( 'NONE',  ( -0.9232088357456459393, -81.54158477673213667, 0.8426130859076562674 ) ) ;
#36048 = APPLICATION_CONTEXT ( 'automotive_design' ) ;
#36049 = CARTESIAN_POINT ( 'NONE',  ( 4.711402524194999941, -78.58337134055398110, 10.11406376844000121 ) ) ;
#36050 = CARTESIAN_POINT ( 'NONE',  ( -10.75000000000000000, -76.50000000000000000, 0.000000000000000000 ) ) ;
#36051 = LINE ( 'NONE', #13613, #17654 ) ;
#36052 = ADVANCED_FACE ( 'NONE', ( #51519 ), #11078, .T. ) ;
#36053 = DIRECTION ( 'NONE',  ( 0.000000000000000000, 1.000000000000000000, 0.000000000000000000 ) ) ;
#36054 = DIRECTION ( 'NONE',  ( -0.7071067811865474617, 0.000000000000000000, 0.7071067811865474617 ) ) ;
#36055 = CARTESIAN_POINT ( 'NONE',  ( -12.71759155194429347, -60.86493881542617146, -1.809604648260207727 ) ) ;
#36056 =( NAMED_UNIT ( * ) SI_UNIT ( $, .STERADIAN. ) SOLID_ANGLE_UNIT ( ) );
#36057 = CARTESIAN_POINT ( 'NONE',  ( 10.48543666025108401, -77.09166666666666856, 6.043427764450814976 ) ) ;
#36058 = ORIENTED_EDGE ( 'NONE', *, *, #14909, .F. ) ;
#36059 = VERTEX_POINT ( 'NONE', #9901 ) ;
#36060 = DIRECTION ( 'NONE',  ( -1.000000000000000000, 0.000000000000000000, 0.000000000000000000 ) ) ;
#36061 = CARTESIAN_POINT ( 'NONE',  ( 4.959417147384999502, -77.95960665246400367, 7.893364288540000828 ) ) ;
#36062 = VECTOR ( 'NONE', #50484, 1000.000000000000000 ) ;
#36063 = ORIENTED_EDGE ( 'NONE', *, *, #44473, .T. ) ;
#36064 = CARTESIAN_POINT ( 'NONE',  ( -12.10179013622999911, -78.56494648961000848, -1.986401539992999954 ) ) ;
#36065 = ORIENTED_EDGE ( 'NONE', *, *, #36427, .T. ) ;
#36066 = CARTESIAN_POINT ( 'NONE',  ( 7.969039355681999837, -24.62377467844000023, 9.934746417635000881 ) ) ;
#36067 = CARTESIAN_POINT ( 'NONE',  ( -5.656567264032000608, -77.72329328214799204, -9.471271359694998893 ) ) ;
#36068 = CARTESIAN_POINT ( 'NONE',  ( 8.107762507645121630, -55.28308356097012677, -7.434020715871730189 ) ) ;
#36069 = CARTESIAN_POINT ( 'NONE',  ( 5.259675013629999896, -79.30162331913099649, -7.751687108632999035 ) ) ;
#36070 = CARTESIAN_POINT ( 'NONE',  ( -3.495466746200742492, -78.19430050195801130, -8.564046205178371451 ) ) ;
#36071 = AXIS2_PLACEMENT_3D ( 'NONE', #29332, #47379, #25703 ) ;
#36072 = CARTESIAN_POINT ( 'NONE',  ( 10.49311453041000064, -79.98736301501259049, -3.963918880051000126 ) ) ;
#36073 = CARTESIAN_POINT ( 'NONE',  ( -2.364683833628040688, -79.44460282387935024, 9.258118656371037147 ) ) ;
#36074 = ORIENTED_EDGE ( 'NONE', *, *, #23252, .F. ) ;
#36075 = ORIENTED_EDGE ( 'NONE', *, *, #25630, .T. ) ;
#36076 = CARTESIAN_POINT ( 'NONE',  ( -1.451214355047547366, -77.48760472878844041, 9.135408314824262632 ) ) ;
#36077 = CARTESIAN_POINT ( 'NONE',  ( 10.42639159904000046, -77.22087918317399158, -2.617796444239999687 ) ) ;
#36078 = CARTESIAN_POINT ( 'NONE',  ( 4.784380313523554307, -77.56666666666666288, -8.300970689365442468 ) ) ;
#36079 = CARTESIAN_POINT ( 'NONE',  ( 8.240135455977000589, -78.09617334028799007, -5.125512367919999868 ) ) ;
#36080 = VECTOR ( 'NONE', #9906, 1000.000000000000000 ) ;
#36081 = CARTESIAN_POINT ( 'NONE',  ( -10.01856959424999971, -76.06150170016000800, -8.476471298849000746 ) ) ;
#36082 = CARTESIAN_POINT ( 'NONE',  ( -5.397519881558073607, -79.47672766764729602, -7.818984972944852174 ) ) ;
#36083 = CARTESIAN_POINT ( 'NONE',  ( 1.153380192234999990, -78.58271294291999709, 1.148206073167999941 ) ) ;
#36084 = CARTESIAN_POINT ( 'NONE',  ( 7.710095619854000937, -20.24935285776999905, -10.18496935401000059 ) ) ;
#36085 = CONICAL_SURFACE ( 'NONE', #26624, 2.699999999213000379, 0.7853981633972997312 ) ;
#36086 = DIRECTION ( 'NONE',  ( 1.000000000000000000, 0.000000000000000000, 0.000000000000000000 ) ) ;
#36087 = EDGE_CURVE ( 'NONE', #15959, #50939, #52884, .T. ) ;
#36088 = CARTESIAN_POINT ( 'NONE',  ( -10.52682159650000138, -23.42567232067999683, -7.605689092050000433 ) ) ;
#36089 = CARTESIAN_POINT ( 'NONE',  ( 11.79999999988000070, -18.85000000520999919, 0.5999999998848000171 ) ) ;
#36090 = CARTESIAN_POINT ( 'NONE',  ( 3.589194950545000040, -85.26418603921399608, 0.03774597188233999590 ) ) ;
#36091 = VERTEX_POINT ( 'NONE', #50936 ) ;
#36092 = EDGE_CURVE ( 'NONE', #22393, #50254, #14604, .T. ) ;
#36093 = CARTESIAN_POINT ( 'NONE',  ( -6.568157394400000015, -79.86252639446888679, 9.960850882888999891 ) ) ;
#36094 = CARTESIAN_POINT ( 'NONE',  ( 0.1565658240112999811, -75.94730213011300179, 11.25550456148000045 ) ) ;
#36095 = CARTESIAN_POINT ( 'NONE',  ( -5.081867896333786661, -78.01424454617936988, 9.472916454327915403 ) ) ;
#36096 = CARTESIAN_POINT ( 'NONE',  ( 11.88382656225999945, -78.37381361479698683, -1.513515996960000054 ) ) ;
#36097 = CARTESIAN_POINT ( 'NONE',  ( -10.35398565887000011, -18.59211376270000216, 7.619387877927000119 ) ) ;
#36098 = CARTESIAN_POINT ( 'NONE',  ( -10.68107435978283526, -79.08975591983691800, 1.407249667601314203 ) ) ;
#36099 = CARTESIAN_POINT ( 'NONE',  ( -8.485281374238999419, -55.64999999967000122, -8.485281374238999419 ) ) ;
#36100 = CARTESIAN_POINT ( 'NONE',  ( 1.676866965995471581, -80.96289916692815325, 10.61818188551169762 ) ) ;
#36101 = CARTESIAN_POINT ( 'NONE',  ( -8.648182244747999903, -80.06748455509199403, 6.853707971299000334 ) ) ;
#36102 = CARTESIAN_POINT ( 'NONE',  ( -0.6878299077642000547, -82.26466602871199996, -1.043738481606000024 ) ) ;
#36103 = CARTESIAN_POINT ( 'NONE',  ( 10.27624888046999985, -78.10947499715699394, -4.318947732659999872 ) ) ;
#36104 = CARTESIAN_POINT ( 'NONE',  ( -1.997276839918484148, -1.927083333333333037, 2.598917237794077018 ) ) ;
#36105 = CARTESIAN_POINT ( 'NONE',  ( -11.11481121949999995, -80.89657200469704890, -0.7603797884353999947 ) ) ;
#36106 = ORIENTED_EDGE ( 'NONE', *, *, #39005, .T. ) ;
#36107 = CARTESIAN_POINT ( 'NONE',  ( -0.4701041210481999855, -53.79203065542999695, 12.54901038410999980 ) ) ;
#36108 = CARTESIAN_POINT ( 'NONE',  ( -1.933650113854000097, -60.20786252993000431, -12.70909635757000089 ) ) ;
#36109 = EDGE_CURVE ( 'NONE', #38390, #17250, #7113, .T. ) ;
#36110 = CARTESIAN_POINT ( 'NONE',  ( -1.682691453581999896, -2.307097686686999882, -3.413847142597000062 ) ) ;
#36111 = CARTESIAN_POINT ( 'NONE',  ( -11.16975252231999960, -76.69102026436699759, 1.027088271520000040 ) ) ;
#36112 = DIRECTION ( 'NONE',  ( -0.5721800009715952706, 0.8201280671261930166, 0.000000000000000000 ) ) ;
#36113 = AXIS2_PLACEMENT_3D ( 'NONE', #53750, #21852, #9169 ) ;
#36114 = CARTESIAN_POINT ( 'NONE',  ( 10.40641373605281572, -76.87100247242075568, 2.787300749583467852 ) ) ;
#36115 = CARTESIAN_POINT ( 'NONE',  ( 10.75000000000000000, -77.19999999999998863, -6.141891925717000695E-13 ) ) ;
#36116 = CARTESIAN_POINT ( 'NONE',  ( -1.200170490667999967, -61.23405701964999537, 12.43444080554000131 ) ) ;
#36117 = FACE_OUTER_BOUND ( 'NONE', #25791, .T. ) ;
#36118 = CARTESIAN_POINT ( 'NONE',  ( 3.637908496719999718, -85.52057450217398582, -1.955537114970999912 ) ) ;
#36119 = DIRECTION ( 'NONE',  ( 0.7071067811865474617, 0.7071067811865474617, 4.569532939869306191E-09 ) ) ;
#36120 = CARTESIAN_POINT ( 'NONE',  ( 10.98582032482000059, -79.21006532114999743, -5.054225604206000533 ) ) ;
#36121 = B_SPLINE_SURFACE_WITH_KNOTS ( 'NONE', 3, 3, ( 
 ( #36272, #5274, #872, #31830, #22990, #593, #36563, #14125, #32121, #33865, #42464, #56329, #24450, #6144, #28570, #23855, #2030, #19442, #14996, #28860, #51328, #10885, #32993, #20030, #15295, #33288, #15587, #41872, #24153, #1448, #37433, #46909, #42752, #5849, #51905 ),
 ( #51039, #1739, #47201, #38016, #55452, #24738, #33584, #29154, #6436, #56039, #51622, #11177, #6730, #2317, #10586, #42171, #20311, #15880, #11462, #38309, #46617, #19732, #37729, #50749, #55750, #10293, #28274, #46324, #23465, #23756, #55349, #54765, #41769, #32889, #19048 ),
 ( #54191, #32019, #13729, #14601, #40607, #27592, #19338, #5748, #41477, #40898, #41186, #32597, #54485, #50934, #45635, #22886, #31726, #50645, #5175, #487, #14891, #55055, #37332, #50061, #4888, #10192, #28171, #14020, #10481, #27307, #9899, #45338, #18754, #46224, #45045 ),
 ( #4598, #22597, #32302, #205, #9607, #14308, #36458, #36748, #18179, #36174, #50350, #9313, #49771, #23180, #776, #27881, #45928, #5461, #1060, #11649, #2496, #46515, #11362, #29056, #2216, #6335, #20501, #38497, #28466, #1932, #37914, #24048, #6917, #51517, #56514 ) ),
 .UNSPECIFIED., .F., .F., .F.,
 ( 4, 4 ),
 ( 4, 1, 1, 1, 1, 1, 1, 1, 1, 1, 1, 1, 1, 1, 1, 1, 1, 1, 1, 1, 1, 1, 1, 1, 1, 1, 1, 1, 1, 1, 1, 1, 4 ),
 ( -0.1566102636784000024, 1.156610263678000017 ),
 ( -0.02000000000000000042, 0.01250000000000000069, 0.04499999999999999833, 0.07749999999999999944, 0.1100000000000000006, 0.1424999999999999878, 0.1749999999999999889, 0.2074999999999999900, 0.2399999999999999911, 0.2725000000000000200, 0.3049999999999999933, 0.3375000000000000222, 0.3699999999999999956, 0.4025000000000000244, 0.4349999999999999978, 0.4675000000000000266, 0.5000000000000000000, 0.5324999999999999734, 0.5649999999999999467, 0.5975000000000000311, 0.6300000000000000044, 0.6624999999999999778, 0.6949999999999999512, 0.7275000000000000355, 0.7600000000000000089, 0.7924999999999999822, 0.8249999999999999556, 0.8575000000000000400, 0.8900000000000000133, 0.9224999999999999867, 0.9549999999999999600, 0.9875000000000000444, 1.020000000000000018 ),
 .UNSPECIFIED. ) ;
#36122 = CARTESIAN_POINT ( 'NONE',  ( -0.9550654082404999023, -78.15834718399401027, 11.22148896650999816 ) ) ;
#36123 = CARTESIAN_POINT ( 'NONE',  ( 0.7545134501129999727, -80.54877167723999776, 1.485250302772000097 ) ) ;
#36124 = CARTESIAN_POINT ( 'NONE',  ( -0.5989072293159000138, -79.04738729812999054, -1.303606512140000007 ) ) ;
#36125 = CARTESIAN_POINT ( 'NONE',  ( -0.8405563561534999950, -77.00853010409947785, -9.635375415708001157 ) ) ;
#36126 = CARTESIAN_POINT ( 'NONE',  ( -0.2578204775944251126, -83.13866164002989478, 1.488022452193133116 ) ) ;
#36127 = CARTESIAN_POINT ( 'NONE',  ( -12.49830695671999869, -60.00970582242000262, 1.666977511085999897 ) ) ;
#36128 = CARTESIAN_POINT ( 'NONE',  ( 8.318585563179999198, -78.15655403032357640, 7.159970128962999780 ) ) ;
#36129 = DIRECTION ( 'NONE',  ( 0.7071067811865475727, 0.000000000000000000, 0.7071067811865475727 ) ) ;
#36130 = DIRECTION ( 'NONE',  ( 0.6562721000522208081, -0.7545243075561237633, 7.874468564641248377E-10 ) ) ;
#36131 = AXIS2_PLACEMENT_3D ( 'NONE', #21728, #49787, #45357 ) ;
#36132 = AXIS2_PLACEMENT_3D ( 'NONE', #55075, #14622, #27326 ) ;
#36133 = CARTESIAN_POINT ( 'NONE',  ( 1.161390734570817651, -81.81998499750356757, -0.4620521855202992523 ) ) ;
#36134 = CARTESIAN_POINT ( 'NONE',  ( -0.04193593510302838501, -61.81009741308654526, 12.50649570009192679 ) ) ;
#36135 = CARTESIAN_POINT ( 'NONE',  ( -7.255688098778000139, -79.32253981239199447, 8.462245020330000145 ) ) ;
#36136 = LINE ( 'NONE', #13694, #58234 ) ;
#36137 = VERTEX_POINT ( 'NONE', #54767 ) ;
#36138 = ORIENTED_EDGE ( 'NONE', *, *, #18704, .T. ) ;
#36139 = CARTESIAN_POINT ( 'NONE',  ( -1.586818774941000099, -81.50674860663099253, -0.2986973412923999982 ) ) ;
#36140 = ORIENTED_EDGE ( 'NONE', *, *, #29545, .F. ) ;
#36141 = MANIFOLD_SOLID_BREP ( 'Stock-MAS-694-1', #27688 ) ;
#36142 = CARTESIAN_POINT ( 'NONE',  ( 9.723199427898999048, -54.32306055827000080, -7.958735709912999390 ) ) ;
#36144 = ADVANCED_FACE ( 'NONE', ( #25210 ), #23166, .F. ) ;
#36143 = ORIENTED_EDGE ( 'NONE', *, *, #45897, .T. ) ;
#36145 = CARTESIAN_POINT ( 'NONE',  ( 1.154746208549590092, -80.38136168085064526, 0.4784273033405310183 ) ) ;
#36146 = CARTESIAN_POINT ( 'NONE',  ( -12.00000000000000000, 0.000000000000000000, 0.000000000000000000 ) ) ;
#36147 = DIRECTION ( 'NONE',  ( 1.000000000000000000, 0.000000000000000000, 0.000000000000000000 ) ) ;
#36148 = CARTESIAN_POINT ( 'NONE',  ( -13.99936781018472232, -32.88214388149999934, -0.1330447863085613691 ) ) ;
#36149 = CARTESIAN_POINT ( 'NONE',  ( 3.301590358683000215, -82.54207433891198775, -1.408156201170000177 ) ) ;
#36150 = CARTESIAN_POINT ( 'NONE',  ( -9.473686928965467047, -79.39394681044888102, 0.7053954857237642040 ) ) ;
#36151 = CARTESIAN_POINT ( 'NONE',  ( -1.996894868142000012, -77.23947401164122084, 10.85801781015000067 ) ) ;
#36152 = CARTESIAN_POINT ( 'NONE',  ( 8.197900261343999517, -78.42976952347000008, -8.644410496647001452 ) ) ;
#36153 = EDGE_LOOP ( 'NONE', ( #3851, #52996, #28695 ) ) ;
#36154 = VERTEX_POINT ( 'NONE', #44093 ) ;
#36155 = FACE_OUTER_BOUND ( 'NONE', #52701, .T. ) ;
#36156 = CARTESIAN_POINT ( 'NONE',  ( -5.508096857961803927, -76.98721230508247970, -10.70907476296403971 ) ) ;
#36157 = CARTESIAN_POINT ( 'NONE',  ( -1.779623408236357784, -60.93630868993977856, -12.71471627660551285 ) ) ;
#36158 = CARTESIAN_POINT ( 'NONE',  ( -2.183112477083999803, -77.60260244285699116, 9.455407409464999802 ) ) ;
#36159 = CARTESIAN_POINT ( 'NONE',  ( 0.4681120926950248506, -86.36264283715696877, -4.447836629928476171 ) ) ;
#36160 = CARTESIAN_POINT ( 'NONE',  ( 1.895286063978128821, -85.89372256580323040, 2.922279908445652552 ) ) ;
#36161 = CARTESIAN_POINT ( 'NONE',  ( -12.75337166745000061, -76.83816582529999550, -1.077318095482000082 ) ) ;
#36162 = CARTESIAN_POINT ( 'NONE',  ( -9.533257042556000371, -78.28128649030999497, 6.958047573390000018 ) ) ;
#36163 = CIRCLE ( 'NONE', #35162, 13.89999999999999858 ) ;
#36164 = CARTESIAN_POINT ( 'NONE',  ( -7.568094764011999764, -76.39424791087300548, 7.981591190547998593 ) ) ;
#36165 = DIRECTION ( 'NONE',  ( 0.000000000000000000, 1.000000000000000000, 0.000000000000000000 ) ) ;
#36166 = ADVANCED_FACE ( 'NONE', ( #13361 ), #28352, .F. ) ;
#36167 = CARTESIAN_POINT ( 'NONE',  ( -3.703359171702000019, -80.49781712273099288, -1.828563516828999980 ) ) ;
#36168 = CARTESIAN_POINT ( 'NONE',  ( 10.70339364929999881, -81.10241592956339218, 2.537196166659999808 ) ) ;
#36169 = CARTESIAN_POINT ( 'NONE',  ( -10.21381326472999795, -56.02870851050000311, 7.668949790007999923 ) ) ;
#36170 = CARTESIAN_POINT ( 'NONE',  ( 2.956485620267946590, -2.885265340294828729, 1.348054739062900742 ) ) ;
#36171 = CARTESIAN_POINT ( 'NONE',  ( 3.440332551270000039, -82.44647163347798369, -0.2267637900948999974 ) ) ;
#36172 = TOROIDAL_SURFACE ( 'NONE', #11703, 1.250000000000000000, 0.5000000000000000000 ) ;
#36174 = CARTESIAN_POINT ( 'NONE',  ( 0.1443438050804999873, -78.13203116825889083, 1.325798245762999983 ) ) ;
#36173 = CARTESIAN_POINT ( 'NONE',  ( 5.136988255280226845, -77.24434066579330249, -10.56734161811198369 ) ) ;
#36175 = CARTESIAN_POINT ( 'NONE',  ( 0.000000000000000000, -81.19999999999998863, -7.000000000000000000 ) ) ;
#36176 = CARTESIAN_POINT ( 'NONE',  ( -10.58783149161999937, -80.92942299481059365, -3.847989116766000084 ) ) ;
#36177 = CARTESIAN_POINT ( 'NONE',  ( -3.593558748265999636, -1.814443158354000163, 0.1459214154804999997 ) ) ;
#36178 = CARTESIAN_POINT ( 'NONE',  ( -0.9505604537480174532, -80.69197842858829972, 0.8492125078390942994 ) ) ;
#36179 = VERTEX_POINT ( 'NONE', #41994 ) ;
#36180 = CARTESIAN_POINT ( 'NONE',  ( -0.1610657711387516733, -23.74946977292809080, 10.99997582743960756 ) ) ;
#36181 = DIRECTION ( 'NONE',  ( 0.000000000000000000, 0.000000000000000000, -1.000000000000000000 ) ) ;
#36182 = EDGE_CURVE ( 'NONE', #39462, #22013, #19554, .T. ) ;
#36183 = PLANE ( 'NONE',  #43468 ) ;
#36185 = ADVANCED_FACE ( 'NONE', ( #41411 ), #20348, .T. ) ;
#36184 = CARTESIAN_POINT ( 'NONE',  ( 1.667961445601999992, -58.54800977479000323, 12.58338334669999981 ) ) ;
#36186 = CARTESIAN_POINT ( 'NONE',  ( 5.579996517577999526, -77.35706742927000334, 11.75597208960999929 ) ) ;
#36187 = CARTESIAN_POINT ( 'NONE',  ( -7.792426477875908475, -61.09102098674076586, -10.18245125509822380 ) ) ;
#36188 = CARTESIAN_POINT ( 'NONE',  ( 12.49168451098999988, -23.29848884437999956, -1.667916687331000070 ) ) ;
#36189 = ORIENTED_EDGE ( 'NONE', *, *, #46191, .T. ) ;
#36190 = CARTESIAN_POINT ( 'NONE',  ( 8.666925696308020122, -53.80708316136156100, -9.019429295813042202 ) ) ;
#36191 = B_SPLINE_CURVE_WITH_KNOTS ( 'NONE', 3,
 ( #52298, #38997, #2711, #52013 ),
 .UNSPECIFIED., .F., .F.,
 ( 4, 4 ),
 ( 0.000000000000000000, 1.000000000000000000 ),
 .UNSPECIFIED. ) ;
#36192 = CARTESIAN_POINT ( 'NONE',  ( -0.4410321586598999755, -81.19765838811301251, 1.337641107945999996 ) ) ;
#36193 = CARTESIAN_POINT ( 'NONE',  ( 7.640030264156999706, -23.30716680861999990, -10.18491080493000212 ) ) ;
#36194 = CARTESIAN_POINT ( 'NONE',  ( -7.562571750566999818, -77.50890875220699172, -5.786002763631000079 ) ) ;
#36196 = CARTESIAN_POINT ( 'NONE',  ( -3.754890333716000228, -1.380863097740999912, -1.424957469106999941 ) ) ;
#36195 = CARTESIAN_POINT ( 'NONE',  ( -3.315815974107000130, -82.85917773387799912, 2.462494273907000153 ) ) ;
#36197 = CARTESIAN_POINT ( 'NONE',  ( -1.250000000000001332, -82.48958333333335702, 0.1636246173744632659 ) ) ;
#36198 = CARTESIAN_POINT ( 'NONE',  ( 0.2630806288481999933, -79.79903304826800081, -1.292808645144999824 ) ) ;
#36199 = ORIENTED_EDGE ( 'NONE', *, *, #25141, .F. ) ;
#36200 = CARTESIAN_POINT ( 'NONE',  ( 0.6835541566232417043, -77.23019398958709303, -10.73029167179032228 ) ) ;
#36201 = CARTESIAN_POINT ( 'NONE',  ( -11.75000000000000000, -78.70000000000000284, -1.701764645356999850E-14 ) ) ;
#36202 = ORIENTED_EDGE ( 'NONE', *, *, #23435, .T. ) ;
#36203 = ORIENTED_EDGE ( 'NONE', *, *, #30390, .F. ) ;
#36204 = DIRECTION ( 'NONE',  ( 1.000000000000000000, 0.000000000000000000, 0.000000000000000000 ) ) ;
#36205 = VECTOR ( 'NONE', #52897, 1000.000000000000000 ) ;
#36206 = DIRECTION ( 'NONE',  ( -0.9999896828222031298, 0.000000000000000000, -0.004542493714850020202 ) ) ;
#36207 = CARTESIAN_POINT ( 'NONE',  ( 0.000000000000000000, -75.15999999999999659, 0.000000000000000000 ) ) ;
#36208 = ORIENTED_EDGE ( 'NONE', *, *, #4331, .T. ) ;
#36209 = CARTESIAN_POINT ( 'NONE',  ( -4.725986768004000638, -78.71600984204799545, -10.95903971673999955 ) ) ;
#36210 = ORIENTED_EDGE ( 'NONE', *, *, #24530, .F. ) ;
#36212 = ADVANCED_FACE ( 'NONE', ( #994 ), #32585, .F. ) ;
#36211 = EDGE_LOOP ( 'NONE', ( #33224, #7669, #8837, #53157 ) ) ;
#36213 = FACE_OUTER_BOUND ( 'NONE', #35179, .T. ) ;
#36214 = EDGE_CURVE ( 'NONE', #31986, #20195, #9015, .T. ) ;
#36215 = CARTESIAN_POINT ( 'NONE',  ( 9.596002108778145967, -78.60208333333332575, 7.374560639699001996 ) ) ;
#36216 = DIRECTION ( 'NONE',  ( 0.000000000000000000, 1.000000000000000000, 0.000000000000000000 ) ) ;
#36217 = ORIENTED_EDGE ( 'NONE', *, *, #5405, .T. ) ;
#36218 = EDGE_LOOP ( 'NONE', ( #31317, #25528, #28426, #10760, #27135 ) ) ;
#36219 = CARTESIAN_POINT ( 'NONE',  ( 0.5768166144513863225, -79.81260153199569629, -1.136130408118528390 ) ) ;
#36220 = CARTESIAN_POINT ( 'NONE',  ( 3.999999999999815703, -78.72610001270986402, -2.360693579763180949 ) ) ;
#36221 = LINE ( 'NONE', #41236, #15175 ) ;
#36222 = CARTESIAN_POINT ( 'NONE',  ( -0.5999999999999999778, -18.84999999999999787, 10.98362417419999915 ) ) ;
#36223 = DIRECTION ( 'NONE',  ( 0.000000000000000000, -1.000000000000000000, 0.000000000000000000 ) ) ;
#36224 = CARTESIAN_POINT ( 'NONE',  ( -11.75000000000000711, -78.78958333333332575, 1.538071403319954955 ) ) ;
#36225 = AXIS2_PLACEMENT_3D ( 'NONE', #23945, #1534, #55838 ) ;
#36226 = CARTESIAN_POINT ( 'NONE',  ( 11.97742283006000363, -77.90159203722610926, 0.2395971301470839476 ) ) ;
#36227 = CARTESIAN_POINT ( 'NONE',  ( 7.705485901114815128, -78.80336997934396948, -5.117403104356717414 ) ) ;
#36228 = CARTESIAN_POINT ( 'NONE',  ( 1.000000000000000000, -81.19999999999998863, -7.000000000000000000 ) ) ;
#36229 = CARTESIAN_POINT ( 'NONE',  ( -9.008922265110777872, -77.62093321339025920, -2.421082990426596027 ) ) ;
#36230 = CARTESIAN_POINT ( 'NONE',  ( 3.075537641221509411, -76.65416666666669698, 11.44417895085272008 ) ) ;
#36231 = B_SPLINE_CURVE_WITH_KNOTS ( 'NONE', 3,
 ( #13632, #54672, #14213, #13335, #27202, #40798, #26912, #9802, #18369, #27785, #49671, #40508, #967, #32497, #9216, #45830, #49966, #27494, #36943, #8922, #23373, #5081, #31629, #23076, #41091, #682, #5366, #103, #18665, #18078 ),
 .UNSPECIFIED., .F., .F.,
 ( 4, 2, 1, 2, 2, 2, 2, 2, 2, 1, 2, 2, 2, 2, 2, 4 ),
 ( 0.000000000000000000, 0.1250000000000001665, 0.1875000000000002498, 0.2187500000000002776, 0.2500000000000003331, 0.3125000000000004996, 0.3750000000000006106, 0.4375000000000007772, 0.5000000000000008882, 0.5625000000000009992, 0.5937500000000008882, 0.6250000000000008882, 0.6875000000000006661, 0.7500000000000005551, 0.8750000000000002220, 1.000000000000000000 ),
 .UNSPECIFIED. ) ;
#36232 = AXIS2_PLACEMENT_3D ( 'NONE', #46958, #51376, #38070 ) ;
#36233 = CARTESIAN_POINT ( 'NONE',  ( -3.165774207400000151, -78.67817549782625974, -2.652657151789000078 ) ) ;
#36234 = CARTESIAN_POINT ( 'NONE',  ( 0.9451020025315389761, -76.28046875000043769, 11.98011734817885987 ) ) ;
#36235 = DIRECTION ( 'NONE',  ( 0.7071067811865475727, 0.000000000000000000, -0.7071067811865475727 ) ) ;
#36236 = CARTESIAN_POINT ( 'NONE',  ( -1.389926494651000155, -24.62381336254999908, 12.65988803923000106 ) ) ;
#36237 = CARTESIAN_POINT ( 'NONE',  ( -0.6762394706190373306, -81.66777882001223077, 1.139646768752475614 ) ) ;
#36238 = CARTESIAN_POINT ( 'NONE',  ( 2.426647618366999603E-14, -5.949999999936550488, -12.94999999994000106 ) ) ;
#36239 = CARTESIAN_POINT ( 'NONE',  ( -0.7707219435497000282, -1.772058083081000213, 3.880749451301000352 ) ) ;
#36240 = DIRECTION ( 'NONE',  ( -0.9999999930530777403, 0.000000000000000000, -0.0001178721535689973885 ) ) ;
#36241 = VECTOR ( 'NONE', #27420, 1000.000000000000114 ) ;
#36242 = EDGE_CURVE ( 'NONE', #34959, #17250, #19383, .T. ) ;
#36243 = DIRECTION ( 'NONE',  ( 0.000000000000000000, 0.000000000000000000, -1.000000000000000000 ) ) ;
#36244 = CARTESIAN_POINT ( 'NONE',  ( -0.7958789691180911952, -80.93029656945788020, -1.286331066359134745 ) ) ;
#36245 = CARTESIAN_POINT ( 'NONE',  ( 12.66313299637999989, -61.97803434819999779, 0.06050769725595000342 ) ) ;
#36246 = LINE ( 'NONE', #275, #3335 ) ;
#36247 = CARTESIAN_POINT ( 'NONE',  ( -8.096452064242996016, -19.21421830981000056, -13.15643568217000769 ) ) ;
#36248 = EDGE_CURVE ( 'NONE', #10750, #46183, #47542, .T. ) ;
#36249 = CARTESIAN_POINT ( 'NONE',  ( -10.82730428396000022, -77.53678420793599457, -1.394578048285000094 ) ) ;
#36250 = CARTESIAN_POINT ( 'NONE',  ( 10.75000000000000000, -77.19999999999998863, -6.141891925717000695E-13 ) ) ;
#36251 = LINE ( 'NONE', #54271, #31661 ) ;
#36253 = CARTESIAN_POINT ( 'NONE',  ( 0.2897255177615999933, -79.15593676564900250, 1.387848051154999762 ) ) ;
#36252 = CARTESIAN_POINT ( 'NONE',  ( 0.000000000000000000, -55.54999999966999980, 12.00000000000000000 ) ) ;
#36254 = CARTESIAN_POINT ( 'NONE',  ( 1.362316189135000188, -81.41390831549000495, -0.8114345006153000917 ) ) ;
#36255 = ORIENTED_EDGE ( 'NONE', *, *, #36357, .T. ) ;
#36256 = CARTESIAN_POINT ( 'NONE',  ( -2.900113492901999823, -86.11024735065198854, 2.038129431027000393 ) ) ;
#36257 = CARTESIAN_POINT ( 'NONE',  ( -10.90197693778999977, -79.65663117581799213, -4.835570938503999550 ) ) ;
#36258 = CARTESIAN_POINT ( 'NONE',  ( -1.599027143172000009, -80.95995837030230291, 10.93957212085000030 ) ) ;
#36259 = DIRECTION ( 'NONE',  ( 0.000000000000000000, -1.000000000000000000, 0.000000000000000000 ) ) ;
#36260 = CARTESIAN_POINT ( 'NONE',  ( 3.442912721433392775, -85.44479167442446510, -0.07965019996499557442 ) ) ;
#36261 = DIRECTION ( 'NONE',  ( 0.000000000000000000, 1.000000000000000000, 0.000000000000000000 ) ) ;
#36262 = CARTESIAN_POINT ( 'NONE',  ( -5.702118101738999911, -78.40441511928399621, -7.895919506952999711 ) ) ;
#36263 = DIRECTION ( 'NONE',  ( 3.552713678800000476E-14, -1.000000000000000000, 2.634929311776999987E-13 ) ) ;
#36264 = CARTESIAN_POINT ( 'NONE',  ( -10.07627163191000008, -23.24999999688999708, 7.601397897754999633 ) ) ;
#36265 = CARTESIAN_POINT ( 'NONE',  ( 12.66001556632000025, -24.63260856943000121, -1.381621105852999909 ) ) ;
#36266 = CARTESIAN_POINT ( 'NONE',  ( 11.00000000000000000, -78.84999999999999432, 0.000000000000000000 ) ) ;
#36267 = ORIENTED_EDGE ( 'NONE', *, *, #5783, .T. ) ;
#36268 = CARTESIAN_POINT ( 'NONE',  ( -0.5222397221871039052, -53.63701780567495092, -12.70447686579387003 ) ) ;
#36269 = CARTESIAN_POINT ( 'NONE',  ( 8.346732565571000961, -79.46528667140100310, -4.809657925418000524 ) ) ;
#36270 = ADVANCED_FACE ( 'NONE', ( #26214 ), #18458, .F. ) ;
#36271 = CARTESIAN_POINT ( 'NONE',  ( 7.653261585152177027, -75.88086419595920518, -8.963777150644636649 ) ) ;
#36272 = CARTESIAN_POINT ( 'NONE',  ( -1.159125165887999964, -77.60380812847459708, 0.4678983327651999868 ) ) ;
#36273 = AXIS2_PLACEMENT_3D ( 'NONE', #8363, #21935, #39946 ) ;
#36274 = LINE ( 'NONE', #54298, #25575 ) ;
#36275 = EDGE_LOOP ( 'NONE', ( #2038, #29881, #28336, #45734 ) ) ;
#36276 = CARTESIAN_POINT ( 'NONE',  ( 10.62615472113999893, -77.21722575893699059, -3.576548769619000367 ) ) ;
#36277 = TOROIDAL_SURFACE ( 'NONE', #27791, 1.250000000000000000, 0.5000000000000000000 ) ;
#36278 = CARTESIAN_POINT ( 'NONE',  ( 8.532660243229310382, -61.92798380502804889, -9.433531203619960337 ) ) ;
#36279 = VERTEX_POINT ( 'NONE', #26495 ) ;
#36280 = ORIENTED_EDGE ( 'NONE', *, *, #18574, .T. ) ;
#36281 = CARTESIAN_POINT ( 'NONE',  ( -8.292781013277000568, -53.74469293044000295, -9.770415148702999986 ) ) ;
#36282 = EDGE_CURVE ( 'NONE', #33149, #38390, #51471, .T. ) ;
#36283 = CIRCLE ( 'NONE', #20246, 2.500000000000000000 ) ;
#36284 = CARTESIAN_POINT ( 'NONE',  ( 5.411006671257999834, -79.09812462199599281, 8.131518144102999557 ) ) ;
#36285 = EDGE_LOOP ( 'NONE', ( #28853, #20826, #26345, #743 ) ) ;
#36286 = CARTESIAN_POINT ( 'NONE',  ( -2.015231956295000071, -76.14730429832600578, 11.93705991877000017 ) ) ;
#36287 = CARTESIAN_POINT ( 'NONE',  ( 10.10447584118665887, -24.45118490549160484, -7.864774383118550816 ) ) ;
#36288 = CARTESIAN_POINT ( 'NONE',  ( 1.354794440577000048, -78.47175142865999931, -0.9388388050506000226 ) ) ;
#36289 = ORIENTED_EDGE ( 'NONE', *, *, #39686, .T. ) ;
#36290 = CARTESIAN_POINT ( 'NONE',  ( -9.454379850511999805, -77.62267694988499045, 0.8787206290761000460 ) ) ;
#36291 = CARTESIAN_POINT ( 'NONE',  ( 0.5018392586016090506, -80.25806588323808910, -1.144748121017402198 ) ) ;
#36292 = CARTESIAN_POINT ( 'NONE',  ( 11.80688451001000061, -77.86523079875999542, 5.334804138346999736 ) ) ;
#36293 = CARTESIAN_POINT ( 'NONE',  ( 6.043427764450807871, -78.96666666666664014, -10.48543666025108934 ) ) ;
#36294 = CARTESIAN_POINT ( 'NONE',  ( 1.260641617779999946, -77.61463347755076825, 9.621927669549000584 ) ) ;
#36295 = CARTESIAN_POINT ( 'NONE',  ( 8.904755119730189961, -79.87193893653522991, 2.506716701817723436 ) ) ;
#36296 = CARTESIAN_POINT ( 'NONE',  ( 0.1182020803831417416, -79.81770832474683175, 4.050395722669112963 ) ) ;
#36297 = ORIENTED_EDGE ( 'NONE', *, *, #13935, .T. ) ;
#36298 = CYLINDRICAL_SURFACE ( 'NONE', #12620, 1.750000000000000000 ) ;
#36299 = CARTESIAN_POINT ( 'NONE',  ( -2.858407197967999913, -77.19999999999998863, -8.797272775729998884 ) ) ;
#36300 = CARTESIAN_POINT ( 'NONE',  ( -0.3384184472371999930, -79.74559824363400651, 1.477976681755000188 ) ) ;
#36301 = CARTESIAN_POINT ( 'NONE',  ( 1.423904377723752779, -61.10512805135451941, -12.50677628660343110 ) ) ;
#36302 = CARTESIAN_POINT ( 'NONE',  ( -1.552255264827246073, -3.260542986159845835, 3.161068809798809554 ) ) ;
#36303 = CARTESIAN_POINT ( 'NONE',  ( 12.75763395699000036, -19.22204592323999961, 1.931043742978000077 ) ) ;
#36304 = CARTESIAN_POINT ( 'NONE',  ( 10.82405698390000026, -79.34094587766000473, 5.765268246940999930 ) ) ;
#36305 = CARTESIAN_POINT ( 'NONE',  ( 6.725657209017000149, -77.37424939625499576, -9.843613558058999402 ) ) ;
#36306 = CARTESIAN_POINT ( 'NONE',  ( -7.229432123817375100, -80.45000000000000284, -8.035240866824315376 ) ) ;
#36307 = CARTESIAN_POINT ( 'NONE',  ( -4.857034759904000687, -77.52603832859900024, -8.313817338163000059 ) ) ;
#36308 = CARTESIAN_POINT ( 'NONE',  ( 4.589427651721361023, -77.39382578420598691, 11.10760103527476517 ) ) ;
#36309 = CARTESIAN_POINT ( 'NONE',  ( 10.42531125072000009, -55.53514854654000032, 7.624341767124000135 ) ) ;
#36310 = AXIS2_PLACEMENT_3D ( 'NONE', #29929, #6937, #31307 ) ;
#36311 = VERTEX_POINT ( 'NONE', #25637 ) ;
#36312 = CARTESIAN_POINT ( 'NONE',  ( 1.358765745638999878, -82.73761497235999229, 0.5569594143531000352 ) ) ;
#36313 = CIRCLE ( 'NONE', #28770, 30.50000000000000355 ) ;
#36314 = CYLINDRICAL_SURFACE ( 'NONE', #17384, 1.750000000000000000 ) ;
#36315 = DIRECTION ( 'NONE',  ( 0.000000000000000000, 1.000000000000000000, 0.000000000000000000 ) ) ;
#36316 = CARTESIAN_POINT ( 'NONE',  ( -1.092232985442824100, -78.95833333333330017, 0.6295237254636200097 ) ) ;
#36317 = CARTESIAN_POINT ( 'NONE',  ( 3.648104590558693072, -76.95000000000000284, -8.803297125097907738 ) ) ;
#36318 = AXIS2_PLACEMENT_3D ( 'NONE', #49845, #50427, #46298 ) ;
#36319 = CARTESIAN_POINT ( 'NONE',  ( -4.070249838183999991, -78.47928582732099301, 11.21911621747999810 ) ) ;
#36320 = CARTESIAN_POINT ( 'NONE',  ( -3.339615680726000235, -78.41274415034598633, 9.131854552393999569 ) ) ;
#36321 = CARTESIAN_POINT ( 'NONE',  ( -9.055195227533998192, -78.80082360769699790, -3.586521308946000186 ) ) ;
#36322 = CARTESIAN_POINT ( 'NONE',  ( 9.096888433124238560, -76.00412923759679984, 7.436607333932903074 ) ) ;
#36323 = CARTESIAN_POINT ( 'NONE',  ( -4.041492642110999789, -79.62141199922800183, -10.14108984350000142 ) ) ;
#36324 = CARTESIAN_POINT ( 'NONE',  ( 1.412628807274612042, -85.83735717367099483, 3.255037163431188318 ) ) ;
#36325 = VERTEX_POINT ( 'NONE', #25924 ) ;
#36326 = CARTESIAN_POINT ( 'NONE',  ( 9.754023262367997660, -76.24778881791411322, -7.509630405475999915 ) ) ;
#36327 = CARTESIAN_POINT ( 'NONE',  ( 3.400000000000109157, -78.67390000031814168, -1.233279971202261294E-15 ) ) ;
#36328 = CARTESIAN_POINT ( 'NONE',  ( -10.44304457033000055, -78.40526006745598409, 3.377400876517000050 ) ) ;
#36329 = DIRECTION ( 'NONE',  ( 0.000000000000000000, 1.000000000000000000, 0.000000000000000000 ) ) ;
#36330 = CARTESIAN_POINT ( 'NONE',  ( -1.570796326794937636, -77.78541666666664867, 11.99999999999999467 ) ) ;
#36331 = DIRECTION ( 'NONE',  ( 0.000000000000000000, -1.000000000000000000, 0.000000000000000000 ) ) ;
#36332 = DIRECTION ( 'NONE',  ( 0.000000000000000000, 0.000000000000000000, -1.000000000000000000 ) ) ;
#36333 = ORIENTED_EDGE ( 'NONE', *, *, #20105, .F. ) ;
#36334 = CARTESIAN_POINT ( 'NONE',  ( -0.2277317800897999955, -78.33225536775100295, -10.99999347944999961 ) ) ;
#36335 = CARTESIAN_POINT ( 'NONE',  ( 12.70556836319933858, -53.57227722548668680, 0.2598513551479147976 ) ) ;
#36336 = CARTESIAN_POINT ( 'NONE',  ( -9.393203674808288994, -79.95833333333331439, 5.413904038987134015 ) ) ;
#36337 = CARTESIAN_POINT ( 'NONE',  ( -2.127490618600312633, -78.43735717367052018, 3.528455733208861300 ) ) ;
#36338 = ADVANCED_FACE ( 'NONE', ( #22375 ), #4070, .F. ) ;
#36339 = CARTESIAN_POINT ( 'NONE',  ( 11.29148473951573450, -76.42758390997302342, -3.256410895415154716 ) ) ;
#36340 = CARTESIAN_POINT ( 'NONE',  ( 3.325053339351000226, -78.95626297899599422, -10.53669369097999997 ) ) ;
#36341 = CARTESIAN_POINT ( 'NONE',  ( 12.05000000000000071, -74.80000000000001137, 0.000000000000000000 ) ) ;
#36342 = CARTESIAN_POINT ( 'NONE',  ( 1.395804191767038516, -81.56793092504486253, -0.5836528581437869789 ) ) ;
#36343 = CARTESIAN_POINT ( 'NONE',  ( 1.460959015002474048, -81.22916666666668561, -0.3926218265389178064 ) ) ;
#36344 = CARTESIAN_POINT ( 'NONE',  ( 2.421167930323313566, -79.85416666666665719, 9.009247259181924150 ) ) ;
#36345 = CARTESIAN_POINT ( 'NONE',  ( 5.155010784763280896, -79.53646688885500282, 9.790528303537312738 ) ) ;
#36346 = EDGE_CURVE ( 'NONE', #15231, #23858, #30919, .T. ) ;
#36347 = AXIS2_PLACEMENT_3D ( 'NONE', #50647, #36750, #24050 ) ;
#36348 = PLANE ( 'NONE',  #4511 ) ;
#36349 = EDGE_LOOP ( 'NONE', ( #30852, #12256, #53410, #48565 ) ) ;
#36350 = ORIENTED_EDGE ( 'NONE', *, *, #2605, .T. ) ;
#36351 = CARTESIAN_POINT ( 'NONE',  ( 4.784380313523554307, -78.56666666666666288, -8.300970689365442468 ) ) ;
#36352 = CARTESIAN_POINT ( 'NONE',  ( -1.407199056997702646, -77.71460739497811687, -10.68073707906693848 ) ) ;
#36353 = ORIENTED_EDGE ( 'NONE', *, *, #35001, .T. ) ;
#36354 = CARTESIAN_POINT ( 'NONE',  ( 10.91276041655392959, -80.28723958337666033, -1.427624777354248975 ) ) ;
#36355 = CARTESIAN_POINT ( 'NONE',  ( 8.870414880995999951, -25.06963060262999932, 8.878264461096000204 ) ) ;
#36356 = CARTESIAN_POINT ( 'NONE',  ( 0.5327216036087999429, -76.70229421267099212, -10.90374125898999935 ) ) ;
#36357 = EDGE_CURVE ( 'NONE', #36570, #32986, #49561, .T. ) ;
#36358 = DIRECTION ( 'NONE',  ( 0.000000000000000000, 1.000000000000000000, 0.000000000000000000 ) ) ;
#36359 = CARTESIAN_POINT ( 'NONE',  ( -5.580112777935000601, -78.05318998579799938, 7.918523194479999638 ) ) ;
#36360 = CARTESIAN_POINT ( 'NONE',  ( -5.840324968496969582, -78.17066989859858950, -7.173046464363928010 ) ) ;
#36361 = CARTESIAN_POINT ( 'NONE',  ( 10.54265532893000135, -78.54383683591599663, 3.830212845596999927 ) ) ;
#36362 = CARTESIAN_POINT ( 'NONE',  ( 5.645589344077617255, -79.37440282387937884, 7.709202350186582287 ) ) ;
#36363 = EDGE_CURVE ( 'NONE', #55676, #16697, #35055, .T. ) ;
#36364 = ORIENTED_EDGE ( 'NONE', *, *, #30558, .T. ) ;
#36365 = CARTESIAN_POINT ( 'NONE',  ( -7.764217752274555018, -24.25600304964931198, 10.21028588416213800 ) ) ;
#36366 = ORIENTED_EDGE ( 'NONE', *, *, #37862, .T. ) ;
#36367 = CARTESIAN_POINT ( 'NONE',  ( 2.115181327729357630, -77.45675243142653699, 9.004852716841607929 ) ) ;
#36368 = CARTESIAN_POINT ( 'NONE',  ( 10.65102452230999930, -77.70134130481397960, 2.905137941168000282 ) ) ;
#36369 = CYLINDRICAL_SURFACE ( 'NONE', #23441, 1.750000000000001332 ) ;
#36370 = CARTESIAN_POINT ( 'NONE',  ( -9.022250383429000209, -78.92046438502799788, -3.573472734901999903 ) ) ;
#36371 = CARTESIAN_POINT ( 'NONE',  ( -9.702684712557999802, -76.47625438773999917, -8.600453018952999074 ) ) ;
#36372 = CARTESIAN_POINT ( 'NONE',  ( -11.68767212001978706, -78.42083333333333428, -3.140974612311364655 ) ) ;
#36373 = CARTESIAN_POINT ( 'NONE',  ( 0.1742577344548000007, -77.63612625665999190, 1.489843697164999980 ) ) ;
#36374 = DIRECTION ( 'NONE',  ( 1.000000000000000000, 0.000000000000000000, 0.000000000000000000 ) ) ;
#36375 = CARTESIAN_POINT ( 'NONE',  ( -6.898009915208000109, -79.49989681241999051, -8.491482529321999095 ) ) ;
#36376 = CARTESIAN_POINT ( 'NONE',  ( -9.963467980702999327, -23.68274967071999981, -7.659239661648999942 ) ) ;
#36377 = CARTESIAN_POINT ( 'NONE',  ( 12.64502302236999931, -59.57129148919000272, -1.799490220168999954 ) ) ;
#36378 = CARTESIAN_POINT ( 'NONE',  ( 1.091356032651999985, -83.46042981021199125, -3.419457127327000023 ) ) ;
#36379 = ORIENTED_EDGE ( 'NONE', *, *, #3326, .F. ) ;
#36380 = CARTESIAN_POINT ( 'NONE',  ( 7.541040361361999622, -78.82956348204299957, 9.261319756036000328 ) ) ;
#36381 = CARTESIAN_POINT ( 'NONE',  ( 1.566004458289000034, -76.34473956280800166, -11.38667055607000123 ) ) ;
#36382 = CARTESIAN_POINT ( 'NONE',  ( -5.117374279120588731, -78.01454871243346645, 9.453798672375675949 ) ) ;
#36383 = CARTESIAN_POINT ( 'NONE',  ( -8.148905501844000199, -78.69936539988199797, -8.781309899900000104 ) ) ;
#36384 = EDGE_CURVE ( 'NONE', #50394, #34384, #46531, .T. ) ;
#36385 = CARTESIAN_POINT ( 'NONE',  ( 0.000000000000000000, 4.040000000000000036, 0.000000000000000000 ) ) ;
#36386 = CARTESIAN_POINT ( 'NONE',  ( -0.7999999999999001243, -18.84999999997999964, -12.00000000000000000 ) ) ;
#36387 = DIRECTION ( 'NONE',  ( -1.147001872821000084E-14, 0.000000000000000000, 1.000000000000000000 ) ) ;
#36388 = CARTESIAN_POINT ( 'NONE',  ( 6.897442179429761566, -80.91971616786906907, 8.256491842899244205 ) ) ;
#36389 = CARTESIAN_POINT ( 'NONE',  ( 10.35747145894000099, -60.11584731951999316, -7.626500777253000685 ) ) ;
#36390 = B_SPLINE_CURVE_WITH_KNOTS ( 'NONE', 3,
 ( #43911, #21462, #16462, #25309, #26178, #7597 ),
 .UNSPECIFIED., .F., .F.,
 ( 4, 1, 1, 4 ),
 ( 0.000000000000000000, 0.3333333333333000081, 0.6666666666667000474, 1.000000000000000000 ),
 .UNSPECIFIED. ) ;
#36391 = CARTESIAN_POINT ( 'NONE',  ( -6.760416188461989329, -85.88547955770000897, -5.559977880783894655 ) ) ;
#36392 = CARTESIAN_POINT ( 'NONE',  ( 8.230685248253001518, -78.08223865415499176, -7.517341346183999740 ) ) ;
#36393 = CARTESIAN_POINT ( 'NONE',  ( -12.50000000000000000, -55.54999999966999980, 0.000000000000000000 ) ) ;
#36394 = ORIENTED_EDGE ( 'NONE', *, *, #47117, .F. ) ;
#36395 = CARTESIAN_POINT ( 'NONE',  ( 10.13881649148000008, -76.90783510652001098, -5.938594122520999719 ) ) ;
#36396 = CARTESIAN_POINT ( 'NONE',  ( 8.256620083228000340, -77.35889903538301837, -4.688888258373000717 ) ) ;
#36397 = DIRECTION ( 'NONE',  ( -0.7071067811865475727, 0.000000000000000000, -0.7071067811865475727 ) ) ;
#36398 = B_SPLINE_CURVE_WITH_KNOTS ( 'NONE', 3,
 ( #15050, #56090, #37778, #33343, #33042, #51674, #2363, #18404, #51089, #10638, #54423, #15636, #24205, #20360, #46665, #13959, #15928, #47544 ),
 .UNSPECIFIED., .F., .F.,
 ( 4, 2, 2, 2, 2, 2, 2, 2, 4 ),
 ( 0.000000000000000000, 0.1250000000000000833, 0.2500000000000001665, 0.3750000000000002220, 0.5000000000000002220, 0.6250000000000002220, 0.7500000000000001110, 0.8750000000000001110, 1.000000000000000000 ),
 .UNSPECIFIED. ) ;
#36399 = CARTESIAN_POINT ( 'NONE',  ( 10.29113596735999892, -77.48087421142000153, 4.462133020506000136 ) ) ;
#36400 = CARTESIAN_POINT ( 'NONE',  ( 11.00000000000000000, -79.94999999999998863, 0.000000000000000000 ) ) ;
#36401 = CARTESIAN_POINT ( 'NONE',  ( -1.243547092045951041, -77.41458333333332575, -9.500000000000000000 ) ) ;
#36402 = CARTESIAN_POINT ( 'NONE',  ( 3.912590402935000267, -82.39999999999999147, -0.8316467632710000668 ) ) ;
#36403 = CARTESIAN_POINT ( 'NONE',  ( -7.102903299382814062, -78.56775757425661766, -8.111946779019795883 ) ) ;
#36404 = CARTESIAN_POINT ( 'NONE',  ( 12.54673279573000144, -17.17202488779000191, 0.9078290272347999679 ) ) ;
#36405 = AXIS2_PLACEMENT_3D ( 'NONE', #571, #22073, #22677 ) ;
#36406 = CARTESIAN_POINT ( 'NONE',  ( 3.805232393909999900, -82.34726287204199480, -1.402232436220000045 ) ) ;
#36407 = CARTESIAN_POINT ( 'NONE',  ( -11.75000000038751580, -76.05000000000001137, 1.230457119308518754 ) ) ;
#36408 = CARTESIAN_POINT ( 'NONE',  ( 9.906487715838999009, -79.19307150910000814, -7.400253471101999381 ) ) ;
#36409 = VECTOR ( 'NONE', #44164, 1000.000000000000000 ) ;
#36410 = CARTESIAN_POINT ( 'NONE',  ( -8.764875654205999567, -77.72256569596500242, 7.071839882566000490 ) ) ;
#36411 = CARTESIAN_POINT ( 'NONE',  ( 1.640574411872000038, -79.47506502036999620, 0.2893137654249999802 ) ) ;
#36412 = CARTESIAN_POINT ( 'NONE',  ( 0.3991026885628000120, -79.54088630715999386, -1.370848940981999942 ) ) ;
#36413 = CARTESIAN_POINT ( 'NONE',  ( 5.491552160713999875, -77.21740503984499071, 7.961786551375001686 ) ) ;
#36414 = DIRECTION ( 'NONE',  ( 0.9999999924279686647, 0.000000000000000000, 0.0001230612157835738363 ) ) ;
#36415 = CARTESIAN_POINT ( 'NONE',  ( -12.65989858210999941, -61.74344101100000159, 0.9743214026256999949 ) ) ;
#36416 = CARTESIAN_POINT ( 'NONE',  ( -5.755176823513999729, -78.26892344765445841, 9.345691860246999383 ) ) ;
#36417 = CARTESIAN_POINT ( 'NONE',  ( 12.60354432325999952, -19.24899162885999715, -1.750000000000000000 ) ) ;
#36418 = CARTESIAN_POINT ( 'NONE',  ( -0.5949767217100950800, -78.06343852817556694, 1.127525434812421512 ) ) ;
#36419 = EDGE_LOOP ( 'NONE', ( #48802, #50271, #17628, #35232, #813, #7098 ) ) ;
#36420 = CARTESIAN_POINT ( 'NONE',  ( 0.8175227547224469538, -81.78223890415932829, -0.9484037626542538568 ) ) ;
#36421 = ADVANCED_FACE ( 'NONE', ( #35348 ), #44827, .F. ) ;
#36422 = FACE_OUTER_BOUND ( 'NONE', #25402, .T. ) ;
#36423 = CARTESIAN_POINT ( 'NONE',  ( 1.092964466808999946, -79.75832130042100232, 11.09324250366999998 ) ) ;
#36424 = CARTESIAN_POINT ( 'NONE',  ( 7.892048199458332469, -55.05053022673563135, 7.664266801482971125 ) ) ;
#36425 = VERTEX_POINT ( 'NONE', #26791 ) ;
#36426 = VERTEX_POINT ( 'NONE', #7637 ) ;
#36427 = EDGE_CURVE ( 'NONE', #51686, #53803, #4374, .T. ) ;
#36428 = CARTESIAN_POINT ( 'NONE',  ( 1.142015885854000157, -81.80442434691700271, 1.141496088348999960 ) ) ;
#36429 = VERTEX_POINT ( 'NONE', #58394 ) ;
#36430 = ORIENTED_EDGE ( 'NONE', *, *, #45794, .T. ) ;
#36431 = CARTESIAN_POINT ( 'NONE',  ( -1.667260628941999778, -18.79057987526000062, 12.49858003894999925 ) ) ;
#36432 = LINE ( 'NONE', #53570, #4649 ) ;
#36433 = CARTESIAN_POINT ( 'NONE',  ( -3.250112804463431093, -80.28020832436914134, -1.140199822464329715 ) ) ;
#36434 = CARTESIAN_POINT ( 'NONE',  ( 3.455307648225000250, -82.65846528216999900, -1.473717924758000120 ) ) ;
#36435 = CARTESIAN_POINT ( 'NONE',  ( 9.722718241315000398, -55.54999999966999980, -7.954951288349001004 ) ) ;
#36437 = EDGE_CURVE ( 'NONE', #36505, #15394, #9989, .T. ) ;
#36436 = CARTESIAN_POINT ( 'NONE',  ( -11.91126960539999935, -78.74591742231000069, -0.2303430570443000258 ) ) ;
#36438 = EDGE_LOOP ( 'NONE', ( #20994, #26243, #40037, #53317 ) ) ;
#36439 = EDGE_LOOP ( 'NONE', ( #44204, #29190, #2884, #18287, #35150, #2974 ) ) ;
#36440 = CARTESIAN_POINT ( 'NONE',  ( -12.52582254647393611, -18.19059700816967151, -1.680974932933145816 ) ) ;
#36441 = AXIS2_PLACEMENT_3D ( 'NONE', #33605, #16483, #20621 ) ;
#36442 = CARTESIAN_POINT ( 'NONE',  ( -0.2340539085346999837, -80.11092564237000602, 1.312933706406000267 ) ) ;
#36443 = CARTESIAN_POINT ( 'NONE',  ( -5.159044788988000008, -77.28994032243799950, -8.219183903844999861 ) ) ;
#36444 = CARTESIAN_POINT ( 'NONE',  ( -1.661313768260326951, -86.12610001270964233, -3.638686103992151200 ) ) ;
#36445 = CARTESIAN_POINT ( 'NONE',  ( 3.520322167287936566, -85.82207524133897891, 1.464606465184206563 ) ) ;
#36446 = CIRCLE ( 'NONE', #37414, 10.50000000000000000 ) ;
#36447 = CARTESIAN_POINT ( 'NONE',  ( -12.91626791057999846, -77.42478844368000068, -1.016208772393999871 ) ) ;
#36448 = CARTESIAN_POINT ( 'NONE',  ( -0.6213570041975999825, -80.73357467910000196, -1.330550119908999962 ) ) ;
#36449 = CARTESIAN_POINT ( 'NONE',  ( -12.82904091339000097, -23.32452529362999982, -2.062673488738000049 ) ) ;
#36450 = AXIS2_PLACEMENT_3D ( 'NONE', #13433, #35873, #27308 ) ;
#36451 = DIRECTION ( 'NONE',  ( 0.000000000000000000, 0.000000000000000000, 1.000000000000000000 ) ) ;
#36452 = CARTESIAN_POINT ( 'NONE',  ( 2.777313436393999968, -81.20774294257799397, 3.117072386135000261 ) ) ;
#36453 = CONICAL_SURFACE ( 'NONE', #10089, 0.6999999997695000031, 0.7853981633972997312 ) ;
#36454 = CARTESIAN_POINT ( 'NONE',  ( -9.421357847594000745, -80.24449435892378801, -6.176342950743000770 ) ) ;
#36455 = CARTESIAN_POINT ( 'NONE',  ( 5.320338141332999982, -79.17917000473400435, -7.841092173349999861 ) ) ;
#36456 = CARTESIAN_POINT ( 'NONE',  ( -11.06835501100700014, -78.27189007101333118, 4.078077733570931507 ) ) ;
#36457 = CARTESIAN_POINT ( 'NONE',  ( -0.9790058809313999522, -81.41057046129098751, 3.409706750568999745 ) ) ;
#36458 = CARTESIAN_POINT ( 'NONE',  ( 1.224162466603000210, -77.98319329811559442, -0.5291525010897000225 ) ) ;
#36459 = DIRECTION ( 'NONE',  ( -4.762546956201999894E-11, -1.000000000000000000, -4.762495317921000031E-11 ) ) ;
#36460 = CARTESIAN_POINT ( 'NONE',  ( 5.620590082324000036, -80.50046220949079157, -9.763102121971000358 ) ) ;
#36461 = CARTESIAN_POINT ( 'NONE',  ( 3.594201416108000036, -3.094009561889999649, 1.252117639952999850 ) ) ;
#36462 = CARTESIAN_POINT ( 'NONE',  ( 8.503076353544873456, -77.20000000000000284, -6.721226585468835779 ) ) ;
#36463 = ORIENTED_EDGE ( 'NONE', *, *, #46258, .F. ) ;
#36464 = CYLINDRICAL_SURFACE ( 'NONE', #4637, 14.00000000000000000 ) ;
#36465 = CARTESIAN_POINT ( 'NONE',  ( 8.190859204290999784, -59.94999999967000548, -7.342331066867000544 ) ) ;
#36466 = CARTESIAN_POINT ( 'NONE',  ( 10.71369944335147828, -79.42916666666667425, -2.879226727952064913 ) ) ;
#36467 = CARTESIAN_POINT ( 'NONE',  ( -1.310615285706999922, -81.78046716459000720, -0.2467057407436999972 ) ) ;
#36468 = CARTESIAN_POINT ( 'NONE',  ( 8.655581700850000004, -79.61727500578398065, 4.491190667650000634 ) ) ;
#36469 = CARTESIAN_POINT ( 'NONE',  ( -1.189541931187000134, -77.10038219874999754, -12.95855809378999979 ) ) ;
#36470 = CARTESIAN_POINT ( 'NONE',  ( -4.687291826975000575, -79.51105952742696559, 9.674546195918276581 ) ) ;
#36471 = EDGE_CURVE ( 'NONE', #24242, #21820, #26898, .T. ) ;
#36472 = CARTESIAN_POINT ( 'NONE',  ( -9.519228660049000368, -79.57086001420199750, -0.02392464561790000332 ) ) ;
#36473 = CARTESIAN_POINT ( 'NONE',  ( 10.31003757212999972, -76.29231484251999973, 7.089603455708999746 ) ) ;
#36474 = VERTEX_POINT ( 'NONE', #17073 ) ;
#36475 = CARTESIAN_POINT ( 'NONE',  ( 0.000000000000000000, -13.07071424677999971, 0.000000000000000000 ) ) ;
#36476 = CARTESIAN_POINT ( 'NONE',  ( 9.825879204080999685, -77.53244226292098062, 5.302575144543999919 ) ) ;
#36477 = CARTESIAN_POINT ( 'NONE',  ( -0.8817537164447001308, -80.86848511544799578, -1.098257200506999931 ) ) ;
#36478 = CARTESIAN_POINT ( 'NONE',  ( 7.682344222570999470, -22.76462890193000277, -10.04116292115999975 ) ) ;
#36479 = CARTESIAN_POINT ( 'NONE',  ( 8.981578277711999903, -78.79500914553598534, 2.818234580162000125 ) ) ;
#36481 = CARTESIAN_POINT ( 'NONE',  ( -3.161392481395000065, -1.817959338694000060, -1.501864700490999960 ) ) ;
#36480 = CARTESIAN_POINT ( 'NONE',  ( -3.364564966397000312, -84.79476111440199304, -2.471702357780000359 ) ) ;
#36482 = DIRECTION ( 'NONE',  ( 0.000000000000000000, 1.000000000000000000, 0.000000000000000000 ) ) ;
#36483 = CARTESIAN_POINT ( 'NONE',  ( 1.309314855877999895, -79.89825829503000421, -0.1620500492231000123 ) ) ;
#36484 = VERTEX_POINT ( 'NONE', #57229 ) ;
#36485 = CARTESIAN_POINT ( 'NONE',  ( -4.332804415639630591, -77.19199523647633043, -9.839746177953021089 ) ) ;
#36486 = CARTESIAN_POINT ( 'NONE',  ( -1.500000000000000000, -78.89999999999999147, 0.000000000000000000 ) ) ;
#36487 = FACE_OUTER_BOUND ( 'NONE', #43054, .T. ) ;
#36488 = ORIENTED_EDGE ( 'NONE', *, *, #19466, .T. ) ;
#36489 = AXIS2_PLACEMENT_3D ( 'NONE', #28100, #23398, #46150 ) ;
#36490 = ORIENTED_EDGE ( 'NONE', *, *, #14, .F. ) ;
#36491 = CARTESIAN_POINT ( 'NONE',  ( -1.398183675150702632, -77.75000000000000000, 0.6275176927634855684 ) ) ;
#36492 = CARTESIAN_POINT ( 'NONE',  ( 1.249999993052000047, -76.30000000069199473, 0.6999999993075000093 ) ) ;
#36493 = DIRECTION ( 'NONE',  ( -1.000000000000000000, 0.000000000000000000, 0.000000000000000000 ) ) ;
#36494 = VECTOR ( 'NONE', #50115, 1000.000000000000114 ) ;
#36495 = ORIENTED_EDGE ( 'NONE', *, *, #28273, .T. ) ;
#36496 = EDGE_CURVE ( 'NONE', #6364, #9689, #44403, .T. ) ;
#36497 = CARTESIAN_POINT ( 'NONE',  ( 11.88272347344000046, -77.45440045069699408, 1.999161996513999950 ) ) ;
#36498 = VECTOR ( 'NONE', #5629, 1000.000000000000114 ) ;
#36499 = VERTEX_POINT ( 'NONE', #55132 ) ;
#36500 = EDGE_LOOP ( 'NONE', ( #3184, #8006, #48349, #51854, #20451 ) ) ;
#36501 = CARTESIAN_POINT ( 'NONE',  ( -0.8304832018632568591, -2.705794687591313252, -3.142888880824831421 ) ) ;
#36502 = B_SPLINE_CURVE_WITH_KNOTS ( 'NONE', 3,
 ( #29128, #11726, #42442, #2009, #43019, #20859, #37990, #25286, #16439, #42728 ),
 .UNSPECIFIED., .F., .F.,
 ( 4, 2, 2, 2, 4 ),
 ( 0.000000000000000000, 0.2500000000000000000, 0.5000000000000000000, 0.7500000000000000000, 1.000000000000000000 ),
 .UNSPECIFIED. ) ;
#36503 = CARTESIAN_POINT ( 'NONE',  ( 6.043427764450761686, -78.63333333333329733, 10.48543666025110888 ) ) ;
#36504 = CARTESIAN_POINT ( 'NONE',  ( -10.75000000000000000, -80.09999999999999432, -1.711887504597999906E-14 ) ) ;
#36505 = VERTEX_POINT ( 'NONE', #49850 ) ;
#36507 = ADVANCED_FACE ( 'NONE', ( #41268 ), #36830, .F. ) ;
#36506 = CARTESIAN_POINT ( 'NONE',  ( 1.018183232918382863, -82.80095525923850630, -0.7285541732893786593 ) ) ;
#36508 = ORIENTED_EDGE ( 'NONE', *, *, #51824, .T. ) ;
#36509 = CARTESIAN_POINT ( 'NONE',  ( 0.7895151306900345389, -79.97161635052492556, 1.000479881221597367 ) ) ;
#36510 = CARTESIAN_POINT ( 'NONE',  ( 3.962812355710999768, -78.85171438276198330, -2.338746421483398841 ) ) ;
#36511 = DIRECTION ( 'NONE',  ( 0.000000000000000000, 1.000000000000000000, 1.813364273554000256E-14 ) ) ;
#36512 = CARTESIAN_POINT ( 'NONE',  ( 11.09875712452000052, -75.95812795482899560, 1.375294608629999971 ) ) ;
#36513 = DIRECTION ( 'NONE',  ( -3.497202527557000183E-12, 1.000000000000000000, -1.787423860910000090E-11 ) ) ;
#36514 = DIRECTION ( 'NONE',  ( 0.000000000000000000, 1.000000000000000000, 0.000000000000000000 ) ) ;
#36515 = CARTESIAN_POINT ( 'NONE',  ( 0.4844284812283000119, -77.52178162129314387, 11.97002061315000176 ) ) ;
#36516 = CARTESIAN_POINT ( 'NONE',  ( 0.008117082130627714665, -78.72521557527629454, -9.249909508878625175 ) ) ;
#36517 = CARTESIAN_POINT ( 'NONE',  ( 7.508184180775703709, -77.03326573943833466, -8.333593418791714669 ) ) ;
#36518 = CARTESIAN_POINT ( 'NONE',  ( 4.242467933327000118, -77.84428667140100799, 8.300509423296000833 ) ) ;
#36519 = CARTESIAN_POINT ( 'NONE',  ( -13.86363636363000218, -9.638971321655001034, -1.277887488715999925E-05 ) ) ;
#36520 = CARTESIAN_POINT ( 'NONE',  ( -0.9565643533716999825, -80.07299023059400156, 0.9292797142584000580 ) ) ;
#36521 = CARTESIAN_POINT ( 'NONE',  ( 9.190623734250525700, -77.83975365453363793, -1.210915399504562950 ) ) ;
#36522 = DIRECTION ( 'NONE',  ( 1.000000000000000000, 0.000000000000000000, 0.000000000000000000 ) ) ;
#36523 = AXIS2_PLACEMENT_3D ( 'NONE', #39480, #58067, #48355 ) ;
#36524 = CARTESIAN_POINT ( 'NONE',  ( 3.737144282028000308, -80.72628455456799657, 1.318989544820000193 ) ) ;
#36525 = CARTESIAN_POINT ( 'NONE',  ( -4.371390937481000272, -77.78071332859899201, -8.606055931584998930 ) ) ;
#36526 = CARTESIAN_POINT ( 'NONE',  ( -12.44209697062000153, -17.91557297456000342, 1.464771213333999844 ) ) ;
#36527 = DIRECTION ( 'NONE',  ( 0.4045837979902123238, 0.8201365135193228184, 0.4045837979902123238 ) ) ;
#36528 = CARTESIAN_POINT ( 'NONE',  ( 1.477284502223000118, -24.72631500296999718, 12.77254812468999923 ) ) ;
#36529 = CARTESIAN_POINT ( 'NONE',  ( 6.916454804249409172, -79.99999999999998579, 6.378165265317452537 ) ) ;
#36530 = CARTESIAN_POINT ( 'NONE',  ( -3.335732572513999905, -0.7444651668207999951, 2.419625153821000296 ) ) ;
#36531 = CARTESIAN_POINT ( 'NONE',  ( -10.65320897811829859, -78.11245643503170299, -1.664319544042534904 ) ) ;
#36532 = AXIS2_PLACEMENT_3D ( 'NONE', #12744, #377, #4187 ) ;
#36533 = CARTESIAN_POINT ( 'NONE',  ( 12.72923908218245082, -23.77554307155166313, -1.930512971245056386 ) ) ;
#36534 = CARTESIAN_POINT ( 'NONE',  ( 0.1656092252224484473, -79.71566763053364468, 1.502111356206679460 ) ) ;
#36535 = CARTESIAN_POINT ( 'NONE',  ( -0.01915452949074002847, -78.47644932240093851, 1.249713897098126747 ) ) ;
#36536 = CARTESIAN_POINT ( 'NONE',  ( 11.00000000000000000, -78.34999999999999432, 0.000000000000000000 ) ) ;
#36537 = VECTOR ( 'NONE', #44586, 1000.000000000000114 ) ;
#36538 = LINE ( 'NONE', #28834, #42763 ) ;
#36539 = CARTESIAN_POINT ( 'NONE',  ( 0.3271848554491016414, -80.64583333333330017, -1.217465845835393967 ) ) ;
#36540 = ADVANCED_FACE ( 'NONE', ( #279 ), #44869, .F. ) ;
#36541 = CARTESIAN_POINT ( 'NONE',  ( 12.10970598371999962, -77.13667338628398795, 2.037349774713999917 ) ) ;
#36542 = CARTESIAN_POINT ( 'NONE',  ( 7.624341766639000539, -23.26485146254000114, 10.42531125024000005 ) ) ;
#36543 = AXIS2_PLACEMENT_3D ( 'NONE', #5847, #13831, #32120 ) ;
#36545 = CARTESIAN_POINT ( 'NONE',  ( -1.376714249866999973, -78.31828123251710849, 0.6352952275891999845 ) ) ;
#36544 = CARTESIAN_POINT ( 'NONE',  ( 0.000000000000000000, -46.09579702914000165, 0.000000000000000000 ) ) ;
#36546 = CARTESIAN_POINT ( 'NONE',  ( 0.6959559787155999988, -82.04550046658999918, 1.424795421937999906 ) ) ;
#36547 = VERTEX_POINT ( 'NONE', #27672 ) ;
#36548 = EDGE_CURVE ( 'NONE', #12329, #52300, #36251, .T. ) ;
#36549 = CARTESIAN_POINT ( 'NONE',  ( -1.507852503906999875, -85.15982450217398991, -3.257317659296999679 ) ) ;
#36550 = CARTESIAN_POINT ( 'NONE',  ( -9.893264523052000214, -80.61023151026600431, -4.935169213743999528 ) ) ;
#36551 = FACE_OUTER_BOUND ( 'NONE', #47856, .T. ) ;
#36552 = PLANE ( 'NONE',  #11360 ) ;
#36553 = CARTESIAN_POINT ( 'NONE',  ( 3.895497176768000003, -77.18066982994299963, 10.51870773133999926 ) ) ;
#36554 = CARTESIAN_POINT ( 'NONE',  ( 12.66232176271000043, -53.66513311386999874, -0.5079086068997000769 ) ) ;
#36555 = DIRECTION ( 'NONE',  ( 1.000000000000000000, 0.000000000000000000, 0.000000000000000000 ) ) ;
#36556 = CARTESIAN_POINT ( 'NONE',  ( 3.849498977080000106, -0.9616681123999000214, -0.3332954958730999784 ) ) ;
#36557 = CARTESIAN_POINT ( 'NONE',  ( 4.222580443737000699, -79.11071469600697981, 8.944559048890999620 ) ) ;
#36558 = CARTESIAN_POINT ( 'NONE',  ( 10.29636973964252356, -81.00000000000000000, -3.915276559953854818 ) ) ;
#36559 = EDGE_LOOP ( 'NONE', ( #49951, #5222, #25465 ) ) ;
#36560 = CARTESIAN_POINT ( 'NONE',  ( 1.042635221160942649, -80.68436150525303674, -1.121867648172004017 ) ) ;
#36561 = CARTESIAN_POINT ( 'NONE',  ( -9.392797912344001077, -79.62373998579799661, 0.6620803225204999753 ) ) ;
#36562 = CARTESIAN_POINT ( 'NONE',  ( 6.159268256616873494, -75.86834440890064002, -10.04771440447366615 ) ) ;
#36563 = CARTESIAN_POINT ( 'NONE',  ( 1.224162466603000210, -77.85187124537999637, -0.5291525010897000225 ) ) ;
#36564 = CARTESIAN_POINT ( 'NONE',  ( -12.71658889739000031, -55.48415522678000400, -1.931087888049999979 ) ) ;
#36565 = CARTESIAN_POINT ( 'NONE',  ( -9.312500000004000356, -79.68749999999599254, 6.570867420027000168E-10 ) ) ;
#36566 = EDGE_LOOP ( 'NONE', ( #9250, #52265, #32433, #8768, #38764 ) ) ;
#36567 = ADVANCED_FACE ( 'NONE', ( #19126 ), #13806, .T. ) ;
#36568 = CARTESIAN_POINT ( 'NONE',  ( -4.763107053801999946, -77.14659090128088792, -9.977925823576001108 ) ) ;
#36569 = CARTESIAN_POINT ( 'NONE',  ( -1.799475295154000065, -20.24916621771999914, 12.69619287815999975 ) ) ;
#36570 = VERTEX_POINT ( 'NONE', #41851 ) ;
#36571 = LINE ( 'NONE', #46333, #26370 ) ;
#36572 = CARTESIAN_POINT ( 'NONE',  ( -0.5483576180056000116, -79.51098439765999615, -9.751923335751000010 ) ) ;
#36573 = ORIENTED_EDGE ( 'NONE', *, *, #37483, .T. ) ;
#36575 = EDGE_CURVE ( 'NONE', #50457, #32275, #1139, .T. ) ;
#36574 = CARTESIAN_POINT ( 'NONE',  ( 0.03238307785349000406, -75.99818925673099557, 11.70563754594999750 ) ) ;
#36576 = CARTESIAN_POINT ( 'NONE',  ( 7.635939347796300680, -23.77525282322134359, -10.36595956260444673 ) ) ;
#36577 = CARTESIAN_POINT ( 'NONE',  ( 0.9462631019772999030, -78.94363555667999321, -1.349619363059000099 ) ) ;
#36578 = EDGE_CURVE ( 'NONE', #23569, #1101, #49601, .T. ) ;
#36579 = ORIENTED_EDGE ( 'NONE', *, *, #12177, .T. ) ;
#36580 = CARTESIAN_POINT ( 'NONE',  ( -4.802567994450000377, -77.15274805011500803, -8.191018798270000900 ) ) ;
#36581 = AXIS2_PLACEMENT_3D ( 'NONE', #48185, #7431, #24860 ) ;
#36582 = CARTESIAN_POINT ( 'NONE',  ( -0.8830740761637451142, -80.16309161040983611, -0.8842243533770794972 ) ) ;
#36583 = CARTESIAN_POINT ( 'NONE',  ( 5.555615362064000529, -77.42119367106998595, 11.70460571637999969 ) ) ;
#36584 = CARTESIAN_POINT ( 'NONE',  ( -3.778552491321000240, -78.40681307243859521, -1.659736609915999906E-10 ) ) ;
#36585 = CARTESIAN_POINT ( 'NONE',  ( 9.244022517729193922, -79.85467752281239484, 0.4841345082002578848 ) ) ;
#36586 = B_SPLINE_CURVE_WITH_KNOTS ( 'NONE', 3,
 ( #10803, #37060, #55078, #32910 ),
 .UNSPECIFIED., .F., .F.,
 ( 4, 4 ),
 ( 0.000000000000000000, 1.000000000000000000 ),
 .UNSPECIFIED. ) ;
#36587 = CARTESIAN_POINT ( 'NONE',  ( 0.1757403804742654341, -79.08541664991678033, -4.009081873298199206 ) ) ;
#36588 = EDGE_LOOP ( 'NONE', ( #16693, #15649, #13034 ) ) ;
#36589 = CARTESIAN_POINT ( 'NONE',  ( 7.685661446562000343, -76.94999999999998863, -5.583959896778000420 ) ) ;
#36590 = CARTESIAN_POINT ( 'NONE',  ( -3.438348731682000281, -76.58513991147000866, -11.82003900998999946 ) ) ;
#36591 = CARTESIAN_POINT ( 'NONE',  ( -1.273775855157000203, -79.39830987996700173, -0.8223283506838999779 ) ) ;
#36592 = CARTESIAN_POINT ( 'NONE',  ( 1.942972292769964193, -2.177744011644287436, 2.933851992493632821 ) ) ;
#36593 = EDGE_CURVE ( 'NONE', #52871, #51923, #52421, .T. ) ;
#36594 = CARTESIAN_POINT ( 'NONE',  ( 7.758897894450000443, -61.10081253415999925, -10.31443085085999911 ) ) ;
#36595 = CARTESIAN_POINT ( 'NONE',  ( 11.93255069029000026, -79.24879777483999987, -2.830763026309000008 ) ) ;
#36596 = DIRECTION ( 'NONE',  ( 0.000000000000000000, 1.000000000000000000, 0.000000000000000000 ) ) ;
#36597 = CARTESIAN_POINT ( 'NONE',  ( 12.70556836347999941, -16.77227722772000007, -1.774194455291999869E-09 ) ) ;
#36598 = CARTESIAN_POINT ( 'NONE',  ( 7.864930754364000798, -77.17951498579800784, 5.740674767402000001 ) ) ;
#36599 = DIRECTION ( 'NONE',  ( 0.000000000000000000, 1.000000000000000000, 0.000000000000000000 ) ) ;
#36600 = CARTESIAN_POINT ( 'NONE',  ( -10.16130211225899771, -76.39871602286838481, 8.152202769023755735 ) ) ;
#36601 = B_SPLINE_SURFACE_WITH_KNOTS ( 'NONE', 3, 3, ( 
 ( #51566, #14938, #28806, #2261 ),
 ( #1980, #50979, #52138, #10531 ),
 ( #5795, #28213, #28513, #20262 ),
 ( #38253, #42990, #46271, #41816 ),
 ( #1391, #19672, #19386, #46563 ),
 ( #6087, #1682, #19975, #37672 ),
 ( #55690, #37960, #55987, #16700 ),
 ( #49371, #40206, #52711, #12263 ) ),
 .UNSPECIFIED., .F., .F., .F.,
 ( 4, 1, 1, 1, 1, 4 ),
 ( 4, 4 ),
 ( -0.01200407345745999922, 0.000000000000000000, 0.3333333333333000081, 0.6666666666667000474, 1.000000000000000000, 1.011997855551999947 ),
 ( -0.3559705542741999906, 1.355970554273999928 ),
 .UNSPECIFIED. ) ;
#36602 = ORIENTED_EDGE ( 'NONE', *, *, #7583, .F. ) ;
#36603 = CARTESIAN_POINT ( 'NONE',  ( -1.436129866501999919, -82.35850220804000799, 0.6722556991877999266 ) ) ;
#36604 = CARTESIAN_POINT ( 'NONE',  ( 1.149971879181999945, -80.22597904509999012, -0.7096026395132000175 ) ) ;
#36605 = CARTESIAN_POINT ( 'NONE',  ( 0.000000000000000000, -75.15999999999999659, 0.000000000000000000 ) ) ;
#36606 = CARTESIAN_POINT ( 'NONE',  ( -11.92766985523999956, -77.50574499180299881, -1.116582401450000095 ) ) ;
#36607 = CARTESIAN_POINT ( 'NONE',  ( -0.6747260877994001316, -82.22962677363800310, -1.052256958371999840 ) ) ;
#36608 = EDGE_CURVE ( 'NONE', #40639, #15436, #54843, .T. ) ;
#36609 = CARTESIAN_POINT ( 'NONE',  ( 1.571434226476000173, -82.99346297181298837, -0.5530452149683998675 ) ) ;
#36610 = CARTESIAN_POINT ( 'NONE',  ( -11.88268207399999987, -77.58401841833600088, -1.112370969927999997 ) ) ;
#36611 = CARTESIAN_POINT ( 'NONE',  ( -1.553298277364999924, -78.59482872126899622, 9.504760619105999453 ) ) ;
#36612 = AXIS2_PLACEMENT_3D ( 'NONE', #32537, #1573, #50583 ) ;
#36613 = CARTESIAN_POINT ( 'NONE',  ( 4.556417092236462629, -76.04278103528405097, 10.83029532527294414 ) ) ;
#36614 = CARTESIAN_POINT ( 'NONE',  ( 10.75129243007999946, -79.22684881879399654, 2.472133787718999720 ) ) ;
#36615 = CARTESIAN_POINT ( 'NONE',  ( -2.557474545126054100, -85.79678895079199208, 3.452189813555863740 ) ) ;
#36616 = ORIENTED_EDGE ( 'NONE', *, *, #34756, .T. ) ;
#36617 = EDGE_CURVE ( 'NONE', #52202, #19448, #45901, .T. ) ;
#36618 = CARTESIAN_POINT ( 'NONE',  ( 3.295079792876998592, -76.40343702272410553, 11.86077433336000020 ) ) ;
#36619 = CARTESIAN_POINT ( 'NONE',  ( -3.893811372584298880, -78.43735716284257364, -2.200139326159465281 ) ) ;
#36621 = CARTESIAN_POINT ( 'NONE',  ( -5.157220473068041322, -76.28856089857794132, -10.55843506099110485 ) ) ;
#36620 = CARTESIAN_POINT ( 'NONE',  ( 2.813789756862229652, -77.35416666666665719, 10.47020627418440064 ) ) ;
#36622 = CARTESIAN_POINT ( 'NONE',  ( -0.6514878906251000412, -79.87018070975999251, 10.95625855609000077 ) ) ;
#36623 = FACE_BOUND ( 'NONE', #8758, .T. ) ;
#36624 = CARTESIAN_POINT ( 'NONE',  ( 4.744332214898999034, -76.52937854621998781, -11.56915240781999898 ) ) ;
#36625 = CARTESIAN_POINT ( 'NONE',  ( 9.500000000000000000, -79.14999999999999147, 0.000000000000000000 ) ) ;
#36626 = CARTESIAN_POINT ( 'NONE',  ( 9.643342484277001248, -17.05965044154000054, -8.260141428683001052 ) ) ;
#36627 = CARTESIAN_POINT ( 'NONE',  ( 1.247385803315000041, -61.27722255996999934, 12.50301438880000049 ) ) ;
#36628 = ORIENTED_EDGE ( 'NONE', *, *, #38818, .F. ) ;
#36629 = CARTESIAN_POINT ( 'NONE',  ( 10.47694508628999976, -78.48659464476099856, 3.806339902057000124 ) ) ;
#36630 = LINE ( 'NONE', #1225, #32364 ) ;
#36631 = CARTESIAN_POINT ( 'NONE',  ( -10.47020627418440242, -79.97916666666665719, 2.813789756862221214 ) ) ;
#36632 = CARTESIAN_POINT ( 'NONE',  ( -3.587190963684412370, -78.43735717367052018, 2.026888547381852312 ) ) ;
#36633 = CARTESIAN_POINT ( 'NONE',  ( -1.247161917481749205, -81.59353255999356236, 0.1116756905574352032 ) ) ;
#36634 = CARTESIAN_POINT ( 'NONE',  ( 4.065750953757999220, -79.46192535698398274, -10.27363435345999854 ) ) ;
#36635 = FACE_OUTER_BOUND ( 'NONE', #19656, .T. ) ;
#36636 = DIRECTION ( 'NONE',  ( 0.000000000000000000, 0.000000000000000000, 1.000000000000000000 ) ) ;
#36637 = DIRECTION ( 'NONE',  ( 1.000000000000000000, 0.000000000000000000, 0.000000000000000000 ) ) ;
#36638 = LINE ( 'NONE', #9783, #47196 ) ;
#36639 = CARTESIAN_POINT ( 'NONE',  ( -10.44320937922884518, -78.42521039652507397, 3.377454177612398745 ) ) ;
#36640 = CARTESIAN_POINT ( 'NONE',  ( -11.75000000000000000, -76.70000000000000284, 1.487410190129999909E-14 ) ) ;
#36641 = ORIENTED_EDGE ( 'NONE', *, *, #21756, .T. ) ;
#36642 = ORIENTED_EDGE ( 'NONE', *, *, #34851, .F. ) ;
#36643 = CARTESIAN_POINT ( 'NONE',  ( 10.10224734436263638, -78.82234514084187538, -3.676033498293930002 ) ) ;
#36644 = CARTESIAN_POINT ( 'NONE',  ( 9.596002108778145967, -79.60208333333332575, 7.374560639699001996 ) ) ;
#36645 = ORIENTED_EDGE ( 'NONE', *, *, #35872, .F. ) ;
#36646 = CYLINDRICAL_SURFACE ( 'NONE', #41596, 3.250000000000000000 ) ;
#36647 = CARTESIAN_POINT ( 'NONE',  ( 10.47513974133999959, -23.80361494181999760, 7.624776006159999397 ) ) ;
#36648 = VECTOR ( 'NONE', #50719, 1000.000000000000000 ) ;
#36649 = CARTESIAN_POINT ( 'NONE',  ( 9.636781270596999960, -61.24031362749000351, 7.948066289865000300 ) ) ;
#36650 = FACE_OUTER_BOUND ( 'NONE', #50614, .T. ) ;
#36651 = CARTESIAN_POINT ( 'NONE',  ( 9.148615368834404293, -77.85575384033435853, 7.734521845670259133 ) ) ;
#36652 = CARTESIAN_POINT ( 'NONE',  ( 8.554126827399000987, -80.02791522528700341, -7.255689219360999864 ) ) ;
#36653 = CARTESIAN_POINT ( 'NONE',  ( 9.540055299840034309, -79.30420282387936481, 0.5400507987868797821 ) ) ;
#36654 = ORIENTED_EDGE ( 'NONE', *, *, #17049, .F. ) ;
#36655 = CARTESIAN_POINT ( 'NONE',  ( -7.635939347796300680, -23.77525282322134359, 10.36595956260444673 ) ) ;
#36656 = ORIENTED_EDGE ( 'NONE', *, *, #7817, .T. ) ;
#36657 = B_SPLINE_CURVE_WITH_KNOTS ( 'NONE', 3,
 ( #55622, #20768, #7190, #24621 ),
 .UNSPECIFIED., .F., .F.,
 ( 4, 4 ),
 ( 0.000000000000000000, 1.000000000000000000 ),
 .UNSPECIFIED. ) ;
#36658 = CARTESIAN_POINT ( 'NONE',  ( 2.071969569050668536, -77.45712744981192088, 9.014943109846830893 ) ) ;
#36659 = CARTESIAN_POINT ( 'NONE',  ( 10.94195044575999987, -77.66953159614799063, -1.468969119710000104 ) ) ;
#36660 = CARTESIAN_POINT ( 'NONE',  ( 0.7554284705563453217, -77.83333333333335702, 1.310679582531389276 ) ) ;
#36661 = CARTESIAN_POINT ( 'NONE',  ( 0.6906586288378000482, -78.65211458439600278, -1.459522026167999975 ) ) ;
#36662 = CARTESIAN_POINT ( 'NONE',  ( -8.385806979697797203, -17.11189753004796898, 9.298530586711937218 ) ) ;
#36663 = AXIS2_PLACEMENT_3D ( 'NONE', #1328, #19030, #10176 ) ;
#36664 = EDGE_CURVE ( 'NONE', #19368, #43853, #27961, .T. ) ;
#36665 = DIRECTION ( 'NONE',  ( 0.000000000000000000, -1.000000000000000000, 0.000000000000000000 ) ) ;
#36666 = CARTESIAN_POINT ( 'NONE',  ( 0.1742577344548000007, -77.57690993279000224, 1.489843697164999980 ) ) ;
#36667 = CARTESIAN_POINT ( 'NONE',  ( 7.674627477105999240, -22.75077028084999853, -10.14950121126000049 ) ) ;
#36668 = CARTESIAN_POINT ( 'NONE',  ( 10.24785796630000156, -78.20764851311697896, 3.830033060943999867 ) ) ;
#36669 = ADVANCED_FACE ( 'NONE', ( #54565 ), #9056, .F. ) ;
#36670 = CARTESIAN_POINT ( 'NONE',  ( 12.71162862753478962, -61.03964265605992523, 1.720599174757304395 ) ) ;
#36671 = FACE_OUTER_BOUND ( 'NONE', #34599, .T. ) ;
#36672 = CARTESIAN_POINT ( 'NONE',  ( -3.420428384795999754, -85.98568853081499697, 0.3738047447517999777 ) ) ;
#36673 = ORIENTED_EDGE ( 'NONE', *, *, #8641, .T. ) ;
#36674 = CARTESIAN_POINT ( 'NONE',  ( 10.33813847379999906, -79.23687103921299979, 6.695438874393000006 ) ) ;
#36675 = CARTESIAN_POINT ( 'NONE',  ( -8.527808771699001866, -76.65038675065599705, 7.705797137820999509 ) ) ;
#36676 = CARTESIAN_POINT ( 'NONE',  ( -2.100575672690006446, -77.99078096341597188, 10.54268409913574445 ) ) ;
#36677 = CARTESIAN_POINT ( 'NONE',  ( -2.839805762151343949, -3.458333333333332593, 1.636761686205412181 ) ) ;
#36678 = CARTESIAN_POINT ( 'NONE',  ( -1.749722766154200304, -60.27588992799915957, -12.54673760685751027 ) ) ;
#36679 = CARTESIAN_POINT ( 'NONE',  ( -0.3094144670187705670, -2.631516015699587818, 3.770305080625714123 ) ) ;
#36680 = CARTESIAN_POINT ( 'NONE',  ( 8.103107792609110405, -80.90736235359815964, 7.063989823860713280 ) ) ;
#36681 = CARTESIAN_POINT ( 'NONE',  ( 9.296222075829000175, -77.84175299886499033, 1.480354560350000126 ) ) ;
#36682 = CARTESIAN_POINT ( 'NONE',  ( 0.3702670344839096850, -85.79678895079197787, -8.265161965197931337 ) ) ;
#36683 = CARTESIAN_POINT ( 'NONE',  ( -9.465408641230000697, -77.34685739310599217, 5.887328751257999926 ) ) ;
#36684 = DIRECTION ( 'NONE',  ( 1.000000000000000000, 0.000000000000000000, 0.000000000000000000 ) ) ;
#36685 = CARTESIAN_POINT ( 'NONE',  ( -11.00003927284999961, -80.96429906910999819, -0.7525280789652001312 ) ) ;
#36686 = EDGE_LOOP ( 'NONE', ( #16916, #13701, #6383, #7753 ) ) ;
#36687 = EDGE_CURVE ( 'NONE', #37820, #42621, #10269, .T. ) ;
#36688 = CARTESIAN_POINT ( 'NONE',  ( 9.475051992780000987, -77.89482403538302435, -0.6170397550469999270 ) ) ;
#36689 = CARTESIAN_POINT ( 'NONE',  ( 3.808251865168000183, -2.578157913353000374, 1.108301075316999951 ) ) ;
#36690 = CARTESIAN_POINT ( 'NONE',  ( -6.659967121051000305, -76.77272929337298990, -9.025682433062998555 ) ) ;
#36691 = CARTESIAN_POINT ( 'NONE',  ( -6.405050160242000246, -78.73413188543698027, 8.912875463421000788 ) ) ;
#36692 = CARTESIAN_POINT ( 'NONE',  ( 7.631896413330000684, -23.22122715205999555, -10.36221694966999962 ) ) ;
#36693 = DIRECTION ( 'NONE',  ( 0.000000000000000000, 0.000000000000000000, -1.000000000000000000 ) ) ;
#36694 = CARTESIAN_POINT ( 'NONE',  ( 0.7264933893478244809, -79.75000000000000000, -9.249999992442631935 ) ) ;
#36695 = CARTESIAN_POINT ( 'NONE',  ( -7.635939924807771284, -55.02474192253894358, -10.36595855974767488 ) ) ;
#36696 = CARTESIAN_POINT ( 'NONE',  ( 3.685140862346000024, -82.54767953870899078, 1.956143928933999687 ) ) ;
#36697 = TOROIDAL_SURFACE ( 'NONE', #15029, 13.50000000000000000, 0.5000000000000000000 ) ;
#36698 = CARTESIAN_POINT ( 'NONE',  ( -0.1963495408493673433, -80.38541666666669983, 1.499999999999999334 ) ) ;
#36699 = EDGE_CURVE ( 'NONE', #33164, #26175, #853, .T. ) ;
#36701 = EDGE_CURVE ( 'NONE', #26900, #36425, #13449, .T. ) ;
#36700 = CARTESIAN_POINT ( 'NONE',  ( 10.30457855490000085, -55.03665569380999756, -7.636266480997000450 ) ) ;
#36702 = CARTESIAN_POINT ( 'NONE',  ( -3.647741209468000179, -77.17783883592798588, 10.65494948965999988 ) ) ;
#36703 = CARTESIAN_POINT ( 'NONE',  ( 1.472546342128999930, -80.48166957088999141, -0.7790162248558000213 ) ) ;
#36704 = CARTESIAN_POINT ( 'NONE',  ( -1.202031245603000009, -78.55388828911000587, -0.5457094238513999773 ) ) ;
#36705 = CARTESIAN_POINT ( 'NONE',  ( 2.309272084855999996, -76.97433654539688064, -9.392260232199999948 ) ) ;
#36706 = CARTESIAN_POINT ( 'NONE',  ( 1.519135534786491659, -82.01515637124201419, 0.3015387213458061155 ) ) ;
#36707 = VECTOR ( 'NONE', #52743, 1000.000000000000114 ) ;
#36708 = DIRECTION ( 'NONE',  ( 0.9999999999995751176, 0.000000000000000000, 9.217554803169769657E-07 ) ) ;
#36709 = CARTESIAN_POINT ( 'NONE',  ( -7.532536244959458394, -80.16368247948770431, -7.669252981571465178 ) ) ;
#36710 = CARTESIAN_POINT ( 'NONE',  ( 1.169986272277216299, -79.82176322311053696, -0.4396409049908809319 ) ) ;
#36711 = AXIS2_PLACEMENT_3D ( 'NONE', #14736, #5312, #19474 ) ;
#36712 = VERTEX_POINT ( 'NONE', #38864 ) ;
#36713 = CARTESIAN_POINT ( 'NONE',  ( 0.5491531115358451176, -81.76143395608764308, -1.122793678249770055 ) ) ;
#36714 = CARTESIAN_POINT ( 'NONE',  ( 6.321411194148057078, -79.08065831076486063, 10.10170745394536596 ) ) ;
#36715 = CARTESIAN_POINT ( 'NONE',  ( 10.56933735542999919, -80.16686644544779483, 3.541701167072000445 ) ) ;
#36716 = CARTESIAN_POINT ( 'NONE',  ( 0.6295237254636258939, -80.16666666666664298, -1.092232985442821658 ) ) ;
#36717 = ORIENTED_EDGE ( 'NONE', *, *, #46934, .F. ) ;
#36718 = ORIENTED_EDGE ( 'NONE', *, *, #38712, .T. ) ;
#36719 = CARTESIAN_POINT ( 'NONE',  ( 0.9631070755298999364, -80.86754356702299162, 1.171053640356000125 ) ) ;
#36720 = ORIENTED_EDGE ( 'NONE', *, *, #15787, .F. ) ;
#36721 = ORIENTED_EDGE ( 'NONE', *, *, #47602, .F. ) ;
#36722 = CARTESIAN_POINT ( 'NONE',  ( -1.801750019963999971, -18.60992573277999895, 12.59656967653999970 ) ) ;
#36723 = CARTESIAN_POINT ( 'NONE',  ( 0.000000000000000000, -80.99999999999998579, 7.000000000000000000 ) ) ;
#36724 = CARTESIAN_POINT ( 'NONE',  ( -3.412338500972434741, -81.66770831895492222, 0.4596473917829690392 ) ) ;
#36725 = CARTESIAN_POINT ( 'NONE',  ( 5.441664396738000065, -79.49294334753599856, -8.019902302782998760 ) ) ;
#36726 = CARTESIAN_POINT ( 'NONE',  ( 5.478502669466799091, -78.27562318616411119, -7.453347129908455493 ) ) ;
#36727 = DIRECTION ( 'NONE',  ( 0.000000000000000000, -1.000000000000000000, 0.000000000000000000 ) ) ;
#36728 = CARTESIAN_POINT ( 'NONE',  ( 11.73609379742999970, -79.06292401665000114, -2.784157491330999878 ) ) ;
#36729 = EDGE_LOOP ( 'NONE', ( #48188, #15526, #32285, #2894, #51490 ) ) ;
#36730 = ORIENTED_EDGE ( 'NONE', *, *, #20861, .T. ) ;
#36731 = FACE_OUTER_BOUND ( 'NONE', #395, .T. ) ;
#36732 = DIRECTION ( 'NONE',  ( 0.000000000000000000, 0.000000000000000000, -1.000000000000000000 ) ) ;
#36733 = CARTESIAN_POINT ( 'NONE',  ( -12.76303204291999904, -55.53514849259999409, -1.980584515756000030 ) ) ;
#36734 = CARTESIAN_POINT ( 'NONE',  ( -9.157500079073999544, -78.68270794975798310, 3.211059275314999795 ) ) ;
#36735 = DIRECTION ( 'NONE',  ( 0.000000000000000000, 0.000000000000000000, -1.000000000000000000 ) ) ;
#36736 = CARTESIAN_POINT ( 'NONE',  ( -10.38646360831000059, -19.22204592323999961, 7.655555357453000198 ) ) ;
#36737 = CARTESIAN_POINT ( 'NONE',  ( -9.186177604835998878, -77.89275400357000478, -8.911975928459002105 ) ) ;
#36738 = CARTESIAN_POINT ( 'NONE',  ( -0.7917463127232999831, -79.72302723733999130, -1.236764296276999797 ) ) ;
#36739 = CARTESIAN_POINT ( 'NONE',  ( -2.664101853300902434, -77.15209693750341557, -9.063520957256455901 ) ) ;
#36740 = CARTESIAN_POINT ( 'NONE',  ( 0.000000000000000000, -75.00000000000000000, -7.200000000000000178 ) ) ;
#36741 = CARTESIAN_POINT ( 'NONE',  ( 0.005922634313507149466, -76.57483508499620939, 11.74990209218339743 ) ) ;
#36742 = CARTESIAN_POINT ( 'NONE',  ( 3.936899005229999471, -81.08749251809699388, 1.389401455896000170 ) ) ;
#36744 = CONICAL_SURFACE ( 'NONE', #29194, 11.96250000010999948, 0.7853981633972997312 ) ;
#36743 = CARTESIAN_POINT ( 'NONE',  ( 3.862060628231000159, -80.68104832551259165, 10.58270681924999934 ) ) ;
#36745 = CARTESIAN_POINT ( 'NONE',  ( -8.885605805125999623, -78.03806001420198868, 3.858414063430999796 ) ) ;
#36746 = CARTESIAN_POINT ( 'NONE',  ( 2.994436520183920258, -2.882819031401844700, 1.261580605330494098 ) ) ;
#36747 = CARTESIAN_POINT ( 'NONE',  ( -3.461625351506000481, -81.76505496681200214, -0.7737650771603999944 ) ) ;
#36748 = CARTESIAN_POINT ( 'NONE',  ( 1.302799686710000016, -78.03280592149668848, 0.2851120931344000020 ) ) ;
#36749 = CARTESIAN_POINT ( 'NONE',  ( 8.852642474645787019, -77.49067155497328940, -8.178101815369194227 ) ) ;
#36750 = DIRECTION ( 'NONE',  ( 0.000000000000000000, 1.000000000000000000, 0.000000000000000000 ) ) ;
#36751 = CARTESIAN_POINT ( 'NONE',  ( 9.231148410301667440, -77.20000000000000284, -5.678455705185387004 ) ) ;
#36752 = ORIENTED_EDGE ( 'NONE', *, *, #24164, .F. ) ;
#36753 = CARTESIAN_POINT ( 'NONE',  ( -8.796335266379976758, -78.25208333333333144, -6.760013919724066511 ) ) ;
#36754 = EDGE_CURVE ( 'NONE', #38883, #11264, #47265, .T. ) ;
#36755 = CARTESIAN_POINT ( 'NONE',  ( -5.088691759813757095E-08, -76.94999999999998863, -9.499908983443795307 ) ) ;
#36756 = CARTESIAN_POINT ( 'NONE',  ( 7.958763980604000032, -17.52301961031999866, 9.723170659100999202 ) ) ;
#36757 = CARTESIAN_POINT ( 'NONE',  ( -6.888064133618999385, -79.26660310668899001, 6.902496683615999551 ) ) ;
#36758 = CARTESIAN_POINT ( 'NONE',  ( -12.97295173694999981, -77.45424801882001020, -1.020668466325000079 ) ) ;
#36759 = CARTESIAN_POINT ( 'NONE',  ( -7.614443659027361200, -79.53779634012535382, 7.588181420400903932 ) ) ;
#36760 = DIRECTION ( 'NONE',  ( 0.000000000000000000, 0.000000000000000000, 1.000000000000000000 ) ) ;
#36761 = CARTESIAN_POINT ( 'NONE',  ( 11.62735544928448483, -78.45878212527921391, 1.746294367094141764 ) ) ;
#36762 = EDGE_LOOP ( 'NONE', ( #3185, #46561, #21175, #38932, #33635 ) ) ;
#36763 = CARTESIAN_POINT ( 'NONE',  ( 12.76303204525000012, -60.06485147653999945, 1.980584515753000208 ) ) ;
#36764 = CARTESIAN_POINT ( 'NONE',  ( 8.063504857351000865, -77.93227818423599729, -7.723038145240000318 ) ) ;
#36765 = EDGE_CURVE ( 'NONE', #49440, #39336, #40220, .T. ) ;
#36766 = STYLED_ITEM ( 'NONE', ( #15849 ), #56346 ) ;
#36767 = CARTESIAN_POINT ( 'NONE',  ( -0.2581798279218999737, -82.29592158156299320, 1.583182092587000156 ) ) ;
#36768 = CARTESIAN_POINT ( 'NONE',  ( 7.718368845776000242, -21.74800977511999989, -10.07722254365999959 ) ) ;
#36769 = CARTESIAN_POINT ( 'NONE',  ( 8.779834778627000347, -77.80017512602198337, 3.394951511978999914 ) ) ;
#36771 = CARTESIAN_POINT ( 'NONE',  ( -3.431352783032999731, -1.239182682365999932, 2.086989923523999924 ) ) ;
#36770 = CARTESIAN_POINT ( 'NONE',  ( -2.655896506213000219, -83.21992897967898273, -3.163025014367999876 ) ) ;
#36772 = CARTESIAN_POINT ( 'NONE',  ( 1.249999999999999778, -82.26041666666665719, 0.1636246173744711763 ) ) ;
#36773 = CARTESIAN_POINT ( 'NONE',  ( -0.7554284705563544255, -81.41666666666668561, 1.310679582531384169 ) ) ;
#36774 = ORIENTED_EDGE ( 'NONE', *, *, #3067, .T. ) ;
#36775 = CARTESIAN_POINT ( 'NONE',  ( -1.250000000000000000, -82.09999999999999432, 0.000000000000000000 ) ) ;
#36776 = CARTESIAN_POINT ( 'NONE',  ( -0.9218200799623714747, -78.97291666666669130, -1.199500263597270466 ) ) ;
#36777 = CARTESIAN_POINT ( 'NONE',  ( -3.851650068367032276, -78.96264283715741783, 7.703300136734017478 ) ) ;
#36778 = VERTEX_POINT ( 'NONE', #2865 ) ;
#36779 = ORIENTED_EDGE ( 'NONE', *, *, #24433, .F. ) ;
#36780 = CARTESIAN_POINT ( 'NONE',  ( 10.84079038992999955, -79.61007816076597976, -1.471421101766999806 ) ) ;
#36781 = FACE_OUTER_BOUND ( 'NONE', #25314, .T. ) ;
#36782 = ORIENTED_EDGE ( 'NONE', *, *, #2056, .T. ) ;
#36783 = CARTESIAN_POINT ( 'NONE',  ( 10.75624577990000041, -78.40392649052799356, -5.431293436759999871 ) ) ;
#36784 = ADVANCED_FACE ( 'NONE', ( #51600 ), #24429, .F. ) ;
#36785 = ORIENTED_EDGE ( 'NONE', *, *, #19076, .F. ) ;
#36786 = B_SPLINE_SURFACE_WITH_KNOTS ( 'NONE', 3, 3, ( 
 ( #25051, #43073, #34470, #56647, #34181, #52501, #12059, #20628, #40065, #3482, #53961, #44805, #40371, #58082, #44503, #35630, #48940, #58379, #17641, #17060, #31193, #17941, #4661, #22661, #49536, #25911, #35333, #35041, #18244, #53075, #30622, #30329, #27069, #12626, #26775 ),
 ( #45108, #48655, #31490, #52787, #9083, #35932, #13498, #8199, #53658, #48371, #53359, #40671, #261, #12342, #49232, #26201, #21487, #3768, #7909, #12907, #44219, #30905, #43933, #39494, #57498, #21771, #4356, #39774, #57789, #17344, #22358, #8485, #26480, #4054, #22058 ),
 ( #13198, #8784, #14960, #23819, #32957, #27658, #5814, #18533, #36525, #37103, #51002, #32087, #41838, #10551, #41252, #28533, #24116, #5521, #23244, #1700, #13789, #9380, #50127, #45701, #5239, #839, #18822, #36814, #54832, #32373, #57624, #17472, #27189, #40199, #49660 ),
 ( #8323, #36061, #44337, #49067, #39901, #57915, #45229, #35462, #13620, #53791, #13031, #26903, #8913, #40496, #4191, #35761, #44931, #39333, #4488, #22486, #93, #42767, #51634, #42181, #10897, #11476, #11188, #27485, #29164, #47211, #6446, #51916, #1750, #38318, #45526 ) ),
 .UNSPECIFIED., .F., .F., .F.,
 ( 4, 4 ),
 ( 4, 1, 1, 1, 1, 1, 1, 1, 1, 1, 1, 1, 1, 1, 1, 1, 1, 1, 1, 1, 1, 1, 1, 1, 1, 1, 1, 1, 1, 1, 1, 1, 4 ),
 ( -0.1377334280162000046, 1.137733428016000081 ),
 ( -0.01671641791045000089, 0.01044776119403000025, 0.03761194029850999793, 0.06477611940298999560, 0.09194029850746000820, 0.1191044776118999893, 0.1462686567163999918, 0.1734328358208999943, 0.2005970149253999968, 0.2277611940298999993, 0.2549253731343000262, 0.2820895522388000010, 0.3092537313432999757, 0.3364179104478000060, 0.3635820895522000051, 0.3907462686567000354, 0.4179104477612000101, 0.4450746268656999849, 0.4722388059701999596, 0.4994029850746000143, 0.5265671641790999891, 0.5537313432836000748, 0.5808955223881000496, 0.6080597014924999932, 0.6352238805969999680, 0.6623880597014999427, 0.6895522388060000285, 0.7167164179105000033, 0.7438805970148999469, 0.7710447761194000327, 0.7982089552239000074, 0.8253731343283999822, 0.8525373134328000368 ),
 .UNSPECIFIED. ) ;
#36787 = VERTEX_POINT ( 'NONE', #28838 ) ;
#36788 = VECTOR ( 'NONE', #53273, 1000.000000000000000 ) ;
#36789 = CARTESIAN_POINT ( 'NONE',  ( -0.9863005837836278378, -2.701660951675892708, -3.096296943042188499 ) ) ;
#36790 = CIRCLE ( 'NONE', #11363, 5.500000000000000000 ) ;
#36791 = EDGE_LOOP ( 'NONE', ( #35306, #39913, #9348, #49024, #41041, #7143 ) ) ;
#36792 = CARTESIAN_POINT ( 'NONE',  ( 7.374560639698954034, -78.62291666666662593, 9.596002108778181494 ) ) ;
#36793 = CARTESIAN_POINT ( 'NONE',  ( -7.000000000000000000, -81.19999999999998863, 0.000000000000000000 ) ) ;
#36794 = ORIENTED_EDGE ( 'NONE', *, *, #16973, .F. ) ;
#36795 = CARTESIAN_POINT ( 'NONE',  ( -10.12290050256999940, -18.75000002239000096, -7.648026768411000376 ) ) ;
#36796 = ORIENTED_EDGE ( 'NONE', *, *, #53848, .F. ) ;
#36797 = CARTESIAN_POINT ( 'NONE',  ( 10.42531125068999920, -23.26485145404000221, -7.624341767093000044 ) ) ;
#36798 = CARTESIAN_POINT ( 'NONE',  ( 9.583569705204123323, -78.11247223426698838, 1.526112543548083345 ) ) ;
#36799 = DIRECTION ( 'NONE',  ( 0.000000000000000000, -1.000000000000000000, 0.000000000000000000 ) ) ;
#36800 = DIRECTION ( 'NONE',  ( 0.000000000000000000, 1.000000000000000000, 0.000000000000000000 ) ) ;
#36801 = CARTESIAN_POINT ( 'NONE',  ( -5.279550234765999939, -76.28419320068699960, -9.859017853534000508 ) ) ;
#36802 = DIRECTION ( 'NONE',  ( -1.000000000000000000, 0.000000000000000000, 0.000000000000000000 ) ) ;
#36803 = CARTESIAN_POINT ( 'NONE',  ( 13.89248035986000041, -46.40840747658999277, 2.632528379853999966E-05 ) ) ;
#36804 = CARTESIAN_POINT ( 'NONE',  ( -1.667212297213999994, -76.71026873785200451, 11.10423992239999968 ) ) ;
#36805 = CARTESIAN_POINT ( 'NONE',  ( 6.549831546891490497, -78.78778326711085356, -6.531473034326317872 ) ) ;
#36806 = CARTESIAN_POINT ( 'NONE',  ( 6.299964168848140922, -76.52989574100779180, 9.922046080742738638 ) ) ;
#36807 = AXIS2_PLACEMENT_3D ( 'NONE', #22388, #50154, #36842 ) ;
#36808 = CARTESIAN_POINT ( 'NONE',  ( 0.1610657711267718117, -23.74946977292816186, -10.99997582743960578 ) ) ;
#36809 = CARTESIAN_POINT ( 'NONE',  ( -0.2340539085346999837, -80.02337760721299276, 1.312933706406000267 ) ) ;
#36810 = CARTESIAN_POINT ( 'NONE',  ( -9.189182874619413965, -80.14647585629263915, -6.046231220059206102 ) ) ;
#36811 = MANIFOLD_SOLID_BREP ( 'Stock-MAS-694-1', #35216 ) ;
#36812 = CARTESIAN_POINT ( 'NONE',  ( -1.538071403320043551, -76.68541666666665435, 11.74999999999999467 ) ) ;
#36813 = CARTESIAN_POINT ( 'NONE',  ( 3.459153386863000446, -79.39967549782629419, 2.256714709944000141 ) ) ;
#36814 = CARTESIAN_POINT ( 'NONE',  ( -2.517806253849999898, -77.08911332859899801, 9.318471479766001764 ) ) ;
#36815 = DIRECTION ( 'NONE',  ( 0.000000000000000000, 1.000000000000000000, 0.000000000000000000 ) ) ;
#36816 = CARTESIAN_POINT ( 'NONE',  ( 5.413904038987179312, -79.66666666666662877, -9.393203674808262349 ) ) ;
#36817 = DIRECTION ( 'NONE',  ( 0.000000000000000000, 0.7071067811866525998, -0.7071067811864425456 ) ) ;
#36818 = LINE ( 'NONE', #55123, #57217 ) ;
#36819 = CARTESIAN_POINT ( 'NONE',  ( -10.48543666025111776, -79.35833333333330586, 6.043427764450754580 ) ) ;
#36820 = CARTESIAN_POINT ( 'NONE',  ( -3.533965481030999722, -1.844405165121999923, 1.774394495578000219 ) ) ;
#36821 = EDGE_CURVE ( 'NONE', #32447, #44781, #10697, .T. ) ;
#36822 = CARTESIAN_POINT ( 'NONE',  ( 0.9995835529977233902, -80.80208333333332860, 0.7681833999686461523 ) ) ;
#36823 = CARTESIAN_POINT ( 'NONE',  ( 10.07722254367000048, -58.54800977479000323, 7.718368845781999887 ) ) ;
#36825 = EDGE_CURVE ( 'NONE', #53933, #17027, #13669, .T. ) ;
#36824 = CARTESIAN_POINT ( 'NONE',  ( -1.629367637659999923, -23.68263643397999729, -12.46114270826000059 ) ) ;
#36826 = CIRCLE ( 'NONE', #14191, 1.200000000000000622 ) ;
#36827 = LINE ( 'NONE', #5250, #542 ) ;
#36828 = CARTESIAN_POINT ( 'NONE',  ( -8.485281374238999419, -18.75000000000000000, -8.485281374238999419 ) ) ;
#36829 = CARTESIAN_POINT ( 'NONE',  ( -7.347140770713999736, -77.29944927882600325, 9.839476697348001011 ) ) ;
#36830 = CYLINDRICAL_SURFACE ( 'NONE', #1521, 1.750000000000001332 ) ;
#36832 = CARTESIAN_POINT ( 'NONE',  ( -1.183003490338000008, -79.33784971804600161, -0.6653023415106000815 ) ) ;
#36831 = CARTESIAN_POINT ( 'NONE',  ( -7.624341766656999475, -60.06485146221000093, -10.42531125026000005 ) ) ;
#36833 = CARTESIAN_POINT ( 'NONE',  ( 0.6444261930239000291, -82.61409087623900405, 1.576239777183000124 ) ) ;
#36834 = ORIENTED_EDGE ( 'NONE', *, *, #50771, .F. ) ;
#36835 = CARTESIAN_POINT ( 'NONE',  ( -0.6947249814979998828, -83.71682450217399207, -3.521518806877999896 ) ) ;
#36836 = CARTESIAN_POINT ( 'NONE',  ( -2.662490087786000270, -79.23049308225799336, -11.62527415693000066 ) ) ;
#36837 = CARTESIAN_POINT ( 'NONE',  ( -1.649606550861999921, -81.16313956354109393, 11.28560569546000103 ) ) ;
#36838 = EDGE_CURVE ( 'NONE', #17863, #32930, #32475, .T. ) ;
#36839 = DIRECTION ( 'NONE',  ( 0.000000000000000000, 1.000000000000000000, 0.000000000000000000 ) ) ;
#36840 = CARTESIAN_POINT ( 'NONE',  ( 0.4739077948423049413, -85.79166667334425256, 3.377908686572150820 ) ) ;
#36841 = CARTESIAN_POINT ( 'NONE',  ( 12.66316398243999863, -53.62133896622000151, 0.04044089952533000409 ) ) ;
#36842 = DIRECTION ( 'NONE',  ( 1.000000000000000000, 0.000000000000000000, 0.000000000000000000 ) ) ;
#36843 = CARTESIAN_POINT ( 'NONE',  ( -0.6556216971886000833, -0.8299739483179999766, -3.808213771107999968 ) ) ;
#36844 = CARTESIAN_POINT ( 'NONE',  ( 9.890776657308000708, -79.52153893684399577, 0.09015406917691999589 ) ) ;
#36845 = CARTESIAN_POINT ( 'NONE',  ( 3.399186938124000079, -81.00000000000000000, -10.46162167925000119 ) ) ;
#36846 = ORIENTED_EDGE ( 'NONE', *, *, #23496, .F. ) ;
#36847 = CARTESIAN_POINT ( 'NONE',  ( -1.178447680628000205, -80.55308451575899653, -0.9280415206345000723 ) ) ;
#36848 = CARTESIAN_POINT ( 'NONE',  ( -11.75000000000000000, -77.20000000000000284, -1.435311119447000145E-14 ) ) ;
#36849 = CARTESIAN_POINT ( 'NONE',  ( 0.000000000000000000, -79.79999999999999716, 0.000000000000000000 ) ) ;
#36850 = B_SPLINE_CURVE_WITH_KNOTS ( 'NONE', 3,
 ( #11599, #29860, #52328, #8016, #29287, #47632, #7155, #16313, #52613, #47336, #25156, #43182, #7447, #38734, #44039, #34294, #43466, #56753, #20164, #48200, #11883, #43758, #6865, #39312 ),
 .UNSPECIFIED., .F., .F.,
 ( 4, 2, 2, 2, 2, 2, 2, 2, 2, 2, 2, 4 ),
 ( 0.000000000000000000, 0.1249999999999986400, 0.2499999999999972800, 0.3749999999999958922, 0.4374999999999955036, 0.4999999999999951150, 0.6249999999999954481, 0.7499999999999956701, 0.8124999999999944489, 0.8437499999999938938, 0.8749999999999933387, 1.000000000000000000 ),
 .UNSPECIFIED. ) ;
#36851 = CARTESIAN_POINT ( 'NONE',  ( -12.69619287815999975, -57.04916621739000249, -1.799475295154000065 ) ) ;
#36852 = CARTESIAN_POINT ( 'NONE',  ( 1.218242831762920586, -80.82990848825727426, -0.3279570865790462642 ) ) ;
#36853 = EDGE_LOOP ( 'NONE', ( #24329, #15592, #13915, #52667, #57855 ) ) ;
#36854 = AXIS2_PLACEMENT_3D ( 'NONE', #4026, #34443, #35304 ) ;
#36855 = CARTESIAN_POINT ( 'NONE',  ( -0.8126767071385999630, -78.94632035071100518, -12.25297252704000073 ) ) ;
#36856 = CARTESIAN_POINT ( 'NONE',  ( 10.73068991439000186, -77.28110149971999476, -3.611733201485999967 ) ) ;
#36857 = CARTESIAN_POINT ( 'NONE',  ( -1.930989179114000143, -21.75453807238000081, 12.80896991324000034 ) ) ;
#36858 = VERTEX_POINT ( 'NONE', #34710 ) ;
#36859 = ORIENTED_EDGE ( 'NONE', *, *, #35264, .F. ) ;
#36860 = CARTESIAN_POINT ( 'NONE',  ( -1.158645246675607199, -80.56947091650550874, 0.4690212617335481893 ) ) ;
#36861 = CARTESIAN_POINT ( 'NONE',  ( 3.366547962069000199, -79.66330989936849960, -9.168809063548000182 ) ) ;
#36862 = ORIENTED_EDGE ( 'NONE', *, *, #19623, .F. ) ;
#36863 = CARTESIAN_POINT ( 'NONE',  ( -12.00000000000000000, -23.25000000000000000, 0.000000000000000000 ) ) ;
#36864 = DIRECTION ( 'NONE',  ( -0.7071067811865474617, 0.000000000000000000, -0.7071067811865474617 ) ) ;
#36865 = AXIS2_PLACEMENT_3D ( 'NONE', #11701, #56855, #23949 ) ;
#36866 = CARTESIAN_POINT ( 'NONE',  ( -12.57434559697999887, -23.71110719500000030, -1.760800161976000089 ) ) ;
#36867 = ORIENTED_EDGE ( 'NONE', *, *, #22940, .F. ) ;
#36868 = CARTESIAN_POINT ( 'NONE',  ( 2.962511214703000384, -77.78030194988500057, -9.021140561863999707 ) ) ;
#36869 = EDGE_CURVE ( 'NONE', #51020, #17089, #41590, .T. ) ;
#36870 = CARTESIAN_POINT ( 'NONE',  ( -0.8777456576965628754, -80.16355898801532476, -0.8895264229757680052 ) ) ;
#36871 = CARTESIAN_POINT ( 'NONE',  ( -0.1380878922993147850, -16.77265597675732423, -12.70555840932534508 ) ) ;
#36872 = CARTESIAN_POINT ( 'NONE',  ( -9.546815224142999767, -17.31472046677999899, -8.130854305520999858 ) ) ;
#36873 = B_SPLINE_CURVE_WITH_KNOTS ( 'NONE', 3,
 ( #48661, #49840, #270, #49240, #17949, #18540 ),
 .UNSPECIFIED., .F., .F.,
 ( 4, 1, 1, 4 ),
 ( 0.000000000000000000, 0.3333333333333000081, 0.6666666666667000474, 1.000000000000000000 ),
 .UNSPECIFIED. ) ;
#36874 = CARTESIAN_POINT ( 'NONE',  ( 9.250000000000000000, -79.84999999999999432, 0.000000000000000000 ) ) ;
#36875 = CARTESIAN_POINT ( 'NONE',  ( -1.531361644451373349, -78.35640210815725482, -0.1250911378582522659 ) ) ;
#36876 = CARTESIAN_POINT ( 'NONE',  ( -3.856336781450672824, -80.12604166151689356, 1.240447633703557706 ) ) ;
#36877 = ORIENTED_EDGE ( 'NONE', *, *, #43832, .F. ) ;
#36878 = CARTESIAN_POINT ( 'NONE',  ( -9.500000000000000000, -77.79999999999999716, 0.000000000000000000 ) ) ;
#36879 = CARTESIAN_POINT ( 'NONE',  ( -12.19234209666000091, -76.02834339985999179, -1.697737568323999913 ) ) ;
#36880 = CARTESIAN_POINT ( 'NONE',  ( 1.293420685949000060, -79.64637299687198890, 0.7912046490545000532 ) ) ;
#36881 = CARTESIAN_POINT ( 'NONE',  ( -2.606762920072624556, -2.407945368431018807, -2.366633524576750247 ) ) ;
#36882 = CARTESIAN_POINT ( 'NONE',  ( 12.71658889741000031, -18.68415522710999710, 1.931087888049999979 ) ) ;
#36883 = CARTESIAN_POINT ( 'NONE',  ( -7.421655993048999811, -78.40939100203998180, 9.763070719336001346 ) ) ;
#36884 = CARTESIAN_POINT ( 'NONE',  ( -1.750000000001000089, -19.24922971542000028, 12.60356226396999979 ) ) ;
#36885 = CARTESIAN_POINT ( 'NONE',  ( -3.184161977317994108, -85.88547957940599531, 1.417680250971013356 ) ) ;
#36886 = CARTESIAN_POINT ( 'NONE',  ( 9.998727717550137228, -60.72738947565300549, -7.709134076929346158 ) ) ;
#36887 = CARTESIAN_POINT ( 'NONE',  ( 4.105073526112258619, -77.20258383217594655, -11.34720543678841231 ) ) ;
#36888 = CARTESIAN_POINT ( 'NONE',  ( -9.931063219235598538, -17.87724209356603566, 7.763994033422829233 ) ) ;
#36889 = ORIENTED_EDGE ( 'NONE', *, *, #46148, .F. ) ;
#36891 = EDGE_CURVE ( 'NONE', #48925, #29378, #3158, .T. ) ;
#36890 = CARTESIAN_POINT ( 'NONE',  ( 0.000000000000000000, -18.75000000000000000, 12.00000000000000000 ) ) ;
#36892 = CARTESIAN_POINT ( 'NONE',  ( -1.172849536488999922, -80.47861590553999633, 0.6711148834816000885 ) ) ;
#36893 = CARTESIAN_POINT ( 'NONE',  ( 7.712213536729100483, -24.06179137615005814, 10.27334987165781399 ) ) ;
#36894 = CARTESIAN_POINT ( 'NONE',  ( 1.250000000000000000, -82.74999999999998579, 0.000000000000000000 ) ) ;
#36895 = CARTESIAN_POINT ( 'NONE',  ( 7.377665174502719303, -77.00000000000001421, 5.715929696616472100 ) ) ;
#36896 = CARTESIAN_POINT ( 'NONE',  ( 0.6062141276560999437, -82.42503003582099552, -1.551696954864999922 ) ) ;
#36897 = CARTESIAN_POINT ( 'NONE',  ( -7.140570215937000143, -77.50263047206500744, 9.562832187120999805 ) ) ;
#36898 = CARTESIAN_POINT ( 'NONE',  ( 8.831426253027000683, -78.42428574649498785, -3.841760052678000026 ) ) ;
#36899 = CARTESIAN_POINT ( 'NONE',  ( 8.452817831826150652, -76.01051698363419007, 8.161467144352542391 ) ) ;
#36900 = CARTESIAN_POINT ( 'NONE',  ( -0.2253802134100999777, -78.58225536775100295, -10.88640714497000062 ) ) ;
#36901 = CARTESIAN_POINT ( 'NONE',  ( -2.503178322335409600, -85.80681307385597734, 3.378898422409377655 ) ) ;
#36902 = ORIENTED_EDGE ( 'NONE', *, *, #31899, .F. ) ;
#36903 = CARTESIAN_POINT ( 'NONE',  ( 0.5999999999999999778, -18.84999999999999787, -10.98362417419999915 ) ) ;
#36904 = CARTESIAN_POINT ( 'NONE',  ( 7.396628201097954936, -77.90225191519014913, 5.684307536487873236 ) ) ;
#36905 = EDGE_CURVE ( 'NONE', #378, #19974, #53069, .T. ) ;
#36906 = CONICAL_SURFACE ( 'NONE', #44452, 3.899999999992999733, 0.7853981633972997312 ) ;
#36907 = CARTESIAN_POINT ( 'NONE',  ( -9.438868967565998247, -79.53307245776798595, -5.601050722391000214 ) ) ;
#36908 = EDGE_CURVE ( 'NONE', #47018, #35080, #33259, .T. ) ;
#36909 = CARTESIAN_POINT ( 'NONE',  ( 1.250000000000000000, -60.04999999966999980, -12.00000000000000000 ) ) ;
#36910 = CARTESIAN_POINT ( 'NONE',  ( -10.78924115793999938, -76.83124045265999769, 6.320304850973999855 ) ) ;
#36911 = CARTESIAN_POINT ( 'NONE',  ( -1.750000000000000000, -55.55000000278000272, -12.50000000000000000 ) ) ;
#36912 = CARTESIAN_POINT ( 'NONE',  ( 8.643969996075000495, -16.74046576158000121, -9.422817222712001950 ) ) ;
#36913 = CARTESIAN_POINT ( 'NONE',  ( -12.70556836347999941, -25.22772277227999993, -2.424223956931999920E-09 ) ) ;
#36914 = ORIENTED_EDGE ( 'NONE', *, *, #36687, .F. ) ;
#36915 = AXIS2_PLACEMENT_3D ( 'NONE', #9707, #23283, #41292 ) ;
#36916 = CARTESIAN_POINT ( 'NONE',  ( 0.9518616847512999524, -78.84066710378499465, -11.10623968335000100 ) ) ;
#36917 = CARTESIAN_POINT ( 'NONE',  ( -9.250000000000000000, -77.49999999999998579, -1.203901273580999948E-14 ) ) ;
#36918 = CARTESIAN_POINT ( 'NONE',  ( 6.606377239730313988, -79.82291666666665719, 8.596418555780454440 ) ) ;
#36919 = CARTESIAN_POINT ( 'NONE',  ( -3.850965828042431482, -78.43735716284258785, -0.07259779887146158850 ) ) ;
#36920 = CARTESIAN_POINT ( 'NONE',  ( -1.500000000000000000, -79.00000000000000000, 0.000000000000000000 ) ) ;
#36921 = CARTESIAN_POINT ( 'NONE',  ( 11.48314430570033373, -76.43277512481758151, -2.489787879572519458 ) ) ;
#36922 = CARTESIAN_POINT ( 'NONE',  ( -7.934077584064515243, -77.00000000000000000, -5.060727184842107818 ) ) ;
#36923 = CARTESIAN_POINT ( 'NONE',  ( 3.171758640500000226, -3.532739359372000010, 1.479846994257000059 ) ) ;
#36924 = EDGE_CURVE ( 'NONE', #37143, #37146, #56885, .T. ) ;
#36925 = CARTESIAN_POINT ( 'NONE',  ( -9.760776772971999193, -92.33215535459000023, -3.252729338753999803E-10 ) ) ;
#36926 = CARTESIAN_POINT ( 'NONE',  ( 10.74358412115683770, -79.18370396350707097, -2.245711267065026551 ) ) ;
#36927 = CARTESIAN_POINT ( 'NONE',  ( -4.658152026654871491, -79.73958333333277437, -8.062158950714737315 ) ) ;
#36928 = ORIENTED_EDGE ( 'NONE', *, *, #7961, .T. ) ;
#36929 = ORIENTED_EDGE ( 'NONE', *, *, #28605, .T. ) ;
#36930 = B_SPLINE_CURVE_WITH_KNOTS ( 'NONE', 3,
 ( #1334, #2487, #50921, #20491, #16059, #29329, #51217, #38487, #41759, #24914, #32877, #14881, #19913, #6028, #42933, #20204, #56504, #19329 ),
 .UNSPECIFIED., .F., .F.,
 ( 4, 2, 2, 2, 2, 2, 2, 2, 4 ),
 ( 0.000000000000000000, 0.1250000000000000278, 0.2500000000000000555, 0.3750000000000000000, 0.5000000000000000000, 0.6250000000000000000, 0.7500000000000000000, 0.8750000000000001110, 1.000000000000000000 ),
 .UNSPECIFIED. ) ;
#36931 = CARTESIAN_POINT ( 'NONE',  ( 7.184181682494999777, -77.75082999526600247, 6.343145485738000744 ) ) ;
#36932 =( GEOMETRIC_REPRESENTATION_CONTEXT ( 3 ) GLOBAL_UNCERTAINTY_ASSIGNED_CONTEXT ( ( #51429 ) ) GLOBAL_UNIT_ASSIGNED_CONTEXT ( ( #40420, #31241, #45158 ) ) REPRESENTATION_CONTEXT ( 'NONE', 'WORKASPACE' ) );
#36933 = CARTESIAN_POINT ( 'NONE',  ( 9.567317839327603934, -78.81236982575325101, -4.905351266707688396 ) ) ;
#36934 = ORIENTED_EDGE ( 'NONE', *, *, #55333, .T. ) ;
#36935 = CARTESIAN_POINT ( 'NONE',  ( 1.849737152796000039, -76.61177708502411576, 11.02961253863000124 ) ) ;
#36936 = CARTESIAN_POINT ( 'NONE',  ( -3.374925386387973347, -83.24791668126330535, -0.6818111582454060571 ) ) ;
#36937 = ADVANCED_FACE ( 'NONE', ( #53029 ), #575, .F. ) ;
#36938 = EDGE_CURVE ( 'NONE', #34885, #37074, #49332, .T. ) ;
#36939 = CARTESIAN_POINT ( 'NONE',  ( 10.30458248780999853, -60.56332651778999576, 7.636263891343999965 ) ) ;
#36940 = CARTESIAN_POINT ( 'NONE',  ( -12.18072440915408450, -77.04494352351606778, 0.6797451543154154896 ) ) ;
#36941 = CARTESIAN_POINT ( 'NONE',  ( 2.228715616918034215, -77.91001247118138906, 11.77084610582519453 ) ) ;
#36942 = CARTESIAN_POINT ( 'NONE',  ( -5.394429334091999984, -79.91896985327970526, -9.834543342166998769 ) ) ;
#36943 = CARTESIAN_POINT ( 'NONE',  ( 7.685486533051383518, -81.00000000000001421, 7.726202419513529485 ) ) ;
#36944 = VERTEX_POINT ( 'NONE', #15935 ) ;
#36945 = CARTESIAN_POINT ( 'NONE',  ( 10.53001524630587404, -77.97857283748489010, -2.879224655733970017 ) ) ;
#36946 = ORIENTED_EDGE ( 'NONE', *, *, #39380, .T. ) ;
#36947 = CARTESIAN_POINT ( 'NONE',  ( 9.240164464789534904, -77.35383050921583958, 0.4429433074386741609 ) ) ;
#36948 = CARTESIAN_POINT ( 'NONE',  ( -4.789974786805000662, -78.01943839146699133, -9.946872946892002076 ) ) ;
#36949 = AXIS2_PLACEMENT_3D ( 'NONE', #41100, #23955, #14805 ) ;
#36950 = LINE ( 'NONE', #1258, #32860 ) ;
#36951 = AXIS2_PLACEMENT_3D ( 'NONE', #14475, #51964, #20371 ) ;
#36952 = CARTESIAN_POINT ( 'NONE',  ( -1.472799192485999997, -77.56639593435953373, -0.3599880333205999761 ) ) ;
#36953 = CARTESIAN_POINT ( 'NONE',  ( -12.00000000000000000, -77.39999999999999147, 0.000000000000000000 ) ) ;
#36954 = CARTESIAN_POINT ( 'NONE',  ( -2.317157120869037801, -2.062400358190874083, -2.314279884217083971 ) ) ;
#36955 = CARTESIAN_POINT ( 'NONE',  ( 1.314530797355000225, -77.97021567534000042, -0.9595159925157999981 ) ) ;
#36956 = CARTESIAN_POINT ( 'NONE',  ( 4.044903269867999640, -79.46000000000000796, -8.595856998426999240 ) ) ;
#36957 = CARTESIAN_POINT ( 'NONE',  ( 3.166366903731000271, -79.78082035574699660, 10.47195928638999973 ) ) ;
#36958 = CARTESIAN_POINT ( 'NONE',  ( -7.943805570347999279, -24.43402324524999969, -9.641149735076000482 ) ) ;
#36959 = CARTESIAN_POINT ( 'NONE',  ( -8.768124086712999699, -59.94999999967000548, 7.919595949288999570 ) ) ;
#36960 = CARTESIAN_POINT ( 'NONE',  ( 2.949808988708999991, -82.26950239379898733, -1.686642012998000206 ) ) ;
#36961 = VERTEX_POINT ( 'NONE', #20936 ) ;
#36962 = CARTESIAN_POINT ( 'NONE',  ( -11.00000000000000000, -77.19999999999998863, 5.688460190305999883E-13 ) ) ;
#36963 = CARTESIAN_POINT ( 'NONE',  ( 9.696452258889999953, -75.92770142656900134, 4.797923606538000207 ) ) ;
#36964 = CARTESIAN_POINT ( 'NONE',  ( 10.45679952538025503, -77.86866984986814089, 2.493435623531266021 ) ) ;
#36965 = CARTESIAN_POINT ( 'NONE',  ( -3.085175050843000477, -78.17037848440200776, -11.57574012064000080 ) ) ;
#36966 = CARTESIAN_POINT ( 'NONE',  ( -10.15323015673999940, -17.76919784905000199, 7.760928569209999850 ) ) ;
#36967 = AXIS2_PLACEMENT_3D ( 'NONE', #4979, #32405, #54582 ) ;
#36969 = DIRECTION ( 'NONE',  ( 0.000000000000000000, 0.000000000000000000, -1.000000000000000000 ) ) ;
#36968 = CARTESIAN_POINT ( 'NONE',  ( 9.396085398178630754, -78.49791666666665435, -7.220923959705230821 ) ) ;
#36970 = CARTESIAN_POINT ( 'NONE',  ( -3.388399644966007873, -2.776263346416080857, -1.176069256401409691 ) ) ;
#36971 = CARTESIAN_POINT ( 'NONE',  ( 3.981698583510459244, -80.94499118605105537, 9.985454001900388121 ) ) ;
#36972 = CARTESIAN_POINT ( 'NONE',  ( 9.086766343481999186, -78.80816318924999564, -2.458053382951000287 ) ) ;
#36973 = CARTESIAN_POINT ( 'NONE',  ( -3.518657424384993959, -85.83735716284299144, 1.566607219110014659 ) ) ;
#36974 = CARTESIAN_POINT ( 'NONE',  ( -9.936460025306999455, -77.42856642211100393, -5.051867252445999767 ) ) ;
#36975 = CYLINDRICAL_SURFACE ( 'NONE', #7337, 11.00000000000000000 ) ;
#36976 = CARTESIAN_POINT ( 'NONE',  ( 9.669337410324999382, -80.66897452307009075, -5.298214362520000442 ) ) ;
#36977 = ORIENTED_EDGE ( 'NONE', *, *, #16242, .F. ) ;
#36978 = CARTESIAN_POINT ( 'NONE',  ( 4.574312611392000072, -77.48499903538302647, 8.320643751074999983 ) ) ;
#36979 = CARTESIAN_POINT ( 'NONE',  ( -3.409844804438999954, -1.755159555871000032, -1.689431510286000027 ) ) ;
#36980 = CARTESIAN_POINT ( 'NONE',  ( -10.54491486739000017, -77.72600129843600314, -3.823987582478999947 ) ) ;
#36981 = CARTESIAN_POINT ( 'NONE',  ( -4.277738290159001089, -78.90268601143299065, -10.10766895494000117 ) ) ;
#36982 = CARTESIAN_POINT ( 'NONE',  ( 9.213114944024999531, -25.00524898755999814, -8.533795138592999763 ) ) ;
#36983 = EDGE_CURVE ( 'NONE', #19319, #30464, #43065, .T. ) ;
#36984 = CARTESIAN_POINT ( 'NONE',  ( 1.000000000000000000, -78.00000000000000000, 7.200000000000000178 ) ) ;
#36985 = CARTESIAN_POINT ( 'NONE',  ( -1.247385801080000078, -24.47722256257000240, -12.50301438876999960 ) ) ;
#36986 = CARTESIAN_POINT ( 'NONE',  ( 0.000000000000000000, -0.7781249991808000255, 0.000000000000000000 ) ) ;
#36987 = CARTESIAN_POINT ( 'NONE',  ( 4.043613182668000405, -83.99694503318799832, 1.029201014592999952 ) ) ;
#36988 = CARTESIAN_POINT ( 'NONE',  ( -7.651147547606000465, -22.76256650325000308, -10.45204383577999963 ) ) ;
#36989 = CARTESIAN_POINT ( 'NONE',  ( 8.643969996042999426, -53.54046576124999746, -9.422817222680000881 ) ) ;
#36990 = CARTESIAN_POINT ( 'NONE',  ( 9.101894997447999458, -78.37903382810698361, -6.639611571546000235 ) ) ;
#36991 = LINE ( 'NONE', #50013, #33301 ) ;
#36992 = CARTESIAN_POINT ( 'NONE',  ( -0.7426966924155999905, -78.44252514954999356, 1.091365894571999950 ) ) ;
#36993 = CARTESIAN_POINT ( 'NONE',  ( -6.043427764450832740, -77.71666666666666856, 10.48543666025107512 ) ) ;
#36994 = CARTESIAN_POINT ( 'NONE',  ( 0.08823669215798200793, -81.62041127680433306, 1.507463071252419962 ) ) ;
#36995 = LINE ( 'NONE', #37287, #38389 ) ;
#36996 = CARTESIAN_POINT ( 'NONE',  ( -6.805157294386518174, -80.17080800408460561, -8.328756680024682169 ) ) ;
#36997 = CARTESIAN_POINT ( 'NONE',  ( -5.838193839761688153, -77.87291666666668277, -7.596835002782716728 ) ) ;
#36998 = EDGE_CURVE ( 'NONE', #4635, #26450, #35140, .T. ) ;
#36999 = VERTEX_POINT ( 'NONE', #24794 ) ;
#37000 = CARTESIAN_POINT ( 'NONE',  ( -0.3656892198172155273, -81.70169265833098393, -1.195345686084333225 ) ) ;
#37001 = EDGE_CURVE ( 'NONE', #56208, #42344, #52167, .T. ) ;
#37002 = TOROIDAL_SURFACE ( 'NONE', #21901, 17.50000000000000000, 5.000000000000000000 ) ;
#37003 = CARTESIAN_POINT ( 'NONE',  ( 2.005614507304999794, -80.09841179485169960, -10.84800649278999884 ) ) ;
#37004 = CARTESIAN_POINT ( 'NONE',  ( -11.00000000000000000, -79.19999999999998863, 0.000000000000000000 ) ) ;
#37005 = ORIENTED_EDGE ( 'NONE', *, *, #55170, .F. ) ;
#37006 = ORIENTED_EDGE ( 'NONE', *, *, #18945, .T. ) ;
#37007 = CARTESIAN_POINT ( 'NONE',  ( -0.9780501945912999373, -81.66710460546799766, -1.026390372485000091 ) ) ;
#37008 = ORIENTED_EDGE ( 'NONE', *, *, #18893, .F. ) ;
#37009 = ORIENTED_EDGE ( 'NONE', *, *, #8705, .T. ) ;
#37010 = CARTESIAN_POINT ( 'NONE',  ( -0.4701041210474999898, -16.99203065576000071, 12.54901038416000070 ) ) ;
#37011 = AXIS2_PLACEMENT_3D ( 'NONE', #56609, #33580, #46320 ) ;
#37012 = CARTESIAN_POINT ( 'NONE',  ( -3.321932689531000182, -80.44999999999998863, -10.22385755016999909 ) ) ;
#37013 = DIRECTION ( 'NONE',  ( 1.000000000000000000, 0.000000000000000000, 0.000000000000000000 ) ) ;
#37014 = CARTESIAN_POINT ( 'NONE',  ( -3.292147582310161802, -81.62916665243866987, 1.011281930930018058 ) ) ;
#37015 = ADVANCED_FACE ( 'NONE', ( #3231 ), #51021, .F. ) ;
#37016 = AXIS2_PLACEMENT_3D ( 'NONE', #36986, #28705, #6275 ) ;
#37017 = CARTESIAN_POINT ( 'NONE',  ( -9.896988620242000323, -79.33326001420199702, -1.580285165976000217 ) ) ;
#37018 = CARTESIAN_POINT ( 'NONE',  ( 5.660329970366285046, -78.27756882288660734, -7.317403316748722020 ) ) ;
#37019 = CARTESIAN_POINT ( 'NONE',  ( -1.250000000000000000, -55.54999999966999980, -12.00000000000000000 ) ) ;
#37020 = ORIENTED_EDGE ( 'NONE', *, *, #19155, .F. ) ;
#37021 = ORIENTED_EDGE ( 'NONE', *, *, #21413, .T. ) ;
#37022 = DIRECTION ( 'NONE',  ( 0.000000000000000000, -1.000000000000000000, 0.000000000000000000 ) ) ;
#37023 = CARTESIAN_POINT ( 'NONE',  ( -6.000000000000000000, -81.19999999999998863, 0.000000000000000000 ) ) ;
#37024 = CARTESIAN_POINT ( 'NONE',  ( 0.6295237254636211199, -81.33333333333334281, 1.092232985442824322 ) ) ;
#37025 = DIRECTION ( 'NONE',  ( 0.000000000000000000, 1.000000000000000000, 0.000000000000000000 ) ) ;
#37026 = CARTESIAN_POINT ( 'NONE',  ( 7.890274420948999001, -78.97040150846099493, -5.649267206312000411 ) ) ;
#37027 = CARTESIAN_POINT ( 'NONE',  ( 12.00000000000000000, -55.54999999966999980, 0.000000000000000000 ) ) ;
#37028 = CARTESIAN_POINT ( 'NONE',  ( 2.410958077658777565, -85.88312199482444953, 3.074828045483646743 ) ) ;
#37029 = CARTESIAN_POINT ( 'NONE',  ( -1.316656843623999817, -77.94825864453000008, -12.73088833989999991 ) ) ;
#37030 = CARTESIAN_POINT ( 'NONE',  ( 0.5538255850406000880, -80.86005058297999426, -1.485824439479999981 ) ) ;
#37031 = ADVANCED_FACE ( 'NONE', ( #53986 ), #30355, .T. ) ;
#37032 = CARTESIAN_POINT ( 'NONE',  ( -12.92181194099999963, -20.24351820077000141, -2.062502994258999856 ) ) ;
#37033 = CARTESIAN_POINT ( 'NONE',  ( 1.961420010778000211, -79.76473784880299434, 3.685436439494999661 ) ) ;
#37035 = VECTOR ( 'NONE', #918, 1000.000000000000000 ) ;
#37034 = CARTESIAN_POINT ( 'NONE',  ( 11.14639666075000157, -81.00452969028360428, -1.632917082138999776 ) ) ;
#37036 = CARTESIAN_POINT ( 'NONE',  ( -3.140974612311405512, -76.69583333333332575, 11.68767212001977640 ) ) ;
#37037 = CARTESIAN_POINT ( 'NONE',  ( -11.75023268171679725, -76.70812393556080622, -1.278857244370948498 ) ) ;
#37038 = CARTESIAN_POINT ( 'NONE',  ( -2.502884433417999599, -81.52455496681199065, 2.513390501795000009 ) ) ;
#37039 = CARTESIAN_POINT ( 'NONE',  ( 9.596002108778145967, -78.20208333333333428, 7.374560639699002884 ) ) ;
#37040 = DIRECTION ( 'NONE',  ( 0.000000000000000000, -1.000000000000000000, 0.000000000000000000 ) ) ;
#37041 = CARTESIAN_POINT ( 'NONE',  ( -3.370587613551000228, -1.795626005361000033, 0.9429417476038000068 ) ) ;
#37042 = DIRECTION ( 'NONE',  ( -1.000000000000000000, 0.000000000000000000, 0.000000000000000000 ) ) ;
#37043 = ORIENTED_EDGE ( 'NONE', *, *, #16332, .F. ) ;
#37044 = CARTESIAN_POINT ( 'NONE',  ( -10.71369944335147117, -78.22083333333330302, -2.879226727952084453 ) ) ;
#37045 = CARTESIAN_POINT ( 'NONE',  ( 7.387512494710278155, -60.21532333328941888, -8.150146600852353984 ) ) ;
#37046 = PLANE ( 'NONE',  #21147 ) ;
#37047 = CARTESIAN_POINT ( 'NONE',  ( 9.639239310942999239, -79.09126715714099021, 1.474640406829000217 ) ) ;
#37048 = CARTESIAN_POINT ( 'NONE',  ( -1.264141272797000060, -77.56525730074000080, -12.95149364859999963 ) ) ;
#37049 = CARTESIAN_POINT ( 'NONE',  ( -1.743222555440693489, -79.48802005694665240, 10.60902930704550506 ) ) ;
#37050 = AXIS2_PLACEMENT_3D ( 'NONE', #42591, #38143, #42881 ) ;
#37051 = DIRECTION ( 'NONE',  ( 0.000000000000000000, 1.000000000000000000, 0.000000000000000000 ) ) ;
#37052 = CARTESIAN_POINT ( 'NONE',  ( 11.23127327872411207, -78.47254254513119065, 3.450269100463493999 ) ) ;
#37053 = CIRCLE ( 'NONE', #16341, 1.250000000000000444 ) ;
#37054 = CYLINDRICAL_SURFACE ( 'NONE', #18417, 10.75000000000000000 ) ;
#37055 = CARTESIAN_POINT ( 'NONE',  ( 8.142057126146999835, -77.86840244345297890, -7.798273688473000398 ) ) ;
#37056 = CARTESIAN_POINT ( 'NONE',  ( -3.815503583757167139, -76.29810812315825785, -11.11946675543801177 ) ) ;
#37057 = CARTESIAN_POINT ( 'NONE',  ( 0.1975732027802999946, -81.48815384203000178, -1.493273510172999918 ) ) ;
#37058 = LINE ( 'NONE', #13746, #3152 ) ;
#37060 = CARTESIAN_POINT ( 'NONE',  ( -3.288006932140723038, -1.664267874433481786, -0.5432996569361712158 ) ) ;
#37059 = CARTESIAN_POINT ( 'NONE',  ( -1.646006820151000083, -82.62253637535398809, 3.605086534529000186 ) ) ;
#37061 = CARTESIAN_POINT ( 'NONE',  ( 0.000000000000000000, -87.15000000002500258, 0.000000000000000000 ) ) ;
#37062 = DIRECTION ( 'NONE',  ( 0.7071067811865474617, 0.000000000000000000, 0.7071067811865474617 ) ) ;
#37063 = CARTESIAN_POINT ( 'NONE',  ( -0.2315393795184000070, -80.04709616517300219, 1.298828366650000010 ) ) ;
#37064 = CARTESIAN_POINT ( 'NONE',  ( -5.721970631177883071, -77.18051251777001198, -9.113473785769789615 ) ) ;
#37065 = CARTESIAN_POINT ( 'NONE',  ( 6.365665562422999635, -79.13050366622999832, 10.17242851768000023 ) ) ;
#37066 = EDGE_CURVE ( 'NONE', #12948, #24745, #19116, .T. ) ;
#37067 = VERTEX_POINT ( 'NONE', #26504 ) ;
#37068 = CARTESIAN_POINT ( 'NONE',  ( -9.625846388754000671, -79.18507706297299364, -7.214584339064000318 ) ) ;
#37069 = DIRECTION ( 'NONE',  ( 1.000000000000000000, 0.000000000000000000, 0.000000000000000000 ) ) ;
#37070 = FACE_OUTER_BOUND ( 'NONE', #27345, .T. ) ;
#37071 = VERTEX_POINT ( 'NONE', #31517 ) ;
#37072 = CARTESIAN_POINT ( 'NONE',  ( 9.113984702984998520, -77.92925969475899706, 7.705244011730999709 ) ) ;
#37073 = AXIS2_PLACEMENT_3D ( 'NONE', #49404, #26355, #52950 ) ;
#37074 = VERTEX_POINT ( 'NONE', #3794 ) ;
#37075 = ORIENTED_EDGE ( 'NONE', *, *, #252, .F. ) ;
#37076 = CARTESIAN_POINT ( 'NONE',  ( -9.393203674808288994, -78.95833333333332860, 5.413904038987134015 ) ) ;
#37077 = EDGE_LOOP ( 'NONE', ( #7302, #39083, #48217, #2196 ) ) ;
#37078 = EDGE_CURVE ( 'NONE', #13032, #42169, #34788, .T. ) ;
#37079 = CARTESIAN_POINT ( 'NONE',  ( 1.378041103583000027, -80.65142343270998992, -3.268877919052000092 ) ) ;
#37080 = CARTESIAN_POINT ( 'NONE',  ( -8.768124086712999699, -55.64999999965999677, -7.919595949288999570 ) ) ;
#37081 = B_SPLINE_SURFACE_WITH_KNOTS ( 'NONE', 3, 3, ( 
 ( #46702, #1819, #19816, #20389, #38387, #11251, #56120, #16538, #7383, #30086, #33663, #47854, #56695, #3256, #52836, #34518, #52550, #12391, #12105, #56407, #29231, #21536, #25384, #43981, #56976, #7959, #2961, #7100, #29518, #47280, #48139, #42832, #15956, #43399, #29798 ),
 ( #11822, #33947, #57263, #7671, #30381, #51703, #6809, #20959, #15666, #38964, #43123, #52267, #24817, #16829, #51987, #20676, #21245, #25673, #2393, #34811, #43700, #39247, #48420, #25959, #3534, #11541, #47574, #25099, #2682, #38675, #16253, #34231, #9430, #36286, #12676 ),
 ( #4109, #17106, #16, #40424, #13844, #9136, #54308, #3820, #22111, #53127, #21822, #4997, #39825, #17396, #35093, #31843, #17994, #18292, #49885, #49287, #27419, #45455, #13552, #39541, #27121, #30952, #26827, #57547, #35381, #30667, #54011, #58133, #26250, #4409, #53406 ),
 ( #48991, #48705, #40120, #12956, #8248, #45161, #17698, #8536, #44265, #31544, #57839, #44557, #26530, #4710, #22709, #35688, #53715, #13252, #31245, #40722, #8838, #314, #44857, #22412, #35986, #49589, #886, #33006, #37743, #23002, #18870, #19163, #45753, #5286, #36574 ) ),
 .UNSPECIFIED., .F., .F., .F.,
 ( 4, 4 ),
 ( 4, 1, 1, 1, 1, 1, 1, 1, 1, 1, 1, 1, 1, 1, 1, 1, 1, 1, 1, 1, 1, 1, 1, 1, 1, 1, 1, 1, 1, 1, 1, 1, 4 ),
 ( -0.1772706441294000235, 1.177270644128999955 ),
 ( -0.01510644027126000107, 0.009441525169539000117, 0.03398949061033999797, 0.05853745605114000355, 0.08308542149195000115, 0.1076333869326999981, 0.1321813523735999862, 0.1567293178143999988, 0.1812772832552000113, 0.2058252486960000238, 0.2303732141367999808, 0.2549211795776000211, 0.2794691450183999781, 0.3040171104591999907, 0.3285650759000000032, 0.3531130413408000157, 0.3776610067816000282, 0.4022089722223999853, 0.4267569376631999978, 0.4513049031039999548, 0.4758528685447999673, 0.5004008339856000909, 0.5249487994264000479, 0.5494967648672000049, 0.5740447303079999619, 0.5985926957488000300, 0.6231406611895999870, 0.6476886266303999440, 0.6722365920712000120, 0.6967845575119999690, 0.7213325229527999261, 0.7458804883935999941, 0.7704284538343999511 ),
 .UNSPECIFIED. ) ;
#37082 = EDGE_LOOP ( 'NONE', ( #3401, #47324, #42572, #4922 ) ) ;
#37083 = DIRECTION ( 'NONE',  ( 0.000000000000000000, 1.000000000000000000, 0.000000000000000000 ) ) ;
#37084 = VERTEX_POINT ( 'NONE', #49566 ) ;
#37085 = CARTESIAN_POINT ( 'NONE',  ( 1.423904377506844954, -17.69487194798980667, 12.50677628656596774 ) ) ;
#37086 = FACE_OUTER_BOUND ( 'NONE', #12319, .T. ) ;
#37087 = CARTESIAN_POINT ( 'NONE',  ( -4.043785186575744817, -78.69999999999998863, -2.284879765406194974 ) ) ;
#37088 = AXIS2_PLACEMENT_3D ( 'NONE', #21869, #21587, #38726 ) ;
#37089 = DIRECTION ( 'NONE',  ( -0.9957542217973148757, 0.04890179604796068835, 0.07798810240099117441 ) ) ;
#37091 = EDGE_CURVE ( 'NONE', #31953, #23662, #40697, .T. ) ;
#37090 = CARTESIAN_POINT ( 'NONE',  ( 10.02574878253000001, -76.48484873660000005, 4.955627619753999902 ) ) ;
#37092 = CARTESIAN_POINT ( 'NONE',  ( -8.060180467139032245, -24.62064870851448006, 9.621709426110552243 ) ) ;
#37093 = VECTOR ( 'NONE', #15651, 1000.000000000000000 ) ;
#37094 = EDGE_CURVE ( 'NONE', #11445, #47767, #53494, .T. ) ;
#37095 = CARTESIAN_POINT ( 'NONE',  ( -7.682331425190000118, -59.56486430393999854, -10.04115011118999945 ) ) ;
#37096 = CARTESIAN_POINT ( 'NONE',  ( 7.931954819903705101, -78.80706091626400678, -4.759922961224686055 ) ) ;
#37097 = CARTESIAN_POINT ( 'NONE',  ( 6.575652215500655373, -76.52754343095485012, 9.737607018781540447 ) ) ;
#37098 = CARTESIAN_POINT ( 'NONE',  ( 9.027899509543001244, -77.73118667140099092, -3.021393903538999837 ) ) ;
#37099 = CARTESIAN_POINT ( 'NONE',  ( -0.1698911186725000078, -80.51950384102399028, 1.322768475116000042 ) ) ;
#37100 = CARTESIAN_POINT ( 'NONE',  ( -7.656495383265241372, -80.16412063804881427, -7.897723017437628279 ) ) ;
#37101 = CARTESIAN_POINT ( 'NONE',  ( -11.51674459389547955, -77.97731020001086222, -3.622551337281552097 ) ) ;
#37102 = CARTESIAN_POINT ( 'NONE',  ( -1.139821578811999858, -81.20342549782600372, 3.969799781000000305 ) ) ;
#37103 = CARTESIAN_POINT ( 'NONE',  ( -7.722699735758999928, -77.74431332859899157, -5.790782847811000167 ) ) ;
#37104 = CARTESIAN_POINT ( 'NONE',  ( -0.1834469635243000107, -79.61327907013999550, -1.236465612773999911 ) ) ;
#37105 = CARTESIAN_POINT ( 'NONE',  ( 0.1782616899984783287, -82.96393278609434674, 1.237108939223909410 ) ) ;
#37106 = CARTESIAN_POINT ( 'NONE',  ( 12.99510751537000353, -52.49705297113997204, 6.911973076623003642 ) ) ;
#37107 = CARTESIAN_POINT ( 'NONE',  ( -1.212057334841439848, -82.22243190943753177, 0.4356794552377592500 ) ) ;
#37108 = CARTESIAN_POINT ( 'NONE',  ( 12.00000000000000000, -78.64999999999999147, 0.000000000000000000 ) ) ;
#37109 = CARTESIAN_POINT ( 'NONE',  ( -10.30458248780999853, -60.56332651778999576, -7.636263891343999965 ) ) ;
#37110 = DIRECTION ( 'NONE',  ( -1.000000000000000000, 0.000000000000000000, 0.000000000000000000 ) ) ;
#37111 = CARTESIAN_POINT ( 'NONE',  ( 12.70457891999001987, -25.17873330329356918, -0.5105076820880790622 ) ) ;
#37112 = CARTESIAN_POINT ( 'NONE',  ( 1.435088794311236482, -79.57396092099332918, -0.4737081478796364431 ) ) ;
#37113 = CARTESIAN_POINT ( 'NONE',  ( -1.250000000000000000, -81.49999999999998579, 0.000000000000000000 ) ) ;
#37114 = CARTESIAN_POINT ( 'NONE',  ( 0.2672301082454999754, -3.175485789881999921, -3.475315813263000209 ) ) ;
#37115 = CARTESIAN_POINT ( 'NONE',  ( -8.114920487384752690, -24.82884529334158685, -9.847900218102966008 ) ) ;
#37116 = EDGE_CURVE ( 'NONE', #23736, #4408, #17246, .T. ) ;
#37117 = CARTESIAN_POINT ( 'NONE',  ( 0.9995835529977264988, -80.69791666666664298, -0.7681833999686417114 ) ) ;
#37118 = CARTESIAN_POINT ( 'NONE',  ( -9.098371730874241337, -77.49610366954293283, -5.890886578694863651 ) ) ;
#37119 = DIRECTION ( 'NONE',  ( 0.000000000000000000, 0.000000000000000000, 1.000000000000000000 ) ) ;
#37120 = B_SPLINE_CURVE_WITH_KNOTS ( 'NONE', 3,
 ( #51698, #20103, #56115, #37804, #1814, #2388 ),
 .UNSPECIFIED., .F., .F.,
 ( 4, 1, 1, 4 ),
 ( 0.000000000000000000, 0.3333333333333000081, 0.6666666666667000474, 1.000000000000000000 ),
 .UNSPECIFIED. ) ;
#37122 = CARTESIAN_POINT ( 'NONE',  ( 10.55657102546000203, -78.57793934531359525, -3.003801718854000047 ) ) ;
#37121 = CARTESIAN_POINT ( 'NONE',  ( 1.933650113854000097, -60.20786252993000431, 12.70909635757000089 ) ) ;
#37123 = DIRECTION ( 'NONE',  ( 1.000000000000000000, 0.000000000000000000, 0.000000000000000000 ) ) ;
#37124 = VERTEX_POINT ( 'NONE', #37131 ) ;
#37125 = CARTESIAN_POINT ( 'NONE',  ( 1.255715561858000040, -83.83707450217399071, -3.934676852947000203 ) ) ;
#37126 = CONICAL_SURFACE ( 'NONE', #11691, 0.6999999997695030007, 0.7853981633972997312 ) ;
#37127 = CARTESIAN_POINT ( 'NONE',  ( -11.40251694347999845, -80.77844001750112568, -0.2650480098012999997 ) ) ;
#37128 = CARTESIAN_POINT ( 'NONE',  ( -7.764005369055772654, -17.87720632479159022, -9.931049915325859345 ) ) ;
#37129 = CARTESIAN_POINT ( 'NONE',  ( -0.3926218265389190276, -81.60416666666667140, -1.460959015002473826 ) ) ;
#37130 = CARTESIAN_POINT ( 'NONE',  ( 8.196653188619999142, -77.71147621424999841, 7.657217973713000170 ) ) ;
#37131 = CARTESIAN_POINT ( 'NONE',  ( -1.164828128805999992E-14, -72.70000000000000284, -13.99999999999998401 ) ) ;
#37132 = CARTESIAN_POINT ( 'NONE',  ( -1.173259754689000234, -79.00834361351799373, -9.559114633834001395 ) ) ;
#37133 = CARTESIAN_POINT ( 'NONE',  ( 2.359810653458999763, -0.8958210303590000700, -3.059514552098999918 ) ) ;
#37134 = CARTESIAN_POINT ( 'NONE',  ( 3.778552491321000240, -78.99318692756679638, 0.000000000000000000 ) ) ;
#37135 = VECTOR ( 'NONE', #49448, 1000.000000000000000 ) ;
#37136 = CARTESIAN_POINT ( 'NONE',  ( -5.497476511162663115, -76.12291666666041579, 9.512467313639556110 ) ) ;
#37137 = ORIENTED_EDGE ( 'NONE', *, *, #33394, .F. ) ;
#37139 = AXIS2_PLACEMENT_3D ( 'NONE', #27008, #26711, #45926 ) ;
#37138 = CARTESIAN_POINT ( 'NONE',  ( -3.270833333333188264, -0.9791666666665451713, 0.3403392041390183587 ) ) ;
#37140 = CARTESIAN_POINT ( 'NONE',  ( -1.931736162948558544, -55.03329604256487073, -12.72978979887498063 ) ) ;
#37141 = CARTESIAN_POINT ( 'NONE',  ( -11.26045488449999965, -80.69595964897830243, 0.3336940576009999604 ) ) ;
#37142 = PLANE ( 'NONE',  #4522 ) ;
#37143 = VERTEX_POINT ( 'NONE', #9994 ) ;
#37144 = CARTESIAN_POINT ( 'NONE',  ( 12.50000000000000000, -60.04999999966999980, -1.250000000000000000 ) ) ;
#37145 = DIRECTION ( 'NONE',  ( -1.000000000000000000, 0.000000000000000000, 0.000000000000000000 ) ) ;
#37146 = VERTEX_POINT ( 'NONE', #27973 ) ;
#37147 = CARTESIAN_POINT ( 'NONE',  ( 2.739292792226000195, -77.90193793104199926, -11.85237552491999935 ) ) ;
#37148 = CARTESIAN_POINT ( 'NONE',  ( -10.25776238537000040, -77.96041360879199544, -4.245464761278999966 ) ) ;
#37149 = DIRECTION ( 'NONE',  ( 1.000000000000000000, 0.000000000000000000, 0.000000000000000000 ) ) ;
#37150 = VERTEX_POINT ( 'NONE', #46023 ) ;
#37151 = CARTESIAN_POINT ( 'NONE',  ( -10.36222501928999939, -55.57880030132999849, -7.631889976297999922 ) ) ;
#37152 = EDGE_CURVE ( 'NONE', #39513, #2249, #33099, .T. ) ;
#37153 = FILL_AREA_STYLE ('',( #9427 ) ) ;
#37154 = CARTESIAN_POINT ( 'NONE',  ( 1.841371367509999857, -80.03054692978699336, -9.592189096167999196 ) ) ;
#37155 = AXIS2_PLACEMENT_3D ( 'NONE', #39706, #7553, #20834 ) ;
#37156 = ORIENTED_EDGE ( 'NONE', *, *, #47000, .T. ) ;
#37157 = CARTESIAN_POINT ( 'NONE',  ( -3.500000000146000101, -0.7499999998540000101, 2.054632350152999929E-08 ) ) ;
#37158 = CARTESIAN_POINT ( 'NONE',  ( 7.624341764926000131, -23.26485149464000202, -10.42531124853000080 ) ) ;
#37159 = ADVANCED_FACE ( 'NONE', ( #46314 ), #14983, .F. ) ;
#37160 = ORIENTED_EDGE ( 'NONE', *, *, #13970, .F. ) ;
#37161 = CARTESIAN_POINT ( 'NONE',  ( -12.78037829248000001, -24.29316779390000036, -1.812823010630000065 ) ) ;
#37162 = CARTESIAN_POINT ( 'NONE',  ( -2.205007487985999770, -77.02370194988500884, 9.235565851336001941 ) ) ;
#37163 = FACE_OUTER_BOUND ( 'NONE', #23195, .T. ) ;
#37164 = CARTESIAN_POINT ( 'NONE',  ( -0.8423982081441719894, -80.16660507476834141, -0.9234063250311906890 ) ) ;
#37165 = CARTESIAN_POINT ( 'NONE',  ( -1.980610890452897399, -18.47926110518529441, -12.74374574607219834 ) ) ;
#37166 = CARTESIAN_POINT ( 'NONE',  ( 0.9999999970599000587, -81.20000000293998710, 7.000000017349999659 ) ) ;
#37167 = CARTESIAN_POINT ( 'NONE',  ( -2.759932835649922200, -86.17851881763701272, 3.725476775316761469 ) ) ;
#37168 = AXIS2_PLACEMENT_3D ( 'NONE', #38304, #55148, #50448 ) ;
#37169 = CARTESIAN_POINT ( 'NONE',  ( -9.233182284105000193, -77.12377164566318299, -0.8981109299819999281 ) ) ;
#37170 = EDGE_CURVE ( 'NONE', #52834, #32058, #42223, .T. ) ;
#37171 = CARTESIAN_POINT ( 'NONE',  ( 1.508773389166936818, -79.09704892049856539, -0.04912781361764535087 ) ) ;
#37172 = DIRECTION ( 'NONE',  ( -0.7071067811865474617, 0.000000000000000000, -0.7071067811865474617 ) ) ;
#37173 = ORIENTED_EDGE ( 'NONE', *, *, #17449, .T. ) ;
#37174 = CARTESIAN_POINT ( 'NONE',  ( 7.568503529865000523, -76.33963980947999062, 9.708412483427999007 ) ) ;
#37175 = CARTESIAN_POINT ( 'NONE',  ( -2.337444978021420372, -2.416471344608311256, -2.633833035016341473 ) ) ;
#37176 = CARTESIAN_POINT ( 'NONE',  ( 7.659225027833000077, -60.48266641633000518, -9.963489011801000217 ) ) ;
#37177 = CARTESIAN_POINT ( 'NONE',  ( -10.61911868076999887, -78.52435387434999825, -6.134606423928000041 ) ) ;
#37178 = CARTESIAN_POINT ( 'NONE',  ( -6.620362748380999918, -76.14579926823699907, -10.34376132320999986 ) ) ;
#37179 = DIRECTION ( 'NONE',  ( 0.7071067811865975328, -0.7071067811864976127, -4.006680953078982088E-09 ) ) ;
#37180 = CARTESIAN_POINT ( 'NONE',  ( 10.03846658019363502, -60.59367507117051588, -7.678639819092057728 ) ) ;
#37181 = CARTESIAN_POINT ( 'NONE',  ( 5.455390417367294020, -77.88749686968762376, 10.70987740487309559 ) ) ;
#37182 = CARTESIAN_POINT ( 'NONE',  ( -9.735611069857000643, -79.20864007176808741, 5.570995215215999607 ) ) ;
#37183 = EDGE_LOOP ( 'NONE', ( #1612, #56712, #56272, #52914 ) ) ;
#37184 = CARTESIAN_POINT ( 'NONE',  ( -0.7723712723579000405, -81.53758988526999474, -1.248632555533999877 ) ) ;
#37185 = CARTESIAN_POINT ( 'NONE',  ( 7.502868599214999712, -77.08946594610628722, -5.987157122012000343 ) ) ;
#37186 = CARTESIAN_POINT ( 'NONE',  ( 8.266617305338565203, -24.97234527442468632, 9.697375114818715502 ) ) ;
#37187 = CARTESIAN_POINT ( 'NONE',  ( 0.7681833999686413783, -82.82291666666667140, 0.9995835529977274980 ) ) ;
#37188 = CARTESIAN_POINT ( 'NONE',  ( -3.452134515939000003, -3.351393098589999564, 1.370126006426999998 ) ) ;
#37189 = CARTESIAN_POINT ( 'NONE',  ( -5.241653689492999924, -77.66540636460800329, -10.72196665943000049 ) ) ;
#37190 = CARTESIAN_POINT ( 'NONE',  ( -3.509962959857999554, -78.11162362607598197, 8.968465308258000590 ) ) ;
#37191 = CARTESIAN_POINT ( 'NONE',  ( 0.02495217850030486892, -76.07451107435575466, 11.74976244630887479 ) ) ;
#37192 = CARTESIAN_POINT ( 'NONE',  ( -2.772348231745000113, -79.13115782519599861, -10.55885653242000011 ) ) ;
#37193 = CARTESIAN_POINT ( 'NONE',  ( 12.00000000000000000, -76.54999999999999716, 0.000000000000000000 ) ) ;
#37194 = ORIENTED_EDGE ( 'NONE', *, *, #17429, .T. ) ;
#37195 = CYLINDRICAL_SURFACE ( 'NONE', #28534, 9.549999999999998934 ) ;
#37196 = CIRCLE ( 'NONE', #30605, 10.25000000000000000 ) ;
#37197 = CARTESIAN_POINT ( 'NONE',  ( 9.250030457523495286, -77.86058932347035011, 1.210900974741199621 ) ) ;
#37198 = CARTESIAN_POINT ( 'NONE',  ( 2.839805762151335511, -2.291666666666666519, 1.636761686205429278 ) ) ;
#37199 = CARTESIAN_POINT ( 'NONE',  ( -7.508490145779999736, -79.05550243411299505, -8.005410190140000992 ) ) ;
#37200 = CARTESIAN_POINT ( 'NONE',  ( -0.5656538306440472841, -79.18769777830807755, -1.114770703783219963 ) ) ;
#37201 = CARTESIAN_POINT ( 'NONE',  ( 3.245333607557999933, -76.22751663978100112, 12.07566914630000099 ) ) ;
#37202 = FACE_OUTER_BOUND ( 'NONE', #31164, .T. ) ;
#37203 = CARTESIAN_POINT ( 'NONE',  ( 7.756275637039999893, -17.77995361836999777, -10.15825999916999933 ) ) ;
#37204 = CYLINDRICAL_SURFACE ( 'NONE', #8902, 11.70000000000000107 ) ;
#37205 = VERTEX_POINT ( 'NONE', #27684 ) ;
#37206 = EDGE_CURVE ( 'NONE', #48292, #52871, #27611, .T. ) ;
#37207 = CARTESIAN_POINT ( 'NONE',  ( 8.769046271958000460, -78.47261268016799818, -7.066663249742999753 ) ) ;
#37208 = CARTESIAN_POINT ( 'NONE',  ( 12.70253230850417481, -17.02944272791701863, 0.9891673677968747525 ) ) ;
#37209 = CARTESIAN_POINT ( 'NONE',  ( -1.407171709420465211, -79.88541666666665719, 10.74999999999999467 ) ) ;
#37210 = CARTESIAN_POINT ( 'NONE',  ( 8.054632438192243171, -77.27014976278788083, 9.064962413430851740 ) ) ;
#37212 = CARTESIAN_POINT ( 'NONE',  ( -1.192707094028399473, -81.57616841835279331, 0.3740703197376714639 ) ) ;
#37211 = AXIS2_PLACEMENT_3D ( 'NONE', #16680, #57407, #47992 ) ;
#37213 = CARTESIAN_POINT ( 'NONE',  ( -3.655354238636269848, -77.00000000000000000, -8.765527374921106230 ) ) ;
#37214 = CARTESIAN_POINT ( 'NONE',  ( -0.4587696627765999735, -3.363384982433000214, -3.778272981138000031 ) ) ;
#37215 = CARTESIAN_POINT ( 'NONE',  ( -0.4521203515703999809, -78.17693822280000404, -1.227342538824000018 ) ) ;
#37216 = CARTESIAN_POINT ( 'NONE',  ( 10.47020627418438643, -79.27083333333335702, 2.813789756862283387 ) ) ;
#37217 = DIRECTION ( 'NONE',  ( -0.7071067811865474617, 0.000000000000000000, -0.7071067811865474617 ) ) ;
#37218 = CARTESIAN_POINT ( 'NONE',  ( -9.147655554837982095, -79.69791666666337449, -1.948585094003928431 ) ) ;
#37219 = ORIENTED_EDGE ( 'NONE', *, *, #9566, .F. ) ;
#37220 = ORIENTED_EDGE ( 'NONE', *, *, #35443, .F. ) ;
#37221 = CARTESIAN_POINT ( 'NONE',  ( -5.674993058560000136, -78.45643998579799927, -8.260872093916999503 ) ) ;
#37222 = CARTESIAN_POINT ( 'NONE',  ( 10.19409538785635405, -78.82440253168712729, -3.416663174436564088 ) ) ;
#37223 = EDGE_CURVE ( 'NONE', #35617, #15196, #5606, .T. ) ;
#37224 = ORIENTED_EDGE ( 'NONE', *, *, #24317, .F. ) ;
#37225 = CARTESIAN_POINT ( 'NONE',  ( 11.06808393496999976, -76.51144931706768659, 1.603559079323000347 ) ) ;
#37226 = CARTESIAN_POINT ( 'NONE',  ( 1.103369793158732737, -82.74687501615673568, 3.250074485770516830 ) ) ;
#37227 = CARTESIAN_POINT ( 'NONE',  ( -0.9218200799623778030, -80.32708333333337691, 1.199500263597266914 ) ) ;
#37228 = CARTESIAN_POINT ( 'NONE',  ( 7.634438871678000282, -60.54781730666999806, 10.30764054783999839 ) ) ;
#37229 = CARTESIAN_POINT ( 'NONE',  ( -10.47957108958864758, -76.59215066385610271, -6.245855599599564378 ) ) ;
#37230 = CARTESIAN_POINT ( 'NONE',  ( -11.61470386271144584, -77.53020205524934738, 2.935752974902272161 ) ) ;
#37231 = CARTESIAN_POINT ( 'NONE',  ( 9.376438147752001129, -79.46987249797800246, -6.156339679782000474 ) ) ;
#37232 = AXIS2_PLACEMENT_3D ( 'NONE', #24367, #28482, #55955 ) ;
#37233 = ADVANCED_FACE ( 'NONE', ( #5544 ), #581, .T. ) ;
#37234 = ORIENTED_EDGE ( 'NONE', *, *, #44074, .T. ) ;
#37235 = CARTESIAN_POINT ( 'NONE',  ( -10.20678250197623882, -24.23575784472138039, 7.770339463571165339 ) ) ;
#37236 = VERTEX_POINT ( 'NONE', #24140 ) ;
#37237 = CARTESIAN_POINT ( 'NONE',  ( 9.045497074381291469, -77.36695256801532139, 1.937463959486106946 ) ) ;
#37238 = LINE ( 'NONE', #42849, #15006 ) ;
#37239 = VECTOR ( 'NONE', #25329, 1000.000000000000000 ) ;
#37240 = B_SPLINE_CURVE_WITH_KNOTS ( 'NONE', 3,
 ( #13021, #17460, #8604, #21603, #26591, #4476, #44626, #13315, #53192, #49353 ),
 .UNSPECIFIED., .F., .F.,
 ( 4, 2, 2, 2, 4 ),
 ( 0.000000000000000000, 0.5000000000000089928, 0.6250000000000092149, 0.7500000000000095479, 1.000000000000000000 ),
 .UNSPECIFIED. ) ;
#37241 = FACE_OUTER_BOUND ( 'NONE', #9203, .T. ) ;
#37242 = CARTESIAN_POINT ( 'NONE',  ( -2.183112477083999803, -77.78351121986898420, 9.455407409464999802 ) ) ;
#37243 = CARTESIAN_POINT ( 'NONE',  ( -8.130813118010999929, -17.31476110167000115, 9.546856411653001473 ) ) ;
#37244 = CARTESIAN_POINT ( 'NONE',  ( 12.00000000000000000, -78.64999999999999147, 0.000000000000000000 ) ) ;
#37245 = CARTESIAN_POINT ( 'NONE',  ( 1.314530797355000225, -77.91099935146999655, -0.9595159925157999981 ) ) ;
#37246 = CARTESIAN_POINT ( 'NONE',  ( 2.775417664047000077, -81.17007046129099024, 3.115060498111000165 ) ) ;
#37247 = CARTESIAN_POINT ( 'NONE',  ( -10.62234821842000088, -78.90995737143398969, 2.617925641156000349 ) ) ;
#37248 = AXIS2_PLACEMENT_3D ( 'NONE', #24793, #1502, #33050 ) ;
#37249 = CARTESIAN_POINT ( 'NONE',  ( -7.620012114214000043, -23.20560398649000078, -10.53562503194000044 ) ) ;
#37250 = CARTESIAN_POINT ( 'NONE',  ( 12.71658889743999943, -60.11584477251999203, -1.931087888049999979 ) ) ;
#37251 = CARTESIAN_POINT ( 'NONE',  ( 1.096008713999000017, -84.26256135553198590, 3.373475151840000130 ) ) ;
#37252 = ORIENTED_EDGE ( 'NONE', *, *, #52776, .T. ) ;
#37253 = CARTESIAN_POINT ( 'NONE',  ( 12.50000000000000000, -55.55000000278000272, -1.750000000000000000 ) ) ;
#37254 = CARTESIAN_POINT ( 'NONE',  ( 0.6690176526880000640, -81.17289485077999700, 1.565960205386000004 ) ) ;
#37255 = CARTESIAN_POINT ( 'NONE',  ( -1.665424875009057004, -77.98744771326413172, 10.62927728148073214 ) ) ;
#37256 = CARTESIAN_POINT ( 'NONE',  ( 1.720939166139000109, -77.27055478756399509, -11.69973432676000158 ) ) ;
#37257 = CARTESIAN_POINT ( 'NONE',  ( -7.620012214426000519, -18.79439747922000237, 10.53562508625000049 ) ) ;
#37258 = CARTESIAN_POINT ( 'NONE',  ( -0.9644448879797564711, -78.30674845405408746, -0.8345157321849741017 ) ) ;
#37259 = CARTESIAN_POINT ( 'NONE',  ( 1.739823320037857002, -3.083851424189317569, 3.063316470677002190 ) ) ;
#37260 = CARTESIAN_POINT ( 'NONE',  ( 9.280195964196915170, -80.89241446635494981, 5.426651790427706068 ) ) ;
#37261 = CARTESIAN_POINT ( 'NONE',  ( 2.192362874646999860, -78.72289170186299145, -9.154492618432000128 ) ) ;
#37262 = CARTESIAN_POINT ( 'NONE',  ( 3.112536659741979239, -86.02148120184399716, -1.385790604991046671 ) ) ;
#37263 = CARTESIAN_POINT ( 'NONE',  ( 7.081068198472000752, -77.27840274250999641, 8.459326660559002065 ) ) ;
#37264 = CARTESIAN_POINT ( 'NONE',  ( -11.80208112488000083, -77.17229294297220576, -3.396125071686999952 ) ) ;
#37265 = CARTESIAN_POINT ( 'NONE',  ( 10.97353685322999972, -80.65494283066439607, 1.923198805891999985 ) ) ;
#37266 = VERTEX_POINT ( 'NONE', #23554 ) ;
#37267 = CARTESIAN_POINT ( 'NONE',  ( -9.050966799188000067, -55.64999999964999233, -7.919595949288999570 ) ) ;
#37268 = CYLINDRICAL_SURFACE ( 'NONE', #29539, 1.000000000000000000 ) ;
#37269 = CARTESIAN_POINT ( 'NONE',  ( -10.86658628928999981, -76.71825660736899977, -2.781249891074999869 ) ) ;
#37270 = CARTESIAN_POINT ( 'NONE',  ( 10.55657102546000026, -78.53748540510798648, -3.003801718854000047 ) ) ;
#37271 = CARTESIAN_POINT ( 'NONE',  ( -12.85144117163000033, -21.75472017028999971, 1.980464439859999981 ) ) ;
#37272 = CARTESIAN_POINT ( 'NONE',  ( -1.257344828728125696, -82.90104165186102136, 3.810723461902208342 ) ) ;
#37273 = CARTESIAN_POINT ( 'NONE',  ( 1.637338945544639213, -1.934839485303867290, 2.842420532304482883 ) ) ;
#37274 = DIRECTION ( 'NONE',  ( 0.000000000000000000, 1.000000000000000000, 0.000000000000000000 ) ) ;
#37275 = B_SPLINE_SURFACE_WITH_KNOTS ( 'NONE', 3, 3, ( 
 ( #21297, #43454, #17444, #29852, #16878, #26574, #22162, #52319, #12723, #43751, #3015, #3303, #57596, #39303, #57314, #25438, #53172, #39016, #52604, #44031, #26006, #11874, #48466, #34858, #3582, #21586, #8296, #57028, #48752, #40168, #47906, #16586, #7438, #34572, #31292 ),
 ( #27458, #14470, #50506, #22458, #28326, #14754, #33047, #10646, #28625, #46670, #42228, #39223, #39515, #57237, #47828, #30062, #48677, #53381, #12928, #39797, #16224, #25644, #7359, #8506, #25358, #20933, #20650, #17369, #43373, #17081, #43670, #57520, #21792, #30925, #35062 ),
 ( #34494, #30351, #35355, #38935, #57810, #53099, #3228, #30642, #12649, #44238, #56952, #52523, #48112, #48963, #21508, #12362, #21216, #16801, #7644, #34785, #48394, #43099, #8221, #2932, #26222, #3791, #25931, #2656, #52810, #38650, #16511, #52240, #56668, #34204, #12080 ),
 ( #11796, #7931, #29772, #43958, #3506, #22382, #36257, #4079, #27391, #40985, #18556, #14110, #54278, #32107, #40087, #13815, #27094, #27680, #23267, #45724, #5259, #18843, #36836, #40393, #14395, #53683, #31815, #17666, #35653, #13221, #31216, #58402, #49856, #49254, #8806 ) ),
 .UNSPECIFIED., .F., .F., .F.,
 ( 4, 4 ),
 ( 4, 1, 1, 1, 1, 1, 1, 1, 1, 1, 1, 1, 1, 1, 1, 1, 1, 1, 1, 1, 1, 1, 1, 1, 1, 1, 1, 1, 1, 1, 1, 1, 4 ),
 ( -0.1772706441294000235, 1.177270644128999955 ),
 ( 0.4993183012519999964, 0.5152713945944999985, 0.5312244879369000250, 0.5471775812793999716, 0.5631306746219000292, 0.5790837679642999447, 0.5950368613068000023, 0.6109899546492000288, 0.6269430479917000865, 0.6428961413342000331, 0.6588492346765999486, 0.6748023280191000062, 0.6907554213615000327, 0.7067085147039999793, 0.7226616080465000369, 0.7386147013889000634, 0.7545677947314000100, 0.7705208880737999255, 0.7864739814162999831, 0.8024270747588000408, 0.8183801681012000673, 0.8343332614437000139, 0.8502863547860999294, 0.8662394481285999870, 0.8821925414711000446, 0.8981456348135000711, 0.9140987281560000177, 0.9300518214983999332, 0.9460049148408999908, 0.9619580081833999374, 0.9779111015257999640, 0.9938641948683000216, 1.009817288211000141 ),
 .UNSPECIFIED. ) ;
#37276 = ADVANCED_FACE ( 'NONE', ( #9405 ), #18269, .F. ) ;
#37277 = CARTESIAN_POINT ( 'NONE',  ( -2.683170449497999765, -83.39569503318799093, -3.195412127327000196 ) ) ;
#37278 = CARTESIAN_POINT ( 'NONE',  ( 1.460959015002472494, -80.27083333333337123, 0.3926218265389233020 ) ) ;
#37279 = EDGE_CURVE ( 'NONE', #6154, #36787, #31820, .T. ) ;
#37280 = CARTESIAN_POINT ( 'NONE',  ( -1.250000000000000000, -76.50000000000000000, -0.5000000000000000000 ) ) ;
#37281 = AXIS2_PLACEMENT_3D ( 'NONE', #8212, #35646, #17659 ) ;
#37282 = CARTESIAN_POINT ( 'NONE',  ( 1.728979404161999911, -78.04192557611499126, 11.13281482770999986 ) ) ;
#37283 = CARTESIAN_POINT ( 'NONE',  ( 0.6544915521845998674, -81.23169436972999335, 1.531959166345999934 ) ) ;
#37284 = DIRECTION ( 'NONE',  ( 1.000000000000000000, 0.000000000000000000, 0.000000000000000000 ) ) ;
#37285 = CARTESIAN_POINT ( 'NONE',  ( -7.958776492183998741, -24.47699850274999989, 9.723157982400998378 ) ) ;
#37286 = CARTESIAN_POINT ( 'NONE',  ( 0.4637052088425716589, -81.60016793862807560, 1.437828183278014649 ) ) ;
#37287 = CARTESIAN_POINT ( 'NONE',  ( 0.000000000000000000, -77.04999999999999716, -9.400000000000000355 ) ) ;
#37288 = CARTESIAN_POINT ( 'NONE',  ( -7.599722349268615673, -80.16297892688153581, -7.602663284551876011 ) ) ;
#37289 = DIRECTION ( 'NONE',  ( 0.000000000000000000, -1.000000000000000000, 0.000000000000000000 ) ) ;
#37290 = CARTESIAN_POINT ( 'NONE',  ( -1.310679582531386389, -77.94166666666667709, -0.7554284705563492075 ) ) ;
#37291 = ORIENTED_EDGE ( 'NONE', *, *, #5679, .F. ) ;
#37292 = CARTESIAN_POINT ( 'NONE',  ( -0.2634504916890236803, -81.70857297640610284, -1.222512182397711200 ) ) ;
#37293 =( NAMED_UNIT ( * ) SI_UNIT ( $, .STERADIAN. ) SOLID_ANGLE_UNIT ( ) );
#37294 = CARTESIAN_POINT ( 'NONE',  ( -7.286644543156999276, -79.52644859181400250, -8.282906837769999697 ) ) ;
#37295 = CARTESIAN_POINT ( 'NONE',  ( 0.000000000000000000, -81.79999999999998295, -4.100000000000000533 ) ) ;
#37296 = ORIENTED_EDGE ( 'NONE', *, *, #52241, .T. ) ;
#37297 = EDGE_LOOP ( 'NONE', ( #36645, #9139, #11858, #22465 ) ) ;
#37298 = CARTESIAN_POINT ( 'NONE',  ( -1.026725001539000148, -82.16323083927800042, -0.9776035232744000325 ) ) ;
#37299 = ADVANCED_FACE ( 'NONE', ( #45730 ), #55230, .F. ) ;
#37300 = ORIENTED_EDGE ( 'NONE', *, *, #41443, .T. ) ;
#37301 = ORIENTED_EDGE ( 'NONE', *, *, #51094, .F. ) ;
#37302 = CARTESIAN_POINT ( 'NONE',  ( -0.3926218265389255779, -81.89583333334149984, 1.460959015002472494 ) ) ;
#37303 = DIRECTION ( 'NONE',  ( 0.000000000000000000, -1.000000000000000000, 0.000000000000000000 ) ) ;
#37304 = CARTESIAN_POINT ( 'NONE',  ( 0.000000000000000000, 0.000000000000000000, 0.000000000000000000 ) ) ;
#37305 = CARTESIAN_POINT ( 'NONE',  ( 0.7812709553989065636, -82.13020831715014936, -3.320429094668629677 ) ) ;
#37306 = CARTESIAN_POINT ( 'NONE',  ( 6.874531804813999614, -78.50581001420199811, -7.293035489291000317 ) ) ;
#37307 = CARTESIAN_POINT ( 'NONE',  ( 6.544128014875892241, -78.28754515060697372, -6.537337346629323420 ) ) ;
#37308 = CARTESIAN_POINT ( 'NONE',  ( -8.768124086549999419, -55.65000000488999632, 7.919595949288999570 ) ) ;
#37309 = EDGE_CURVE ( 'NONE', #48492, #6877, #48363, .T. ) ;
#37310 = ORIENTED_EDGE ( 'NONE', *, *, #26760, .F. ) ;
#37311 = ORIENTED_EDGE ( 'NONE', *, *, #11752, .F. ) ;
#37312 = FACE_OUTER_BOUND ( 'NONE', #18066, .T. ) ;
#37313 = CARTESIAN_POINT ( 'NONE',  ( 4.336551063001058637, -77.05429869360747830, -11.23466680206521850 ) ) ;
#37314 = CARTESIAN_POINT ( 'NONE',  ( 0.3926218265389159190, -79.35416666666668561, 1.460959015002474715 ) ) ;
#37315 = ADVANCED_FACE ( 'NONE', ( #47762 ), #39874, .T. ) ;
#37316 = DIRECTION ( 'NONE',  ( 0.000000000000000000, 0.000000000000000000, -1.000000000000000000 ) ) ;
#37317 = CARTESIAN_POINT ( 'NONE',  ( -9.626984307556000431, -78.25980578023599321, 1.221426423741999834 ) ) ;
#37318 = DIRECTION ( 'NONE',  ( 0.000000000000000000, -1.000000000000000000, 0.000000000000000000 ) ) ;
#37319 = CARTESIAN_POINT ( 'NONE',  ( 3.516302236083875599, -85.82247364775101062, 1.476714140108094542 ) ) ;
#37320 = CARTESIAN_POINT ( 'NONE',  ( -10.98749645531777830, -77.33354319426250356, -4.929334125398810329 ) ) ;
#37321 = B_SPLINE_SURFACE_WITH_KNOTS ( 'NONE', 3, 3, ( 
 ( #44846, #21238, #48694, #30369, #13543, #48411, #12945, #43691, #7, #7948, #31234, #30943, #44545, #17986, #48130, #49276, #3246, #4099, #57252, #52826, #16819, #34803, #28279, #46038, #50165, #19152, #1165, #37148, #5562, #27411, #50753, #9709, #45151, #14415, #27700 ),
 ( #23572, #41586, #31534, #4987, #55160, #36276, #14706, #10298, #5854, #45445, #27113, #23860, #18284, #41876, #1453, #37440, #18579, #55456, #9129, #49582, #22994, #54868, #4703, #41005, #40713, #27989, #54300, #13837, #596, #45742, #31834, #49877, #9421, #10011, #18864 ),
 ( #41295, #36568, #14128, #23285, #878, #36856, #32414, #50459, #33590, #24455, #6441, #20035, #33870, #51628, #1744, #2609, #24743, #46621, #42758, #56619, #55757, #51911, #42469, #51045, #2322, #20318, #20604, #11471, #29442, #2036, #38023, #38604, #16178, #56046, #34157 ),
 ( #15595, #19738, #32998, #10890, #10592, #47497, #11182, #7024, #25027, #28576, #29158, #47207, #38314, #24159, #43047, #56335, #37733, #42176, #15301, #15887, #33296, #51333, #28867, #46913, #55356, #37341, #50652, #37630, #27887, #24055, #14029, #18474, #27314, #32896, #9613 ) ),
 .UNSPECIFIED., .F., .F., .F.,
 ( 4, 4 ),
 ( 4, 1, 1, 1, 1, 1, 1, 1, 1, 1, 1, 1, 1, 1, 1, 1, 1, 1, 1, 1, 1, 1, 1, 1, 1, 1, 1, 1, 1, 1, 1, 1, 4 ),
 ( -0.1387574078320000237, 1.138757407831999968 ),
 ( 0.3340109127995999905, 0.3552311533231000129, 0.3764513938467000109, 0.3976716343701999778, 0.4188918748937999759, 0.4401121154172999983, 0.4613323559408000207, 0.4825525964644000187, 0.5037728369878999857, 0.5249930775114999282, 0.5462133180349999506, 0.5674335585586000041, 0.5886537990821000266, 0.6098740396056000490, 0.6310942801291999915, 0.6523145206527000139, 0.6735347611762999565, 0.6947550016997999789, 0.7159752422233999214, 0.7371954827468999438, 0.7584157232704000773, 0.7796359637940000198, 0.8008562043175000422, 0.8220764448410999847, 0.8432966853646000072, 0.8645169258881999497, 0.8857371664116999721, 0.9069574069351999945, 0.9281776474588000481, 0.9493978879823000705, 0.9706181285059000130, 0.9918383690294000354, 1.013058609553000089 ),
 .UNSPECIFIED. ) ;
#37322 = CARTESIAN_POINT ( 'NONE',  ( -0.8049692409160000839, -81.21779532827999049, -1.105758127848999850 ) ) ;
#37323 = VECTOR ( 'NONE', #5533, 999.9999999999998863 ) ;
#37324 = CARTESIAN_POINT ( 'NONE',  ( -12.49168433579000137, -23.29849137228000444, -1.667916687244999974 ) ) ;
#37325 = CARTESIAN_POINT ( 'NONE',  ( 0.3436388712391041933, -76.57261070421138527, 11.74524196079921623 ) ) ;
#37326 = CARTESIAN_POINT ( 'NONE',  ( -3.809107967971999908, -78.61343171100860161, 1.220272423491999936 ) ) ;
#37327 = CARTESIAN_POINT ( 'NONE',  ( 11.02326530841000007, -81.09238336756219212, 1.187788371667000131 ) ) ;
#37328 = DIRECTION ( 'NONE',  ( -0.7071067811864976127, 0.7071067811865975328, 1.669581477361993759E-09 ) ) ;
#37329 = CARTESIAN_POINT ( 'NONE',  ( 12.50000000000000000, -55.54999999966999980, 0.000000000000000000 ) ) ;
#37330 = CARTESIAN_POINT ( 'NONE',  ( 2.359605203086000191, -81.16380496681199475, 2.648362822824000151 ) ) ;
#37332 = CARTESIAN_POINT ( 'NONE',  ( -1.320128238786999919, -78.73322125463400312, -0.1893081677438999966 ) ) ;
#37331 = DIRECTION ( 'NONE',  ( 0.000000000000000000, 1.000000000000000000, 0.000000000000000000 ) ) ;
#37333 = EDGE_CURVE ( 'NONE', #57192, #39540, #37053, .T. ) ;
#37334 = CARTESIAN_POINT ( 'NONE',  ( 7.374560639698954922, -78.22291666666667709, 9.596002108778179718 ) ) ;
#37335 = LINE ( 'NONE', #15193, #32545 ) ;
#37336 = CARTESIAN_POINT ( 'NONE',  ( 3.190249742999000215, -2.021431841278999553, -2.075671974272999876 ) ) ;
#37337 = CIRCLE ( 'NONE', #47732, 1.750000000000000444 ) ;
#37338 = FACE_OUTER_BOUND ( 'NONE', #14572, .T. ) ;
#37339 = ORIENTED_EDGE ( 'NONE', *, *, #11017, .T. ) ;
#37340 = CARTESIAN_POINT ( 'NONE',  ( -2.730984724245073103, -3.499999999999999556, -1.917875800217215598 ) ) ;
#37341 = CARTESIAN_POINT ( 'NONE',  ( -9.866499134202999954, -78.07867141381099430, 5.775311262588999739 ) ) ;
#37342 = CYLINDRICAL_SURFACE ( 'NONE', #35453, 1.750000000000001332 ) ;
#37343 = CARTESIAN_POINT ( 'NONE',  ( 1.799475295154000065, -58.55083378327000077, 12.69619287811999797 ) ) ;
#37344 = CARTESIAN_POINT ( 'NONE',  ( 1.750000000001000089, -55.54999998977000075, -12.56594317853999954 ) ) ;
#37345 = CARTESIAN_POINT ( 'NONE',  ( 10.44234272621953608, -79.36931961362199672, 2.576411631240690614 ) ) ;
#37346 = CARTESIAN_POINT ( 'NONE',  ( -2.437266298365000416, -79.27423998579799047, 9.542290714110000849 ) ) ;
#37347 = EDGE_CURVE ( 'NONE', #35775, #2137, #56029, .T. ) ;
#37348 = CYLINDRICAL_SURFACE ( 'NONE', #8030, 14.00000000000000000 ) ;
#37349 = CARTESIAN_POINT ( 'NONE',  ( -10.99144026735999979, -77.69704419146098928, -2.508820398717999556 ) ) ;
#37350 = CARTESIAN_POINT ( 'NONE',  ( -1.427775756650000005, -82.36594923580300076, -0.2438566963919999719 ) ) ;
#37351 = CARTESIAN_POINT ( 'NONE',  ( 7.642160924865000204, -22.78461666469000235, -10.55911395186000057 ) ) ;
#37352 = DIRECTION ( 'NONE',  ( -0.7071067811865475727, 0.000000000000000000, -0.7071067811865475727 ) ) ;
#37354 = CARTESIAN_POINT ( 'NONE',  ( 7.588757936995927963E-07, -80.21583927563050054, -10.98470495943546688 ) ) ;
#37353 = CARTESIAN_POINT ( 'NONE',  ( -3.242523719075999900, -85.74904717229100015, 2.278511022525999685 ) ) ;
#37355 = CARTESIAN_POINT ( 'NONE',  ( -6.053394164830000257, -79.70045194988499304, -7.392643757108000813 ) ) ;
#37356 = LINE ( 'NONE', #20240, #48724 ) ;
#37357 = CARTESIAN_POINT ( 'NONE',  ( -0.9004272109156999937, -80.59283502236499430, 0.9642496934733999492 ) ) ;
#37358 = DIRECTION ( 'NONE',  ( 0.000000000000000000, 1.000000000000000000, 0.000000000000000000 ) ) ;
#37359 = CARTESIAN_POINT ( 'NONE',  ( -9.199999999999999289, -80.59999999999999432, 0.000000000000000000 ) ) ;
#37360 = ORIENTED_EDGE ( 'NONE', *, *, #11674, .T. ) ;
#37361 = VERTEX_POINT ( 'NONE', #20591 ) ;
#37362 = CARTESIAN_POINT ( 'NONE',  ( 11.92746894621999942, -79.39426247890499155, 1.562891678063999867 ) ) ;
#37363 = FACE_OUTER_BOUND ( 'NONE', #46375, .T. ) ;
#37364 = LINE ( 'NONE', #19372, #5813 ) ;
#37365 = ORIENTED_EDGE ( 'NONE', *, *, #57193, .T. ) ;
#37366 = CARTESIAN_POINT ( 'NONE',  ( -9.654076420390000024, -78.17342353357300055, -7.016716533807999312 ) ) ;
#37367 = ORIENTED_EDGE ( 'NONE', *, *, #2194, .F. ) ;
#37368 = AXIS2_PLACEMENT_3D ( 'NONE', #8501, #43368, #26496 ) ;
#37369 = ORIENTED_EDGE ( 'NONE', *, *, #31484, .T. ) ;
#37371 = ORIENTED_EDGE ( 'NONE', *, *, #48114, .T. ) ;
#37370 = AXIS2_PLACEMENT_3D ( 'NONE', #56587, #56881, #57158 ) ;
#37372 = CIRCLE ( 'NONE', #26027, 0.5000000000000004441 ) ;
#37373 = CARTESIAN_POINT ( 'NONE',  ( 3.225423266044999959, -79.32866876341660145, -1.476890314707000051 ) ) ;
#37374 = CARTESIAN_POINT ( 'NONE',  ( 9.499988113994666250, -79.15199854361453902, 0.2409522322386896676 ) ) ;
#37375 = ORIENTED_EDGE ( 'NONE', *, *, #57042, .F. ) ;
#37376 = CARTESIAN_POINT ( 'NONE',  ( 1.160213112257555412, -82.81967442626978482, -0.4651854077409782739 ) ) ;
#37377 = AXIS2_PLACEMENT_3D ( 'NONE', #44372, #31946, #27228 ) ;
#37378 = CARTESIAN_POINT ( 'NONE',  ( -2.962050278768000311, -2.514727077435000346, 1.672015632479999958 ) ) ;
#37379 = ORIENTED_EDGE ( 'NONE', *, *, #52968, .T. ) ;
#37380 = CARTESIAN_POINT ( 'NONE',  ( 10.47020627418439531, -80.72916666666667140, -2.813789756862242974 ) ) ;
#37381 = CARTESIAN_POINT ( 'NONE',  ( -9.161389328174658786, -77.37563928610997266, -3.065743153103684726 ) ) ;
#37382 = DIRECTION ( 'NONE',  ( 0.000000000000000000, 0.7071067811866525998, -0.7071067811864425456 ) ) ;
#37383 = CARTESIAN_POINT ( 'NONE',  ( -10.74969614785317340, -80.09697912524651997, 0.4764947645818390920 ) ) ;
#37384 = CARTESIAN_POINT ( 'NONE',  ( 9.583411031200000707, -78.01256708535665041, 1.526087275887999750 ) ) ;
#37385 = CARTESIAN_POINT ( 'NONE',  ( -5.007180289739999068, -76.67804699982200134, 10.00009952528999868 ) ) ;
#37386 = CARTESIAN_POINT ( 'NONE',  ( 9.396085398178598780, -77.10208333333331154, 7.220923959705271677 ) ) ;
#37387 = CARTESIAN_POINT ( 'NONE',  ( -7.655555357438999842, -56.02204592290999585, -10.38646360829000059 ) ) ;
#37388 = CARTESIAN_POINT ( 'NONE',  ( -5.105871269591521155, -78.67859004320752092, -7.713068480137897254 ) ) ;
#37389 = CARTESIAN_POINT ( 'NONE',  ( 6.619314962793000134, -77.25773501420199807, -6.690398925867999225 ) ) ;
#37390 = DIRECTION ( 'NONE',  ( -1.000000000000000000, 0.000000000000000000, 0.000000000000000000 ) ) ;
#37391 = CARTESIAN_POINT ( 'NONE',  ( 17.50000000000000000, -26.93717104351999936, 4.519611351839000330E-10 ) ) ;
#37392 = CARTESIAN_POINT ( 'NONE',  ( -12.65372179304999811, -58.55064713745999683, -1.750000000000000000 ) ) ;
#37393 = CARTESIAN_POINT ( 'NONE',  ( 2.545076011845999631, -82.04517549782597996, -3.252891696798999810 ) ) ;
#37394 = DIRECTION ( 'NONE',  ( 0.000000000000000000, -1.000000000000000000, 0.000000000000000000 ) ) ;
#37395 = DIRECTION ( 'NONE',  ( 0.000000000000000000, 1.000000000000000000, 0.000000000000000000 ) ) ;
#37396 = EDGE_CURVE ( 'NONE', #47003, #34794, #15578, .T. ) ;
#37397 = CARTESIAN_POINT ( 'NONE',  ( 0.2409842076378775344, -82.95976104365308856, 1.226430088683852615 ) ) ;
#37398 = DIRECTION ( 'NONE',  ( -0.7071067811865969777, 1.533578360404995178E-11, -0.7071067811864980568 ) ) ;
#37399 = CARTESIAN_POINT ( 'NONE',  ( -12.50000000000000000, -18.75000000310999937, 1.750000000000000000 ) ) ;
#37400 = CARTESIAN_POINT ( 'NONE',  ( -9.549999999999998934, -80.99999999999998579, 0.000000000000000000 ) ) ;
#37401 = CARTESIAN_POINT ( 'NONE',  ( 12.54435915805012769, -23.52412882219289969, 1.733925320388620683 ) ) ;
#37402 = CARTESIAN_POINT ( 'NONE',  ( -12.00000000000000000, -77.29999999999999716, 0.000000000000000000 ) ) ;
#37403 = CARTESIAN_POINT ( 'NONE',  ( -1.382886570147999983, -24.63098219832000169, -12.65982054476000052 ) ) ;
#37404 = DIRECTION ( 'NONE',  ( 0.000000000000000000, 0.7071067811865475727, -0.7071067811865475727 ) ) ;
#37405 = CARTESIAN_POINT ( 'NONE',  ( -9.646692012709999986, -78.49984415034599294, 1.218660606027000215 ) ) ;
#37406 = CARTESIAN_POINT ( 'NONE',  ( 12.59682790092999838, -23.38734115225999943, 1.801645751184999922 ) ) ;
#37407 = CARTESIAN_POINT ( 'NONE',  ( -1.217465845835394411, -80.52083333333330017, -0.3271848554491003647 ) ) ;
#37408 = CIRCLE ( 'NONE', #27959, 14.00000000000000000 ) ;
#37409 = CARTESIAN_POINT ( 'NONE',  ( 11.65296779515999859, -77.59787174848798941, -3.873515295708999773 ) ) ;
#37410 = DIRECTION ( 'NONE',  ( -0.7071067811865475727, 0.000000000000000000, -0.7071067811865475727 ) ) ;
#37411 = CARTESIAN_POINT ( 'NONE',  ( -9.254388464354001087, -79.80752053325198858, 5.469807505829999528 ) ) ;
#37412 = CARTESIAN_POINT ( 'NONE',  ( 10.85336555362000155, -76.97361153625999464, -4.603040914152999541 ) ) ;
#37413 = EDGE_LOOP ( 'NONE', ( #1163, #30397, #41691, #47756, #56277 ) ) ;
#37414 = AXIS2_PLACEMENT_3D ( 'NONE', #17211, #35199, #48248 ) ;
#37415 = EDGE_CURVE ( 'NONE', #35080, #51790, #14421, .T. ) ;
#37416 = CARTESIAN_POINT ( 'NONE',  ( 2.998912544640999656, -83.95732450217400356, -2.839899128081999624 ) ) ;
#37417 = CARTESIAN_POINT ( 'NONE',  ( 9.852601822233998163, -80.56860390147939199, 5.745770655690999540 ) ) ;
#37418 = VECTOR ( 'NONE', #31186, 1000.000000000000114 ) ;
#37419 = CARTESIAN_POINT ( 'NONE',  ( 8.743304200629554046, -78.32361866804367878, -3.019380310087202535 ) ) ;
#37420 = DIRECTION ( 'NONE',  ( -0.7071067811865475727, 0.000000000000000000, 0.7071067811865475727 ) ) ;
#37421 = CARTESIAN_POINT ( 'NONE',  ( -9.998780405325002008, -77.43911278423200883, -5.083552005986999411 ) ) ;
#37422 = CARTESIAN_POINT ( 'NONE',  ( 9.332529440374916163, -78.90131187205814456, 0.09866230578322067457 ) ) ;
#37423 = CARTESIAN_POINT ( 'NONE',  ( 4.155310858692000231, -78.55356234745399036, -8.688302574878001394 ) ) ;
#37424 = VECTOR ( 'NONE', #14917, 1000.000000000000227 ) ;
#37425 = CARTESIAN_POINT ( 'NONE',  ( -2.682853591918000102, -83.42707394314300018, -3.195129404054000144 ) ) ;
#37426 = CARTESIAN_POINT ( 'NONE',  ( -3.799999999999999822, 0.000000000000000000, 0.000000000000000000 ) ) ;
#37427 = CARTESIAN_POINT ( 'NONE',  ( 0.000000000000000000, -7.000000000000000000, 0.000000000000000000 ) ) ;
#37428 = ORIENTED_EDGE ( 'NONE', *, *, #6956, .T. ) ;
#37429 = CARTESIAN_POINT ( 'NONE',  ( -0.9849936891751999157, -80.81635039299281686, -11.22225356808999841 ) ) ;
#37430 = CARTESIAN_POINT ( 'NONE',  ( 11.21020301114814011, -75.92468345066387769, -3.640793229887494764 ) ) ;
#37431 = EDGE_CURVE ( 'NONE', #18217, #8616, #40812, .T. ) ;
#37432 = ORIENTED_EDGE ( 'NONE', *, *, #5903, .F. ) ;
#37433 = CARTESIAN_POINT ( 'NONE',  ( -0.5409299486741000473, -79.04257420652599819, 1.218996123443000013 ) ) ;
#37434 = EDGE_CURVE ( 'NONE', #4000, #8688, #7818, .T. ) ;
#37435 = CARTESIAN_POINT ( 'NONE',  ( 2.500028546529174278, -77.64653440364209303, -8.986588875504750717 ) ) ;
#37436 = CARTESIAN_POINT ( 'NONE',  ( 0.3244733924317961260, -80.74656484181741689, -1.210953765918606706 ) ) ;
#37437 = ORIENTED_EDGE ( 'NONE', *, *, #34403, .F. ) ;
#37438 = B_SPLINE_CURVE_WITH_KNOTS ( 'NONE', 3,
 ( #43507, #30192, #7778, #39064, #34336, #43220 ),
 .UNSPECIFIED., .F., .F.,
 ( 4, 1, 1, 4 ),
 ( 0.000000000000000000, 0.3333333333333000081, 0.6666666666667000474, 1.000000000000000000 ),
 .UNSPECIFIED. ) ;
#37439 = CARTESIAN_POINT ( 'NONE',  ( -12.14750708673999924, -78.25461903155100174, 0.6485384821269000177 ) ) ;
#37440 = CARTESIAN_POINT ( 'NONE',  ( -4.644564950407000126, -77.58407284559099537, -10.20464596076999975 ) ) ;
#37441 = CARTESIAN_POINT ( 'NONE',  ( -1.667961445601999992, -20.25199022618999933, 12.58338334675000070 ) ) ;
#37442 = ORIENTED_EDGE ( 'NONE', *, *, #14909, .T. ) ;
#37443 = ORIENTED_EDGE ( 'NONE', *, *, #5363, .F. ) ;
#37444 = DIRECTION ( 'NONE',  ( 0.000000000000000000, 0.7071067811866525998, -0.7071067811864425456 ) ) ;
#37445 = CARTESIAN_POINT ( 'NONE',  ( 1.739862777674999972, -79.19090020592499002, 9.611119481339999382 ) ) ;
#37446 = ORIENTED_EDGE ( 'NONE', *, *, #48486, .F. ) ;
#37447 = CARTESIAN_POINT ( 'NONE',  ( 12.61112375829999976, -55.58433928934000079, 1.798929377343999825 ) ) ;
#37448 = DIRECTION ( 'NONE',  ( 0.000000000000000000, -1.000000000000000000, 0.000000000000000000 ) ) ;
#37449 = ORIENTED_EDGE ( 'NONE', *, *, #37684, .F. ) ;
#37450 = CARTESIAN_POINT ( 'NONE',  ( -1.595587217727999940, -77.79014102152999044, -0.4130859425818000363 ) ) ;
#37451 = ADVANCED_FACE ( 'NONE', ( #52181 ), #27389, .F. ) ;
#37452 = CARTESIAN_POINT ( 'NONE',  ( -9.061228178001998756, -77.53399415034598974, -2.837532765875999896 ) ) ;
#37453 = CIRCLE ( 'NONE', #41211, 9.750000000000000000 ) ;
#37454 = CARTESIAN_POINT ( 'NONE',  ( -0.4317206087502349354, -80.19718752668565287, -1.173039634006793452 ) ) ;
#37455 = CARTESIAN_POINT ( 'NONE',  ( -0.6484536763576147500, -16.87597017290601897, -12.70397497891858052 ) ) ;
#37456 = CARTESIAN_POINT ( 'NONE',  ( 1.500000000000000000, -81.25000000000000000, 0.000000000000000000 ) ) ;
#37457 = CARTESIAN_POINT ( 'NONE',  ( -1.817250558667000027, -77.00611544385418483, 9.487466121941999120 ) ) ;
#37458 = CARTESIAN_POINT ( 'NONE',  ( 1.375849008456478506, -78.13331571889540328, 0.6192971689456351347 ) ) ;
#37459 = CARTESIAN_POINT ( 'NONE',  ( 2.022162896325808479, -79.20104165120571338, -3.466033633082603593 ) ) ;
#37460 = CARTESIAN_POINT ( 'NONE',  ( 11.50190934395000042, -76.74432514197999922, -3.421415122956000143 ) ) ;
#37461 = CYLINDRICAL_SURFACE ( 'NONE', #44588, 1.250000000000000000 ) ;
#37462 = CARTESIAN_POINT ( 'NONE',  ( 7.646966600034999395, -59.99642081684000061, -10.19019745249000053 ) ) ;
#37463 = CARTESIAN_POINT ( 'NONE',  ( -12.02296678431999943, -78.46687243819999935, 2.418109797047000242 ) ) ;
#37464 = CARTESIAN_POINT ( 'NONE',  ( 3.090997446795999970, -77.27913901744200587, -11.88544462247999967 ) ) ;
#37465 = CARTESIAN_POINT ( 'NONE',  ( -3.112536659741994338, -86.02148120184399716, 1.385790604991013142 ) ) ;
#37466 = CARTESIAN_POINT ( 'NONE',  ( -7.954951288349001004, -23.25000000000000000, 9.722718241315000398 ) ) ;
#37467 = B_SPLINE_CURVE_WITH_KNOTS ( 'NONE', 3,
 ( #29084, #50960, #56257, #15219, #10216, #15516, #55669, #28789, #10511, #47129 ),
 .UNSPECIFIED., .F., .F.,
 ( 4, 2, 2, 2, 4 ),
 ( 0.000000000000000000, 0.1874999983493903788, 0.3749999966987807576, 0.5624999950481708311, 0.7499999933975610711 ),
 .UNSPECIFIED. ) ;
#37468 = CARTESIAN_POINT ( 'NONE',  ( -1.720220533992320888, -77.93641922950823187, 11.89284491344992922 ) ) ;
#37469 = CARTESIAN_POINT ( 'NONE',  ( 4.038993597075479336, -78.40481902541532122, -10.27651239117697557 ) ) ;
#37470 = VERTEX_POINT ( 'NONE', #35890 ) ;
#37471 = CARTESIAN_POINT ( 'NONE',  ( -1.505598529332060842, -81.25603118963000782, -0.1141384907295430601 ) ) ;
#37472 = CARTESIAN_POINT ( 'NONE',  ( 10.26699006316253637, -78.00833333333331154, -5.917523019358050362 ) ) ;
#37473 = CARTESIAN_POINT ( 'NONE',  ( -1.750000000000000000, -57.04935285922000077, -12.65372179284000076 ) ) ;
#37474 = CARTESIAN_POINT ( 'NONE',  ( 0.9995835529977233902, -78.80208333333334281, 0.7681833999686461523 ) ) ;
#37475 = CARTESIAN_POINT ( 'NONE',  ( 3.239642551180000218, -2.998304953963999875, -2.117792278697999908 ) ) ;
#37476 = CARTESIAN_POINT ( 'NONE',  ( 0.3849455888886000321, -77.20420800240398762, -11.69935108946000035 ) ) ;
#37477 = CARTESIAN_POINT ( 'NONE',  ( 7.600999290758999827, -78.50955723388199203, 5.914221820906000460 ) ) ;
#37479 = CARTESIAN_POINT ( 'NONE',  ( -2.769480662737825671, -77.80484845553691287, -10.72687993797706341 ) ) ;
#37478 = CARTESIAN_POINT ( 'NONE',  ( -9.226664435044119372, -76.14651772991450684, 7.278599119727092059 ) ) ;
#37480 = CARTESIAN_POINT ( 'NONE',  ( -1.225487488653999923, -83.09783910444198796, -0.2866612609456000160 ) ) ;
#37481 = CARTESIAN_POINT ( 'NONE',  ( 3.333665159394552546, -85.83735717367099483, 2.421341216326917678 ) ) ;
#37482 = ORIENTED_EDGE ( 'NONE', *, *, #25391, .T. ) ;
#37483 = EDGE_CURVE ( 'NONE', #14498, #27418, #50701, .T. ) ;
#37484 = CARTESIAN_POINT ( 'NONE',  ( 1.042635221160942871, -81.08436150525301400, -1.121867648172004017 ) ) ;
#37485 = CARTESIAN_POINT ( 'NONE',  ( -9.250231375314745819, -78.08973357792895342, 1.210876817583024678 ) ) ;
#37486 = EDGE_CURVE ( 'NONE', #36484, #37361, #46532, .T. ) ;
#37487 = DIRECTION ( 'NONE',  ( 0.000000000000000000, 1.000000000000000000, 0.000000000000000000 ) ) ;
#37488 = CARTESIAN_POINT ( 'NONE',  ( 3.303001513109999898, -79.13977949711097892, -10.46681410869999951 ) ) ;
#37489 = LINE ( 'NONE', #31223, #39254 ) ;
#37490 = CARTESIAN_POINT ( 'NONE',  ( -4.038530367108999819, -79.98972034371799111, 8.407770091669000578 ) ) ;
#37491 = CARTESIAN_POINT ( 'NONE',  ( 10.13402152809999990, -18.27694524397999842, -7.647754144029000223 ) ) ;
#37492 = CARTESIAN_POINT ( 'NONE',  ( 9.431004454607295528, -17.19940410572471023, 8.251853356785181504 ) ) ;
#37493 = VERTEX_POINT ( 'NONE', #3730 ) ;
#37494 = CARTESIAN_POINT ( 'NONE',  ( -10.38493632045999959, -78.74497611018699672, 4.357414620914999759 ) ) ;
#37495 = CARTESIAN_POINT ( 'NONE',  ( 4.904027517709028672, -76.51100935185411345, -10.05130150382343679 ) ) ;
#37496 = CARTESIAN_POINT ( 'NONE',  ( 8.348814612957056625, -79.73768109752721500, -8.297071948231263150 ) ) ;
#37497 = DIRECTION ( 'NONE',  ( 0.000000000000000000, 0.000000000000000000, 1.000000000000000000 ) ) ;
#37498 = CARTESIAN_POINT ( 'NONE',  ( 6.047259872863349983, -77.78606555346475204, 10.39103189327145138 ) ) ;
#37499 = CARTESIAN_POINT ( 'NONE',  ( 1.234146787099059228, -81.36395189309098441, 0.2159370409434396010 ) ) ;
#37500 = B_SPLINE_CURVE_WITH_KNOTS ( 'NONE', 3,
 ( #12439, #33708, #30432, #21294, #16876, #47620, #57023, #29277 ),
 .UNSPECIFIED., .F., .F.,
 ( 4, 2, 2, 4 ),
 ( 0.000000000000000000, 0.2500000000000000000, 0.5000000000000000000, 1.000000000000000000 ),
 .UNSPECIFIED. ) ;
#37501 = EDGE_CURVE ( 'NONE', #89, #14353, #28582, .T. ) ;
#37502 = CARTESIAN_POINT ( 'NONE',  ( -7.408952625746029419, -79.41749330375276372, -8.421937422778746907 ) ) ;
#37503 = CARTESIAN_POINT ( 'NONE',  ( -12.50485633183174450, -53.93407854620129882, -0.6924329878416003448 ) ) ;
#37504 = CARTESIAN_POINT ( 'NONE',  ( 13.86363636363000218, -9.638971321655001034, 1.277887488545999904E-05 ) ) ;
#37505 = VECTOR ( 'NONE', #5555, 1000.000000000000000 ) ;
#37506 = DIRECTION ( 'NONE',  ( 0.000000000000000000, 0.000000000000000000, -1.000000000000000000 ) ) ;
#37507 = B_SPLINE_CURVE_WITH_KNOTS ( 'NONE', 3,
 ( #13286, #14457, #49321, #40457, #4147, #41333, #4739, #23029, #22738, #45482, #5318, #54904, #18900, #22147 ),
 .UNSPECIFIED., .F., .F.,
 ( 4, 2, 2, 2, 2, 2, 4 ),
 ( 0.000000000000000000, 0.1249999999999997502, 0.2499999999999995004, 0.4999999999999996669, 0.7499999999999997780, 0.8749999999999998890, 1.000000000000000000 ),
 .UNSPECIFIED. ) ;
#37508 = CARTESIAN_POINT ( 'NONE',  ( 1.749722766158709142, -18.52411007112894836, -12.54673760678543282 ) ) ;
#37509 = CARTESIAN_POINT ( 'NONE',  ( 2.550540064461633616, -78.59376452252105594, -10.67532501814229207 ) ) ;
#37510 = CARTESIAN_POINT ( 'NONE',  ( -12.00000000000000355, -77.28958333333331154, 1.570796326794848596 ) ) ;
#37511 = ORIENTED_EDGE ( 'NONE', *, *, #47202, .F. ) ;
#37512 = VERTEX_POINT ( 'NONE', #58339 ) ;
#37513 = DIRECTION ( 'NONE',  ( 0.000000000000000000, 0.000000000000000000, -1.000000000000000000 ) ) ;
#37514 = CARTESIAN_POINT ( 'NONE',  ( 6.653919560569870661, -78.77822032348952064, -8.445832356448455869 ) ) ;
#37515 = VERTEX_POINT ( 'NONE', #12586 ) ;
#37516 = ADVANCED_FACE ( 'NONE', ( #52749 ), #56216, .F. ) ;
#37517 = CARTESIAN_POINT ( 'NONE',  ( 1.546553306619000256, -76.38603960712254093, -11.07619323538000344 ) ) ;
#37518 = CARTESIAN_POINT ( 'NONE',  ( 1.310679582531385501, -80.19166666666669130, 0.7554284705563518720 ) ) ;
#37519 = CARTESIAN_POINT ( 'NONE',  ( 8.252521514740998043, -61.73405767862000459, 9.650901483168000894 ) ) ;
#37520 = CARTESIAN_POINT ( 'NONE',  ( -6.471588721810545231, -76.62988340216107019, -10.34169530630836320 ) ) ;
#37521 = CARTESIAN_POINT ( 'NONE',  ( 10.18080324349809729, -78.34408151796235131, 6.314367479422754670 ) ) ;
#37522 = CARTESIAN_POINT ( 'NONE',  ( 7.910349975595998728, -79.57881786998500218, 7.952639426948999279 ) ) ;
#37523 = ORIENTED_EDGE ( 'NONE', *, *, #30015, .F. ) ;
#37524 = CARTESIAN_POINT ( 'NONE',  ( -7.861032689861890077, -24.46660299217103329, 10.10708926022225107 ) ) ;
#37525 = EDGE_LOOP ( 'NONE', ( #49090, #55843, #44845, #27052 ) ) ;
#37526 = CARTESIAN_POINT ( 'NONE',  ( 9.203835967791539119, -77.35804978725602155, 0.9230458045160537806 ) ) ;
#37527 = CARTESIAN_POINT ( 'NONE',  ( 5.341789944771999643, -77.82526364781499240, 9.661750877468000098 ) ) ;
#37528 = CYLINDRICAL_SURFACE ( 'NONE', #15899, 12.50000000000000000 ) ;
#37529 = EDGE_CURVE ( 'NONE', #52707, #46363, #1362, .T. ) ;
#37530 = CARTESIAN_POINT ( 'NONE',  ( -0.1273708076881999995, -77.66562118112170765, -1.510858618444999912 ) ) ;
#37531 = CARTESIAN_POINT ( 'NONE',  ( 11.68767212001979239, -77.62916666666667709, -3.140974612311342451 ) ) ;
#37532 = TOROIDAL_SURFACE ( 'NONE', #42274, 1.250000000000000000, 0.5000000000000000000 ) ;
#37533 = CARTESIAN_POINT ( 'NONE',  ( 10.35396498619769012, -76.72450177318867759, -6.064612950829413762 ) ) ;
#37534 = CARTESIAN_POINT ( 'NONE',  ( -1.566959183383000109, -78.30783984810999243, 0.4396611996733000294 ) ) ;
#37535 = CARTESIAN_POINT ( 'NONE',  ( -0.9416178767894587409, -79.15734073197442910, -0.8218901853645335098 ) ) ;
#37536 = VECTOR ( 'NONE', #40289, 1000.000000000000114 ) ;
#37537 = CARTESIAN_POINT ( 'NONE',  ( 5.365758882164000099, -78.32770896256499782, 9.658494679878000255 ) ) ;
#37538 = LINE ( 'NONE', #38122, #23466 ) ;
#37539 = CARTESIAN_POINT ( 'NONE',  ( -7.633403016703000254, -23.38650073851000144, -10.18126993294000115 ) ) ;
#37540 = CARTESIAN_POINT ( 'NONE',  ( 12.64500484464000074, -56.02847221959000024, -1.799490225533999732 ) ) ;
#37541 = CARTESIAN_POINT ( 'NONE',  ( -2.900222056821999850, -85.99726526706999152, 2.037976741810000103 ) ) ;
#37542 = VERTEX_POINT ( 'NONE', #55367 ) ;
#37543 = FACE_OUTER_BOUND ( 'NONE', #8148, .T. ) ;
#37544 = CARTESIAN_POINT ( 'NONE',  ( 1.585573224116000102, -81.10973563566999189, 0.6211121348122999875 ) ) ;
#37545 = CARTESIAN_POINT ( 'NONE',  ( 10.45259816626330007, -77.86880115736309449, 2.510970294598007690 ) ) ;
#37546 = CARTESIAN_POINT ( 'NONE',  ( -6.777984382448000389, -78.14324916897800222, -9.878005474088999094 ) ) ;
#37547 = CARTESIAN_POINT ( 'NONE',  ( -8.790679651960999763, -17.06186536190000069, 8.797972003296999688 ) ) ;
#37548 = CARTESIAN_POINT ( 'NONE',  ( 10.75000000000000000, -78.85000000000000853, 0.000000000000000000 ) ) ;
#37549 = AXIS2_PLACEMENT_3D ( 'NONE', #9165, #49023, #4144 ) ;
#37550 = CARTESIAN_POINT ( 'NONE',  ( -0.1800737450312397958, -3.129084965038133603, 3.516770117047313349 ) ) ;
#37551 = CARTESIAN_POINT ( 'NONE',  ( 10.75000000000000000, -80.84999999999999432, -1.053639850055999980E-14 ) ) ;
#37552 = CARTESIAN_POINT ( 'NONE',  ( 4.939304878001000709, -78.41022958144498034, 8.013392654152999839 ) ) ;
#37553 = CARTESIAN_POINT ( 'NONE',  ( -6.895820826652922619, -86.02148118236289065, -5.671338893525836866 ) ) ;
#37554 = CARTESIAN_POINT ( 'NONE',  ( -8.507210620304000770, -78.01378400355899601, -7.023467935662000450 ) ) ;
#37555 = CARTESIAN_POINT ( 'NONE',  ( 1.808018834342399295, -77.28683563664310441, -11.88153690539541074 ) ) ;
#37556 = CARTESIAN_POINT ( 'NONE',  ( -6.315983860361000346, -80.60246315746479695, -8.896737291152998495 ) ) ;
#37557 = ORIENTED_EDGE ( 'NONE', *, *, #32265, .F. ) ;
#37558 = CARTESIAN_POINT ( 'NONE',  ( -0.1832406609208000192, -81.83591839377399424, -1.320984106490000087 ) ) ;
#37559 = EDGE_CURVE ( 'NONE', #30862, #26517, #19743, .T. ) ;
#37560 = CARTESIAN_POINT ( 'NONE',  ( 1.537519735729477643, -77.06247989013436950, 11.74357244733737105 ) ) ;
#37561 = CARTESIAN_POINT ( 'NONE',  ( -11.75000000000000000, -78.70000000000000284, -1.701764645356999850E-14 ) ) ;
#37562 = B_SPLINE_CURVE_WITH_KNOTS ( 'NONE', 3,
 ( #29840, #43442, #12430, #57303, #30423, #25427, #7998, #3291, #21284, #57584, #47892, #30130, #3003, #20999, #39291, #44301 ),
 .UNSPECIFIED., .F., .F.,
 ( 4, 2, 2, 2, 2, 2, 2, 4 ),
 ( 0.000000000000000000, 0.2499999999999975575, 0.3749999999999970024, 0.4999999999999964473, 0.6249999999999958922, 0.6874999999999954481, 0.7499999999999951150, 1.000000000000000000 ),
 .UNSPECIFIED. ) ;
#37563 = DIRECTION ( 'NONE',  ( 7.038562604822999888E-12, 1.000000000000000000, -4.198155382477000102E-10 ) ) ;
#37564 = ADVANCED_FACE ( 'NONE', ( #32038, #9919 ), #27615, .F. ) ;
#37565 = CARTESIAN_POINT ( 'NONE',  ( -9.302864017704999711, -76.81328150364699070, -6.266965030821000759 ) ) ;
#37566 = CARTESIAN_POINT ( 'NONE',  ( 3.176617583302000281, -79.66117957841500186, 10.50586082162000068 ) ) ;
#37567 = CARTESIAN_POINT ( 'NONE',  ( -12.76303204517000012, -18.73514852243999940, 1.980584515753000208 ) ) ;
#37568 = CARTESIAN_POINT ( 'NONE',  ( 2.599519341589024091, -85.65677084819145648, 3.056421543846630673 ) ) ;
#37569 = CARTESIAN_POINT ( 'NONE',  ( -1.704789469149992298, -23.70346161524693684, -12.53199752960662394 ) ) ;
#37570 = CARTESIAN_POINT ( 'NONE',  ( -10.10448976474953575, -54.34884052577077540, -7.864761218127002351 ) ) ;
#37571 = CARTESIAN_POINT ( 'NONE',  ( 0.2925143690059999746, -85.07919503318798604, -4.162270734640999947 ) ) ;
#37572 = CARTESIAN_POINT ( 'NONE',  ( -7.651147547618999845, -56.03743349692000209, 10.45204383579000051 ) ) ;
#37573 = CARTESIAN_POINT ( 'NONE',  ( 7.943801774140000660, -54.36598212437999678, -9.641153612765998915 ) ) ;
#37574 = CARTESIAN_POINT ( 'NONE',  ( 1.514497777301999859, -77.64085666695899590, 11.15976079676000055 ) ) ;
#37575 = CARTESIAN_POINT ( 'NONE',  ( 0.3704480504712000521, -79.91323663489998808, -1.624200486671999899 ) ) ;
#37576 = CARTESIAN_POINT ( 'NONE',  ( -1.271021473223000076, -78.49820671932999971, 0.3566262807950000280 ) ) ;
#37577 = CARTESIAN_POINT ( 'NONE',  ( -1.931736162949572622, -60.56670395678658281, 12.72978979893449392 ) ) ;
#37578 = CARTESIAN_POINT ( 'NONE',  ( 0.000000000000000000, -81.99999999999998579, 0.000000000000000000 ) ) ;
#37579 = DIRECTION ( 'NONE',  ( 0.000000000000000000, 0.7071067811866525998, -0.7071067811864425456 ) ) ;
#37580 = ORIENTED_EDGE ( 'NONE', *, *, #14100, .T. ) ;
#37581 = CARTESIAN_POINT ( 'NONE',  ( 9.000000000000000000, -0.5000000000000000000, 0.000000000000000000 ) ) ;
#37582 = TOROIDAL_SURFACE ( 'NONE', #12127, 17.50000000000000000, 5.000000000000000000 ) ;
#37583 = CARTESIAN_POINT ( 'NONE',  ( -1.460959015002473826, -77.92083333333336270, -0.3926218265389207485 ) ) ;
#37584 = EDGE_LOOP ( 'NONE', ( #28514, #47477 ) ) ;
#37585 = CARTESIAN_POINT ( 'NONE',  ( 0.09314403347896584029, -81.73140747789805971, -1.246441406727125223 ) ) ;
#37586 = SURFACE_STYLE_USAGE ( .BOTH. , #19586 ) ;
#37587 = CARTESIAN_POINT ( 'NONE',  ( 9.953654131039998632, -79.74433933582800194, 4.756732473150000473 ) ) ;
#37588 = DIRECTION ( 'NONE',  ( 0.000000000000000000, -1.000000000000000000, 1.958765290093000082E-13 ) ) ;
#37589 = ORIENTED_EDGE ( 'NONE', *, *, #1881, .T. ) ;
#37590 = ORIENTED_EDGE ( 'NONE', *, *, #25227, .T. ) ;
#37591 = CARTESIAN_POINT ( 'NONE',  ( -1.373488406293000175, -81.51250767097698713, 0.6422396358374999892 ) ) ;
#37592 = EDGE_LOOP ( 'NONE', ( #55530, #50147, #24007, #55966, #4399, #46480, #35241, #6962, #32855, #52913, #17329 ) ) ;
#37593 = B_SPLINE_CURVE_WITH_KNOTS ( 'NONE', 3,
 ( #53145, #52858, #13783, #30403, #18525, #21556, #9373, #7980, #25977, #4656 ),
 .UNSPECIFIED., .F., .F.,
 ( 4, 2, 2, 2, 4 ),
 ( 0.000000000000000000, 0.2500000000000000555, 0.5000000000000001110, 0.7500000000000002220, 1.000000000000000000 ),
 .UNSPECIFIED. ) ;
#37594 = CARTESIAN_POINT ( 'NONE',  ( 0.000000000000000000, -81.79999999999998295, 0.000000000000000000 ) ) ;
#37595 = ORIENTED_EDGE ( 'NONE', *, *, #20636, .T. ) ;
#37596 = CARTESIAN_POINT ( 'NONE',  ( 2.061649843245999758, -18.79438692412999856, 12.83797346714000120 ) ) ;
#37597 = AXIS2_PLACEMENT_3D ( 'NONE', #46929, #6455, #38040 ) ;
#37598 = DIRECTION ( 'NONE',  ( 0.000000000000000000, 0.000000000000000000, 1.000000000000000000 ) ) ;
#37599 = CARTESIAN_POINT ( 'NONE',  ( 3.325701842495000005, -82.39999999999999147, -0.7068997487804000723 ) ) ;
#37600 = CARTESIAN_POINT ( 'NONE',  ( 2.278690965393999956, -79.46391001420199984, -9.759650287631000509 ) ) ;
#37601 = CARTESIAN_POINT ( 'NONE',  ( 5.170697374967133442, -78.27237039058387325, -7.669726363621671261 ) ) ;
#37602 = CARTESIAN_POINT ( 'NONE',  ( -11.75000000000000000, -77.29999999999999716, 0.000000000000000000 ) ) ;
#37603 = ORIENTED_EDGE ( 'NONE', *, *, #46254, .T. ) ;
#37604 = VERTEX_POINT ( 'NONE', #9337 ) ;
#37605 = CARTESIAN_POINT ( 'NONE',  ( -1.750000000000000000, -77.10000000000000853, 0.000000000000000000 ) ) ;
#37606 = CARTESIAN_POINT ( 'NONE',  ( -12.70457891999271283, -25.17873330329357273, 0.5105076820425886730 ) ) ;
#37607 = CARTESIAN_POINT ( 'NONE',  ( 1.310679582531385279, -79.29166666666667140, 0.7554284705563519831 ) ) ;
#37608 = EDGE_CURVE ( 'NONE', #31168, #58211, #11626, .T. ) ;
#37609 = CARTESIAN_POINT ( 'NONE',  ( 1.501534314749353394, -61.35152951622894335, -12.70455943744364724 ) ) ;
#37610 = CARTESIAN_POINT ( 'NONE',  ( 9.703485699160999900, -77.52078622288298959, 0.1143444355825999903 ) ) ;
#37611 = FACE_OUTER_BOUND ( 'NONE', #55811, .T. ) ;
#37612 = CARTESIAN_POINT ( 'NONE',  ( 3.574842537148360755, -85.81605190634385849, 1.280382247947833063 ) ) ;
#37613 = CARTESIAN_POINT ( 'NONE',  ( 5.246383657897999875, -77.46100733245999947, -10.79237965019999912 ) ) ;
#37614 = CARTESIAN_POINT ( 'NONE',  ( -1.413725673013999984, -80.16514174310999863, -0.3972755495651000279 ) ) ;
#37615 = CARTESIAN_POINT ( 'NONE',  ( -5.650756493884554033, -77.12382193750340775, -7.570587593239054947 ) ) ;
#37616 = CARTESIAN_POINT ( 'NONE',  ( -1.405052895698000182, -81.97417810200299471, -3.928409158472000229 ) ) ;
#37617 = CARTESIAN_POINT ( 'NONE',  ( -1.473604374833289654, -79.76814583366768829, -0.3405220590759504007 ) ) ;
#37618 = CARTESIAN_POINT ( 'NONE',  ( -12.00000000000000000, -76.79999999999999716, 1.164316068523999942E-14 ) ) ;
#37619 = CARTESIAN_POINT ( 'NONE',  ( -3.321932689531000182, -80.44999999999998863, -10.22385755016999909 ) ) ;
#37620 = CARTESIAN_POINT ( 'NONE',  ( -7.605690612615000568, -18.57434870741999688, -10.52682230157000021 ) ) ;
#37622 = CARTESIAN_POINT ( 'NONE',  ( 0.4701041210474000143, -16.99203065576000071, -12.54901038416000070 ) ) ;
#37621 = DIRECTION ( 'NONE',  ( 0.7071067811865475727, 0.000000000000000000, -0.7071067811865475727 ) ) ;
#37623 = VECTOR ( 'NONE', #7792, 1000.000000000000000 ) ;
#37624 = CARTESIAN_POINT ( 'NONE',  ( 3.140974612311326908, -78.25416666666664867, 11.68767212001979772 ) ) ;
#37625 = CARTESIAN_POINT ( 'NONE',  ( -1.500000000000000000, -78.50000000000000000, 0.000000000000000000 ) ) ;
#37626 = CARTESIAN_POINT ( 'NONE',  ( 3.938458446976999205, -79.21000000000000796, -8.369650235310999165 ) ) ;
#37627 = CARTESIAN_POINT ( 'NONE',  ( -1.461856643173269132, -1.340935351588901758, -3.213633154597908437 ) ) ;
#37628 = VERTEX_POINT ( 'NONE', #14911 ) ;
#37629 = CARTESIAN_POINT ( 'NONE',  ( 5.911015991360685007, -78.96666666666666856, -10.22919423417961937 ) ) ;
#37630 = CARTESIAN_POINT ( 'NONE',  ( -10.56350348457000088, -78.15204083114099376, -4.372004352851999620 ) ) ;
#37631 = CARTESIAN_POINT ( 'NONE',  ( 10.71369944335147828, -78.97083333333333144, 2.879226727952054254 ) ) ;
#37632 = CARTESIAN_POINT ( 'NONE',  ( -6.876280931137317864, -77.17439650227632342, -6.298142934911103552 ) ) ;
#37633 = EDGE_CURVE ( 'NONE', #44472, #49809, #5478, .T. ) ;
#37634 = CARTESIAN_POINT ( 'NONE',  ( -9.492978868049998908, -79.94958509515598166, 0.8796340255361999594 ) ) ;
#37635 = CONICAL_SURFACE ( 'NONE', #49916, 10.29999999990999981, 0.7853981633972997312 ) ;
#37636 = CARTESIAN_POINT ( 'NONE',  ( -10.64207148833999916, -76.89920160919999148, 7.489034475093999887 ) ) ;
#37637 = CYLINDRICAL_SURFACE ( 'NONE', #10137, 0.5000000000000006661 ) ;
#37638 = CARTESIAN_POINT ( 'NONE',  ( -1.268951038218919747, -79.48456372641344103, 10.67475623963393083 ) ) ;
#37639 = AXIS2_PLACEMENT_3D ( 'NONE', #53637, #814, #23505 ) ;
#37640 = CARTESIAN_POINT ( 'NONE',  ( -9.848602347018999836, -79.37953998579800441, -0.02475245940598000058 ) ) ;
#37641 = DIRECTION ( 'NONE',  ( 0.000000000000000000, 0.000000000000000000, -1.000000000000000000 ) ) ;
#37642 = CARTESIAN_POINT ( 'NONE',  ( 7.337378888528000687, -77.56100197158698961, 8.415941797739000307 ) ) ;
#37643 = EDGE_CURVE ( 'NONE', #56437, #28871, #37058, .T. ) ;
#37644 = CARTESIAN_POINT ( 'NONE',  ( -1.885855158825846090, -76.31202484814713216, -11.60495004190995516 ) ) ;
#37645 = CARTESIAN_POINT ( 'NONE',  ( 1.219183338402999750, -81.21435225709299743, 1.042466414804000152 ) ) ;
#37646 = CARTESIAN_POINT ( 'NONE',  ( -7.530775182571000315, -78.20449514476064223, -6.150709233331998149 ) ) ;
#37647 = CYLINDRICAL_SURFACE ( 'NONE', #1950, 0.6000000000000008660 ) ;
#37648 = EDGE_CURVE ( 'NONE', #46028, #4126, #47467, .T. ) ;
#37650 = CARTESIAN_POINT ( 'NONE',  ( -1.636761686205434607, -2.916666666666667407, 2.839805762151332402 ) ) ;
#37649 = CARTESIAN_POINT ( 'NONE',  ( -3.015813095775000008, -82.74278679062099684, 2.239696815961000009 ) ) ;
#37651 = CARTESIAN_POINT ( 'NONE',  ( 1.813979036992999783, -79.54995584965399757, 9.381055131006998948 ) ) ;
#37652 = CARTESIAN_POINT ( 'NONE',  ( -3.630949683906000036, -75.80000000000001137, -11.17491406647000041 ) ) ;
#37653 = CARTESIAN_POINT ( 'NONE',  ( 6.842135374053461838, -80.28010575421185990, -8.291310720910153975 ) ) ;
#37654 = CARTESIAN_POINT ( 'NONE',  ( 0.000000000000000000, 4.040000000000000036, 0.000000000000000000 ) ) ;
#37655 = CARTESIAN_POINT ( 'NONE',  ( 0.000000000000000000, -86.20000000000000284, 0.000000000000000000 ) ) ;
#37656 = EDGE_LOOP ( 'NONE', ( #33582, #57694, #17775, #32628 ) ) ;
#37657 = VERTEX_POINT ( 'NONE', #32614 ) ;
#37658 = CARTESIAN_POINT ( 'NONE',  ( -0.9103933733443999587, -79.75286604907600463, -11.99492895764000089 ) ) ;
#37659 = DIRECTION ( 'NONE',  ( -0.7071067811865475727, 0.000000000000000000, -0.7071067811865475727 ) ) ;
#37660 = CARTESIAN_POINT ( 'NONE',  ( 7.764005369058246231, -17.87720632478401583, 9.931049915323967525 ) ) ;
#37661 = EDGE_LOOP ( 'NONE', ( #21162, #5714, #48128, #50970 ) ) ;
#37662 = CARTESIAN_POINT ( 'NONE',  ( 8.241770352740999783, -78.30907011069199086, -8.631843597936001089 ) ) ;
#37663 = ORIENTED_EDGE ( 'NONE', *, *, #17692, .T. ) ;
#37664 = VERTEX_POINT ( 'NONE', #50665 ) ;
#37665 = ADVANCED_FACE ( 'NONE', ( #46241 ), #21958, .F. ) ;
#37666 = EDGE_LOOP ( 'NONE', ( #56038, #42043, #867, #10641, #45449, #42684, #33287, #19747, #38478 ) ) ;
#37667 = CARTESIAN_POINT ( 'NONE',  ( -3.180857842748000319, -80.29067215926599488, -1.570574263471999910 ) ) ;
#37668 = CARTESIAN_POINT ( 'NONE',  ( 4.060630270881947723, -79.23944037031237997, 8.588476052470577216 ) ) ;
#37669 = EDGE_LOOP ( 'NONE', ( #29260, #46414, #30178, #11307, #51264, #52745, #38021 ) ) ;
#37670 = CARTESIAN_POINT ( 'NONE',  ( 1.237861236329913295, -82.83936588051422234, -0.1724589212497519564 ) ) ;
#37671 = B_SPLINE_CURVE_WITH_KNOTS ( 'NONE', 3,
 ( #21059, #39060, #57074, #56503, #15762, #29328, #56792, #11639, #2486, #16636, #6615, #16058, #20203, #28746, #6905, #25197, #16352, #34332 ),
 .UNSPECIFIED., .F., .F.,
 ( 4, 2, 2, 2, 2, 2, 2, 2, 4 ),
 ( 0.000000000000000000, 0.1250000000000000000, 0.2499999999999999722, 0.3750000000000000000, 0.5000000000000000000, 0.6250000000000000000, 0.7500000000000000000, 0.8750000000000000000, 1.000000000000000000 ),
 .UNSPECIFIED. ) ;
#37672 = CARTESIAN_POINT ( 'NONE',  ( -7.682344222584999827, -59.56462890159999546, 10.04116292117000064 ) ) ;
#37673 = ORIENTED_EDGE ( 'NONE', *, *, #13106, .F. ) ;
#37674 = CARTESIAN_POINT ( 'NONE',  ( -1.209088188845623968, -79.58012613440236294, 0.3181738888800063059 ) ) ;
#37675 = CARTESIAN_POINT ( 'NONE',  ( 0.01373196070286510778, -78.87593435104115258, -1.531465514063894640 ) ) ;
#37676 = VECTOR ( 'NONE', #41793, 1000.000000000000114 ) ;
#37677 = CARTESIAN_POINT ( 'NONE',  ( -8.653929927890716911, -79.80000000000001137, -8.194783130391765980 ) ) ;
#37678 = ADVANCED_FACE ( 'NONE', ( #5767 ), #23775, .F. ) ;
#37679 = CARTESIAN_POINT ( 'NONE',  ( 0.000000000000000000, -45.91785611817000046, 0.000000000000000000 ) ) ;
#37680 = CARTESIAN_POINT ( 'NONE',  ( 2.361413772017329382, -0.9453124996592523477, 2.369150859468821313 ) ) ;
#37681 = CARTESIAN_POINT ( 'NONE',  ( -0.1538805260929127228, -78.12626240187222493, 9.702939253146000809 ) ) ;
#37682 = CARTESIAN_POINT ( 'NONE',  ( 8.332845033087998843, -75.89124277619099246, -7.273191856730000460 ) ) ;
#37683 = CARTESIAN_POINT ( 'NONE',  ( -7.220923959705292994, -77.22708333333335418, 9.396085398178589898 ) ) ;
#37684 = EDGE_CURVE ( 'NONE', #5875, #31891, #7697, .T. ) ;
#37685 = CARTESIAN_POINT ( 'NONE',  ( 0.7681833999686451531, -81.17708333333334281, -0.9995835529977240563 ) ) ;
#37686 = FACE_OUTER_BOUND ( 'NONE', #1508, .T. ) ;
#37687 = CARTESIAN_POINT ( 'NONE',  ( -5.072857026477922915, -78.67892529861725848, -7.734870698971506364 ) ) ;
#37688 = CARTESIAN_POINT ( 'NONE',  ( 2.604752141441593505, -76.55672158594160237, 11.45797238997031720 ) ) ;
#37689 = CARTESIAN_POINT ( 'NONE',  ( 1.980532758766000212, -22.76256650694000072, -12.80088938802999898 ) ) ;
#37690 = CARTESIAN_POINT ( 'NONE',  ( 0.000000000000000000, -9.638971321655001034, 0.000000000000000000 ) ) ;
#37691 = CARTESIAN_POINT ( 'NONE',  ( -7.593646480162997925, -80.16477289014299856, -7.958079035431402382 ) ) ;
#37692 = CARTESIAN_POINT ( 'NONE',  ( -3.004722042233088697, -3.070212179489009152, 1.236557240987053996 ) ) ;
#37693 = CARTESIAN_POINT ( 'NONE',  ( -3.606252685672000524, -81.32753455456798974, 1.051809756341999913 ) ) ;
#37694 = CARTESIAN_POINT ( 'NONE',  ( 3.496086695581000381, -79.86073619718679595, 11.68876967166999847 ) ) ;
#37695 = CARTESIAN_POINT ( 'NONE',  ( -9.886815349277940257, -78.06793176728791650, 4.222132225938193706 ) ) ;
#37696 = CARTESIAN_POINT ( 'NONE',  ( -0.03211217802971453456, -82.97766872073640343, 1.249454676527944397 ) ) ;
#37697 = CARTESIAN_POINT ( 'NONE',  ( 7.342331066867000544, -55.64999999967000122, 8.190859204290999784 ) ) ;
#37698 = CARTESIAN_POINT ( 'NONE',  ( -0.1636246173744726473, -80.38541666666664298, 1.249999999999999112 ) ) ;
#37699 = CARTESIAN_POINT ( 'NONE',  ( 9.596002108778145967, -79.20208333333333428, 7.374560639699002884 ) ) ;
#37700 = CARTESIAN_POINT ( 'NONE',  ( -3.480424184914000296, -1.078054798046000018, -1.007877577829999982 ) ) ;
#37701 = CARTESIAN_POINT ( 'NONE',  ( -2.500000000000000000, -80.69999999999998863, 0.000000000000000000 ) ) ;
#37702 = CARTESIAN_POINT ( 'NONE',  ( -0.1187445621502999926, -81.25224412480599767, -1.328335755224000048 ) ) ;
#37703 = CARTESIAN_POINT ( 'NONE',  ( 13.13047446164998711, -22.78578169018998878, 0.8260994316375004365 ) ) ;
#37704 = CARTESIAN_POINT ( 'NONE',  ( -0.1963495408493606265, -80.51458333333334849, -1.500000000000000222 ) ) ;
#37705 = CARTESIAN_POINT ( 'NONE',  ( 12.99999999992999911, -5.999999999934902739, 2.526608922016999658E-09 ) ) ;
#37706 = DIRECTION ( 'NONE',  ( 0.000000000000000000, 0.000000000000000000, 1.000000000000000000 ) ) ;
#37707 = CARTESIAN_POINT ( 'NONE',  ( 7.662045806512479906, -78.13848195020216281, -7.571676706850216654 ) ) ;
#37708 = CARTESIAN_POINT ( 'NONE',  ( 10.26300017817222177, -78.31922858884991001, -4.172146172881584292 ) ) ;
#37709 = CARTESIAN_POINT ( 'NONE',  ( -7.022507694777002207, -79.28024820363059177, 8.434951230355999030 ) ) ;
#37710 = DIRECTION ( 'NONE',  ( 0.000000000000000000, 1.000000000000000000, 0.000000000000000000 ) ) ;
#37711 = ORIENTED_EDGE ( 'NONE', *, *, #6505, .T. ) ;
#37712 = CARTESIAN_POINT ( 'NONE',  ( -3.852759956968999866, -83.47632450217398059, -1.488201649610999988 ) ) ;
#37713 = CARTESIAN_POINT ( 'NONE',  ( 11.27907281578000109, -80.95552175511359394, -0.4739325926940000100 ) ) ;
#37714 = CARTESIAN_POINT ( 'NONE',  ( 8.654766271459692462, -78.32129049133318688, -3.269801377774523399 ) ) ;
#37715 = DIRECTION ( 'NONE',  ( 0.000000000000000000, 1.000000000000000000, 0.000000000000000000 ) ) ;
#37716 = CARTESIAN_POINT ( 'NONE',  ( -6.984027423104000043, -77.33016741222499491, 8.777327129872999123 ) ) ;
#37717 = DIRECTION ( 'NONE',  ( 0.000000000000000000, -1.000000000000000000, 0.000000000000000000 ) ) ;
#37718 = CARTESIAN_POINT ( 'NONE',  ( 8.831426253027000683, -78.61041000571199788, -3.841760052678000026 ) ) ;
#37719 = AXIS2_PLACEMENT_3D ( 'NONE', #48208, #16892, #44048 ) ;
#37720 = CARTESIAN_POINT ( 'NONE',  ( 3.029408902660999825, -83.78782518894399800, -2.868664668380999760 ) ) ;
#37721 = DIRECTION ( 'NONE',  ( 0.000000000000000000, 1.000000000000000000, 2.010360378377999880E-13 ) ) ;
#37722 = CARTESIAN_POINT ( 'NONE',  ( 0.000000000000000000, -80.99999999999998579, 0.000000000000000000 ) ) ;
#37723 = VERTEX_POINT ( 'NONE', #19945 ) ;
#37724 = DIRECTION ( 'NONE',  ( 0.000000000000000000, 1.000000000000000000, 0.000000000000000000 ) ) ;
#37725 = CIRCLE ( 'NONE', #12230, 14.00000000000000000 ) ;
#37726 = CARTESIAN_POINT ( 'NONE',  ( 10.70339364929999881, -80.96683882301098834, 2.537196166659999808 ) ) ;
#37727 = CARTESIAN_POINT ( 'NONE',  ( -1.703153893272331576, -78.82703160532072673, -2.986442783030232917 ) ) ;
#37728 = ORIENTED_EDGE ( 'NONE', *, *, #36908, .T. ) ;
#37729 = CARTESIAN_POINT ( 'NONE',  ( -1.320128238786999919, -78.68944723705600097, -0.1893081677438999966 ) ) ;
#37730 = CARTESIAN_POINT ( 'NONE',  ( -8.473216720655999623, -79.62385733274298616, 7.068873142094000528 ) ) ;
#37731 = ORIENTED_EDGE ( 'NONE', *, *, #10642, .F. ) ;
#37732 = CARTESIAN_POINT ( 'NONE',  ( 0.3960817336853000303, -77.45420800240398762, -12.03780325391999995 ) ) ;
#37733 = CARTESIAN_POINT ( 'NONE',  ( 0.3871641813082000172, -77.74850903582299111, -11.42594107635000178 ) ) ;
#37734 = CARTESIAN_POINT ( 'NONE',  ( 9.838187006391597933, -78.71594490248966736, -4.482782177594915041 ) ) ;
#37735 = ORIENTED_EDGE ( 'NONE', *, *, #50662, .F. ) ;
#37736 = ORIENTED_EDGE ( 'NONE', *, *, #27660, .T. ) ;
#37737 = EDGE_CURVE ( 'NONE', #49445, #28402, #22904, .T. ) ;
#37738 = CARTESIAN_POINT ( 'NONE',  ( -0.9065758875347766921, -80.54017105660118148, 0.8601027002304681979 ) ) ;
#37739 = ADVANCED_FACE ( 'NONE', ( #37934 ), #52199, .F. ) ;
#37740 = CARTESIAN_POINT ( 'NONE',  ( -8.596574492439220450, -77.65209465126851285, -6.606491961039523630 ) ) ;
#37741 = CARTESIAN_POINT ( 'NONE',  ( -8.448510849392999233, -79.34862110636998977, 4.901364000006999788 ) ) ;
#37742 = ORIENTED_EDGE ( 'NONE', *, *, #20574, .F. ) ;
#37743 = CARTESIAN_POINT ( 'NONE',  ( -6.595392621385999909, -76.20310294825600295, -10.30474759485999847 ) ) ;
#37744 = CARTESIAN_POINT ( 'NONE',  ( 1.984688374631000007, -79.71295766602599997, -10.73482082212999877 ) ) ;
#37745 = VECTOR ( 'NONE', #18439, 1000.000000000000114 ) ;
#37746 = ORIENTED_EDGE ( 'NONE', *, *, #32159, .F. ) ;
#37747 = DIRECTION ( 'NONE',  ( 1.000000000000000000, 0.000000000000000000, 0.000000000000000000 ) ) ;
#37748 = CARTESIAN_POINT ( 'NONE',  ( -2.038544480927453773, -78.69999999999998863, -3.380937442862138376 ) ) ;
#37749 = B_SPLINE_CURVE_WITH_KNOTS ( 'NONE', 3,
 ( #16675, #34941, #15801, #29363, #52973, #44118 ),
 .UNSPECIFIED., .F., .F.,
 ( 4, 1, 1, 4 ),
 ( 0.000000000000000000, 0.3333333333333000081, 0.6666666666667000474, 1.000000000000000000 ),
 .UNSPECIFIED. ) ;
#37750 = CARTESIAN_POINT ( 'NONE',  ( -0.4749605806518016893, -80.19414814864481400, -1.156137223762152111 ) ) ;
#37751 = CARTESIAN_POINT ( 'NONE',  ( 17.49999986748943925, -49.87071424677999687, 0.002153571276233540773 ) ) ;
#37752 = FACE_BOUND ( 'NONE', #16983, .T. ) ;
#37753 = EDGE_CURVE ( 'NONE', #46987, #34267, #52078, .T. ) ;
#37754 = CARTESIAN_POINT ( 'NONE',  ( 8.206391254555001069, -76.92626680923629579, -4.933833811651999746 ) ) ;
#37755 = CARTESIAN_POINT ( 'NONE',  ( 1.479639340215956889, -78.11546880775445345, 0.2990852677476950605 ) ) ;
#37756 = CARTESIAN_POINT ( 'NONE',  ( 4.044298153132396045, -80.93541667053997912, -0.2531087429660031640 ) ) ;
#37757 = CARTESIAN_POINT ( 'NONE',  ( -11.84062247810999935, -76.46062134762000539, 3.366775603358000080 ) ) ;
#37758 = CARTESIAN_POINT ( 'NONE',  ( -10.75000000000000000, -77.50000000000000000, 0.000000000000000000 ) ) ;
#37759 = AXIS2_PLACEMENT_3D ( 'NONE', #44923, #23357, #373 ) ;
#37760 = DIRECTION ( 'NONE',  ( 0.000000000000000000, 1.000000000000000000, 0.000000000000000000 ) ) ;
#37762 = EDGE_CURVE ( 'NONE', #19162, #8320, #47121, .T. ) ;
#37761 = CARTESIAN_POINT ( 'NONE',  ( -11.55418265775999842, -78.92079797882001913, 4.110954701505000308 ) ) ;
#37763 = CARTESIAN_POINT ( 'NONE',  ( -8.598496321198998871, -77.19717354083199723, -8.768570137950998600 ) ) ;
#37764 = CARTESIAN_POINT ( 'NONE',  ( 12.71005124797207131, -17.70500926711284606, -1.687536500540181228 ) ) ;
#37765 = CARTESIAN_POINT ( 'NONE',  ( 1.971342833597536037, -2.778145728227555011, -2.591225479259308351 ) ) ;
#37766 = CARTESIAN_POINT ( 'NONE',  ( 11.72382527513436656, -77.78075717553235791, -2.897248159155891400 ) ) ;
#37767 = CARTESIAN_POINT ( 'NONE',  ( 2.179295889402999897, -78.60944052572851604, 11.00312592022000047 ) ) ;
#37768 = EDGE_CURVE ( 'NONE', #44932, #36858, #43686, .T. ) ;
#37769 = ORIENTED_EDGE ( 'NONE', *, *, #49057, .F. ) ;
#37770 = FACE_OUTER_BOUND ( 'NONE', #35375, .T. ) ;
#37771 = CARTESIAN_POINT ( 'NONE',  ( -0.8342061549693000622, -77.01113784520168792, -9.562582470975000248 ) ) ;
#37772 = DIRECTION ( 'NONE',  ( -1.000000000000000000, 0.000000000000000000, 0.000000000000000000 ) ) ;
#37773 = CARTESIAN_POINT ( 'NONE',  ( -1.250000000000001332, -82.98958333333332860, 0.1636246173744632659 ) ) ;
#37774 = CARTESIAN_POINT ( 'NONE',  ( 2.810448636938000178, -3.104707871922999907, 2.661147811754999370 ) ) ;
#37775 = CARTESIAN_POINT ( 'NONE',  ( 7.822091542723999424, -77.25846663325098973, -9.013910121987001034 ) ) ;
#37776 = CARTESIAN_POINT ( 'NONE',  ( -1.570837462060999945, -78.65870446205198618, 9.612084340777000691 ) ) ;
#37778 = CARTESIAN_POINT ( 'NONE',  ( 9.209295718512867879, -76.99427083334457222, 2.475804447281278353 ) ) ;
#37777 = CARTESIAN_POINT ( 'NONE',  ( -8.300354423835440087, -76.13742599171457925, 8.316632957359784584 ) ) ;
#37779 = CARTESIAN_POINT ( 'NONE',  ( -1.223837560276999969, -82.04518551926999237, 0.5728811815464999180 ) ) ;
#37780 = DIRECTION ( 'NONE',  ( -0.7071067811865474617, 0.000000000000000000, -0.7071067811865474617 ) ) ;
#37781 = ORIENTED_EDGE ( 'NONE', *, *, #2552, .T. ) ;
#37782 = CARTESIAN_POINT ( 'NONE',  ( 1.217465845835394855, -82.22916666666667140, -0.3271848554490981997 ) ) ;
#37783 = CARTESIAN_POINT ( 'NONE',  ( 10.14999999999999858, -87.09999999999999432, 0.000000000000000000 ) ) ;
#37784 = VECTOR ( 'NONE', #15868, 999.9999999999998863 ) ;
#37785 = CARTESIAN_POINT ( 'NONE',  ( -11.75000000000000355, -76.81041666666668277, -1.538071403320004249 ) ) ;
#37786 = CARTESIAN_POINT ( 'NONE',  ( -9.505686244346000180, -79.44879539476998787, 5.486888517706000279 ) ) ;
#37787 = CARTESIAN_POINT ( 'NONE',  ( -10.47809169991074896, -80.07556136232952326, 3.347707656643508223 ) ) ;
#37788 = CARTESIAN_POINT ( 'NONE',  ( 7.648026766733999615, -18.74999999413999774, 10.12290050089000104 ) ) ;
#37789 = CARTESIAN_POINT ( 'NONE',  ( 9.205836503716000152, -16.99200673936999806, -8.541144771069001607 ) ) ;
#37790 = CARTESIAN_POINT ( 'NONE',  ( -3.399999999999999911, -78.69999997992952956, 5.715921273723000819E-07 ) ) ;
#37791 = VERTEX_POINT ( 'NONE', #17236 ) ;
#37792 = CARTESIAN_POINT ( 'NONE',  ( 10.63213186872000016, -78.49984902316998614, -3.713725309742000213 ) ) ;
#37793 = CARTESIAN_POINT ( 'NONE',  ( 0.000000000000000000, -23.94999999999946994, -12.00000000000000000 ) ) ;
#37794 = CARTESIAN_POINT ( 'NONE',  ( -11.90000000000000036, -21.00000000000000000, 0.6999999999999999556 ) ) ;
#37795 = CARTESIAN_POINT ( 'NONE',  ( 3.407095545933005454, -78.62148120184446043, 2.010777053086950872 ) ) ;
#37796 = CARTESIAN_POINT ( 'NONE',  ( -11.65386922465466846, -77.47918460901016147, -3.926725210437132851 ) ) ;
#37797 = CARTESIAN_POINT ( 'NONE',  ( -0.2267887403928895707, -81.48972645057914121, 1.230552019311672574 ) ) ;
#37798 = CARTESIAN_POINT ( 'NONE',  ( -12.52133763467701755, -54.87246868424995938, 1.618901766958424027 ) ) ;
#37799 = VECTOR ( 'NONE', #49263, 999.9999999999998863 ) ;
#37800 = CARTESIAN_POINT ( 'NONE',  ( -8.764769494928954074, -76.99999999999998579, -3.351978445651452532 ) ) ;
#37801 = CARTESIAN_POINT ( 'NONE',  ( 3.542727183245000244, -2.968224769577000099, -1.391102635753999950 ) ) ;
#37802 = VECTOR ( 'NONE', #42416, 1000.000000000000000 ) ;
#37803 = CARTESIAN_POINT ( 'NONE',  ( 1.266435358863000182, -77.80991723433999141, -0.3269927860501000150 ) ) ;
#37804 = CARTESIAN_POINT ( 'NONE',  ( -1.980464439859999981, -20.24527982672000093, 12.85144117157999943 ) ) ;
#37805 = CARTESIAN_POINT ( 'NONE',  ( -9.505836260145096972, -79.40844279816811024, 5.486975110082571661 ) ) ;
#37806 = CARTESIAN_POINT ( 'NONE',  ( -2.858407197967999913, -79.75000000000000000, -8.797272775729998884 ) ) ;
#37807 = ORIENTED_EDGE ( 'NONE', *, *, #1288, .F. ) ;
#37808 = ORIENTED_EDGE ( 'NONE', *, *, #18235, .T. ) ;
#37809 = CARTESIAN_POINT ( 'NONE',  ( 9.665471083832999355, -78.10803998579800123, -2.650702293911000318 ) ) ;
#37810 = CARTESIAN_POINT ( 'NONE',  ( 9.076269682406973516, -78.80512772263888621, -5.761168607463022617 ) ) ;
#37811 = ORIENTED_EDGE ( 'NONE', *, *, #44849, .T. ) ;
#37812 = CARTESIAN_POINT ( 'NONE',  ( 7.758899961888999997, -17.69918178096000005, 10.31442855573999928 ) ) ;
#37813 = CARTESIAN_POINT ( 'NONE',  ( -1.500000000000000000, -80.40000000000000568, 0.000000000000000000 ) ) ;
#37814 = CARTESIAN_POINT ( 'NONE',  ( -11.82502128560000010, -78.31566534667000212, 2.378298163336999949 ) ) ;
#37815 = CARTESIAN_POINT ( 'NONE',  ( 13.97864847978000036, -33.03331574008000615, 0.0001086647257957000046 ) ) ;
#37817 = EDGE_CURVE ( 'NONE', #22264, #50397, #6002, .T. ) ;
#37816 = CARTESIAN_POINT ( 'NONE',  ( 0.4155002556947535730, -76.17709054250207146, -12.19260400794555821 ) ) ;
#37818 = CARTESIAN_POINT ( 'NONE',  ( 4.899921843424915657, -78.20843494084340364, -10.93209756983152658 ) ) ;
#37819 = CARTESIAN_POINT ( 'NONE',  ( 2.315902194296999728, -78.47544367418299771, -10.97517055051999968 ) ) ;
#37820 = VERTEX_POINT ( 'NONE', #53253 ) ;
#37821 = CARTESIAN_POINT ( 'NONE',  ( 7.648026768008000076, -55.55000001556999933, -10.12290050216000026 ) ) ;
#37822 = VECTOR ( 'NONE', #21746, 1000.000000000000000 ) ;
#37823 = ORIENTED_EDGE ( 'NONE', *, *, #26612, .T. ) ;
#37824 = CARTESIAN_POINT ( 'NONE',  ( 8.229772620175682007, -77.38784508169860032, 4.222788055672235252 ) ) ;
#37825 = CARTESIAN_POINT ( 'NONE',  ( 10.94195044575999987, -77.72983452181898656, -1.468969119710000104 ) ) ;
#37826 = CARTESIAN_POINT ( 'NONE',  ( 1.633433878009751483, -77.98653774450133369, -11.09745478611874425 ) ) ;
#37827 = UNCERTAINTY_MEASURE_WITH_UNIT (LENGTH_MEASURE( 1.000000000000000082E-05 ), #56019, 'distance_accuracy_value', 'NONE');
#37828 = CARTESIAN_POINT ( 'NONE',  ( -0.2137776359178999996, -78.10637572720449384, -1.600472757759999753 ) ) ;
#37829 = CARTESIAN_POINT ( 'NONE',  ( -9.621742412363845531, -17.37938300088043775, 8.060146969363517044 ) ) ;
#37830 = DIRECTION ( 'NONE',  ( 0.000000000000000000, 0.000000000000000000, -1.000000000000000000 ) ) ;
#37831 = CARTESIAN_POINT ( 'NONE',  ( -1.481905647302000029, -78.36352141788999859, -0.6727694308694001091 ) ) ;
#37832 = CARTESIAN_POINT ( 'NONE',  ( -0.5228656313312000092, -79.11429488387997822, -11.03650783440000005 ) ) ;
#37833 = CARTESIAN_POINT ( 'NONE',  ( 1.250000000000000000, -60.04999999966999980, -12.00000000000000000 ) ) ;
#37834 = FACE_OUTER_BOUND ( 'NONE', #56553, .T. ) ;
#37835 = B_SPLINE_CURVE_WITH_KNOTS ( 'NONE', 3,
 ( #31618, #49659, #45228, #17471, #13030, #49066, #36351, #40494, #31319, #3606, #4776, #9204, #4190, #49363, #31910, #27188, #48779, #40785 ),
 .UNSPECIFIED., .F., .F.,
 ( 4, 2, 2, 2, 2, 2, 2, 2, 4 ),
 ( 0.000000000000000000, 0.1249999999999999445, 0.2499999999999998890, 0.3749999999999998335, 0.4999999999999997780, 0.6249999999999997780, 0.7499999999999997780, 0.8749999999999997780, 1.000000000000000000 ),
 .UNSPECIFIED. ) ;
#37836 = CARTESIAN_POINT ( 'NONE',  ( 0.000000000000000000, -9.295797029142999435, 0.000000000000000000 ) ) ;
#37837 = CARTESIAN_POINT ( 'NONE',  ( -3.514740471877999983, -83.18030761812998719, 0.4776706111134000343 ) ) ;
#37838 = ORIENTED_EDGE ( 'NONE', *, *, #15455, .T. ) ;
#37839 = CARTESIAN_POINT ( 'NONE',  ( -12.00000000000000178, -79.41041666666664867, -1.570796326794897668 ) ) ;
#37840 = AXIS2_PLACEMENT_3D ( 'NONE', #7011, #14987, #41573 ) ;
#37841 = CARTESIAN_POINT ( 'NONE',  ( -0.5415696896749999656, -80.73078034499999944, 1.614471809804999936 ) ) ;
#37842 = CARTESIAN_POINT ( 'NONE',  ( 0.000000000000000000, -77.19999999999998863, 0.000000000000000000 ) ) ;
#37843 = CARTESIAN_POINT ( 'NONE',  ( 9.789819849890999848, -78.76722342372499952, -6.904744247936999813 ) ) ;
#37844 = CARTESIAN_POINT ( 'NONE',  ( -9.205836503716000152, -16.99200673936999806, 8.541144771069001607 ) ) ;
#37845 = CIRCLE ( 'NONE', #24670, 13.89999999999999858 ) ;
#37846 = CARTESIAN_POINT ( 'NONE',  ( 0.1731036574200994771, -78.38625657596658414, -1.262699286490361894 ) ) ;
#37847 = CARTESIAN_POINT ( 'NONE',  ( -1.888659139779025997, -2.830543595434927173, -3.048522970863501769 ) ) ;
#37848 = CARTESIAN_POINT ( 'NONE',  ( 4.316051676898999823, -79.02855584965399771, 8.712949996777000550 ) ) ;
#37849 = CARTESIAN_POINT ( 'NONE',  ( -3.430696936678000242, -77.98387214451000204, 8.765929102848000198 ) ) ;
#37850 = CARTESIAN_POINT ( 'NONE',  ( -10.58794861553789346, -76.58625634654212888, 1.859587138064856315 ) ) ;
#37851 = CARTESIAN_POINT ( 'NONE',  ( 10.90309719880000117, -77.19669371350400411, -1.680537371260999890 ) ) ;
#37852 = CARTESIAN_POINT ( 'NONE',  ( 2.944803976276252122, -0.8802083256670968359, -1.696304167215174630 ) ) ;
#37853 = CARTESIAN_POINT ( 'NONE',  ( -7.374560639698971798, -78.37291666666666856, -9.596002108778163731 ) ) ;
#37854 = ORIENTED_EDGE ( 'NONE', *, *, #5679, .T. ) ;
#37855 = CARTESIAN_POINT ( 'NONE',  ( -1.179157772963000061, -82.18320675744099901, 0.6230118014947999550 ) ) ;
#37856 = CARTESIAN_POINT ( 'NONE',  ( -1.477284502223000118, -61.52631500263999698, -12.77254812472999923 ) ) ;
#37857 = CARTESIAN_POINT ( 'NONE',  ( -7.364280830344936746, -55.45989902437826657, 8.171144579305440914 ) ) ;
#37858 = CARTESIAN_POINT ( 'NONE',  ( 11.01642476345000077, -77.03117224766199911, 2.111041454437999842 ) ) ;
#37859 = CARTESIAN_POINT ( 'NONE',  ( 10.87588596538000019, -79.54881016108498670, -1.476184626237000197 ) ) ;
#37860 = CARTESIAN_POINT ( 'NONE',  ( 8.485538010655998775, -24.88067982437999959, -9.101501073481999882 ) ) ;
#37861 = CARTESIAN_POINT ( 'NONE',  ( 0.9857603460642816451, -83.63333332641040840, -3.930466141329476581 ) ) ;
#37862 = EDGE_CURVE ( 'NONE', #2615, #37882, #18999, .T. ) ;
#37863 = CARTESIAN_POINT ( 'NONE',  ( -11.74310723221000075, -76.06594802940500699, 1.595441940087999999 ) ) ;
#37864 = CARTESIAN_POINT ( 'NONE',  ( 0.000000000000000000, -9.638971321655001034, 0.000000000000000000 ) ) ;
#37865 = ORIENTED_EDGE ( 'NONE', *, *, #44501, .F. ) ;
#37866 = CARTESIAN_POINT ( 'NONE',  ( -0.2572323282450250659, -79.99163916602751101, 1.224162942274605426 ) ) ;
#37867 = CARTESIAN_POINT ( 'NONE',  ( -1.500000000000000888, -80.48958333333335702, 0.1963495408493559080 ) ) ;
#37868 = B_SPLINE_CURVE_WITH_KNOTS ( 'NONE', 3,
 ( #19406, #5524, #14376, #45111, #41841, #55122, #45703, #32376, #14963, #32663, #31792, #50716, #10257, #27949, #32960, #23246, #1416, #49835 ),
 .UNSPECIFIED., .F., .F.,
 ( 4, 2, 2, 2, 2, 2, 2, 2, 4 ),
 ( 0.000000000000000000, 0.1250000000000000555, 0.2500000000000001110, 0.3750000000000001665, 0.5000000000000002220, 0.6250000000000001110, 0.7500000000000001110, 0.8750000000000000000, 1.000000000000000000 ),
 .UNSPECIFIED. ) ;
#37869 = CARTESIAN_POINT ( 'NONE',  ( 8.533817832752999877, -53.79473856423000200, -9.213092693279001821 ) ) ;
#37870 = CARTESIAN_POINT ( 'NONE',  ( 8.429898053969001381, -77.87337145011899509, -7.120476661986999467 ) ) ;
#37871 = CARTESIAN_POINT ( 'NONE',  ( -0.7735022424363000582, -79.44479340558000047, 1.069754805883999849 ) ) ;
#37872 = CARTESIAN_POINT ( 'NONE',  ( -3.140974612311405512, -77.69583333333332575, 11.68767212001977640 ) ) ;
#37873 = CARTESIAN_POINT ( 'NONE',  ( -0.02829167690231079030, -81.87345300400795622, -1.509943273689894339 ) ) ;
#37874 = CARTESIAN_POINT ( 'NONE',  ( -0.4474063622920959604, -83.24816762388498148, 1.444966699100387997 ) ) ;
#37875 = CARTESIAN_POINT ( 'NONE',  ( -4.000000000000000000, -5.000000000000000000, 0.5999999999999999778 ) ) ;
#37876 = CARTESIAN_POINT ( 'NONE',  ( -1.500000000000000000, -77.89999999999999147, 0.000000000000000000 ) ) ;
#37877 = EDGE_LOOP ( 'NONE', ( #41855, #57054, #22530, #29086 ) ) ;
#37878 = CARTESIAN_POINT ( 'NONE',  ( -0.7818257270255812852, -81.67163890709370833, -0.9757561653316191297 ) ) ;
#37879 = CARTESIAN_POINT ( 'NONE',  ( -11.00000000000000000, -79.59999999999999432, 0.000000000000000000 ) ) ;
#37880 = CARTESIAN_POINT ( 'NONE',  ( -2.665716224216999830, -79.85328470783530008, 10.70493771085999946 ) ) ;
#37881 = CYLINDRICAL_SURFACE ( 'NONE', #28056, 1.250000000000000000 ) ;
#37882 = VERTEX_POINT ( 'NONE', #13383 ) ;
#37883 = ORIENTED_EDGE ( 'NONE', *, *, #3241, .F. ) ;
#37884 = CARTESIAN_POINT ( 'NONE',  ( 1.482789947567000111, -81.31405717745300876, 0.3166640546479999596 ) ) ;
#37885 = ORIENTED_EDGE ( 'NONE', *, *, #13316, .F. ) ;
#37886 = ORIENTED_EDGE ( 'NONE', *, *, #15325, .F. ) ;
#37887 = VECTOR ( 'NONE', #1966, 1000.000000000000000 ) ;
#37888 = CARTESIAN_POINT ( 'NONE',  ( -0.5390150933987999382, -16.73739108348000215, 12.77520261005000002 ) ) ;
#37889 = DIRECTION ( 'NONE',  ( -1.000000000000000000, 0.000000000000000000, 0.000000000000000000 ) ) ;
#37890 = SHAPE_DEFINITION_REPRESENTATION ( #21031, #52046 ) ;
#37891 = CARTESIAN_POINT ( 'NONE',  ( -1.500000000000000000, -78.00000000000000000, 0.000000000000000000 ) ) ;
#37892 = EDGE_CURVE ( 'NONE', #57635, #37143, #36991, .T. ) ;
#37893 = CARTESIAN_POINT ( 'NONE',  ( 6.576607919464698249, -78.28793833107616251, -6.504691508555049850 ) ) ;
#37894 = DIRECTION ( 'NONE',  ( 0.000000000000000000, -1.000000000000000000, 0.000000000000000000 ) ) ;
#37895 = ORIENTED_EDGE ( 'NONE', *, *, #7536, .T. ) ;
#37897 = ORIENTED_EDGE ( 'NONE', *, *, #4311, .T. ) ;
#37896 = ADVANCED_FACE ( 'NONE', ( #13975 ), #54754, .F. ) ;
#37898 = CARTESIAN_POINT ( 'NONE',  ( -8.920832483808519342, -77.57870377730691303, 2.448822063241335112 ) ) ;
#37899 = CARTESIAN_POINT ( 'NONE',  ( -8.485281374238999419, -18.75000000000000000, -8.485281374238999419 ) ) ;
#37900 = CARTESIAN_POINT ( 'NONE',  ( 0.2678032735957956989, -62.01432775256377283, -12.70526550773551833 ) ) ;
#37901 = CARTESIAN_POINT ( 'NONE',  ( 5.417083560473000325, -78.94197767933198406, -8.051455326762999576 ) ) ;
#37902 = DIRECTION ( 'NONE',  ( 0.000000000000000000, 0.000000000000000000, 1.000000000000000000 ) ) ;
#37903 = CARTESIAN_POINT ( 'NONE',  ( -8.190859204290999784, -55.64999999967000122, -7.342331066867000544 ) ) ;
#37904 = CARTESIAN_POINT ( 'NONE',  ( -11.99999999999999822, -77.30670863885249844, -1.011638905658493126 ) ) ;
#37905 = CARTESIAN_POINT ( 'NONE',  ( 0.8987165921316000450, -79.53370706566998649, 1.306408957324000086 ) ) ;
#37906 = CARTESIAN_POINT ( 'NONE',  ( 0.000000000000000000, -18.75000000000000000, 12.50000000000000000 ) ) ;
#37907 = ADVANCED_FACE ( 'NONE', ( #12942 ), #9986, .T. ) ;
#37908 = CARTESIAN_POINT ( 'NONE',  ( 2.483853621210999840, -79.20841833893540240, -3.352167031944000009 ) ) ;
#37909 = CARTESIAN_POINT ( 'NONE',  ( 1.156695879979905417, -79.44425242284700062, -0.9743152201541099844 ) ) ;
#37910 = CARTESIAN_POINT ( 'NONE',  ( 4.399173910654000430, -78.78151332859899014, 8.880751478442000746 ) ) ;
#37911 = CARTESIAN_POINT ( 'NONE',  ( 12.00000000000000000, -77.14999999999999147, 0.000000000000000000 ) ) ;
#37912 = CARTESIAN_POINT ( 'NONE',  ( 1.667961430005999945, -21.74888345808999901, -12.58335110161999815 ) ) ;
#37914 = CARTESIAN_POINT ( 'NONE',  ( -0.5409299486741000473, -79.17389625926099939, 1.218996123443000013 ) ) ;
#37913 = DIRECTION ( 'NONE',  ( 0.7071067811865475727, 0.000000000000000000, 0.7071067811865475727 ) ) ;
#37915 = CARTESIAN_POINT ( 'NONE',  ( 10.48543666025108045, -78.19166666666664867, 6.043427764450817641 ) ) ;
#37916 = CARTESIAN_POINT ( 'NONE',  ( 9.499693205731109202, -80.00008708754018016, -1.997583897032410100E-06 ) ) ;
#37917 = DIRECTION ( 'NONE',  ( 0.000000000000000000, 0.000000000000000000, -1.000000000000000000 ) ) ;
#37918 = LINE ( 'NONE', #20222, #49608 ) ;
#37919 = ORIENTED_EDGE ( 'NONE', *, *, #23091, .T. ) ;
#37920 = CARTESIAN_POINT ( 'NONE',  ( 7.901937437517356777, -78.98333333333333428, -8.782705133628073924 ) ) ;
#37921 = CARTESIAN_POINT ( 'NONE',  ( -1.181111693982000110, -79.17654225787899236, -0.4092372983238000139 ) ) ;
#37922 = CARTESIAN_POINT ( 'NONE',  ( 11.00000000000000355, -78.96041666666668846, 1.439896632895290018 ) ) ;
#37923 = CARTESIAN_POINT ( 'NONE',  ( 1.084783777416393535, -78.39160765235115491, 0.6217191435999254168 ) ) ;
#37924 = CARTESIAN_POINT ( 'NONE',  ( 4.848544560051999852, -80.06104530392099150, -8.085983706936000104 ) ) ;
#37925 = AXIS2_PLACEMENT_3D ( 'NONE', #29327, #43502, #52648 ) ;
#37926 = CARTESIAN_POINT ( 'NONE',  ( 12.56594317984999876, -18.75000000536999778, -1.750000000000000000 ) ) ;
#37927 = CARTESIAN_POINT ( 'NONE',  ( 1.980584515752000119, -60.06485146591000301, -12.76303204605000197 ) ) ;
#37928 = CARTESIAN_POINT ( 'NONE',  ( -1.154578316665619164, -79.48373165137867602, 10.68778363297984058 ) ) ;
#37929 = CARTESIAN_POINT ( 'NONE',  ( 6.603857951666999959, -79.12741332859900467, -7.157719488480999814 ) ) ;
#37930 = CARTESIAN_POINT ( 'NONE',  ( 5.694538069269999623E-14, -72.84999999994899156, 0.000000000000000000 ) ) ;
#37931 = CARTESIAN_POINT ( 'NONE',  ( 10.78300809584000142, -77.53919858637399898, -2.444354666989000169 ) ) ;
#37932 = CARTESIAN_POINT ( 'NONE',  ( -0.7276578379041465094, -76.32000254687065421, -11.72896174709909367 ) ) ;
#37933 = CARTESIAN_POINT ( 'NONE',  ( 1.283682315402000063, -82.14650038736000681, 0.7880738512438000276 ) ) ;
#37934 = FACE_OUTER_BOUND ( 'NONE', #50744, .T. ) ;
#37935 = CARTESIAN_POINT ( 'NONE',  ( 9.296222075829000175, -78.28338022121498341, 1.480354560350000126 ) ) ;
#37937 = CARTESIAN_POINT ( 'NONE',  ( 3.981113306789000106, -1.091474769576999959, -0.5296481109823999445 ) ) ;
#37936 = CARTESIAN_POINT ( 'NONE',  ( -0.7669882343743998909, -83.22378845168798023, -3.888151105264999519 ) ) ;
#37938 = LINE ( 'NONE', #1086, #3877 ) ;
#37939 = CARTESIAN_POINT ( 'NONE',  ( -1.500000000000000000, -80.90000000000000568, 0.000000000000000000 ) ) ;
#37940 = CARTESIAN_POINT ( 'NONE',  ( 7.705541234979771836, -80.28859837433554958, -7.495979100088282721 ) ) ;
#37941 = ADVANCED_FACE ( 'NONE', ( #5127 ), #23124, .F. ) ;
#37942 = CARTESIAN_POINT ( 'NONE',  ( -10.46839011967282040, -77.12114419157363443, -2.819731185745065538 ) ) ;
#37943 = CARTESIAN_POINT ( 'NONE',  ( 7.954951288349001004, -60.04999999966999980, 9.722718241315000398 ) ) ;
#37944 = CIRCLE ( 'NONE', #16246, 1.000000000000000000 ) ;
#37945 = ORIENTED_EDGE ( 'NONE', *, *, #4982, .F. ) ;
#37946 = AXIS2_PLACEMENT_3D ( 'NONE', #57100, #3091, #30219 ) ;
#37947 = CARTESIAN_POINT ( 'NONE',  ( 9.785129497364000173, -79.33449521720999087, -6.997026981537000090 ) ) ;
#37948 = CARTESIAN_POINT ( 'NONE',  ( 0.1637460699175452006, -78.23548803879329228, -1.249514800815695104 ) ) ;
#37949 = DIRECTION ( 'NONE',  ( 0.000000000000000000, -1.000000000000000000, 0.000000000000000000 ) ) ;
#37950 = VERTEX_POINT ( 'NONE', #39028 ) ;
#37951 = CARTESIAN_POINT ( 'NONE',  ( 6.420671964385999964, -77.79361311763999254, -10.06034164291999922 ) ) ;
#37952 = EDGE_LOOP ( 'NONE', ( #25367, #22780, #17100, #2547, #56843 ) ) ;
#37953 = ORIENTED_EDGE ( 'NONE', *, *, #46771, .T. ) ;
#37954 = CARTESIAN_POINT ( 'NONE',  ( -5.413904038987206846, -78.91666666666665719, 9.393203674808249914 ) ) ;
#37955 = DIRECTION ( 'NONE',  ( -0.9135454576426007556, 0.000000000000000000, 0.4067366430758003193 ) ) ;
#37956 = CARTESIAN_POINT ( 'NONE',  ( -3.026593009001000034, -80.05017131030399469, 1.850485041987000034 ) ) ;
#37957 = CARTESIAN_POINT ( 'NONE',  ( 7.172098529503864839, -79.20654853075065205, 6.236001066935767945 ) ) ;
#37958 = VERTEX_POINT ( 'NONE', #16316 ) ;
#37959 = CARTESIAN_POINT ( 'NONE',  ( 0.7772493032054257345, -82.77886188811029911, -0.9788881955388119005 ) ) ;
#37960 = CARTESIAN_POINT ( 'NONE',  ( -7.627487606627999739, -60.09778595451999905, 10.35845616728999907 ) ) ;
#37962 = EDGE_LOOP ( 'NONE', ( #20819, #7258, #8182, #30125 ) ) ;
#37961 = ADVANCED_FACE ( 'NONE', ( #33431 ), #16019, .F. ) ;
#37963 = CARTESIAN_POINT ( 'NONE',  ( 1.250000000000000000, -77.10000000000000853, 0.5000000000000000000 ) ) ;
#37964 = CARTESIAN_POINT ( 'NONE',  ( 1.491636372696257151, -78.01887984504998030, 0.3555933071290897640 ) ) ;
#37965 = AXIS2_PLACEMENT_3D ( 'NONE', #46355, #14444, #27437 ) ;
#37966 = CARTESIAN_POINT ( 'NONE',  ( 10.72073260548720874, -79.79999999999999716, 4.953289013571211541 ) ) ;
#37967 = LINE ( 'NONE', #1986, #37802 ) ;
#37968 = B_SPLINE_CURVE_WITH_KNOTS ( 'NONE', 3,
 ( #26026, #39038, #8609, #40191, #35754, #44054, #39611, #57615, #35160, #55229, #32482, #13912, #40780, #27183, #1235, #37216, #4771, #23643 ),
 .UNSPECIFIED., .F., .F.,
 ( 4, 2, 2, 2, 2, 2, 2, 2, 4 ),
 ( 0.000000000000000000, 0.1250000000000000000, 0.2500000000000000000, 0.3750000000000000000, 0.5000000000000000000, 0.6250000000000000000, 0.7500000000000000000, 0.8750000000000000000, 1.000000000000000000 ),
 .UNSPECIFIED. ) ;
#37969 = CARTESIAN_POINT ( 'NONE',  ( -9.446433787353997857, -78.26838154751725085, -2.221620594898999990 ) ) ;
#37970 = CARTESIAN_POINT ( 'NONE',  ( -10.67244467921999984, -76.88050928501199621, 2.904229794498999873 ) ) ;
#37971 = CARTESIAN_POINT ( 'NONE',  ( 6.384645922588179090, -76.42558410655975365, 8.681868184700029190 ) ) ;
#37972 = CARTESIAN_POINT ( 'NONE',  ( -5.148784662568076406E-06, -79.56241750339395935, -9.437165819784945953 ) ) ;
#37973 = AXIS2_PLACEMENT_3D ( 'NONE', #28310, #5886, #23893 ) ;
#37974 = CARTESIAN_POINT ( 'NONE',  ( -9.979434319869000092, -76.78551456381899243, 5.147272234993000239 ) ) ;
#37975 = EDGE_CURVE ( 'NONE', #55326, #23097, #38993, .T. ) ;
#37976 = CARTESIAN_POINT ( 'NONE',  ( -6.510594146543013494, -78.66291057767605821, -6.570709974646258722 ) ) ;
#37977 = EDGE_CURVE ( 'NONE', #32341, #34809, #31624, .T. ) ;
#37978 = CARTESIAN_POINT ( 'NONE',  ( -6.042415835457781270, -80.17903136551073828, -9.199162289450645957 ) ) ;
#37979 = CARTESIAN_POINT ( 'NONE',  ( -2.472112973585029128, -3.044024123572891316, 2.111677630882527801 ) ) ;
#37980 = CARTESIAN_POINT ( 'NONE',  ( 3.006216744975000132, -79.39967549782629419, 1.961223684219999930 ) ) ;
#37981 = CARTESIAN_POINT ( 'NONE',  ( -11.80615446477999875, -79.05949749041099039, 2.575676343767999921 ) ) ;
#37982 = CARTESIAN_POINT ( 'NONE',  ( 6.268664514307507929, -76.25703125000501359, 10.22525207047880258 ) ) ;
#37983 = CARTESIAN_POINT ( 'NONE',  ( 0.2351644692787993596, -82.96014985781650353, 1.227555708270977819 ) ) ;
#37984 = FACE_OUTER_BOUND ( 'NONE', #24029, .T. ) ;
#37985 = CARTESIAN_POINT ( 'NONE',  ( -6.862679483819019488, -76.27517955669237892, -9.537716243547501804 ) ) ;
#37986 = CARTESIAN_POINT ( 'NONE',  ( 10.38645071870000081, -19.22180874373999870, 7.655542440091000600 ) ) ;
#37987 = AXIS2_PLACEMENT_3D ( 'NONE', #48616, #3167, #13155 ) ;
#37988 = CARTESIAN_POINT ( 'NONE',  ( -1.064906745635000096, -0.9574763279779000547, 3.122496867089999739 ) ) ;
#37989 = CARTESIAN_POINT ( 'NONE',  ( 10.18491080495000034, -60.10716680829000325, 7.640030264173999441 ) ) ;
#37990 = CARTESIAN_POINT ( 'NONE',  ( -0.4631590389519468220, -79.10102817191933866, -1.469247881823791957 ) ) ;
#37991 = CARTESIAN_POINT ( 'NONE',  ( 12.43422056531000131, -24.43655741434000106, 1.197404442627999943 ) ) ;
#37992 = CARTESIAN_POINT ( 'NONE',  ( -8.205098860340234168, -77.89376641471295670, 7.080053407133187982 ) ) ;
#37993 = FILL_AREA_STYLE_COLOUR ( '', #4327 ) ;
#37994 = PRODUCT_RELATED_PRODUCT_CATEGORY ( 'part', '', ( #41849 ) ) ;
#37995 = CARTESIAN_POINT ( 'NONE',  ( -4.277738290159001089, -78.94313995163858522, -10.10766895494000117 ) ) ;
#37996 = CARTESIAN_POINT ( 'NONE',  ( 8.784635449156001030, -76.44554346881000129, -8.265499852908000378 ) ) ;
#37997 = ORIENTED_EDGE ( 'NONE', *, *, #55680, .T. ) ;
#37998 = CARTESIAN_POINT ( 'NONE',  ( 0.3111154154752000522, -82.99532450217398605, 4.118461730375999608 ) ) ;
#37999 = CARTESIAN_POINT ( 'NONE',  ( 5.088741150401000723, -79.97850485460629955, 9.946204611282000840 ) ) ;
#38000 = CARTESIAN_POINT ( 'NONE',  ( 9.201707288021751197, -78.34189891696935604, -0.9444728895368803556 ) ) ;
#38001 = FACE_OUTER_BOUND ( 'NONE', #33447, .T. ) ;
#38002 = CARTESIAN_POINT ( 'NONE',  ( 7.508079800428999917, -77.08504032520899329, -8.333477563431999968 ) ) ;
#38003 = CARTESIAN_POINT ( 'NONE',  ( 12.43359548531999970, -54.09290601346000216, -0.8500179128028999553 ) ) ;
#38004 = CARTESIAN_POINT ( 'NONE',  ( -9.173272937381000247, -77.30536039296298156, 2.837265496132999942 ) ) ;
#38005 = AXIS2_PLACEMENT_3D ( 'NONE', #19480, #50790, #14165 ) ;
#38006 = CARTESIAN_POINT ( 'NONE',  ( -1.458706046781999888, -81.84871131734999494, 0.8046341008317999810 ) ) ;
#38007 = CARTESIAN_POINT ( 'NONE',  ( 8.747999954847186288, -80.26119791688729777, -6.721802296415280153 ) ) ;
#38008 = CARTESIAN_POINT ( 'NONE',  ( 1.590911073979999868, -80.22826946565700723, -0.2760724992506000119 ) ) ;
#38009 = ORIENTED_EDGE ( 'NONE', *, *, #17656, .F. ) ;
#38010 = EDGE_CURVE ( 'NONE', #47367, #53060, #38448, .T. ) ;
#38011 = CARTESIAN_POINT ( 'NONE',  ( -10.75000000000000000, -80.00000000000000000, 0.000000000000000000 ) ) ;
#38012 = DIRECTION ( 'NONE',  ( 0.000000000000000000, 1.000000000000000000, 0.000000000000000000 ) ) ;
#38013 = CARTESIAN_POINT ( 'NONE',  ( 2.845090514860381781, -78.98918610123767792, -2.490951044996013497 ) ) ;
#38014 = EDGE_LOOP ( 'NONE', ( #52700, #30298, #54731, #44409, #24753 ) ) ;
#38015 = EDGE_CURVE ( 'NONE', #43389, #7477, #16912, .T. ) ;
#38016 = CARTESIAN_POINT ( 'NONE',  ( -0.8668440880359000733, -77.74680739281529895, -1.013523202003999923 ) ) ;
#38017 = CARTESIAN_POINT ( 'NONE',  ( -10.98042387750000159, -78.81580120733299566, -1.228081885531999928 ) ) ;
#38018 = VECTOR ( 'NONE', #22796, 1000.000000000000000 ) ;
#38019 = CARTESIAN_POINT ( 'NONE',  ( 12.60552511012999943, -60.08917723397000543, 1.799501877793999949 ) ) ;
#38020 = DIRECTION ( 'NONE',  ( -3.675129797337999037E-09, -0.9999999999999997780, 2.168720877525999531E-08 ) ) ;
#38021 = ORIENTED_EDGE ( 'NONE', *, *, #33338, .T. ) ;
#38022 = CARTESIAN_POINT ( 'NONE',  ( 10.73158301355000077, -77.61698389494598871, 5.968995448363000556 ) ) ;
#38023 = CARTESIAN_POINT ( 'NONE',  ( 2.300365334442000087, -78.19821921635399065, -11.08603795934999958 ) ) ;
#38024 = CARTESIAN_POINT ( 'NONE',  ( -2.787250405516429996, -77.49586229219684697, 10.40630179466836225 ) ) ;
#38025 = ORIENTED_EDGE ( 'NONE', *, *, #2903, .T. ) ;
#38026 = ORIENTED_EDGE ( 'NONE', *, *, #17049, .T. ) ;
#38027 = ORIENTED_EDGE ( 'NONE', *, *, #47448, .F. ) ;
#38028 = AXIS2_PLACEMENT_3D ( 'NONE', #4960, #53670, #4673 ) ;
#38029 = B_SPLINE_CURVE_WITH_KNOTS ( 'NONE', 3,
 ( #27470, #4760, #5053, #41939, #54649, #31893, #40771, #19215, #14188, #45507, #5914, #37208, #32764, #653, #13900, #14766 ),
 .UNSPECIFIED., .F., .F.,
 ( 4, 2, 2, 2, 2, 2, 2, 4 ),
 ( 0.000000000000000000, 0.2500000000000064948, 0.3750000000000097700, 0.4375000000000099365, 0.5000000000000101030, 0.6250000000000078826, 0.7500000000000056621, 1.000000000000000000 ),
 .UNSPECIFIED. ) ;
#38030 = CARTESIAN_POINT ( 'NONE',  ( 0.8712539910064536208, -80.41418404898685424, 0.8959414737579669552 ) ) ;
#38031 = CIRCLE ( 'NONE', #45596, 1.500000000000000000 ) ;
#38032 = CARTESIAN_POINT ( 'NONE',  ( 9.708203932502000200, -79.25000000000000000, -7.053423027506000587 ) ) ;
#38033 = CARTESIAN_POINT ( 'NONE',  ( -4.373213035511999358, -79.59836458285249705, -8.733596771889999388 ) ) ;
#38034 = ORIENTED_EDGE ( 'NONE', *, *, #39411, .T. ) ;
#38035 = CARTESIAN_POINT ( 'NONE',  ( 12.43569863936000175, -53.91799904124000165, 0.4278707626186999957 ) ) ;
#38036 = CARTESIAN_POINT ( 'NONE',  ( -7.105843098096999988, -79.00481274797898834, 8.287482117959999783 ) ) ;
#38037 = VERTEX_POINT ( 'NONE', #40180 ) ;
#38038 = CARTESIAN_POINT ( 'NONE',  ( -12.66761950490999844, -24.22355206198999866, -1.696827901577000031 ) ) ;
#38039 = CARTESIAN_POINT ( 'NONE',  ( -5.597970637881999778, -76.93501915034599392, 7.669424558767000022 ) ) ;
#38040 = DIRECTION ( 'NONE',  ( 1.000000000000000000, 0.000000000000000000, 0.000000000000000000 ) ) ;
#38041 = CARTESIAN_POINT ( 'NONE',  ( 1.500000000000000000, -77.75000000000000000, 0.000000000000000000 ) ) ;
#38042 = CARTESIAN_POINT ( 'NONE',  ( 1.575772165387015367, -17.53845457196653967, -12.70597445617457666 ) ) ;
#38043 = CARTESIAN_POINT ( 'NONE',  ( 6.585541864823201585, -78.36492913613842859, 7.155704809941277666 ) ) ;
#38044 = CARTESIAN_POINT ( 'NONE',  ( -11.75000000000000000, -77.79999999999999716, 1.702919296826999607E-14 ) ) ;
#38045 = CARTESIAN_POINT ( 'NONE',  ( -0.1208381380149903539, -78.73118724211690278, 1.533608188374127712 ) ) ;
#38046 = EDGE_CURVE ( 'NONE', #10899, #43630, #8429, .T. ) ;
#38047 = CARTESIAN_POINT ( 'NONE',  ( 3.740094692943897403, -82.36145835310306040, -1.455080866065831868 ) ) ;
#38048 = CARTESIAN_POINT ( 'NONE',  ( 7.331368884251999951, -75.77223222076000297, 9.888700222343000945 ) ) ;
#38049 = EDGE_CURVE ( 'NONE', #43600, #20895, #10070, .T. ) ;
#38050 = CARTESIAN_POINT ( 'NONE',  ( 5.684557159767942736, -77.82291666666665719, 7.396918292183182864 ) ) ;
#38051 = CARTESIAN_POINT ( 'NONE',  ( 17.49999999998999911, -28.92928575306000383, 1.613072089683000333E-05 ) ) ;
#38052 = CARTESIAN_POINT ( 'NONE',  ( -1.777672186646999997, -78.83457582460000879, 12.13420648597999829 ) ) ;
#38053 = CARTESIAN_POINT ( 'NONE',  ( -11.94395460750000204, -77.11520806422198859, 2.857367593729999822 ) ) ;
#38054 = CARTESIAN_POINT ( 'NONE',  ( -9.369164850722000892, -23.25000000000000000, -7.601397897754999633 ) ) ;
#38055 = CARTESIAN_POINT ( 'NONE',  ( 9.210801724128419465, -77.85636445889269908, 7.879641758992598000 ) ) ;
#38056 = CARTESIAN_POINT ( 'NONE',  ( 11.14115696400000033, -78.99074932775353375, -1.301050381412999890 ) ) ;
#38057 = CIRCLE ( 'NONE', #43710, 1.749999999999999556 ) ;
#38058 = B_SPLINE_CURVE_WITH_KNOTS ( 'NONE', 3,
 ( #26156, #44176, #44456, #4007, #31445, #54498, #13447, #4902, #45649, #53915, #49487, #35583, #788, #5189, #30860, #35285, #9035, #36187, #27022, #40322, #4307, #26434, #45354, #18480 ),
 .UNSPECIFIED., .F., .F.,
 ( 4, 2, 2, 2, 2, 2, 2, 2, 2, 2, 2, 4 ),
 ( 0.000000000000000000, 0.1249999999999988343, 0.2499999999999976685, 0.3749999999999960587, 0.4374999999999961142, 0.4999999999999962252, 0.6249999999999952260, 0.7499999999999943379, 0.8124999999999953371, 0.8437499999999955591, 0.8749999999999957812, 1.000000000000000000 ),
 .UNSPECIFIED. ) ;
#38059 = ORIENTED_EDGE ( 'NONE', *, *, #47046, .F. ) ;
#38060 = CARTESIAN_POINT ( 'NONE',  ( -1.403176326237301152, -80.71958272795352229, 0.5630851912215953936 ) ) ;
#38061 = CARTESIAN_POINT ( 'NONE',  ( 11.75000000000000000, -78.04999999999999716, 0.000000000000000000 ) ) ;
#38062 = DIRECTION ( 'NONE',  ( 0.000000000000000000, -1.000000000000000000, 0.000000000000000000 ) ) ;
#38063 = CARTESIAN_POINT ( 'NONE',  ( 1.247385801072999900, -24.47722256257999973, 12.50301438876999960 ) ) ;
#38064 = CARTESIAN_POINT ( 'NONE',  ( -3.152753737320999949, -2.925781426754000325, -1.963312250333000053 ) ) ;
#38065 = VECTOR ( 'NONE', #920, 1000.000000000000000 ) ;
#38066 = CARTESIAN_POINT ( 'NONE',  ( -4.817132589604000259, -78.53373690646100158, -11.17039677886999982 ) ) ;
#38067 = CARTESIAN_POINT ( 'NONE',  ( -17.50000000000000000, -63.73717104351998586, -4.519588592266999650E-10 ) ) ;
#38068 = ADVANCED_FACE ( 'NONE', ( #32185, #9483, #9772, #28337 ), #55219, .F. ) ;
#38070 = DIRECTION ( 'NONE',  ( 0.000000000000000000, 1.000000000000000000, 0.000000000000000000 ) ) ;
#38069 = CARTESIAN_POINT ( 'NONE',  ( -9.073759183985567134, -76.14497163204748631, 7.464983690866247024 ) ) ;
#38071 = CARTESIAN_POINT ( 'NONE',  ( -10.74525019809999904, -79.51246662722100211, 1.927424232126999870 ) ) ;
#38072 = DIRECTION ( 'NONE',  ( 0.000000000000000000, 0.000000000000000000, -1.000000000000000000 ) ) ;
#38073 = ORIENTED_EDGE ( 'NONE', *, *, #12471, .T. ) ;
#38074 = CARTESIAN_POINT ( 'NONE',  ( 1.250000000000000000, -82.24999999999998579, 0.000000000000000000 ) ) ;
#38075 = CARTESIAN_POINT ( 'NONE',  ( 1.974456364586083756, -78.70000000000000284, -3.418760544059030959 ) ) ;
#38076 = CARTESIAN_POINT ( 'NONE',  ( -11.75000000000000000, -76.79999999999999716, -1.435311119447000145E-14 ) ) ;
#38077 = DIRECTION ( 'NONE',  ( 0.000000000000000000, 0.8191944459020620295, 0.5735158758074736518 ) ) ;
#38078 = CARTESIAN_POINT ( 'NONE',  ( -10.55666020218318124, -80.07743442317976701, 3.092866764600493479 ) ) ;
#38079 = CARTESIAN_POINT ( 'NONE',  ( -9.448492440162999273, -79.59134532229998626, -1.455010287921000067 ) ) ;
#38080 = CARTESIAN_POINT ( 'NONE',  ( -1.699273914700831334, -3.183575180134248228, -2.900848162400441854 ) ) ;
#38081 = ORIENTED_EDGE ( 'NONE', *, *, #24108, .F. ) ;
#38082 = CARTESIAN_POINT ( 'NONE',  ( -9.369164850722000892, -18.75000000000000000, -7.601397897754999633 ) ) ;
#38083 = CARTESIAN_POINT ( 'NONE',  ( 5.260169723461094904, -79.38792388839776493, 10.53050267336613999 ) ) ;
#38084 = CARTESIAN_POINT ( 'NONE',  ( 3.947555661861085863, -77.60371600676303672, -11.64414702256997458 ) ) ;
#38085 = EDGE_CURVE ( 'NONE', #7670, #31856, #36630, .T. ) ;
#38087 = CARTESIAN_POINT ( 'NONE',  ( 0.8783140891125981176, -81.41347531358452727, 0.8889992555315535672 ) ) ;
#38086 = CARTESIAN_POINT ( 'NONE',  ( 1.181151010425000036, -81.87131416333899381, -0.5877481386164000732 ) ) ;
#38088 = AXIS2_PLACEMENT_3D ( 'NONE', #50114, #19100, #45689 ) ;
#38089 = CARTESIAN_POINT ( 'NONE',  ( 0.4987784050544145642, -78.49277853820406392, 1.172641800718043470 ) ) ;
#38090 = CARTESIAN_POINT ( 'NONE',  ( 0.7676033376664712637, -82.27773949277477072, -0.9994747690136148721 ) ) ;
#38091 = DIRECTION ( 'NONE',  ( 0.000000000000000000, -1.000000000000000000, 0.000000000000000000 ) ) ;
#38092 = B_SPLINE_CURVE_WITH_KNOTS ( 'NONE', 3,
 ( #10805, #29081, #9924, #5483 ),
 .UNSPECIFIED., .F., .F.,
 ( 4, 4 ),
 ( 0.000000000000000000, 1.000000000000000000 ),
 .UNSPECIFIED. ) ;
#38093 = CARTESIAN_POINT ( 'NONE',  ( 1.357743527867999900, -78.86943374892000236, -0.4206474370307000110 ) ) ;
#38094 = CARTESIAN_POINT ( 'NONE',  ( 1.750000000001000089, -18.74999999009000007, -12.56594317857000043 ) ) ;
#38095 = CARTESIAN_POINT ( 'NONE',  ( -0.6514981722053709845, -79.82982811315835647, 10.95643146437133097 ) ) ;
#38096 = AXIS2_PLACEMENT_3D ( 'NONE', #17, #57840, #12957 ) ;
#38097 = CARTESIAN_POINT ( 'NONE',  ( 12.70228859449407111, -53.97803615207048011, -1.213484947631863875 ) ) ;
#38098 = ORIENTED_EDGE ( 'NONE', *, *, #26448, .F. ) ;
#38099 = ORIENTED_EDGE ( 'NONE', *, *, #15132, .T. ) ;
#38100 = CARTESIAN_POINT ( 'NONE',  ( -6.954077596906954817, -77.83999999999998920, 6.533946999607151085 ) ) ;
#38101 = CARTESIAN_POINT ( 'NONE',  ( 2.208636725687457059, -78.74160535473284028, -10.52059596911941952 ) ) ;
#38102 = EDGE_LOOP ( 'NONE', ( #30151, #14055, #52064, #29228 ) ) ;
#38103 = CARTESIAN_POINT ( 'NONE',  ( 9.835237363972000324, -17.91864156569999977, 7.760968332719999196 ) ) ;
#38104 = CARTESIAN_POINT ( 'NONE',  ( -9.452993584203847277, -79.39181711029749522, 0.9501152051606440718 ) ) ;
#38105 = CARTESIAN_POINT ( 'NONE',  ( 7.784308188539000639, -79.14914617087998749, 8.871412621384999753 ) ) ;
#38106 = DIRECTION ( 'NONE',  ( 0.000000000000000000, 0.1122098755727947705, -0.9936845293270585300 ) ) ;
#38107 = CARTESIAN_POINT ( 'NONE',  ( 6.586108526242999694, -80.17391735373439587, 8.810401493720998900 ) ) ;
#38108 = FACE_OUTER_BOUND ( 'NONE', #27885, .T. ) ;
#38109 = CARTESIAN_POINT ( 'NONE',  ( -9.066796825632000179, -78.88398881921099814, -6.603885667862000375 ) ) ;
#38110 = VERTEX_POINT ( 'NONE', #940 ) ;
#38111 = CARTESIAN_POINT ( 'NONE',  ( 11.75000000000000000, -78.05690292554332643, 1.019250468234808471 ) ) ;
#38112 = ORIENTED_EDGE ( 'NONE', *, *, #50332, .T. ) ;
#38113 = CARTESIAN_POINT ( 'NONE',  ( 9.233111569183694911, -77.35500786911740079, 0.5775652420082610927 ) ) ;
#38114 = DIRECTION ( 'NONE',  ( 0.7071067811864976127, -0.7071067811865975328, -1.721794132147993560E-09 ) ) ;
#38115 = CARTESIAN_POINT ( 'NONE',  ( -8.729826100308692105, -77.79588334348935064, 7.043560550046861657 ) ) ;
#38116 = CARTESIAN_POINT ( 'NONE',  ( -0.2736340887363999941, -78.65787364874299215, -1.491330460909999989 ) ) ;
#38117 = CARTESIAN_POINT ( 'NONE',  ( -7.709155920934738226, -60.72747430363508414, -9.998700314201723671 ) ) ;
#38118 = CARTESIAN_POINT ( 'NONE',  ( -1.750000000000000000, -23.24999999688999708, 12.50000000000000000 ) ) ;
#38119 = CARTESIAN_POINT ( 'NONE',  ( -0.9347040216968000026, -78.81250873020999848, 1.332288049216000081 ) ) ;
#38120 = CARTESIAN_POINT ( 'NONE',  ( -7.718368845776000242, -21.74800977511999989, 10.07722254365999959 ) ) ;
#38121 = CARTESIAN_POINT ( 'NONE',  ( 9.366620387600999464, -79.19857194687799051, -5.860402389062000061 ) ) ;
#38122 = CARTESIAN_POINT ( 'NONE',  ( -7.000000000000000000, -81.10000000285099020, -1.099999997148999986 ) ) ;
#38123 = CARTESIAN_POINT ( 'NONE',  ( 3.577370205891725163, -79.79961842550528672, -11.19231790377194713 ) ) ;
#38124 = CARTESIAN_POINT ( 'NONE',  ( 0.1742185655343000128, -85.75676443653598824, 3.540419386099000310 ) ) ;
#38125 = VERTEX_POINT ( 'NONE', #49643 ) ;
#38127 = B_SPLINE_CURVE_WITH_KNOTS ( 'NONE', 3,
 ( #2200, #38480, #19607, #42045, #47081, #1913, #6610, #56498, #6022, #52075, #11633, #25190, #2769, #37606, #15172, #10763 ),
 .UNSPECIFIED., .F., .F.,
 ( 4, 2, 2, 2, 2, 2, 2, 4 ),
 ( 0.000000000000000000, 0.2499999999999962252, 0.3749999999999943379, 0.4374999999999947264, 0.4999999999999951150, 0.6249999999999960032, 0.7499999999999968914, 1.000000000000000000 ),
 .UNSPECIFIED. ) ;
#38126 = CARTESIAN_POINT ( 'NONE',  ( 12.00000000000000711, -79.63958333333333428, -1.570796326794872355 ) ) ;
#38128 = CARTESIAN_POINT ( 'NONE',  ( 9.002946773217001208, -76.07771018338799252, 6.708522467097999709 ) ) ;
#38129 = CARTESIAN_POINT ( 'NONE',  ( 8.098714463133978470, -79.29284371306400203, -7.103727516995692604 ) ) ;
#38130 = CARTESIAN_POINT ( 'NONE',  ( -1.360213228908000005, -77.74983936004998952, -11.90234785270000017 ) ) ;
#38131 = CARTESIAN_POINT ( 'NONE',  ( -7.631889106325000505, -18.77878585407000145, 10.36222439674000029 ) ) ;
#38132 = CARTESIAN_POINT ( 'NONE',  ( 0.4271247780714595432, -78.40215820034904937, -1.201638839774739065 ) ) ;
#38133 = CARTESIAN_POINT ( 'NONE',  ( -3.134290163747470270, -2.287741105247256712, -1.607198584962695520 ) ) ;
#38134 = CARTESIAN_POINT ( 'NONE',  ( -0.5312504855272001114, -78.81080584965400249, -9.708839960653000034 ) ) ;
#38135 = CARTESIAN_POINT ( 'NONE',  ( -9.004250860540000900, -77.10273344151168828, -2.744961831234999927 ) ) ;
#38137 = EDGE_CURVE ( 'NONE', #54879, #39417, #38029, .T. ) ;
#38136 = CARTESIAN_POINT ( 'NONE',  ( 1.930628539546999978, -55.57875555881000196, -12.72375828102000028 ) ) ;
#38138 = CARTESIAN_POINT ( 'NONE',  ( -9.149418163674001292, -77.00603931249200684, -6.163594735446999984 ) ) ;
#38139 = CARTESIAN_POINT ( 'NONE',  ( -8.034660013930000844, -81.08572150553020208, -7.381588020910998971 ) ) ;
#38140 = CARTESIAN_POINT ( 'NONE',  ( 0.6280001350017426764, -81.81618824546241342, -1.109471376811945298 ) ) ;
#38141 = EDGE_LOOP ( 'NONE', ( #50751, #39376, #41225, #24642 ) ) ;
#38142 = CARTESIAN_POINT ( 'NONE',  ( -0.5935892672256000147, -82.13359413406000442, 1.194249225580000129 ) ) ;
#38143 = DIRECTION ( 'NONE',  ( 0.000000000000000000, 0.000000000000000000, -1.000000000000000000 ) ) ;
#38144 = CIRCLE ( 'NONE', #12672, 5.000000000000000888 ) ;
#38145 = CARTESIAN_POINT ( 'NONE',  ( -0.4701041210467000186, -61.80796934391000264, -12.54901038419999892 ) ) ;
#38146 = CARTESIAN_POINT ( 'NONE',  ( -7.356278612544860707, -55.49583131490852850, 8.178338515874328252 ) ) ;
#38147 = CARTESIAN_POINT ( 'NONE',  ( -6.659967121051000305, -76.84051784664899287, -9.025682433062998555 ) ) ;
#38148 = CARTESIAN_POINT ( 'NONE',  ( -9.813193589766999736, -78.90680422843898612, -4.915816122623000162 ) ) ;
#38149 = CARTESIAN_POINT ( 'NONE',  ( -0.2201363562291999698, -79.46327907014000402, -1.483758735329000045 ) ) ;
#38150 = CARTESIAN_POINT ( 'NONE',  ( -4.022178672785524434, -83.17083332143187135, 0.4884531335743385605 ) ) ;
#38151 = CARTESIAN_POINT ( 'NONE',  ( -11.21131451355000053, -77.04216005809600176, -4.985388207940000704 ) ) ;
#38152 = CARTESIAN_POINT ( 'NONE',  ( 11.22740784686473248, -78.47264872320555185, 3.462864101539464112 ) ) ;
#38153 = CARTESIAN_POINT ( 'NONE',  ( 1.343749999883000035, -77.90625000011999646, 3.156563468101999814E-09 ) ) ;
#38154 = ORIENTED_EDGE ( 'NONE', *, *, #20365, .T. ) ;
#38155 = DIRECTION ( 'NONE',  ( 0.000000000000000000, -1.000000000000000000, 0.000000000000000000 ) ) ;
#38156 = CARTESIAN_POINT ( 'NONE',  ( 13.79999999994999982, 4.699973049637762301E-11, 2.072308546948999944E-09 ) ) ;
#38157 = EDGE_CURVE ( 'NONE', #3036, #42393, #50810, .T. ) ;
#38158 = CARTESIAN_POINT ( 'NONE',  ( 4.019191877497999776, -79.02515797775897965, 10.52497178225999974 ) ) ;
#38159 = CARTESIAN_POINT ( 'NONE',  ( -11.87500000004000000, -79.12500000004000356, -1.061343742159000057E-08 ) ) ;
#38160 = CARTESIAN_POINT ( 'NONE',  ( 7.374560639698993114, -79.47708333333332575, -9.596002108778149520 ) ) ;
#38161 = CARTESIAN_POINT ( 'NONE',  ( -1.250754810632284109, -79.07932702254176149, 0.3272114123015318898 ) ) ;
#38162 = CARTESIAN_POINT ( 'NONE',  ( 1.542660238577055365, -82.09427013190894229, -0.1073020398081418886 ) ) ;
#38163 = CARTESIAN_POINT ( 'NONE',  ( 0.1190605478174616982, -79.73281567795952185, -1.244496223888971187 ) ) ;
#38164 = CARTESIAN_POINT ( 'NONE',  ( 0.9218200799623741393, -78.07708333333334849, -1.199500263597268690 ) ) ;
#38165 = ADVANCED_FACE ( 'NONE', ( #46389 ), #17288, .T. ) ;
#38166 = ORIENTED_EDGE ( 'NONE', *, *, #17045, .F. ) ;
#38167 = CARTESIAN_POINT ( 'NONE',  ( 2.062670899361999766, -18.69360215052999763, 12.83044027761000017 ) ) ;
#38168 =( NAMED_UNIT ( * ) SI_UNIT ( $, .STERADIAN. ) SOLID_ANGLE_UNIT ( ) );
#38169 = EDGE_CURVE ( 'NONE', #42100, #29817, #24654, .T. ) ;
#38170 = CIRCLE ( 'NONE', #10840, 1.000000000000000000 ) ;
#38171 = CYLINDRICAL_SURFACE ( 'NONE', #10172, 11.75000000000000000 ) ;
#38172 = ORIENTED_EDGE ( 'NONE', *, *, #37643, .T. ) ;
#38173 = ORIENTED_EDGE ( 'NONE', *, *, #27197, .T. ) ;
#38174 = FACE_OUTER_BOUND ( 'NONE', #26324, .T. ) ;
#38175 = VECTOR ( 'NONE', #52307, 1000.000000000000000 ) ;
#38176 = ORIENTED_EDGE ( 'NONE', *, *, #55632, .F. ) ;
#38177 = CARTESIAN_POINT ( 'NONE',  ( 7.152873968220873735, -79.94241816209181195, -6.324799438550645192 ) ) ;
#38178 = ORIENTED_EDGE ( 'NONE', *, *, #40419, .T. ) ;
#38179 = CARTESIAN_POINT ( 'NONE',  ( 1.295048492660999973, -17.47106480873999956, 12.54716442236999896 ) ) ;
#38180 = DIRECTION ( 'NONE',  ( 1.411455651355999932E-10, 6.386283326366000088E-09, 1.000000000000000000 ) ) ;
#38181 = CARTESIAN_POINT ( 'NONE',  ( 0.000000000000000000, 0.000000000000000000, 0.000000000000000000 ) ) ;
#38182 = CARTESIAN_POINT ( 'NONE',  ( -7.648026766753000416, -60.05000000550000294, 10.12290050090999927 ) ) ;
#38183 = CARTESIAN_POINT ( 'NONE',  ( -0.5353773281849999455, -78.81376332859899492, -9.784259853904000437 ) ) ;
#38184 = VECTOR ( 'NONE', #26351, 1000.000000000000000 ) ;
#38185 = CARTESIAN_POINT ( 'NONE',  ( -0.5684419807725448193, -78.22027183137143425, -9.237336331917868293 ) ) ;
#38186 = CARTESIAN_POINT ( 'NONE',  ( 7.629353270364749307, -76.29218750007841265, -7.631376092477169415 ) ) ;
#38187 = EDGE_LOOP ( 'NONE', ( #25779, #10745, #57561 ) ) ;
#38188 = VERTEX_POINT ( 'NONE', #37793 ) ;
#38189 = CARTESIAN_POINT ( 'NONE',  ( 12.65372179304999811, -58.55064713745999683, 1.750000000000000000 ) ) ;
#38190 = CARTESIAN_POINT ( 'NONE',  ( -9.699999999837999098, -87.69999999983798489, -3.624872775666000097E-09 ) ) ;
#38191 = EDGE_CURVE ( 'NONE', #22103, #4693, #11807, .T. ) ;
#38192 = CARTESIAN_POINT ( 'NONE',  ( -12.77657007944999989, -62.11210281297999813, -0.1589025507403999948 ) ) ;
#38193 = CARTESIAN_POINT ( 'NONE',  ( 6.983565664416999219, -78.45877258413898403, -6.737990796766999857 ) ) ;
#38194 = CARTESIAN_POINT ( 'NONE',  ( 1.750000000000000000, -60.04999999725999515, 12.50000000000000000 ) ) ;
#38195 = CARTESIAN_POINT ( 'NONE',  ( -10.01332852689000141, -18.71943464842000182, 7.654537165467999671 ) ) ;
#38196 = DIRECTION ( 'NONE',  ( 0.7071067811865474617, 0.000000000000000000, 0.7071067811865474617 ) ) ;
#38197 = CARTESIAN_POINT ( 'NONE',  ( -0.5437916395094000155, -79.30212327692998997, -1.373128015768000143 ) ) ;
#38198 = CARTESIAN_POINT ( 'NONE',  ( -0.3750911572844000119, -82.24349422833900292, -1.205494135727000149 ) ) ;
#38199 = CARTESIAN_POINT ( 'NONE',  ( -9.968462051564484838, -76.65502326558416257, 6.229966083963330625 ) ) ;
#38200 = CARTESIAN_POINT ( 'NONE',  ( -6.464912241513801260E-06, -79.20362641130290626, -11.95086305119197689 ) ) ;
#38201 = CARTESIAN_POINT ( 'NONE',  ( -9.929695104576000020, -54.16901065014000238, 7.973993995727001405 ) ) ;
#38202 = CARTESIAN_POINT ( 'NONE',  ( -8.988089064694998243, -77.97428667140098923, 3.902915570549000179 ) ) ;
#38203 = CARTESIAN_POINT ( 'NONE',  ( -9.596002108778193929, -77.34791666666663446, 7.374560639698937159 ) ) ;
#38204 = CARTESIAN_POINT ( 'NONE',  ( 1.250000000000000000, -81.24999999999998579, 0.000000000000000000 ) ) ;
#38206 = CARTESIAN_POINT ( 'NONE',  ( 1.801750019963999971, -18.60992573277999895, -12.59656967653999970 ) ) ;
#38205 = CARTESIAN_POINT ( 'NONE',  ( -1.310679582531389276, -78.85833333333332007, 0.7554284705563443225 ) ) ;
#38207 = CYLINDRICAL_SURFACE ( 'NONE', #1584, 9.199999999999999289 ) ;
#38208 = CARTESIAN_POINT ( 'NONE',  ( 11.00860450206999985, -80.25708356157298340, 1.960025359315999971 ) ) ;
#38209 = DIRECTION ( 'NONE',  ( 1.000000000000000000, 0.000000000000000000, -0.000000000000000000 ) ) ;
#38210 = CARTESIAN_POINT ( 'NONE',  ( -3.527598694514999966, -78.42305673476900552, -10.69532371905999923 ) ) ;
#38211 = CARTESIAN_POINT ( 'NONE',  ( -3.447531475110328092, -1.267068432622050933, -0.7497128906106725887 ) ) ;
#38212 = ORIENTED_EDGE ( 'NONE', *, *, #28146, .T. ) ;
#38213 = LINE ( 'NONE', #33775, #53674 ) ;
#38214 = CARTESIAN_POINT ( 'NONE',  ( 10.07627163191000008, -60.04999999725999515, 7.601397897754999633 ) ) ;
#38215 = CARTESIAN_POINT ( 'NONE',  ( -10.50000000000000000, -81.99999999999998579, 0.000000000000000000 ) ) ;
#38216 = CONICAL_SURFACE ( 'NONE', #58014, 9.649999999909001147, 0.7853981633972997312 ) ;
#38217 = CARTESIAN_POINT ( 'NONE',  ( 1.201809672664051476, -78.37247684905804590, 0.3447628147767792806 ) ) ;
#38218 = AXIS2_PLACEMENT_3D ( 'NONE', #27721, #54025, #53731 ) ;
#38219 = CARTESIAN_POINT ( 'NONE',  ( -4.746402720823999388, -79.54046787954499109, -8.268135452721999457 ) ) ;
#38220 = CARTESIAN_POINT ( 'NONE',  ( -12.57433760364000008, -55.08878254084000048, 1.760777649351999985 ) ) ;
#38221 = CARTESIAN_POINT ( 'NONE',  ( 8.436594745246246418, -79.14112415376850151, 4.819671195624712468 ) ) ;
#38222 = CARTESIAN_POINT ( 'NONE',  ( 1.691611010926999947, -61.03082691197000287, 12.66722148972999840 ) ) ;
#38223 = CARTESIAN_POINT ( 'NONE',  ( 0.2531623955774147117, -79.47320930135717276, 10.74994997524480311 ) ) ;
#38224 = CARTESIAN_POINT ( 'NONE',  ( -12.00000000000000000, -60.04999999966999980, 0.000000000000000000 ) ) ;
#38225 = ADVANCED_FACE ( 'NONE', ( #33057 ), #25084, .F. ) ;
#38226 = CARTESIAN_POINT ( 'NONE',  ( 0.7999999997951000585, -23.14999999072999870, 11.99999999979999821 ) ) ;
#38227 = CARTESIAN_POINT ( 'NONE',  ( 7.194421757875000267, -77.68875345315298375, 8.251970588205999491 ) ) ;
#38228 = ADVANCED_FACE ( 'NONE', ( #47837 ), #11237, .T. ) ;
#38229 = CARTESIAN_POINT ( 'NONE',  ( -0.9453041629244000044, -78.09062011958100413, 11.10679974661999836 ) ) ;
#38230 = CARTESIAN_POINT ( 'NONE',  ( 0.000000000000000000, -52.69905023022000279, 0.000000000000000000 ) ) ;
#38231 = DIRECTION ( 'NONE',  ( 1.000000000000000000, 0.000000000000000000, 0.000000000000000000 ) ) ;
#38232 = CARTESIAN_POINT ( 'NONE',  ( -2.364557222828000072, -79.52495194988499350, 9.257622954664000758 ) ) ;
#38233 = CARTESIAN_POINT ( 'NONE',  ( -1.217465845835394411, -82.52083333333331439, -0.3271848554491003647 ) ) ;
#38234 = CARTESIAN_POINT ( 'NONE',  ( 1.460959015002472494, -81.27083333333332860, 0.3926218265389233020 ) ) ;
#38235 = LINE ( 'NONE', #56256, #8936 ) ;
#38236 = CARTESIAN_POINT ( 'NONE',  ( 9.500000000000001776, -77.16041666666667709, 1.243547092045981239 ) ) ;
#38237 = CARTESIAN_POINT ( 'NONE',  ( 3.552363299575000077, -79.71496112664699751, -11.49294985030999960 ) ) ;
#38238 = DIRECTION ( 'NONE',  ( 0.000000000000000000, 1.000000000000000000, 0.000000000000000000 ) ) ;
#38239 = EDGE_CURVE ( 'NONE', #16697, #9567, #57236, .T. ) ;
#38240 = CARTESIAN_POINT ( 'NONE',  ( 7.648026766733999615, -18.74999999413999774, 10.12290050089000104 ) ) ;
#38241 = ORIENTED_EDGE ( 'NONE', *, *, #10942, .T. ) ;
#38242 = CARTESIAN_POINT ( 'NONE',  ( -4.070249838183999991, -78.52610463408198882, 11.21911621747999810 ) ) ;
#38243 = ORIENTED_EDGE ( 'NONE', *, *, #11767, .F. ) ;
#38244 = ORIENTED_EDGE ( 'NONE', *, *, #13813, .T. ) ;
#38245 =( NAMED_UNIT ( * ) PLANE_ANGLE_UNIT ( ) SI_UNIT ( $, .RADIAN. ) );
#38246 = VERTEX_POINT ( 'NONE', #2379 ) ;
#38247 = CARTESIAN_POINT ( 'NONE',  ( 0.5659361347325999603, -82.09442852648498956, -3.502031804551999805 ) ) ;
#38248 = CARTESIAN_POINT ( 'NONE',  ( 2.135299940751924197, -79.25691378410574828, 9.265864175146425907 ) ) ;
#38249 = CIRCLE ( 'NONE', #2453, 10.69999999999999929 ) ;
#38250 = VERTEX_POINT ( 'NONE', #34214 ) ;
#38251 = CARTESIAN_POINT ( 'NONE',  ( -0.3277207512123008204, -82.70464360152637084, -1.218374181744829698 ) ) ;
#38252 = ORIENTED_EDGE ( 'NONE', *, *, #46337, .F. ) ;
#38253 = CARTESIAN_POINT ( 'NONE',  ( -7.678667886061999681, -57.04263462147999775, 10.59548767699999949 ) ) ;
#38254 = ORIENTED_EDGE ( 'NONE', *, *, #53703, .F. ) ;
#38255 = CARTESIAN_POINT ( 'NONE',  ( -1.184592955636749378, -79.57468984537729284, 0.3985202767571495164 ) ) ;
#38256 = CARTESIAN_POINT ( 'NONE',  ( -0.05333894232729029239, -79.12800920574750307, 1.532713344806896361 ) ) ;
#38257 = CARTESIAN_POINT ( 'NONE',  ( 1.941355800891735761, -79.80000000000001137, -11.64207563132269740 ) ) ;
#38258 = CIRCLE ( 'NONE', #27880, 12.05000000000000071 ) ;
#38259 = CARTESIAN_POINT ( 'NONE',  ( -5.514935242309477736, -80.01815905343127611, 9.228334353175002391 ) ) ;
#38260 = CARTESIAN_POINT ( 'NONE',  ( 11.81453738175115120, -78.72182493446904061, 3.290083300416718259 ) ) ;
#38261 = FACE_OUTER_BOUND ( 'NONE', #34096, .T. ) ;
#38262 = CARTESIAN_POINT ( 'NONE',  ( -9.831705185582000794, -76.29436059729400199, 5.330239850318999828 ) ) ;
#38263 = FACE_OUTER_BOUND ( 'NONE', #30922, .T. ) ;
#38264 = VECTOR ( 'NONE', #36727, 1000.000000000000000 ) ;
#38265 = CARTESIAN_POINT ( 'NONE',  ( 7.560105429166095625, -77.04631109317882931, -6.032831105176230224 ) ) ;
#38266 = CARTESIAN_POINT ( 'NONE',  ( 1.250000000000000222, -81.23958333333334281, -0.1636246173744659582 ) ) ;
#38267 = CARTESIAN_POINT ( 'NONE',  ( 11.02258233089000150, -76.05813824613500174, -2.141614703964000110 ) ) ;
#38268 = CARTESIAN_POINT ( 'NONE',  ( -8.199591636648101201, -78.63841546258160520, -4.282090486464941392 ) ) ;
#38269 = CARTESIAN_POINT ( 'NONE',  ( 1.329937235669000017, -79.42218752083800837, -0.09921221311570001256 ) ) ;
#38270 = CARTESIAN_POINT ( 'NONE',  ( -3.249521313392360167, -3.093723106175902515, 0.2889460297551491585 ) ) ;
#38271 = CARTESIAN_POINT ( 'NONE',  ( -0.9905749567282999823, -81.20342549782600372, 3.449999823992999648 ) ) ;
#38273 = EDGE_CURVE ( 'NONE', #45906, #31098, #24090, .T. ) ;
#38272 = CARTESIAN_POINT ( 'NONE',  ( 8.958886133240000049, -79.26804927549699187, -8.109116339278001462 ) ) ;
#38274 = CARTESIAN_POINT ( 'NONE',  ( -8.024340789631628112, -78.04212779903014052, 7.157226290975113869 ) ) ;
#38275 = CARTESIAN_POINT ( 'NONE',  ( -0.5301937742937986586, -83.00996881353496804, 1.132399620896593850 ) ) ;
#38276 = CARTESIAN_POINT ( 'NONE',  ( 0.000000000000000000, -56.01421830981000483, 13.15643568216998638 ) ) ;
#38277 = CARTESIAN_POINT ( 'NONE',  ( -2.280948012154000004, -83.39569503318799093, -2.716401763145999571 ) ) ;
#38278 = CARTESIAN_POINT ( 'NONE',  ( -8.311834820408467550, -76.26188411096713082, -8.304661350511205242 ) ) ;
#38279 = CARTESIAN_POINT ( 'NONE',  ( 11.68767212001978173, -79.17083333333336270, 3.140974612311388192 ) ) ;
#38280 = CARTESIAN_POINT ( 'NONE',  ( -2.931470798466000005, -1.005707716004999863, 2.126387630743999946 ) ) ;
#38281 = FACE_OUTER_BOUND ( 'NONE', #11750, .T. ) ;
#38282 = CARTESIAN_POINT ( 'NONE',  ( -1.200131629027000102, -80.65689264423299676, -0.3495483843597000373 ) ) ;
#38283 = CARTESIAN_POINT ( 'NONE',  ( 0.000000000000000000, -90.39999999999999147, 0.000000000000000000 ) ) ;
#38284 = CARTESIAN_POINT ( 'NONE',  ( 12.54981857173999948, -25.04836586201999893, -0.03768635776136000648 ) ) ;
#38285 = CARTESIAN_POINT ( 'NONE',  ( 0.4264610271018738907, -77.82239105019517922, 10.82843159672154165 ) ) ;
#38286 = CARTESIAN_POINT ( 'NONE',  ( 9.632126701410999914, -79.13978643196745111, 5.261763182588000909 ) ) ;
#38287 = CARTESIAN_POINT ( 'NONE',  ( 10.27481476821000150, -76.04949241823000250, 6.317949980592000969 ) ) ;
#38288 = ORIENTED_EDGE ( 'NONE', *, *, #14771, .F. ) ;
#38289 = CARTESIAN_POINT ( 'NONE',  ( -2.532550380305000015, -84.79521544543099765, 3.048305984539999791 ) ) ;
#38290 = CARTESIAN_POINT ( 'NONE',  ( 3.112536659742000111, -86.02148120184399716, -1.385790604991000041 ) ) ;
#38291 = B_SPLINE_CURVE_WITH_KNOTS ( 'NONE', 3,
 ( #24683, #47143, #6381, #34097, #33528, #11122 ),
 .UNSPECIFIED., .F., .F.,
 ( 4, 1, 1, 4 ),
 ( 0.000000000000000000, 0.3333333333333000081, 0.6666666666667000474, 1.000000000000000000 ),
 .UNSPECIFIED. ) ;
#38292 = EDGE_CURVE ( 'NONE', #54222, #52985, #13537, .T. ) ;
#38294 = CARTESIAN_POINT ( 'NONE',  ( -4.621634366555106510, -76.29240483638720605, -10.80276227228939234 ) ) ;
#38293 = CARTESIAN_POINT ( 'NONE',  ( 8.413103616488427861, -78.31587669965468024, -3.846938760799505808 ) ) ;
#38295 = CARTESIAN_POINT ( 'NONE',  ( 10.41172548049708801, -55.27988211096354121, 7.610718780864914379 ) ) ;
#38296 = CARTESIAN_POINT ( 'NONE',  ( -8.729704736439998669, -77.84765792925898609, 7.043462628994999974 ) ) ;
#38297 = DIRECTION ( 'NONE',  ( 0.9999999924279686647, 0.000000000000000000, 0.0001230612157847738313 ) ) ;
#38298 = CARTESIAN_POINT ( 'NONE',  ( 9.738918081334000831, -77.58012407454400261, 0.1147619655162999963 ) ) ;
#38299 = CARTESIAN_POINT ( 'NONE',  ( 1.541440768196999933, -82.66978111377999028, 0.6318380856084999664 ) ) ;
#38300 = DIRECTION ( 'NONE',  ( 0.7071067811865474617, 0.7071067811865474617, -1.545239644671104046E-10 ) ) ;
#38301 = CARTESIAN_POINT ( 'NONE',  ( 1.512024872110000029, -79.29138868576299615, -0.1127957995495999927 ) ) ;
#38302 = EDGE_LOOP ( 'NONE', ( #44254, #27048, #1602, #38172, #6636 ) ) ;
#38303 = VECTOR ( 'NONE', #17959, 1000.000000000000000 ) ;
#38304 = CARTESIAN_POINT ( 'NONE',  ( -7.000000000000000000, -80.99999999999998579, 0.000000000000000000 ) ) ;
#38305 = CARTESIAN_POINT ( 'NONE',  ( -3.399999999999999911, -78.69999997992952956, 5.715921273723000819E-07 ) ) ;
#38306 = AXIS2_PLACEMENT_3D ( 'NONE', #56687, #7376, #56970 ) ;
#38307 = VERTEX_POINT ( 'NONE', #47558 ) ;
#38308 = AXIS2_PLACEMENT_3D ( 'NONE', #5047, #50510, #13597 ) ;
#38309 = CARTESIAN_POINT ( 'NONE',  ( 0.2086861075963999945, -78.54060936691300299, 1.317203954600000060 ) ) ;
#38310 = EDGE_CURVE ( 'NONE', #5427, #24905, #28929, .T. ) ;
#38311 = CARTESIAN_POINT ( 'NONE',  ( 0.000000000000000000, -81.79999999999998295, 0.000000000000000000 ) ) ;
#38312 = ORIENTED_EDGE ( 'NONE', *, *, #10786, .T. ) ;
#38313 = CARTESIAN_POINT ( 'NONE',  ( 9.596418076563999477, -77.95619656188999613, -7.476047798475000228 ) ) ;
#38314 = CARTESIAN_POINT ( 'NONE',  ( -11.10670190495999954, -77.60177020116098845, 2.709833645475999919 ) ) ;
#38315 = ORIENTED_EDGE ( 'NONE', *, *, #4415, .T. ) ;
#38316 = ORIENTED_EDGE ( 'NONE', *, *, #41867, .F. ) ;
#38317 = CARTESIAN_POINT ( 'NONE',  ( 0.9476663237611181456, -80.40730976135888852, 0.8183754900101951613 ) ) ;
#38318 = CARTESIAN_POINT ( 'NONE',  ( 6.766607812238000008, -76.81907331913100734, -6.412022843746999712 ) ) ;
#38319 = CARTESIAN_POINT ( 'NONE',  ( 9.534323188421000239, -79.25198956143150042, -1.008198710029000189 ) ) ;
#38320 = EDGE_LOOP ( 'NONE', ( #23225, #39117, #30533 ) ) ;
#38321 = CARTESIAN_POINT ( 'NONE',  ( -2.841169247956853106, -2.559397276877021010, 1.638755559622367519 ) ) ;
#38322 = CARTESIAN_POINT ( 'NONE',  ( 2.253937565478000060, -78.21495880092599862, -10.68151722998999986 ) ) ;
#38323 = EDGE_LOOP ( 'NONE', ( #4792, #16368, #26123, #54455, #51852, #12078 ) ) ;
#38324 = CARTESIAN_POINT ( 'NONE',  ( -1.407276357456320737, -80.71461996621154356, -10.68035269161679146 ) ) ;
#38325 = FACE_OUTER_BOUND ( 'NONE', #20766, .T. ) ;
#38326 = CARTESIAN_POINT ( 'NONE',  ( 7.624341766647000362, -18.73514853758999976, -10.42531125024999916 ) ) ;
#38327 = CARTESIAN_POINT ( 'NONE',  ( 5.000000000000000000, -80.49999999999998579, 0.000000000000000000 ) ) ;
#38328 = CARTESIAN_POINT ( 'NONE',  ( -11.37187252477004940, -77.21997671573330990, -3.043002530333297262 ) ) ;
#38329 = CARTESIAN_POINT ( 'NONE',  ( 8.057046250017998901, -76.82309468548459108, -4.844044839845999206 ) ) ;
#38330 = CARTESIAN_POINT ( 'NONE',  ( 6.917788961651000434, -78.82398876163412638, -9.780606322222999083 ) ) ;
#38331 = CARTESIAN_POINT ( 'NONE',  ( 9.611650271896847286, -79.80833333333332291, -5.539808784079878201 ) ) ;
#38332 = CARTESIAN_POINT ( 'NONE',  ( -8.227501432777001966, -24.82538814609000255, 9.516269854983999466 ) ) ;
#38333 = AXIS2_PLACEMENT_3D ( 'NONE', #42007, #1575, #5984 ) ;
#38334 = CARTESIAN_POINT ( 'NONE',  ( 2.484261087175999805, -79.23980496681159025, -3.352388143773000095 ) ) ;
#38335 = ADVANCED_FACE ( 'NONE', ( #57530 ), #39908, .F. ) ;
#38336 = CARTESIAN_POINT ( 'NONE',  ( 4.784380313523554307, -78.06666666666666288, -8.300970689365442468 ) ) ;
#38337 = CARTESIAN_POINT ( 'NONE',  ( 10.15831671673000081, -61.01991983010999832, -7.756223511098000678 ) ) ;
#38338 = DIRECTION ( 'NONE',  ( 0.000000000000000000, 1.000000000000000000, 0.000000000000000000 ) ) ;
#38339 = CARTESIAN_POINT ( 'NONE',  ( -11.80208112487999905, -77.15619080252700712, -3.396125071686999952 ) ) ;
#38340 = CARTESIAN_POINT ( 'NONE',  ( 1.243547092045927949, -78.76458333333332007, 9.500000000000003553 ) ) ;
#38341 = VECTOR ( 'NONE', #23318, 1000.000000000000000 ) ;
#38342 = EDGE_CURVE ( 'NONE', #54925, #57688, #11667, .T. ) ;
#38343 = CARTESIAN_POINT ( 'NONE',  ( 10.93030503950313026, -77.83412702261058769, 4.999052250161460265 ) ) ;
#38344 = CARTESIAN_POINT ( 'NONE',  ( -13.86301033151699791, -46.43897132165000130, -0.1317488955328562361 ) ) ;
#38345 = AXIS2_PLACEMENT_3D ( 'NONE', #47612, #57305, #57015 ) ;
#38346 = EDGE_LOOP ( 'NONE', ( #6373, #20046 ) ) ;
#38347 = CARTESIAN_POINT ( 'NONE',  ( -1.316334517949519833, -80.29447262625133419, -0.8125667813490581315 ) ) ;
#38348 = DIRECTION ( 'NONE',  ( 0.000000000000000000, 0.000000000000000000, -1.000000000000000000 ) ) ;
#38349 = CYLINDRICAL_SURFACE ( 'NONE', #32343, 14.00000000000000000 ) ;
#38350 = CARTESIAN_POINT ( 'NONE',  ( 9.404538367153101319, -78.70366911081997330, 7.521839627124905725 ) ) ;
#38351 = CARTESIAN_POINT ( 'NONE',  ( -2.525108350097000187, -2.446968295937999915, -2.723651764455000457 ) ) ;
#38352 = CARTESIAN_POINT ( 'NONE',  ( -10.02269271100999859, -77.46203272307600685, 6.688901441487999477 ) ) ;
#38353 = CARTESIAN_POINT ( 'NONE',  ( 7.433005562543999467, -77.46490363863499340, -6.293657445383999516 ) ) ;
#38355 = CARTESIAN_POINT ( 'NONE',  ( 10.18496935385000057, -21.75064714707999869, -7.710095619702999947 ) ) ;
#38354 = CARTESIAN_POINT ( 'NONE',  ( -8.943869871800938398, -76.14366878628676716, 7.620587988577864458 ) ) ;
#38356 = CARTESIAN_POINT ( 'NONE',  ( 2.120986319506000140, -78.88603073817900224, 10.70872462160000005 ) ) ;
#38357 = CARTESIAN_POINT ( 'NONE',  ( -10.60025282971301763, -79.58684258122036681, 1.788823804082396940 ) ) ;
#38358 = ORIENTED_EDGE ( 'NONE', *, *, #51404, .T. ) ;
#38359 = CARTESIAN_POINT ( 'NONE',  ( -1.178447680628000205, -80.95308451575900222, -0.9280415206345000723 ) ) ;
#38360 = CARTESIAN_POINT ( 'NONE',  ( 9.492479839331700475, -79.00604488997433350, 0.7216432697597927604 ) ) ;
#38361 = EDGE_CURVE ( 'NONE', #19814, #19162, #34130, .T. ) ;
#38362 = FACE_OUTER_BOUND ( 'NONE', #43915, .T. ) ;
#38363 = CARTESIAN_POINT ( 'NONE',  ( -7.620037246310000789, -60.00567269791999792, 10.53559750860999955 ) ) ;
#38364 = DIRECTION ( 'NONE',  ( -1.000000000000000000, 0.000000000000000000, 0.000000000000000000 ) ) ;
#38365 = CARTESIAN_POINT ( 'NONE',  ( -9.557645832987999412, -79.65522106308299044, -1.471819245595999970 ) ) ;
#38366 = CARTESIAN_POINT ( 'NONE',  ( 1.570796326794910547, -78.03541666666666288, -11.99999999999999822 ) ) ;
#38367 = CARTESIAN_POINT ( 'NONE',  ( -10.71369944335147117, -78.62083333333333712, -2.879226727952084453 ) ) ;
#38368 = ORIENTED_EDGE ( 'NONE', *, *, #20439, .F. ) ;
#38369 = CARTESIAN_POINT ( 'NONE',  ( -4.036005110416000186, -79.18075759821599036, 10.51402051105999824 ) ) ;
#38370 = CARTESIAN_POINT ( 'NONE',  ( -10.31421052434999908, -76.82175206120300004, 3.823226550887000030 ) ) ;
#38371 = CARTESIAN_POINT ( 'NONE',  ( -3.848761171412311999, -79.14836415611753750, -11.19148989879134248 ) ) ;
#38372 = CARTESIAN_POINT ( 'NONE',  ( -14.00000000000000000, -45.91785611817000046, 0.000000000000000000 ) ) ;
#38373 = CARTESIAN_POINT ( 'NONE',  ( 0.7987623000872553503, -81.42017824848964835, 0.9617713037012455279 ) ) ;
#38374 = EDGE_CURVE ( 'NONE', #54466, #54943, #46573, .T. ) ;
#38375 = CARTESIAN_POINT ( 'NONE',  ( 1.030280495153508280, -78.34966520152786984, -0.7508267048928350951 ) ) ;
#38376 = CARTESIAN_POINT ( 'NONE',  ( 11.05000000000000071, -81.00000000000000000, 0.000000000000000000 ) ) ;
#38377 = CARTESIAN_POINT ( 'NONE',  ( -7.601397897754999633, -18.75000000240999753, -10.07627163191000008 ) ) ;
#38378 = ADVANCED_FACE ( 'NONE', ( #8516 ), #1308, .F. ) ;
#38379 = AXIS2_PLACEMENT_3D ( 'NONE', #54544, #50123, #43427 ) ;
#38380 = DIRECTION ( 'NONE',  ( 0.000000000000000000, -1.000000000000000000, 0.000000000000000000 ) ) ;
#38381 = AXIS2_PLACEMENT_3D ( 'NONE', #56727, #8789, #26780 ) ;
#38382 = CARTESIAN_POINT ( 'NONE',  ( 0.6295237254636211199, -78.33333333333334281, 1.092232985442824322 ) ) ;
#38383 = CARTESIAN_POINT ( 'NONE',  ( 12.71005124793928509, -54.50500926681596781, -1.687536500541976903 ) ) ;
#38384 = VERTEX_POINT ( 'NONE', #16810 ) ;
#38385 = AXIS2_PLACEMENT_3D ( 'NONE', #16640, #2777, #25778 ) ;
#38386 = ORIENTED_EDGE ( 'NONE', *, *, #46924, .F. ) ;
#38387 = CARTESIAN_POINT ( 'NONE',  ( -8.813874136147999749, -77.38986986081299335, -8.988208014853000805 ) ) ;
#38388 = CARTESIAN_POINT ( 'NONE',  ( -4.372067062227771750, -78.69186267950118463, -9.823263076180332121 ) ) ;
#38389 = VECTOR ( 'NONE', #37579, 1000.000000000000000 ) ;
#38390 = VERTEX_POINT ( 'NONE', #21518 ) ;
#38391 = CARTESIAN_POINT ( 'NONE',  ( 7.647736468634000140, -18.27704514451999884, 10.13404651205999940 ) ) ;
#38392 = CARTESIAN_POINT ( 'NONE',  ( 9.611650271896829523, -77.49166666666666003, 5.539808784079915505 ) ) ;
#38393 = EDGE_CURVE ( 'NONE', #12955, #10981, #31228, .T. ) ;
#38394 = CARTESIAN_POINT ( 'NONE',  ( 7.220923959705269013, -75.97708333333335418, -9.396085398178609438 ) ) ;
#38395 = CARTESIAN_POINT ( 'NONE',  ( 11.52003294054999927, -78.03939249822001045, 5.205193576094000463 ) ) ;
#38396 = FACE_OUTER_BOUND ( 'NONE', #7755, .T. ) ;
#38397 = DIRECTION ( 'NONE',  ( 0.000000000000000000, -1.000000000000000000, 0.000000000000000000 ) ) ;
#38398 = CARTESIAN_POINT ( 'NONE',  ( 10.18496935386999880, -20.24935285395000051, 7.710095619721000659 ) ) ;
#38399 = CARTESIAN_POINT ( 'NONE',  ( -10.71602610194999805, -79.81002448127239290, 3.314346869870000489 ) ) ;
#38400 = ORIENTED_EDGE ( 'NONE', *, *, #54062, .T. ) ;
#38401 = ORIENTED_EDGE ( 'NONE', *, *, #22513, .F. ) ;
#38402 = CARTESIAN_POINT ( 'NONE',  ( 9.249977667285287808, -77.35017732644061539, 0.02052228013975116935 ) ) ;
#38403 = CARTESIAN_POINT ( 'NONE',  ( -11.00724581733999941, -77.98431219114199564, 0.8512868710715000287 ) ) ;
#38404 = CARTESIAN_POINT ( 'NONE',  ( -10.31421052434999908, -76.82175206120300004, 3.823226550887000030 ) ) ;
#38405 = CARTESIAN_POINT ( 'NONE',  ( 8.282422341201556293, -78.04101043050533804, -7.564594445558528335 ) ) ;
#38406 = UNCERTAINTY_MEASURE_WITH_UNIT (LENGTH_MEASURE( 1.000000000000000082E-05 ), #19998, 'distance_accuracy_value', 'NONE');
#38408 = EDGE_CURVE ( 'NONE', #38188, #21151, #30473, .T. ) ;
#38407 = CARTESIAN_POINT ( 'NONE',  ( 1.045500971020000058, -78.91169582999499710, 0.9575944129536000382 ) ) ;
#38409 = CARTESIAN_POINT ( 'NONE',  ( -9.199999999999999289, -76.00000000000000000, 0.000000000000000000 ) ) ;
#38410 = CARTESIAN_POINT ( 'NONE',  ( -8.485281374238999419, -18.75000000000000000, 8.485281374238999419 ) ) ;
#38411 = CARTESIAN_POINT ( 'NONE',  ( 0.1660104325307999729, -78.19647670854999433, 1.618982269915999916 ) ) ;
#38412 = CARTESIAN_POINT ( 'NONE',  ( -7.682344222570999470, -22.76462890193000277, 10.04116292115999975 ) ) ;
#38413 = EDGE_CURVE ( 'NONE', #41674, #46158, #35366, .T. ) ;
#38414 = CARTESIAN_POINT ( 'NONE',  ( -2.183649677207000206, -78.38389367123097884, 10.83095413486000069 ) ) ;
#38415 = CARTESIAN_POINT ( 'NONE',  ( 11.66950233118999947, -79.38048444465056264, -2.920592611544999606 ) ) ;
#38416 = CARTESIAN_POINT ( 'NONE',  ( -7.710118476736999682, -57.05022860539000362, -10.18499221088999995 ) ) ;
#38417 = CARTESIAN_POINT ( 'NONE',  ( 3.133403074829000268, -82.58532103627599952, 1.663280530810000268 ) ) ;
#38418 = ORIENTED_EDGE ( 'NONE', *, *, #4638, .F. ) ;
#38419 = CARTESIAN_POINT ( 'NONE',  ( -9.705904104064821070, -77.19999999999998863, 5.072841802772233954 ) ) ;
#38420 = CARTESIAN_POINT ( 'NONE',  ( -0.7205381521189000438, -80.92025799034000499, -1.542932836074000003 ) ) ;
#38421 = DIRECTION ( 'NONE',  ( 1.000000000000000000, 0.000000000000000000, 0.000000000000000000 ) ) ;
#38422 = CARTESIAN_POINT ( 'NONE',  ( 4.458743082292000004, -77.41075765253599172, 11.11915799896999957 ) ) ;
#38423 = CARTESIAN_POINT ( 'NONE',  ( -7.633403241821000051, -18.61350283651999860, 10.18127013549000104 ) ) ;
#38424 = AXIS2_PLACEMENT_3D ( 'NONE', #4038, #44788, #22341 ) ;
#38425 = CARTESIAN_POINT ( 'NONE',  ( 1.272562703582658106, -78.00461759078670809, 0.06755297771290638686 ) ) ;
#38426 = CARTESIAN_POINT ( 'NONE',  ( -3.446482552678597600, -2.233460856228320690, 0.7286176306159007909 ) ) ;
#38427 = CARTESIAN_POINT ( 'NONE',  ( 10.68871602397163301, -80.85933999195634669, 1.217520377858459346 ) ) ;
#38428 = CARTESIAN_POINT ( 'NONE',  ( -1.900968108529000000, -77.18800492889859299, -9.219409434742001253 ) ) ;
#38429 = CARTESIAN_POINT ( 'NONE',  ( 1.629367637664000057, -55.11736356569000606, -12.46114270824000059 ) ) ;
#38430 = CARTESIAN_POINT ( 'NONE',  ( -0.8117802668354000550, -77.57800251553000237, -11.00194288205000070 ) ) ;
#38431 = CARTESIAN_POINT ( 'NONE',  ( 10.47020627418439531, -79.22916666666665719, -2.813789756862242974 ) ) ;
#38432 = CARTESIAN_POINT ( 'NONE',  ( -8.904870325259999220, -80.57561547146119096, -6.304511959018999967 ) ) ;
#38433 = CARTESIAN_POINT ( 'NONE',  ( -1.266772977591273719, -81.64127194508073160, 0.1360379414319277391 ) ) ;
#38434 = VERTEX_POINT ( 'NONE', #34795 ) ;
#38435 = DIRECTION ( 'NONE',  ( 1.000000000000000000, 0.000000000000000000, 0.000000000000000000 ) ) ;
#38436 = CARTESIAN_POINT ( 'NONE',  ( 11.74484861916918277, -76.95718971417709042, 1.539165031385370863 ) ) ;
#38437 = CARTESIAN_POINT ( 'NONE',  ( -0.5045596072229000528, -61.93528913004999481, -12.66210649714999903 ) ) ;
#38438 = AXIS2_PLACEMENT_3D ( 'NONE', #18356, #49063, #40194 ) ;
#38439 = DIRECTION ( 'NONE',  ( -1.996569343957000276E-14, 1.000000000000000000, -1.048636824995000113E-10 ) ) ;
#38440 = CARTESIAN_POINT ( 'NONE',  ( -0.9512330062464999791, -78.14786231073598799, 11.17646036812999988 ) ) ;
#38441 = CARTESIAN_POINT ( 'NONE',  ( -10.65673661723999999, -78.85061951977299088, 2.626400817186000047 ) ) ;
#38442 = CARTESIAN_POINT ( 'NONE',  ( 9.395758989562999375, -24.70491532583000449, -8.188252216825999241 ) ) ;
#38443 = CARTESIAN_POINT ( 'NONE',  ( 2.414596980239923418, -84.17291666555200891, 3.253361081415106604 ) ) ;
#38444 = CARTESIAN_POINT ( 'NONE',  ( 0.000000000000000000, -75.00000000000000000, 7.200000000000000178 ) ) ;
#38445 = CARTESIAN_POINT ( 'NONE',  ( 10.11501736609056579, -78.49136027514339276, 5.984602011854717851 ) ) ;
#38446 = CARTESIAN_POINT ( 'NONE',  ( -10.41172548049582680, -55.27988211093989435, -7.610718780863655830 ) ) ;
#38447 = VERTEX_POINT ( 'NONE', #53110 ) ;
#38448 = LINE ( 'NONE', #47918, #2233 ) ;
#38449 = CONICAL_SURFACE ( 'NONE', #764, 13.94999999997000018, 0.7853981633972997312 ) ;
#38450 = CARTESIAN_POINT ( 'NONE',  ( 7.396918292183150001, -78.19791666666664298, -5.684557159767978263 ) ) ;
#38451 = CARTESIAN_POINT ( 'NONE',  ( 4.145744906942999464, -79.33417387541800281, -10.47576887544000002 ) ) ;
#38452 = CARTESIAN_POINT ( 'NONE',  ( -9.596002108778161954, -76.85208333333332575, -7.374560639698982456 ) ) ;
#38453 = FACE_OUTER_BOUND ( 'NONE', #17888, .T. ) ;
#38454 = CARTESIAN_POINT ( 'NONE',  ( 0.5999999999999999778, -5.000000000000000000, -0.5999999999999999778 ) ) ;
#38455 = CARTESIAN_POINT ( 'NONE',  ( -1.503028869898288322, -81.84122243630122284, 0.1554063332427757516 ) ) ;
#38456 = EDGE_CURVE ( 'NONE', #8613, #13664, #2970, .T. ) ;
#38457 = PRODUCT ( 'Push Button Cover', 'Push Button Cover', '', ( #55615 ) ) ;
#38458 = CARTESIAN_POINT ( 'NONE',  ( 0.6359605339382402578, -79.76804382808089144, -1.076489120615609307 ) ) ;
#38459 = CARTESIAN_POINT ( 'NONE',  ( -10.10712711931551944, -54.33345760842059491, 7.860996423901147168 ) ) ;
#38460 = ORIENTED_EDGE ( 'NONE', *, *, #24981, .T. ) ;
#38461 = CARTESIAN_POINT ( 'NONE',  ( 1.931043742978000077, -22.77795407709999864, 12.75763395695999947 ) ) ;
#38462 = B_SPLINE_CURVE_WITH_KNOTS ( 'NONE', 3,
 ( #51690, #46223, #36173, #28170 ),
 .UNSPECIFIED., .F., .F.,
 ( 4, 4 ),
 ( 0.000000000000000000, 1.000000000000000000 ),
 .UNSPECIFIED. ) ;
#38463 = CARTESIAN_POINT ( 'NONE',  ( -12.59651352881000008, -23.39056208384000257, 1.801710201210000140 ) ) ;
#38464 = VERTEX_POINT ( 'NONE', #30362 ) ;
#38465 = ORIENTED_EDGE ( 'NONE', *, *, #55726, .F. ) ;
#38466 = LINE ( 'NONE', #20184, #8849 ) ;
#38467 = ORIENTED_EDGE ( 'NONE', *, *, #52233, .T. ) ;
#38468 = CARTESIAN_POINT ( 'NONE',  ( 8.645097183540606522, -79.96524141418557008, -4.039558020937342064 ) ) ;
#38469 = ORIENTED_EDGE ( 'NONE', *, *, #22102, .F. ) ;
#38470 = CARTESIAN_POINT ( 'NONE',  ( -9.359443164323526076, -81.00000000000002842, -5.435958517830047576 ) ) ;
#38471 = CARTESIAN_POINT ( 'NONE',  ( 3.425937024882473377E-06, -77.82827182887865547, -1.422119424801547627 ) ) ;
#38472 = EDGE_CURVE ( 'NONE', #22699, #25098, #29421, .T. ) ;
#38473 = CARTESIAN_POINT ( 'NONE',  ( -1.500000000000000222, -78.01041666666668561, -0.1963495408493622085 ) ) ;
#38474 = CARTESIAN_POINT ( 'NONE',  ( 8.283364115789000337, -78.98796332859900815, 5.234906771447999319 ) ) ;
#38475 = ADVANCED_FACE ( 'NONE', ( #49267 ), #14468, .F. ) ;
#38476 = CARTESIAN_POINT ( 'NONE',  ( 5.628633445105355904, -79.32351257642946507, 7.438899466706690333 ) ) ;
#38477 = VERTEX_POINT ( 'NONE', #20943 ) ;
#38478 = ORIENTED_EDGE ( 'NONE', *, *, #30847, .F. ) ;
#38479 = CARTESIAN_POINT ( 'NONE',  ( -6.608220602749067751, -77.53848782482791080, 6.472502597521285317 ) ) ;
#38480 = CARTESIAN_POINT ( 'NONE',  ( -12.74331206680846407, -23.52649290806275317, 1.980611467279653981 ) ) ;
#38481 = CARTESIAN_POINT ( 'NONE',  ( 11.00000000000000000, -79.84999999999999432, 0.000000000000000000 ) ) ;
#38482 = CARTESIAN_POINT ( 'NONE',  ( 8.553489385229999797, -79.11597592151899505, 4.133741566275999979 ) ) ;
#38483 = CARTESIAN_POINT ( 'NONE',  ( -0.5731199659189539775, -86.09999999999978115, 4.609165628485380140 ) ) ;
#38484 = AXIS2_PLACEMENT_3D ( 'NONE', #19438, #41870, #50451 ) ;
#38485 = CARTESIAN_POINT ( 'NONE',  ( -9.400098536042321484, -79.41121447921612742, -1.373460959377882817 ) ) ;
#38486 = CARTESIAN_POINT ( 'NONE',  ( -10.35845616727999996, -18.70221404512000163, 7.627487606607999737 ) ) ;
#38487 = CARTESIAN_POINT ( 'NONE',  ( -3.140974612311405512, -76.79583333333332007, 11.68767212001977640 ) ) ;
#38488 = EDGE_CURVE ( 'NONE', #49656, #48292, #30652, .T. ) ;
#38489 = CARTESIAN_POINT ( 'NONE',  ( 0.8701072296501000114, -80.10229747532000033, 1.463806805601000072 ) ) ;
#38490 = CARTESIAN_POINT ( 'NONE',  ( -7.919595949288999570, -55.65000000893999754, -9.050966798898000931 ) ) ;
#38491 = B_SPLINE_CURVE_WITH_KNOTS ( 'NONE', 3,
 ( #18005, #55697, #24103, #31553 ),
 .UNSPECIFIED., .F., .F.,
 ( 4, 4 ),
 ( 0.000000000000000000, 1.000000000000000000 ),
 .UNSPECIFIED. ) ;
#38492 = CARTESIAN_POINT ( 'NONE',  ( -9.643342484248000446, -53.85965044121000034, 8.260141428653000162 ) ) ;
#38493 = CARTESIAN_POINT ( 'NONE',  ( 1.914689014128999833, -78.36623667140099769, 9.610012265935001352 ) ) ;
#38494 = CARTESIAN_POINT ( 'NONE',  ( 12.56594317984999876, -18.75000000536999778, -1.750000000000000000 ) ) ;
#38495 = CARTESIAN_POINT ( 'NONE',  ( 1.930989179114000143, -21.75453807238000081, -12.80896991324000034 ) ) ;
#38497 = CARTESIAN_POINT ( 'NONE',  ( 1.324344358081999795, -79.02505838911800140, 0.1571239973995999795 ) ) ;
#38496 = CARTESIAN_POINT ( 'NONE',  ( -10.14999999999999858, -86.39999999999999147, 0.000000000000000000 ) ) ;
#38498 = CARTESIAN_POINT ( 'NONE',  ( -9.599999999999999645, -87.59999999999999432, 0.000000000000000000 ) ) ;
#38499 = CARTESIAN_POINT ( 'NONE',  ( -11.00182790298000057, -80.03886997964798411, 2.541920722147000156 ) ) ;
#38500 = CARTESIAN_POINT ( 'NONE',  ( -0.5900578684300998855, -82.22042515683899921, -1.108170840844000082 ) ) ;
#38501 = ADVANCED_FACE ( 'NONE', ( #44248 ), #21804, .F. ) ;
#38502 = CARTESIAN_POINT ( 'NONE',  ( -2.422546195149999804, -2.281904343863999873, 2.935532677474999907 ) ) ;
#38503 = CARTESIAN_POINT ( 'NONE',  ( -12.00000000000000000, -23.25000000000000000, 1.250000000000000000 ) ) ;
#38504 = EDGE_LOOP ( 'NONE', ( #15000, #32485, #8395, #19903 ) ) ;
#38505 = DIRECTION ( 'NONE',  ( 0.000000000000000000, -1.000000000000000000, 0.000000000000000000 ) ) ;
#38506 = CARTESIAN_POINT ( 'NONE',  ( -0.5999999999999999778, -5.000000000000000000, -4.000000000000000000 ) ) ;
#38507 = EDGE_CURVE ( 'NONE', #13166, #10604, #12089, .T. ) ;
#38508 = CARTESIAN_POINT ( 'NONE',  ( -12.50412785609311683, -61.31985834570146920, 1.235051470172120469 ) ) ;
#38509 = CARTESIAN_POINT ( 'NONE',  ( 0.8464868648045736910, -78.41589811855170922, 0.9196883286881438746 ) ) ;
#38510 = CARTESIAN_POINT ( 'NONE',  ( -9.520759628685000919, -79.45279990477098409, 0.4955186682686999466 ) ) ;
#38511 = CARTESIAN_POINT ( 'NONE',  ( -5.413709697356376083, -77.01682545481338593, 9.392928511438244144 ) ) ;
#38512 = CARTESIAN_POINT ( 'NONE',  ( 9.364915788055299117, -79.11789567091318531, 2.156547985526540145 ) ) ;
#38513 = CARTESIAN_POINT ( 'NONE',  ( 1.044910384896000188, -61.85526494161999977, 12.77260826204000033 ) ) ;
#38514 = CARTESIAN_POINT ( 'NONE',  ( 6.954077596906981462, -79.08999999999998920, -6.533946999607122663 ) ) ;
#38515 = AXIS2_PLACEMENT_3D ( 'NONE', #25698, #43727, #57289 ) ;
#38516 = CARTESIAN_POINT ( 'NONE',  ( -17.50000000000000000, -15.06282895647999887, -3.979079565841000010E-10 ) ) ;
#38517 = CARTESIAN_POINT ( 'NONE',  ( -0.03769866006636662936, -78.67389998729011324, 3.999822347433201308 ) ) ;
#38518 = CARTESIAN_POINT ( 'NONE',  ( -6.501459582243999336, -77.88191509035799243, -8.943106734674001856 ) ) ;
#38519 = CARTESIAN_POINT ( 'NONE',  ( 6.822138660719681447, -76.37385742326372906, -9.577683154303922919 ) ) ;
#38520 = CARTESIAN_POINT ( 'NONE',  ( 7.110505486850000167, -78.39021989260101009, -8.302835368086999068 ) ) ;
#38521 = CARTESIAN_POINT ( 'NONE',  ( -7.603664017117999663, -78.59644514476066490, 6.060370778711000384 ) ) ;
#38522 = CARTESIAN_POINT ( 'NONE',  ( -0.9747649511251000876, -79.25484333926999625, 1.348101445433000034 ) ) ;
#38523 = CARTESIAN_POINT ( 'NONE',  ( -3.831287612370999796, -76.86181488578978360, -8.693171758988999187 ) ) ;
#38524 = CARTESIAN_POINT ( 'NONE',  ( 1.813979036992999783, -79.36964415034600506, 9.381055131006998948 ) ) ;
#38525 = CARTESIAN_POINT ( 'NONE',  ( 1.010606015627170340, -3.450854123697218334, 3.127970707052925015 ) ) ;
#38526 = CARTESIAN_POINT ( 'NONE',  ( 7.163861093844410277, -80.28312376644485937, -8.015740724809139905 ) ) ;
#38527 = DIRECTION ( 'NONE',  ( -1.000000000000000000, 0.000000000000000000, 0.000000000000000000 ) ) ;
#38528 = CARTESIAN_POINT ( 'NONE',  ( 7.316118016526345080, -75.80000000000001137, 9.517257946189689122 ) ) ;
#38529 = AXIS2_PLACEMENT_3D ( 'NONE', #4804, #49089, #26926 ) ;
#38530 = CARTESIAN_POINT ( 'NONE',  ( 11.90415444617999974, -79.73682346591400005, -1.731350929957999885 ) ) ;
#38531 = CARTESIAN_POINT ( 'NONE',  ( 5.838193839761673054, -78.62291666666669698, 7.596835002782728274 ) ) ;
#38532 = CARTESIAN_POINT ( 'NONE',  ( 9.414214675708999280, -79.52717617799699212, -6.181142822975999707 ) ) ;
#38533 = ORIENTED_EDGE ( 'NONE', *, *, #14271, .F. ) ;
#38534 = CARTESIAN_POINT ( 'NONE',  ( -1.722320549981885440, -24.23663688825939388, 12.71171904436535272 ) ) ;
#38535 = ORIENTED_EDGE ( 'NONE', *, *, #57438, .T. ) ;
#38536 = ORIENTED_EDGE ( 'NONE', *, *, #53765, .T. ) ;
#38537 = CARTESIAN_POINT ( 'NONE',  ( 8.414570695956999913, -59.94999999967000548, -8.414570695956999913 ) ) ;
#38538 = CARTESIAN_POINT ( 'NONE',  ( -11.75000000000000355, -77.31041666666665435, -1.538071403320004249 ) ) ;
#38539 = CARTESIAN_POINT ( 'NONE',  ( 3.222911977508000181, -79.40398657535959615, -1.475740419821999883 ) ) ;
#38540 = CARTESIAN_POINT ( 'NONE',  ( 6.480685897343804847, -79.21501409628969270, 6.948370975495136825 ) ) ;
#38541 = B_SPLINE_SURFACE_WITH_KNOTS ( 'NONE', 3, 3, ( 
 ( #52938, #22211, #57646, #12205 ),
 ( #35481, #8935, #4214, #40222 ),
 ( #53221, #26924, #44955, #3913 ),
 ( #21916, #43803, #21633, #3349 ),
 ( #30191, #17202, #4509, #53812 ),
 ( #13053, #48512, #21345, #3629 ),
 ( #35190, #12488, #39357, #17797 ),
 ( #26054, #22511, #26625, #31346 ),
 ( #39638, #35783, #49388, #12769 ),
 ( #40521, #39924, #114, #57939 ),
 ( #17494, #52651, #48240, #7777 ) ),
 .UNSPECIFIED., .F., .F., .F.,
 ( 4, 1, 1, 1, 1, 1, 1, 1, 4 ),
 ( 4, 4 ),
 ( -0.01994574723510000175, 0.000000000000000000, 0.1666666666667000196, 0.3333333333333000081, 0.5000000000000000000, 0.6666666666667000474, 0.8333333333333000637, 1.000000000000000000, 1.020511277925000071 ),
 ( -0.3582002740325999635, 1.358574366096999997 ),
 .UNSPECIFIED. ) ;
#38542 = ORIENTED_EDGE ( 'NONE', *, *, #44273, .T. ) ;
#38543 = CARTESIAN_POINT ( 'NONE',  ( 7.601397897754999633, -55.55000000278000272, -10.07627163191000008 ) ) ;
#38544 = ORIENTED_EDGE ( 'NONE', *, *, #17656, .T. ) ;
#38545 = CARTESIAN_POINT ( 'NONE',  ( 1.891006765463000061, -2.727532913352999966, -2.827272806746000011 ) ) ;
#38546 = ORIENTED_EDGE ( 'NONE', *, *, #8823, .T. ) ;
#38547 = CARTESIAN_POINT ( 'NONE',  ( -2.318113117698174186, -79.65520282387936390, -9.269879263659483115 ) ) ;
#38548 = CARTESIAN_POINT ( 'NONE',  ( 1.301538823741287043, -79.04398425417873852, 0.8091645586960490855 ) ) ;
#38549 = CARTESIAN_POINT ( 'NONE',  ( -1.293105744743758390, -79.79999999999998295, -11.73994710747565229 ) ) ;
#38550 = CARTESIAN_POINT ( 'NONE',  ( -7.786690763151178807, -80.03945749923617825, 7.436444533740759866 ) ) ;
#38551 = DIRECTION ( 'NONE',  ( 0.000000000000000000, -1.000000000000000000, 0.000000000000000000 ) ) ;
#38552 = CIRCLE ( 'NONE', #55535, 1.749999999999998446 ) ;
#38553 = FACE_OUTER_BOUND ( 'NONE', #30059, .T. ) ;
#38554 = CARTESIAN_POINT ( 'NONE',  ( 7.995633008690000487, -76.64550778514200147, 7.819446035993999899 ) ) ;
#38555 = CYLINDRICAL_SURFACE ( 'NONE', #42954, 1.250000000000000000 ) ;
#38556 = EDGE_CURVE ( 'NONE', #34384, #49070, #44584, .T. ) ;
#38557 = CARTESIAN_POINT ( 'NONE',  ( -1.168006160022410755, -81.29468525113304622, 0.9590183425694498442 ) ) ;
#38558 = CARTESIAN_POINT ( 'NONE',  ( -4.975971545690999420, -76.80307774425399714, 9.937770923463000727 ) ) ;
#38559 = CARTESIAN_POINT ( 'NONE',  ( -5.122414477196733706, -78.67842178786030161, -7.702078103099229800 ) ) ;
#38560 = CARTESIAN_POINT ( 'NONE',  ( 0.2659376973789999710, -79.81908850788599352, -1.306848610430999980 ) ) ;
#38561 = CYLINDRICAL_SURFACE ( 'NONE', #7286, 0.5000000000000006661 ) ;
#38562 = CARTESIAN_POINT ( 'NONE',  ( 0.04193593510216304943, -61.81009741308703553, -12.50649570009237088 ) ) ;
#38563 = CARTESIAN_POINT ( 'NONE',  ( 0.7976678868801999611, -81.08317549782599087, 3.499637616860999945 ) ) ;
#38564 = CARTESIAN_POINT ( 'NONE',  ( -0.4688094130881000354, -79.13080494938900245, -12.19136368054000030 ) ) ;
#38565 = CARTESIAN_POINT ( 'NONE',  ( -10.63638328646205977, -78.08841358195864757, 1.565909971404836787 ) ) ;
#38566 = AXIS2_PLACEMENT_3D ( 'NONE', #46792, #6316, #17193 ) ;
#38567 = DIRECTION ( 'NONE',  ( 0.000000000000000000, -1.000000000000000000, -3.571217395878000445E-14 ) ) ;
#38568 = DIRECTION ( 'NONE',  ( 0.000000000000000000, -1.000000000000000000, 0.000000000000000000 ) ) ;
#38569 = CARTESIAN_POINT ( 'NONE',  ( -1.472218728959000078, -82.98374735065199559, 3.224520696334999936 ) ) ;
#38570 = CARTESIAN_POINT ( 'NONE',  ( -9.852011461280598681, -76.24562891425179600, -6.431142245721705564 ) ) ;
#38571 = CARTESIAN_POINT ( 'NONE',  ( 10.21380041495000057, -19.22847221992000044, 7.668936932643000581 ) ) ;
#38572 = CARTESIAN_POINT ( 'NONE',  ( -7.981656248376999940, -61.51865039470999363, -10.08154475893999980 ) ) ;
#38573 = EDGE_CURVE ( 'NONE', #24315, #3549, #54436, .T. ) ;
#38574 = CARTESIAN_POINT ( 'NONE',  ( 4.484526869169066288, -79.14462836071079721, 11.18137712903838299 ) ) ;
#38575 = CARTESIAN_POINT ( 'NONE',  ( 10.18589234709999936, -60.08917565288000162, 7.641012386057000505 ) ) ;
#38576 = DIRECTION ( 'NONE',  ( 0.000000000000000000, 0.000000000000000000, -1.000000000000000000 ) ) ;
#38577 = DIRECTION ( 'NONE',  ( -1.000000000000000000, 0.000000000000000000, 0.000000000000000000 ) ) ;
#38578 = CARTESIAN_POINT ( 'NONE',  ( -7.351123050927758307, -78.01612418245753133, -7.965508956423190234 ) ) ;
#38579 = CARTESIAN_POINT ( 'NONE',  ( -11.75000000000000000, -78.20000000000000284, 1.702919296826999607E-14 ) ) ;
#38580 = DIRECTION ( 'NONE',  ( 0.000000000000000000, -1.000000000000000000, 0.000000000000000000 ) ) ;
#38581 = CARTESIAN_POINT ( 'NONE',  ( 12.22350170820999971, -76.34339105127999403, 1.846593319174999914 ) ) ;
#38582 = VERTEX_POINT ( 'NONE', #50159 ) ;
#38583 = CARTESIAN_POINT ( 'NONE',  ( -11.03620408507000050, -80.26607873772769608, -2.260839449595000161 ) ) ;
#38584 = LINE ( 'NONE', #48330, #5951 ) ;
#38585 = AXIS2_PLACEMENT_3D ( 'NONE', #19314, #42037, #51783 ) ;
#38586 = CARTESIAN_POINT ( 'NONE',  ( 12.66322140213000047, -61.98161935699999958, 0.1487435796151000134 ) ) ;
#38587 = CARTESIAN_POINT ( 'NONE',  ( 9.328308112513999717, -79.06345638111000085, 8.294084752732000965 ) ) ;
#38588 = DIRECTION ( 'NONE',  ( 0.6489586469979888861, 0.04890178911492917835, 0.7592504787669867028 ) ) ;
#38589 = CARTESIAN_POINT ( 'NONE',  ( -9.554254755627999529, -78.38301937267999620, 1.212198840764999952 ) ) ;
#38590 = DIRECTION ( 'NONE',  ( 0.000000000000000000, 0.000000000000000000, 1.000000000000000000 ) ) ;
#38591 = CARTESIAN_POINT ( 'NONE',  ( 2.042564453799718294, -79.96020142208192283, 10.55469377556154242 ) ) ;
#38592 = LINE ( 'NONE', #43321, #23596 ) ;
#38593 = EDGE_CURVE ( 'NONE', #36429, #26795, #50312, .T. ) ;
#38594 = ORIENTED_EDGE ( 'NONE', *, *, #39787, .F. ) ;
#38595 = CARTESIAN_POINT ( 'NONE',  ( 10.70940577679425409, -77.34266587486128230, -1.002872783366832499 ) ) ;
#38596 = FACE_OUTER_BOUND ( 'NONE', #27562, .T. ) ;
#38597 = AXIS2_PLACEMENT_3D ( 'NONE', #8077, #52386, #30503 ) ;
#38598 = CARTESIAN_POINT ( 'NONE',  ( -1.003981881343347426, -78.85407511475472120, -3.332975353450012168 ) ) ;
#38599 = EDGE_LOOP ( 'NONE', ( #51367, #17191, #50611, #30103 ) ) ;
#38600 = CARTESIAN_POINT ( 'NONE',  ( -9.837756817742013382, -61.11467795346588616, -7.850057933508078456 ) ) ;
#38601 = CARTESIAN_POINT ( 'NONE',  ( -1.112403273011567162, -80.63938135327609302, -0.5932074133774921654 ) ) ;
#38602 = VERTEX_POINT ( 'NONE', #27981 ) ;
#38603 = CARTESIAN_POINT ( 'NONE',  ( 2.974124060854000273, -79.04598695555699805, 11.51680281503000103 ) ) ;
#38604 = CARTESIAN_POINT ( 'NONE',  ( 6.991733533204999240, -78.23490392501999224, -8.905552786469000281 ) ) ;
#38605 = CIRCLE ( 'NONE', #7511, 14.00000000000000000 ) ;
#38606 = ORIENTED_EDGE ( 'NONE', *, *, #22137, .T. ) ;
#38607 = EDGE_LOOP ( 'NONE', ( #52774, #20183, #5147, #54793, #46017, #54771, #52098, #22038, #42698, #36350, #57234, #14313 ) ) ;
#38608 = AXIS2_PLACEMENT_3D ( 'NONE', #462, #45609, #13407 ) ;
#38609 = CARTESIAN_POINT ( 'NONE',  ( -0.2479305816249914307, -80.49105691730132150, 1.225069668416682855 ) ) ;
#38610 = CARTESIAN_POINT ( 'NONE',  ( -3.451879464883000015, -86.39318692756398832, 1.536875756067000109 ) ) ;
#38611 = CARTESIAN_POINT ( 'NONE',  ( -0.6514213267380000172, -80.01047135062401594, 9.745581310452999801 ) ) ;
#38612 = EDGE_LOOP ( 'NONE', ( #21675, #37919, #52941, #15971, #21976, #16656, #28149, #38401, #1683, #6380, #9202 ) ) ;
#38613 = CARTESIAN_POINT ( 'NONE',  ( 12.54976795928000044, -53.75224499974000025, -0.05636009750360999881 ) ) ;
#38614 = CARTESIAN_POINT ( 'NONE',  ( 9.849799932654001111, -79.35888520700200388, 4.707101791649999534 ) ) ;
#38615 = ORIENTED_EDGE ( 'NONE', *, *, #38802, .T. ) ;
#38616 = CARTESIAN_POINT ( 'NONE',  ( 1.046213688572526390, -79.35145855826110051, -0.7275327676939092880 ) ) ;
#38617 = CARTESIAN_POINT ( 'NONE',  ( -9.391369684923001060, -76.99806915034599797, 1.399863080762999923 ) ) ;
#38618 = CARTESIAN_POINT ( 'NONE',  ( 7.633088938737000007, -55.40992532391999958, 10.18115029110999892 ) ) ;
#38619 = DIRECTION ( 'NONE',  ( -0.7071067811865474617, 0.000000000000000000, -0.7071067811865474617 ) ) ;
#38620 = CARTESIAN_POINT ( 'NONE',  ( -1.460959015002474493, -78.37916666666666288, 0.3926218265389144757 ) ) ;
#38621 = CARTESIAN_POINT ( 'NONE',  ( -7.224190341809336502, -77.27152570786351760, -9.395875115591328708 ) ) ;
#38622 = ADVANCED_FACE ( 'NONE', ( #55149 ), #50449, .F. ) ;
#38623 = CARTESIAN_POINT ( 'NONE',  ( 7.494231858469171392, -80.53311548344800030, -8.337931667626193644 ) ) ;
#38624 = CARTESIAN_POINT ( 'NONE',  ( -7.615853692923001184, -78.57982492282013709, 9.247423260716001181 ) ) ;
#38625 = CARTESIAN_POINT ( 'NONE',  ( -1.828200671114641018, -81.43645834279209339, 3.614657775617112545 ) ) ;
#38626 = ADVANCED_FACE ( 'NONE', ( #41576 ), #46029, .F. ) ;
#38627 = CARTESIAN_POINT ( 'NONE',  ( 10.69843650790000034, -76.23917683518000388, 6.089250768039999429 ) ) ;
#38628 = CARTESIAN_POINT ( 'NONE',  ( 3.793437728763999761, -79.36632046129089701, -1.736771565640999881 ) ) ;
#38629 = CARTESIAN_POINT ( 'NONE',  ( -9.500000000000001776, -77.91041666666669130, -1.243547092045959923 ) ) ;
#38630 = CARTESIAN_POINT ( 'NONE',  ( 9.213114944054998645, -61.80524898723000149, -8.533795138624000742 ) ) ;
#38631 = CARTESIAN_POINT ( 'NONE',  ( -11.38660623898999980, -79.01294608163999555, -4.554589311945999697 ) ) ;
#38632 = CARTESIAN_POINT ( 'NONE',  ( 0.000000000000000000, -80.59999999999999432, 0.000000000000000000 ) ) ;
#38633 = CARTESIAN_POINT ( 'NONE',  ( -17.50000000000000000, -57.79999999999999716, 0.000000000000000000 ) ) ;
#38634 = FACE_OUTER_BOUND ( 'NONE', #11043, .T. ) ;
#38635 = CARTESIAN_POINT ( 'NONE',  ( 3.140974612311377090, -77.94583333333332575, -11.68767212001978528 ) ) ;
#38636 = EDGE_CURVE ( 'NONE', #50254, #900, #38031, .T. ) ;
#38637 = ORIENTED_EDGE ( 'NONE', *, *, #43247, .F. ) ;
#38638 = CARTESIAN_POINT ( 'NONE',  ( -1.216363293580657867, -80.80055608065869421, -0.8954020866757705921 ) ) ;
#38639 = CARTESIAN_POINT ( 'NONE',  ( -9.269456094077998642, -77.52182670896797845, -0.1220293046851000096 ) ) ;
#38640 = DIRECTION ( 'NONE',  ( 1.000000000000000000, 0.000000000000000000, 0.000000000000000000 ) ) ;
#38641 = CARTESIAN_POINT ( 'NONE',  ( -1.460959015002473382, -78.52083333333334281, -0.3926218265389205819 ) ) ;
#38642 = CARTESIAN_POINT ( 'NONE',  ( 2.804370767623999949, -2.074558083080999982, -2.435155557110000313 ) ) ;
#38643 = CARTESIAN_POINT ( 'NONE',  ( 3.299676814977999584, -78.58799553730899845, -11.70874303878999889 ) ) ;
#38644 = CARTESIAN_POINT ( 'NONE',  ( 1.406250000003000045, -82.09374999999700151, -9.314605757769000352E-11 ) ) ;
#38646 = FACE_OUTER_BOUND ( 'NONE', #42748, .T. ) ;
#38645 = CARTESIAN_POINT ( 'NONE',  ( 12.00000000000000000, -18.84999999999999787, 0.000000000000000000 ) ) ;
#38647 = CYLINDRICAL_SURFACE ( 'NONE', #5918, 9.250000000000000000 ) ;
#38648 = VERTEX_POINT ( 'NONE', #27106 ) ;
#38649 = CARTESIAN_POINT ( 'NONE',  ( 14.00000000000000000, -46.09579702914000165, -3.101615809226999909E-11 ) ) ;
#38650 = CARTESIAN_POINT ( 'NONE',  ( -6.534644050777999702, -79.11178473073800888, 10.11388646907000144 ) ) ;
#38651 = CARTESIAN_POINT ( 'NONE',  ( -1.763894203521005233, -79.36019707299011827, -9.362682977635801151 ) ) ;
#38652 = CARTESIAN_POINT ( 'NONE',  ( 0.000000000000000000, -74.64999999999999147, 0.000000000000000000 ) ) ;
#38653 = CARTESIAN_POINT ( 'NONE',  ( -7.948089776799000639, -61.24033979686999629, 9.636757666110000287 ) ) ;
#38654 = LINE ( 'NONE', #42232, #16646 ) ;
#38655 = CARTESIAN_POINT ( 'NONE',  ( 1.635612940292999973, -79.21786873972098419, -9.418908357094000650 ) ) ;
#38656 = DIRECTION ( 'NONE',  ( -1.000000000000000000, 0.000000000000000000, 0.000000000000000000 ) ) ;
#38657 = CARTESIAN_POINT ( 'NONE',  ( -12.70395600756426724, -54.19327811275147155, -1.447166682400345294 ) ) ;
#38658 = ORIENTED_EDGE ( 'NONE', *, *, #44954, .T. ) ;
#38659 = DIRECTION ( 'NONE',  ( 0.000000000000000000, 1.000000000000000000, 0.000000000000000000 ) ) ;
#38660 = CARTESIAN_POINT ( 'NONE',  ( 11.42348641225163242, -79.32084716335937458, 3.093858311050987631 ) ) ;
#38661 = CARTESIAN_POINT ( 'NONE',  ( -2.038544192961673218, -78.67390000031815589, 3.380937561918606615 ) ) ;
#38662 = CARTESIAN_POINT ( 'NONE',  ( 0.8729495473840620523, -81.41394231601826448, 0.8942802001960106217 ) ) ;
#38663 = CARTESIAN_POINT ( 'NONE',  ( -1.445929428138999828, -80.28824903432000326, 0.8273736140038000508 ) ) ;
#38664 = ORIENTED_EDGE ( 'NONE', *, *, #29472, .F. ) ;
#38665 = AXIS2_PLACEMENT_3D ( 'NONE', #23823, #9968, #1127 ) ;
#38666 = CARTESIAN_POINT ( 'NONE',  ( -1.112997722094761111, -78.19065038299876846, -0.6198689731120797797 ) ) ;
#38667 = CARTESIAN_POINT ( 'NONE',  ( 1.218263462486750326, -82.32982652230532494, -0.3278909641266472552 ) ) ;
#38668 = CARTESIAN_POINT ( 'NONE',  ( 2.062673488410000200, -55.47547726255000100, -12.82904109059999875 ) ) ;
#38669 = ADVANCED_FACE ( 'NONE', ( #45143 ), #57738, .T. ) ;
#38670 = FACE_OUTER_BOUND ( 'NONE', #20466, .T. ) ;
#38671 = CARTESIAN_POINT ( 'NONE',  ( -7.357969701303999521, -79.88385172005297363, 8.079184909054573538 ) ) ;
#38672 = DIRECTION ( 'NONE',  ( -1.000000000000000000, 0.000000000000000000, 0.000000000000000000 ) ) ;
#38673 = VERTEX_POINT ( 'NONE', #24735 ) ;
#38674 = ORIENTED_EDGE ( 'NONE', *, *, #38831, .F. ) ;
#38675 = CARTESIAN_POINT ( 'NONE',  ( -11.02398976105000017, -76.29757433877699668, -5.829948365135000365 ) ) ;
#38676 = CARTESIAN_POINT ( 'NONE',  ( 0.01553455395726060714, -78.72521037431218360, -10.74994277546958266 ) ) ;
#38677 = ORIENTED_EDGE ( 'NONE', *, *, #52545, .T. ) ;
#38678 = CARTESIAN_POINT ( 'NONE',  ( 9.650965486090999690, -17.06598967526999999, 8.252456812006998987 ) ) ;
#38679 = STYLED_ITEM ( 'NONE', ( #3966 ), #55564 ) ;
#38680 = DIRECTION ( 'NONE',  ( 0.000000000000000000, -0.7071067811866525998, -0.7071067811864425456 ) ) ;
#38681 = CIRCLE ( 'NONE', #7467, 0.6000000000000008660 ) ;
#38682 = CARTESIAN_POINT ( 'NONE',  ( 1.931736162948486379, -55.03329604253293184, 12.72978979887180095 ) ) ;
#38683 = CARTESIAN_POINT ( 'NONE',  ( -9.533257042556000371, -78.61836734003000515, 6.958047573390000018 ) ) ;
#38684 = CARTESIAN_POINT ( 'NONE',  ( -0.7036264152036126873, -79.71981223434178787, -10.74968282753707882 ) ) ;
#38685 = FACE_BOUND ( 'NONE', #56059, .T. ) ;
#38686 = CARTESIAN_POINT ( 'NONE',  ( 6.000000000000000000, -81.99999999999998579, 0.000000000000000000 ) ) ;
#38687 = CARTESIAN_POINT ( 'NONE',  ( 8.733858618705999888, -78.52991636018700206, -7.038306768505999678 ) ) ;
#38688 = CARTESIAN_POINT ( 'NONE',  ( 2.098039488145003517, -79.95716955824430272, 9.032790411606809400 ) ) ;
#38689 = ORIENTED_EDGE ( 'NONE', *, *, #42061, .F. ) ;
#38690 = LINE ( 'NONE', #28959, #50122 ) ;
#38691 = ORIENTED_EDGE ( 'NONE', *, *, #41284, .F. ) ;
#38692 = EDGE_CURVE ( 'NONE', #21820, #10829, #53113, .T. ) ;
#38693 = CARTESIAN_POINT ( 'NONE',  ( 3.122028716178808061, -77.25255616389402746, -8.707463557169358381 ) ) ;
#38694 = CARTESIAN_POINT ( 'NONE',  ( -1.402375016663000018, -80.28557803647899505, 0.2083355298385999865 ) ) ;
#38695 = CARTESIAN_POINT ( 'NONE',  ( 11.79999999999999893, -23.15000000000999947, 0.5999999999999999778 ) ) ;
#38696 = CARTESIAN_POINT ( 'NONE',  ( -5.859527123903457202, -77.76864700048736267, 9.564912485122741614 ) ) ;
#38697 = CARTESIAN_POINT ( 'NONE',  ( -0.6817061190079000133, -78.45942315521890009, 1.354333385606999896 ) ) ;
#38698 = CARTESIAN_POINT ( 'NONE',  ( 0.000000000000000000, -74.64999999999999147, 0.000000000000000000 ) ) ;
#38699 = DIRECTION ( 'NONE',  ( 0.000000000000000000, 0.000000000000000000, 1.000000000000000000 ) ) ;
#38700 = CARTESIAN_POINT ( 'NONE',  ( 1.169626569868999821, -78.14079513876998817, 1.131652196797999999 ) ) ;
#38701 = CARTESIAN_POINT ( 'NONE',  ( 0.000000000000000000, -0.5000000000000000000, 0.000000000000000000 ) ) ;
#38702 = CARTESIAN_POINT ( 'NONE',  ( 7.267180141948999861, -79.31094136420898622, 8.322618964701998578 ) ) ;
#38703 = CARTESIAN_POINT ( 'NONE',  ( -9.000000000000000000, -92.39999999999999147, 0.000000000000000000 ) ) ;
#38704 = DIRECTION ( 'NONE',  ( -1.000000000000000000, 0.000000000000000000, 0.000000000000000000 ) ) ;
#38705 = CARTESIAN_POINT ( 'NONE',  ( 12.00000000000000000, -23.25000000000000000, -1.750000000000000000 ) ) ;
#38706 = EDGE_CURVE ( 'NONE', #50254, #900, #52121, .T. ) ;
#38707 = CARTESIAN_POINT ( 'NONE',  ( -12.50409240828718360, -61.32129362315841092, -1.233800930083493563 ) ) ;
#38708 = ORIENTED_EDGE ( 'NONE', *, *, #26796, .T. ) ;
#38709 = CARTESIAN_POINT ( 'NONE',  ( -9.309572583879614172, -77.20000000000000284, 5.728019906940674311 ) ) ;
#38710 = CARTESIAN_POINT ( 'NONE',  ( -1.436931233250000162, -79.97318471100000181, -0.3027821832741999786 ) ) ;
#38711 = LINE ( 'NONE', #11861, #34191 ) ;
#38712 = EDGE_CURVE ( 'NONE', #22044, #34387, #26619, .T. ) ;
#38713 = CARTESIAN_POINT ( 'NONE',  ( 11.70594025892000012, -78.26536582366799166, 2.546964289010999583 ) ) ;
#38714 = DIRECTION ( 'NONE',  ( 0.7071067810866970005, 6.386292029988980325E-09, -0.7071067812863980340 ) ) ;
#38715 = CARTESIAN_POINT ( 'NONE',  ( 1.611423453808999984, -81.48158470040999646, 0.4225784326546000447 ) ) ;
#38716 = CARTESIAN_POINT ( 'NONE',  ( -0.9429918526208548313, -1.853499113097019979, -3.393197731231969438 ) ) ;
#38717 = CARTESIAN_POINT ( 'NONE',  ( 9.377128579935000374, -78.35875194988499004, -2.571625947824999869 ) ) ;
#38718 = CARTESIAN_POINT ( 'NONE',  ( -10.75000000000000000, -76.59999999999999432, 0.000000000000000000 ) ) ;
#38719 = CARTESIAN_POINT ( 'NONE',  ( 4.161322419204999790, -77.18271174891199848, -10.09251018087000062 ) ) ;
#38720 = CARTESIAN_POINT ( 'NONE',  ( 6.606377239730347739, -79.17708333333331439, -8.596418555780422466 ) ) ;
#38721 = CARTESIAN_POINT ( 'NONE',  ( -1.199999999999999956, -80.99999999999998579, -7.000000000000000000 ) ) ;
#38722 = CARTESIAN_POINT ( 'NONE',  ( 0.6025325372421354020, -80.81439488872916854, -1.122865852738351489 ) ) ;
#38723 = ORIENTED_EDGE ( 'NONE', *, *, #38239, .F. ) ;
#38724 = CARTESIAN_POINT ( 'NONE',  ( 9.500000000000000000, -77.14999999999999147, 0.000000000000000000 ) ) ;
#38725 = CARTESIAN_POINT ( 'NONE',  ( 0.5154756746309999693, -61.93240599730000184, -12.66205448077000106 ) ) ;
#38726 = DIRECTION ( 'NONE',  ( 0.7071067811865474617, 0.000000000000000000, -0.7071067811865474617 ) ) ;
#38727 = AXIS2_PLACEMENT_3D ( 'NONE', #51897, #19724, #47192 ) ;
#38728 = CARTESIAN_POINT ( 'NONE',  ( -2.185791986076000004, -77.94328743399398718, -11.00183730042999919 ) ) ;
#38729 = CARTESIAN_POINT ( 'NONE',  ( 6.612939829087000732, -79.69339014975298596, 8.759739992124000452 ) ) ;
#38730 = CARTESIAN_POINT ( 'NONE',  ( 10.18949719146000099, -23.21529250218000229, -7.645392405660000001 ) ) ;
#38731 = CARTESIAN_POINT ( 'NONE',  ( -3.766856363023864951, -84.78958333885674392, -1.489932256642206410 ) ) ;
#38732 = CARTESIAN_POINT ( 'NONE',  ( 3.154088538942999786, -76.43069783301999109, 11.73615235293999959 ) ) ;
#38733 = DIRECTION ( 'NONE',  ( -1.000000000000000000, 0.000000000000000000, 0.000000000000000000 ) ) ;
#38734 = CARTESIAN_POINT ( 'NONE',  ( -9.697372265369081035, -61.77233735005969351, 8.266620275728032041 ) ) ;
#38735 = ORIENTED_EDGE ( 'NONE', *, *, #9374, .T. ) ;
#38736 = AXIS2_PLACEMENT_3D ( 'NONE', #32029, #50070, #5977 ) ;
#38737 = CARTESIAN_POINT ( 'NONE',  ( -1.250000000000000000, -77.75000000000000000, 0.000000000000000000 ) ) ;
#38738 = ADVANCED_FACE ( 'NONE', ( #25017 ), #41697, .T. ) ;
#38739 = CARTESIAN_POINT ( 'NONE',  ( 10.99999999999999822, -77.96041666666667425, 1.439896632895345086 ) ) ;
#38740 = CARTESIAN_POINT ( 'NONE',  ( -5.850594862776000049, -78.16198602556298169, 9.500638896661000032 ) ) ;
#38741 = DIRECTION ( 'NONE',  ( -0.7071067812863980340, 6.386274622742979319E-09, -0.7071067810866970005 ) ) ;
#38742 = FACE_OUTER_BOUND ( 'NONE', #1451, .T. ) ;
#38743 = CARTESIAN_POINT ( 'NONE',  ( -9.309367086190000862, -77.13855160546319212, -0.1968645694141999969 ) ) ;
#38744 = CARTESIAN_POINT ( 'NONE',  ( -0.2342375876246420574, -82.23597684144930042, 1.531779633465825130 ) ) ;
#38745 = CARTESIAN_POINT ( 'NONE',  ( 0.3485046458849904161, -79.74754369683780908, -1.203412226622470049 ) ) ;
#38746 = EDGE_CURVE ( 'NONE', #11813, #33386, #37944, .T. ) ;
#38747 = ORIENTED_EDGE ( 'NONE', *, *, #46148, .T. ) ;
#38748 = ADVANCED_FACE ( 'NONE', ( #38596 ), #14991, .T. ) ;
#38749 = CARTESIAN_POINT ( 'NONE',  ( 2.062673488738000049, -18.67547470641000018, 12.82904091339000097 ) ) ;
#38750 =( LENGTH_UNIT ( ) NAMED_UNIT ( * ) SI_UNIT ( .MILLI., .METRE. ) );
#38751 = CARTESIAN_POINT ( 'NONE',  ( 5.917523019358037040, -76.13333333333329733, 10.26699006316254525 ) ) ;
#38752 = VERTEX_POINT ( 'NONE', #51325 ) ;
#38753 = VERTEX_POINT ( 'NONE', #24148 ) ;
#38754 = CONICAL_SURFACE ( 'NONE', #53849, 0.6999999997694995590, 0.7853981633972997312 ) ;
#38755 = CARTESIAN_POINT ( 'NONE',  ( -12.49830607526000037, -55.59028586401999661, -1.666977523254999927 ) ) ;
#38756 = ORIENTED_EDGE ( 'NONE', *, *, #38408, .F. ) ;
#38757 = ORIENTED_EDGE ( 'NONE', *, *, #9374, .F. ) ;
#38758 = CARTESIAN_POINT ( 'NONE',  ( 10.36221643468999964, -23.22123873666000193, 7.631895748949999891 ) ) ;
#38759 = CARTESIAN_POINT ( 'NONE',  ( -9.731251526955000841, -77.11083935769899256, -4.947535720883000643 ) ) ;
#38760 = CONTEXT_DEPENDENT_SHAPE_REPRESENTATION ( #2110, #54563 ) ;
#38761 = DIRECTION ( 'NONE',  ( 0.000000000000000000, 1.000000000000000000, 0.000000000000000000 ) ) ;
#38762 = CARTESIAN_POINT ( 'NONE',  ( -0.8644569908188000085, -79.13883667140099476, 9.872851397518997985 ) ) ;
#38763 = CARTESIAN_POINT ( 'NONE',  ( 3.632329907060999563, -80.04667739574479413, 10.45854222826000068 ) ) ;
#38764 = ORIENTED_EDGE ( 'NONE', *, *, #7840, .F. ) ;
#38765 = ORIENTED_EDGE ( 'NONE', *, *, #44288, .F. ) ;
#38766 = CARTESIAN_POINT ( 'NONE',  ( -5.620083643312043797, -77.52702428364116827, 7.346969722847941142 ) ) ;
#38767 = CIRCLE ( 'NONE', #37840, 1.750000000000000000 ) ;
#38768 = CARTESIAN_POINT ( 'NONE',  ( 10.90987126150000108, -77.07178011482669433, 1.690571823134000118 ) ) ;
#38769 = CARTESIAN_POINT ( 'NONE',  ( -12.25000000000000000, -80.79999999999999716, 0.000000000000000000 ) ) ;
#38770 = AXIS2_PLACEMENT_3D ( 'NONE', #37061, #10804, #51253 ) ;
#38771 = CARTESIAN_POINT ( 'NONE',  ( 7.890274420948999001, -79.03070443413199087, -5.649267206312000411 ) ) ;
#38772 = CARTESIAN_POINT ( 'NONE',  ( 3.654181830569951384, -86.12610001270965654, -1.626946572303266114 ) ) ;
#38773 = CARTESIAN_POINT ( 'NONE',  ( 8.611000705980396575, -61.97488119190063571, 9.355851007348242376 ) ) ;
#38774 = CARTESIAN_POINT ( 'NONE',  ( 1.750000000001000089, -18.75000001325000198, 12.56594318051000059 ) ) ;
#38775 = CARTESIAN_POINT ( 'NONE',  ( -8.744140569415000286, -80.31565346514499026, 7.086030162020000134 ) ) ;
#38776 = DIRECTION ( 'NONE',  ( 0.000000000000000000, -1.000000000000000000, 0.000000000000000000 ) ) ;
#38777 = CARTESIAN_POINT ( 'NONE',  ( 2.500000000000000000, -77.69999999999998863, 0.000000000000000000 ) ) ;
#38778 = CARTESIAN_POINT ( 'NONE',  ( -0.5880095755872802865, -79.65680747369806625, 1.391623923462375068 ) ) ;
#38780 = EDGE_CURVE ( 'NONE', #42403, #47034, #28855, .T. ) ;
#38779 = CARTESIAN_POINT ( 'NONE',  ( -0.6596342590195000133, -77.82341332859900263, 9.888746480308999054 ) ) ;
#38781 = CARTESIAN_POINT ( 'NONE',  ( -0.7928179559538000021, -78.82141258400598360, -11.95355612866999984 ) ) ;
#38782 = FACE_OUTER_BOUND ( 'NONE', #46407, .T. ) ;
#38784 = CARTESIAN_POINT ( 'NONE',  ( 1.477284502223000118, -17.27368499703000282, -12.77254812468999923 ) ) ;
#38783 = CARTESIAN_POINT ( 'NONE',  ( 7.655542440085000067, -59.57819125629999490, 10.38645071868999992 ) ) ;
#38785 = CARTESIAN_POINT ( 'NONE',  ( 9.250225651199979637, -79.36043693044713621, 1.210484955505027882 ) ) ;
#38786 = CARTESIAN_POINT ( 'NONE',  ( 8.479715450285999268, -80.18656123089598964, -7.288724056671999740 ) ) ;
#38787 = CARTESIAN_POINT ( 'NONE',  ( 12.85140862673999784, -21.75560170163999985, 1.980464483675000054 ) ) ;
#38788 = CARTESIAN_POINT ( 'NONE',  ( 7.183928826236000376, -78.50476576377499782, -8.388570749380001246 ) ) ;
#38789 = CARTESIAN_POINT ( 'NONE',  ( 3.313572498374643072, -3.500000000000000888, 1.146852011088394852 ) ) ;
#38790 = DIRECTION ( 'NONE',  ( 0.9999999999999693578, 2.479738742161926003E-07, 1.114546890279966179E-12 ) ) ;
#38791 = VERTEX_POINT ( 'NONE', #20308 ) ;
#38792 = CARTESIAN_POINT ( 'NONE',  ( 0.000000000000000000, -80.79999999999999716, 0.000000000000000000 ) ) ;
#38793 = DIRECTION ( 'NONE',  ( -1.000000000000000000, 0.000000000000000000, 0.000000000000000000 ) ) ;
#38794 = CARTESIAN_POINT ( 'NONE',  ( 1.116474234542908839, -78.38743099930486835, 0.5628238750089364917 ) ) ;
#38795 = CARTESIAN_POINT ( 'NONE',  ( -3.625242457524000095, -3.139913721651000245, -0.3865940047836999849 ) ) ;
#38796 = B_SPLINE_CURVE_WITH_KNOTS ( 'NONE', 3,
 ( #25577, #25866, #43024, #56886 ),
 .UNSPECIFIED., .F., .F.,
 ( 4, 4 ),
 ( 0.000000000000000000, 1.000000000000000000 ),
 .UNSPECIFIED. ) ;
#38797 = CARTESIAN_POINT ( 'NONE',  ( 7.830816902459000417, -79.59348277179398679, -5.626419586328999856 ) ) ;
#38798 = CARTESIAN_POINT ( 'NONE',  ( -12.70956139856000000, -55.39498835716000258, 1.933780970937999832 ) ) ;
#38799 = FACE_OUTER_BOUND ( 'NONE', #45722, .T. ) ;
#38800 = CARTESIAN_POINT ( 'NONE',  ( 1.310679582531387943, -80.20833333333332860, -0.7554284705563468760 ) ) ;
#38801 = CARTESIAN_POINT ( 'NONE',  ( -3.165411199172024848, -3.020833333333332593, -0.8506806241676611036 ) ) ;
#38802 = EDGE_CURVE ( 'NONE', #29877, #52834, #30458, .T. ) ;
#38803 = CARTESIAN_POINT ( 'NONE',  ( 8.796335266379992746, -77.39791666666667425, -6.760013919724047859 ) ) ;
#38804 = CARTESIAN_POINT ( 'NONE',  ( 0.000000000000000000, -18.84999999999999787, 12.00000000000000000 ) ) ;
#38805 = EDGE_CURVE ( 'NONE', #52835, #49740, #53682, .T. ) ;
#38806 = CARTESIAN_POINT ( 'NONE',  ( -0.008233557564672998319, -77.68199712970098858, 11.05658471417999955 ) ) ;
#38807 = B_SPLINE_CURVE_WITH_KNOTS ( 'NONE', 3,
 ( #14837, #36694, #50006, #9552, #10424, #23121, #45872, #5406, #1007, #18992 ),
 .UNSPECIFIED., .F., .F.,
 ( 4, 2, 2, 2, 4 ),
 ( 0.2500000082780876598, 0.4375000062085657726, 0.6250000041390437744, 0.8125000020695218872, 1.000000000000000000 ),
 .UNSPECIFIED. ) ;
#38808 = CARTESIAN_POINT ( 'NONE',  ( 8.288812145454857117, -76.38727426244473406, -8.328108146873651307 ) ) ;
#38809 = CARTESIAN_POINT ( 'NONE',  ( -9.398554024959999253, -78.25403817759199399, -5.993477931829000127 ) ) ;
#38810 = CARTESIAN_POINT ( 'NONE',  ( -1.250000000000000000, -82.09999999999999432, 0.000000000000000000 ) ) ;
#38811 = CARTESIAN_POINT ( 'NONE',  ( -0.7159780689917000229, -78.41961979257999360, -1.501637300520000107 ) ) ;
#38812 = CARTESIAN_POINT ( 'NONE',  ( -6.294203684166999935, -77.26153958204697858, 7.343715272572999275 ) ) ;
#38813 = CARTESIAN_POINT ( 'NONE',  ( -0.1963495408493673433, -78.88541666666668561, 1.499999999999999334 ) ) ;
#38814 = CARTESIAN_POINT ( 'NONE',  ( -11.00000000000000000, -77.59999999999999432, 0.000000000000000000 ) ) ;
#38815 = CARTESIAN_POINT ( 'NONE',  ( 10.12305140789450775, -80.32185189037265616, -3.763052347616244742 ) ) ;
#38816 = CARTESIAN_POINT ( 'NONE',  ( 9.238233337088816555, -79.89317385683257555, 5.558906132332217531 ) ) ;
#38817 = CARTESIAN_POINT ( 'NONE',  ( 9.723174505952000501, -24.47697504198000118, 7.958760297001999717 ) ) ;
#38818 = EDGE_CURVE ( 'NONE', #10750, #46629, #912, .T. ) ;
#38819 = CARTESIAN_POINT ( 'NONE',  ( -11.60111135005000094, -79.08740487884900006, -3.181408645392000523 ) ) ;
#38820 = CARTESIAN_POINT ( 'NONE',  ( -1.216845017716923438, -78.12095369619891017, -0.3271854394012499445 ) ) ;
#38821 = CARTESIAN_POINT ( 'NONE',  ( 11.18604332926000033, -79.06415834696599632, -1.306292155029999957 ) ) ;
#38822 = ORIENTED_EDGE ( 'NONE', *, *, #30439, .T. ) ;
#38823 = CARTESIAN_POINT ( 'NONE',  ( -1.501534314726683306, -24.55152951662029892, 12.70455943739977656 ) ) ;
#38824 = B_SPLINE_CURVE_WITH_KNOTS ( 'NONE', 3,
 ( #27268, #45304, #22258, #31984, #741, #35534, #36716, #40273, #8391, #53562, #13101, #58284, #17847, #24013, #28135, #42327, #1896, #50316 ),
 .UNSPECIFIED., .F., .F.,
 ( 4, 2, 2, 2, 2, 2, 2, 2, 4 ),
 ( 0.000000000000000000, 0.1250000000000000833, 0.2500000000000001110, 0.3750000000000000000, 0.4999999999999999445, 0.6249999999999998890, 0.7499999999999997780, 0.8749999999999998890, 1.000000000000000000 ),
 .UNSPECIFIED. ) ;
#38825 = ORIENTED_EDGE ( 'NONE', *, *, #10734, .F. ) ;
#38826 = ORIENTED_EDGE ( 'NONE', *, *, #51838, .F. ) ;
#38827 = CARTESIAN_POINT ( 'NONE',  ( 1.081559480311999888, -3.500000000000000000, -3.328697807033000000 ) ) ;
#38828 = ORIENTED_EDGE ( 'NONE', *, *, #1178, .T. ) ;
#38829 = CARTESIAN_POINT ( 'NONE',  ( 2.358097774615999676, -81.20774294257799397, 2.646572533277999906 ) ) ;
#38830 = CARTESIAN_POINT ( 'NONE',  ( 3.266878030750679951, -79.24670026210782225, 8.921992862818912684 ) ) ;
#38831 = EDGE_CURVE ( 'NONE', #40540, #49656, #34170, .T. ) ;
#38832 = ORIENTED_EDGE ( 'NONE', *, *, #21070, .T. ) ;
#38833 = CARTESIAN_POINT ( 'NONE',  ( 0.000000000000000000, -79.65000000003199432, 0.000000000000000000 ) ) ;
#38834 = ORIENTED_EDGE ( 'NONE', *, *, #21089, .F. ) ;
#38835 = DIRECTION ( 'NONE',  ( -1.000000000000000000, 0.000000000000000000, 0.000000000000000000 ) ) ;
#38836 = ORIENTED_EDGE ( 'NONE', *, *, #8592, .F. ) ;
#38837 = CARTESIAN_POINT ( 'NONE',  ( 1.127238840805811826, -79.38609853011139705, 0.5400240268550191569 ) ) ;
#38838 = CARTESIAN_POINT ( 'NONE',  ( 0.1063340454544151326, -78.11970978693250345, 1.529732311428813274 ) ) ;
#38839 = DIRECTION ( 'NONE',  ( 0.000000000000000000, -1.000000000000000000, 0.000000000000000000 ) ) ;
#38840 = CARTESIAN_POINT ( 'NONE',  ( -4.848317728770459745, -80.01234159837389370, 9.594520772546756504 ) ) ;
#38841 = CARTESIAN_POINT ( 'NONE',  ( 3.106054555985034771, -86.09999999999998010, -1.382904586457756047 ) ) ;
#38842 = CARTESIAN_POINT ( 'NONE',  ( 10.02574878253000001, -76.62042584315300076, 4.955627619753999902 ) ) ;
#38843 = FACE_OUTER_BOUND ( 'NONE', #44635, .T. ) ;
#38844 = CARTESIAN_POINT ( 'NONE',  ( -6.294306073545501867, -77.28129539589265562, 7.343834734617976423 ) ) ;
#38845 = CARTESIAN_POINT ( 'NONE',  ( 10.95125797090999953, -76.62750415032999740, -1.894616286183999909 ) ) ;
#38846 = DIRECTION ( 'NONE',  ( 0.000000000000000000, 1.000000000000000000, 0.000000000000000000 ) ) ;
#38847 = CARTESIAN_POINT ( 'NONE',  ( 1.170174673132000187, -79.96792637803000048, 0.6397400908730001001 ) ) ;
#38848 = VECTOR ( 'NONE', #48236, 1000.000000000000000 ) ;
#38849 = DIRECTION ( 'NONE',  ( 0.7071067811814418791, 1.254535583516073644E-07, 0.7071067811916420531 ) ) ;
#38850 = CARTESIAN_POINT ( 'NONE',  ( 2.231512935965016986, -2.915198822935428868, 2.362588882341296603 ) ) ;
#38851 = CARTESIAN_POINT ( 'NONE',  ( 0.5020202678138999675, -78.80228455456848735, -3.722814961589000493 ) ) ;
#38852 = CARTESIAN_POINT ( 'NONE',  ( -5.072986942693556323, -78.01416854347621666, 9.477675060726154399 ) ) ;
#38853 = CARTESIAN_POINT ( 'NONE',  ( 1.001315002179000047, -24.68522411714000242, -12.50000000000000000 ) ) ;
#38854 = CARTESIAN_POINT ( 'NONE',  ( -12.51072239526000196, -63.10294702885996543, -0.7871079366006996647 ) ) ;
#38855 = CARTESIAN_POINT ( 'NONE',  ( 3.124270252784000057, -85.31969503318799752, -1.679433785107000032 ) ) ;
#38856 = CARTESIAN_POINT ( 'NONE',  ( 1.250000000000000000, -80.25000000000000000, 0.000000000000000000 ) ) ;
#38857 = CARTESIAN_POINT ( 'NONE',  ( -0.5435958524137841641, -79.34034035607614044, -1.153047142414559856 ) ) ;
#38858 = CARTESIAN_POINT ( 'NONE',  ( -8.252521514740998043, -61.73405767862000459, -9.650901483168000894 ) ) ;
#38859 = CARTESIAN_POINT ( 'NONE',  ( -1.243547092045993674, -78.28541666666666288, 9.499999999999996447 ) ) ;
#38860 = DIRECTION ( 'NONE',  ( 0.000000000000000000, 1.000000000000000000, 0.000000000000000000 ) ) ;
#38861 = CARTESIAN_POINT ( 'NONE',  ( 1.310679582531388387, -80.60833333333333428, -0.7554284705563470981 ) ) ;
#38862 = CARTESIAN_POINT ( 'NONE',  ( -10.64207148833999916, -76.96853494252998473, 7.489034475093999887 ) ) ;
#38864 = CARTESIAN_POINT ( 'NONE',  ( -3.106054822367000146, -86.10000002299598520, 1.382903988153999952 ) ) ;
#38863 = CONICAL_SURFACE ( 'NONE', #13406, 4.899999999795999983, 0.7853981633972997312 ) ;
#38865 = EDGE_CURVE ( 'NONE', #44663, #21904, #25305, .T. ) ;
#38866 = CARTESIAN_POINT ( 'NONE',  ( 0.1380878923104814915, -25.22734402325045977, -12.70555840932425085 ) ) ;
#38867 = CARTESIAN_POINT ( 'NONE',  ( 1.430780206329000048, -75.86025915096999483, 12.43029443217000107 ) ) ;
#38868 = B_SPLINE_CURVE_WITH_KNOTS ( 'NONE', 3,
 ( #40104, #30363, #4092, #16525, #53392, #52820 ),
 .UNSPECIFIED., .F., .F.,
 ( 4, 1, 1, 4 ),
 ( 0.000000000000000000, 0.3333333333333000081, 0.6666666666667000474, 1.000000000000000000 ),
 .UNSPECIFIED. ) ;
#38869 = VERTEX_POINT ( 'NONE', #54220 ) ;
#38870 = CARTESIAN_POINT ( 'NONE',  ( -10.58783149161999759, -80.77773939978943929, -3.847989116766000084 ) ) ;
#38871 = CARTESIAN_POINT ( 'NONE',  ( -5.845697796373999999, -80.35876778545760146, -9.793643869219998521 ) ) ;
#38872 = CARTESIAN_POINT ( 'NONE',  ( 12.54673765600000124, -61.62199238204999574, 0.9174244429637000708 ) ) ;
#38873 = CARTESIAN_POINT ( 'NONE',  ( 12.74575047010000084, -78.83831324550000375, 1.100459882033999914 ) ) ;
#38874 = CARTESIAN_POINT ( 'NONE',  ( -2.062670899361999766, -18.69360215052999763, -12.83044027761000017 ) ) ;
#38875 = CARTESIAN_POINT ( 'NONE',  ( -6.715271092063999525, -77.95666193574498948, -6.903502308617000871 ) ) ;
#38876 = CARTESIAN_POINT ( 'NONE',  ( 1.268661270421000076, -83.66130927919799376, -3.974993213500999545 ) ) ;
#38877 = CARTESIAN_POINT ( 'NONE',  ( -1.587769864458760338, -79.98724231797385187, 10.63181754089058373 ) ) ;
#38878 = CARTESIAN_POINT ( 'NONE',  ( -0.5899402231854000700, -79.08717912789200000, -1.503093382721999882 ) ) ;
#38879 = ORIENTED_EDGE ( 'NONE', *, *, #32753, .T. ) ;
#38880 = CARTESIAN_POINT ( 'NONE',  ( 9.448596496680870871, -77.31041241042555612, -5.152684619491262552 ) ) ;
#38881 = CARTESIAN_POINT ( 'NONE',  ( -5.539808784079903070, -78.78333333333334565, -9.611650271896833075 ) ) ;
#38882 = CARTESIAN_POINT ( 'NONE',  ( 0.5664082909794043719, -78.90708710382101287, -3.437496070717471763 ) ) ;
#38883 = VERTEX_POINT ( 'NONE', #40338 ) ;
#38884 = ADVANCED_FACE ( 'NONE', ( #802 ), #13163, .F. ) ;
#38885 = CARTESIAN_POINT ( 'NONE',  ( 3.902863791433999641, -79.21678520010797797, 10.22034591202999820 ) ) ;
#38886 = CARTESIAN_POINT ( 'NONE',  ( 12.71658889739000031, -55.48415522678000400, 1.931087888049999979 ) ) ;
#38887 = CARTESIAN_POINT ( 'NONE',  ( 3.929414825497000496, -80.02429038178499354, -10.50786154751999923 ) ) ;
#38888 = ORIENTED_EDGE ( 'NONE', *, *, #52146, .F. ) ;
#38889 = ORIENTED_EDGE ( 'NONE', *, *, #9007, .T. ) ;
#38890 = ORIENTED_EDGE ( 'NONE', *, *, #58377, .T. ) ;
#38891 = EDGE_CURVE ( 'NONE', #15713, #17863, #29724, .T. ) ;
#38892 = CARTESIAN_POINT ( 'NONE',  ( -0.002548132935883858086, -80.47577112694141022, 1.249635788585080176 ) ) ;
#38893 = AXIS2_PLACEMENT_3D ( 'NONE', #38652, #21511, #12930 ) ;
#38894 = CARTESIAN_POINT ( 'NONE',  ( -3.106054822367000146, -86.10000002299598520, 1.382903988153999952 ) ) ;
#38895 = CARTESIAN_POINT ( 'NONE',  ( -4.465297566879000257, -80.04294400888201722, 8.686876450551999085 ) ) ;
#38896 = EDGE_CURVE ( 'NONE', #9459, #41516, #14337, .T. ) ;
#38897 = ORIENTED_EDGE ( 'NONE', *, *, #37648, .T. ) ;
#38898 = CARTESIAN_POINT ( 'NONE',  ( 1.638719174300647730, -2.434540441116925358, 2.841788563852642557 ) ) ;
#38899 = VERTEX_POINT ( 'NONE', #40930 ) ;
#38900 = DIRECTION ( 'NONE',  ( 1.000000000000000000, 0.000000000000000000, 0.000000000000000000 ) ) ;
#38901 = CARTESIAN_POINT ( 'NONE',  ( 3.699999999669999262, -79.00321104920828930, -2.183641561086286487 ) ) ;
#38902 = CONICAL_SURFACE ( 'NONE', #5913, 9.649999999948999374, 0.7853981633972997312 ) ;
#38903 = CARTESIAN_POINT ( 'NONE',  ( 9.641218323587999350, -54.36606991882000273, 7.943737929401001985 ) ) ;
#38904 = CARTESIAN_POINT ( 'NONE',  ( 7.864797288620628990, -17.54877151179043793, -10.10445166986456123 ) ) ;
#38905 = CARTESIAN_POINT ( 'NONE',  ( -7.612971414713999962, -23.32452529362999982, -10.53003223722999948 ) ) ;
#38906 = CARTESIAN_POINT ( 'NONE',  ( 8.220803302871821927, -78.84397913613844366, 5.195369692238999804 ) ) ;
#38907 = CARTESIAN_POINT ( 'NONE',  ( 12.74331206683557660, -60.32649290773598239, -1.980611467281674365 ) ) ;
#38908 = CARTESIAN_POINT ( 'NONE',  ( 10.99419336675999936, -78.93250602332912536, 4.758540471090999979 ) ) ;
#38909 = CARTESIAN_POINT ( 'NONE',  ( 2.499201589291803138, -81.16666667311758943, 3.189714631542692747 ) ) ;
#38910 = CARTESIAN_POINT ( 'NONE',  ( -7.605690822180000588, -23.42565082156999878, 10.52682217035000001 ) ) ;
#38911 = ADVANCED_FACE ( 'NONE', ( #517 ), #41505, .F. ) ;
#38912 = CARTESIAN_POINT ( 'NONE',  ( 3.494263450112999880, -79.60682046129089429, 2.279620140072000201 ) ) ;
#38913 = CARTESIAN_POINT ( 'NONE',  ( -1.250000000000000000, -83.49999999999998579, 0.000000000000000000 ) ) ;
#38914 = CARTESIAN_POINT ( 'NONE',  ( 8.541150802335000236, -61.80800189248000009, -9.205830468624000673 ) ) ;
#38915 = CARTESIAN_POINT ( 'NONE',  ( -10.39285214024000048, -78.40346505345000594, 6.510605926401999533 ) ) ;
#38916 = CARTESIAN_POINT ( 'NONE',  ( 9.406806676749999596, -76.69275178953499505, -7.895227358184000899 ) ) ;
#38917 = CARTESIAN_POINT ( 'NONE',  ( -7.364280830344099193, -60.14010097497214247, -8.171144579306195865 ) ) ;
#38918 = CARTESIAN_POINT ( 'NONE',  ( -5.869402599192000025, -78.46567021303999923, 10.46661899222999992 ) ) ;
#38919 = DIRECTION ( 'NONE',  ( 0.000000000000000000, 0.000000000000000000, -1.000000000000000000 ) ) ;
#38920 = CARTESIAN_POINT ( 'NONE',  ( 0.8406634254895485325, -80.92201610971640946, -1.255420779031111822 ) ) ;
#38921 = CARTESIAN_POINT ( 'NONE',  ( -9.252372813388998196, -77.46665409050798701, -1.135340161459000186 ) ) ;
#38922 = FACE_OUTER_BOUND ( 'NONE', #19888, .T. ) ;
#38923 = AXIS2_PLACEMENT_3D ( 'NONE', #5597, #23609, #10049 ) ;
#38924 = PLANE ( 'NONE',  #45510 ) ;
#38925 = CARTESIAN_POINT ( 'NONE',  ( -1.703108177512000054, -3.472353339067000277, 2.944283159703000141 ) ) ;
#38926 = CARTESIAN_POINT ( 'NONE',  ( -11.99726733138999890, -77.51629135392300896, -1.123097615067000010 ) ) ;
#38927 = CARTESIAN_POINT ( 'NONE',  ( 0.8649477812003000254, -78.40288999989098784, -9.701111330267998767 ) ) ;
#38929 = CARTESIAN_POINT ( 'NONE',  ( -1.169594621339999918, -78.70366409087199600, 0.6104211924069999906 ) ) ;
#38928 = CARTESIAN_POINT ( 'NONE',  ( -6.577478410916997476, -75.79999999999999716, 9.905072954783767258 ) ) ;
#38930 = CARTESIAN_POINT ( 'NONE',  ( 0.5557217581696000108, -82.48745749870199973, 1.359272403504999893 ) ) ;
#38931 = CARTESIAN_POINT ( 'NONE',  ( -7.651147547633000201, -19.23743349724999874, 10.45204383579999963 ) ) ;
#38932 = ORIENTED_EDGE ( 'NONE', *, *, #16967, .T. ) ;
#38933 = CARTESIAN_POINT ( 'NONE',  ( -11.29698467241381188, -78.87175061103830842, 4.184771565250527736 ) ) ;
#38934 = VECTOR ( 'NONE', #23508, 1000.000000000000000 ) ;
#38935 = CARTESIAN_POINT ( 'NONE',  ( -1.790564795957000133, -79.80425913277389327, -11.90740541383000028 ) ) ;
#38936 = CARTESIAN_POINT ( 'NONE',  ( 4.657751049633202634, -79.41546676809356597, -8.372025729518147941 ) ) ;
#38937 = CARTESIAN_POINT ( 'NONE',  ( -5.350956159761850017, -79.99999999999998579, -7.703458012427442547 ) ) ;
#38938 = CARTESIAN_POINT ( 'NONE',  ( -7.633089125635001082, -60.19007426270999872, 10.18115018433999985 ) ) ;
#38939 = CARTESIAN_POINT ( 'NONE',  ( -2.973381617294999835, -0.5899651668208000244, -1.916927929355999982 ) ) ;
#38940 = CARTESIAN_POINT ( 'NONE',  ( -0.09809059825999000282, -79.83113977864098842, -9.780255580327999354 ) ) ;
#38941 = CARTESIAN_POINT ( 'NONE',  ( 7.646944981223999349, -18.80364172516999943, -10.19022195330999914 ) ) ;
#38942 = CARTESIAN_POINT ( 'NONE',  ( 5.539808784079905735, -78.76666666666666572, -9.611650271896829523 ) ) ;
#38943 = B_SPLINE_CURVE_WITH_KNOTS ( 'NONE', 3,
 ( #18983, #46156, #5974, #10414, #5681, #10715, #37852, #23978, #1565, #11006 ),
 .UNSPECIFIED., .F., .F.,
 ( 4, 2, 2, 2, 4 ),
 ( 0.4999998626202952212, 0.6249998969652212910, 0.7499999313101475273, 0.8749999656550737637, 1.000000000000000000 ),
 .UNSPECIFIED. ) ;
#38944 = ORIENTED_EDGE ( 'NONE', *, *, #32191, .T. ) ;
#38945 = VECTOR ( 'NONE', #12863, 1000.000000000000227 ) ;
#38946 = DIRECTION ( 'NONE',  ( 0.7071067811865474617, 0.000000000000000000, -0.7071067811865474617 ) ) ;
#38947 = CARTESIAN_POINT ( 'NONE',  ( -8.199429518657952443, -78.98546353816666965, 8.534060759012747965 ) ) ;
#38948 = CARTESIAN_POINT ( 'NONE',  ( -3.046227980494999876, -79.91992668086899698, -9.106622846827001183 ) ) ;
#38949 = VECTOR ( 'NONE', #38588, 1000.000000000000114 ) ;
#38950 = EDGE_CURVE ( 'NONE', #19368, #52985, #45664, .T. ) ;
#38951 = CARTESIAN_POINT ( 'NONE',  ( -10.53101990617999917, -55.49360215019999742, -7.613962745591999592 ) ) ;
#38952 = CARTESIAN_POINT ( 'NONE',  ( -0.5298108134926000634, -80.78957986396000024, 1.579417458585999912 ) ) ;
#38953 = ORIENTED_EDGE ( 'NONE', *, *, #57042, .T. ) ;
#38954 = EDGE_CURVE ( 'NONE', #52059, #4183, #31755, .T. ) ;
#38955 = CARTESIAN_POINT ( 'NONE',  ( -0.9818792729183725143, -78.09524149188138153, 0.8115973957462927491 ) ) ;
#38956 = CARTESIAN_POINT ( 'NONE',  ( -7.483407197968000801, -77.00000000000000000, 5.437013583706000297 ) ) ;
#38957 = LINE ( 'NONE', #20383, #34588 ) ;
#38958 = CARTESIAN_POINT ( 'NONE',  ( 9.392816810221818358, -78.39167583925791405, 5.413628547907069155 ) ) ;
#38959 = B_SPLINE_CURVE_WITH_KNOTS ( 'NONE', 3,
 ( #33895, #57212, #11775, #16779, #48092, #28894, #47804, #7334, #24477, #25336, #42782, #20910, #38050, #47523, #20340, #16491, #11494, #16204 ),
 .UNSPECIFIED., .F., .F.,
 ( 4, 2, 2, 2, 2, 2, 2, 2, 4 ),
 ( 0.000000000000000000, 0.1250000000000000555, 0.2500000000000001110, 0.3750000000000001665, 0.5000000000000001110, 0.6250000000000001110, 0.7500000000000002220, 0.8750000000000001110, 1.000000000000000000 ),
 .UNSPECIFIED. ) ;
#38960 = CARTESIAN_POINT ( 'NONE',  ( 6.653382217586999658, -79.52491157019498758, 7.150748904218000135 ) ) ;
#38961 = ORIENTED_EDGE ( 'NONE', *, *, #44074, .F. ) ;
#38962 = EDGE_CURVE ( 'NONE', #26643, #616, #5790, .T. ) ;
#38963 = ORIENTED_EDGE ( 'NONE', *, *, #28974, .T. ) ;
#38964 = CARTESIAN_POINT ( 'NONE',  ( 2.587846633264999863, -77.11722910487598881, 12.19916123416999909 ) ) ;
#38965 = CARTESIAN_POINT ( 'NONE',  ( 3.614530024087561522, -78.75232390936722027, -10.13845990724425938 ) ) ;
#38966 = CARTESIAN_POINT ( 'NONE',  ( -0.4913337550651999952, -78.24025491156999124, -1.333792686520999915 ) ) ;
#38967 = VERTEX_POINT ( 'NONE', #22916 ) ;
#38968 = CARTESIAN_POINT ( 'NONE',  ( 12.56594317823000040, -18.74999998606000062, 1.750000000000000000 ) ) ;
#38969 = DIRECTION ( 'NONE',  ( 0.000000000000000000, -1.000000000000000000, 0.000000000000000000 ) ) ;
#38970 = CARTESIAN_POINT ( 'NONE',  ( -1.308715794756476702, -54.05595500772570716, 12.70256747352372351 ) ) ;
#38971 = CARTESIAN_POINT ( 'NONE',  ( -12.75936573546999853, -77.67478844368000068, -1.003864233875000123 ) ) ;
#38972 = B_SPLINE_CURVE_WITH_KNOTS ( 'NONE', 3,
 ( #22727, #18309, #36301, #39564, #57566, #30689, #26270, #21839 ),
 .UNSPECIFIED., .F., .F.,
 ( 4, 2, 2, 4 ),
 ( 0.000000000000000000, 0.4999999999999945599, 0.7499999999999972244, 1.000000000000000000 ),
 .UNSPECIFIED. ) ;
#38973 = CARTESIAN_POINT ( 'NONE',  ( -8.596678438649716369, -79.65211059969949758, -6.606629847258154165 ) ) ;
#38974 = CARTESIAN_POINT ( 'NONE',  ( -1.750000000000000000, -23.24999999688999708, 12.50000000000000000 ) ) ;
#38975 = CARTESIAN_POINT ( 'NONE',  ( 0.000000000000000000, 4.040000000000000036, 0.000000000000000000 ) ) ;
#38976 = CARTESIAN_POINT ( 'NONE',  ( -10.34326456654000026, -78.80227979020500584, 4.339929572939999147 ) ) ;
#38977 = DIRECTION ( 'NONE',  ( -1.000000000000000000, 0.000000000000000000, 0.000000000000000000 ) ) ;
#38978 = EDGE_LOOP ( 'NONE', ( #53882, #46815, #39041, #35353, #34091, #10687 ) ) ;
#38979 = DIRECTION ( 'NONE',  ( 1.000000000000000000, 0.000000000000000000, 0.000000000000000000 ) ) ;
#38980 = VERTEX_POINT ( 'NONE', #49198 ) ;
#38981 = CARTESIAN_POINT ( 'NONE',  ( 6.788068531828999497, -79.94435522376399206, 8.991721824839000732 ) ) ;
#38982 = CARTESIAN_POINT ( 'NONE',  ( 7.215423847483414477, -77.29618573409882742, -5.793044792516142572 ) ) ;
#38983 = CARTESIAN_POINT ( 'NONE',  ( 1.275615568647000098, -80.58325377676599999, 0.6187600927687999519 ) ) ;
#38984 = FACE_OUTER_BOUND ( 'NONE', #18358, .T. ) ;
#38985 = CARTESIAN_POINT ( 'NONE',  ( -2.309498544611330750, -77.74141065748534629, 10.97669464986000420 ) ) ;
#38986 = CARTESIAN_POINT ( 'NONE',  ( -1.335620631414000004, -77.58869253983340286, 0.2413337786383999983 ) ) ;
#38987 = CONICAL_SURFACE ( 'NONE', #47540, 1.249999999985999866, 0.7853981633972997312 ) ;
#38988 = DIRECTION ( 'NONE',  ( 0.000000000000000000, 1.000000000000000000, 0.000000000000000000 ) ) ;
#38989 = DIRECTION ( 'NONE',  ( 0.000000000000000000, 0.000000000000000000, -1.000000000000000000 ) ) ;
#38990 = LINE ( 'NONE', #57000, #12905 ) ;
#38991 = DIRECTION ( 'NONE',  ( -0.9936845293270585300, -0.1122098755727947705, 0.000000000000000000 ) ) ;
#38992 = CARTESIAN_POINT ( 'NONE',  ( 5.137083998358000336, -77.31100733245999379, -10.56753840748999984 ) ) ;
#38993 = CIRCLE ( 'NONE', #27649, 1.749999999999999778 ) ;
#38994 = CARTESIAN_POINT ( 'NONE',  ( 7.338671297540000360, -79.37481710499199039, 8.404493039061998516 ) ) ;
#38995 = CARTESIAN_POINT ( 'NONE',  ( 10.59551070215999857, -20.24351820077000141, -7.678690995240000206 ) ) ;
#38996 = CARTESIAN_POINT ( 'NONE',  ( 0.000000000000000000, -5.000000000000000000, 0.000000000000000000 ) ) ;
#38997 = CARTESIAN_POINT ( 'NONE',  ( -3.370516864494922604, -1.912300517193705529, -0.5569799872951896047 ) ) ;
#38998 = CARTESIAN_POINT ( 'NONE',  ( -12.52785920748594428, -60.59405666895369791, -1.668536824536160035 ) ) ;
#38999 = EDGE_LOOP ( 'NONE', ( #642, #96 ) ) ;
#39000 = CARTESIAN_POINT ( 'NONE',  ( 0.5132697287564000899, -81.97938944371999526, -1.623690596030999744 ) ) ;
#39001 = CARTESIAN_POINT ( 'NONE',  ( -0.4036326496859999891, -80.28882331289000263, 1.533452771621000021 ) ) ;
#39002 = CARTESIAN_POINT ( 'NONE',  ( -11.59999999999999964, -90.29999999999999716, 0.000000000000000000 ) ) ;
#39003 = CARTESIAN_POINT ( 'NONE',  ( -5.261498566940000288, -77.65492149134999522, -10.76255997729999869 ) ) ;
#39004 = CARTESIAN_POINT ( 'NONE',  ( -12.00000000000000000, -77.39999999999999147, 0.000000000000000000 ) ) ;
#39005 = EDGE_CURVE ( 'NONE', #46158, #11615, #28365, .T. ) ;
#39006 = CARTESIAN_POINT ( 'NONE',  ( -1.324613189995999862, -83.25004272349499956, -0.7038465009425000085 ) ) ;
#39007 = CARTESIAN_POINT ( 'NONE',  ( -1.680220311666482003, -1.835405696757452132, -3.096472680378186570 ) ) ;
#39008 = CARTESIAN_POINT ( 'NONE',  ( -8.918806285220000518, -78.09745194988499861, 3.872830773119999570 ) ) ;
#39009 = CARTESIAN_POINT ( 'NONE',  ( -3.470329948268000120, -78.04774788529299201, 8.867197205552999506 ) ) ;
#39010 = CARTESIAN_POINT ( 'NONE',  ( -10.73439844295906731, -76.59513923058339913, 0.6615022803101073823 ) ) ;
#39011 = DIRECTION ( 'NONE',  ( -0.7071067812094167238, -2.924114041541068650E-07, -0.7071067811636178035 ) ) ;
#39012 = CARTESIAN_POINT ( 'NONE',  ( -1.175893850647310446, -82.11831640066738203, 0.4910670358417331127 ) ) ;
#39013 = ORIENTED_EDGE ( 'NONE', *, *, #25745, .F. ) ;
#39014 = CARTESIAN_POINT ( 'NONE',  ( 0.000000000000000000, -75.20000000000000284, -8.199999999999999289 ) ) ;
#39015 = CARTESIAN_POINT ( 'NONE',  ( -1.199500263597274241, -79.34791666666667709, 0.9218200799623669228 ) ) ;
#39016 = CARTESIAN_POINT ( 'NONE',  ( 12.17932748403999987, -79.56684242973399535, -1.499464232310999900 ) ) ;
#39017 = CARTESIAN_POINT ( 'NONE',  ( -3.999289396772167660, -78.69999999999998863, 0.07539443523754783827 ) ) ;
#39018 = CARTESIAN_POINT ( 'NONE',  ( -0.7803569495551999635, -81.91581342370000129, -1.471836271561000054 ) ) ;
#39019 = CARTESIAN_POINT ( 'NONE',  ( 11.19952915612999966, -78.07946914900300328, -0.6234238306063999424 ) ) ;
#39020 = CARTESIAN_POINT ( 'NONE',  ( -4.985523414424999800, -78.45732655911598386, -9.777963635945001286 ) ) ;
#39021 = CARTESIAN_POINT ( 'NONE',  ( 10.13694968398000107, -23.70834319340999841, -7.646073915527999532 ) ) ;
#39022 = DIRECTION ( 'NONE',  ( 0.000000000000000000, 1.000000000000000000, 0.000000000000000000 ) ) ;
#39023 = CARTESIAN_POINT ( 'NONE',  ( 9.176121104939999995, -76.88349069267898983, 7.967706572806000587 ) ) ;
#39024 = CARTESIAN_POINT ( 'NONE',  ( 12.00000000000000000, -18.84999999997999964, -0.7999999999999001243 ) ) ;
#39025 = CARTESIAN_POINT ( 'NONE',  ( -10.07627163191000008, -18.75000000240999753, 7.601397897754999633 ) ) ;
#39026 = ORIENTED_EDGE ( 'NONE', *, *, #47978, .F. ) ;
#39027 = CARTESIAN_POINT ( 'NONE',  ( -8.150086036219999386, -78.58228563835899649, 7.434906319739000402 ) ) ;
#39028 = CARTESIAN_POINT ( 'NONE',  ( -8.485281374238999419, -60.74999999967048581, 8.485281374238999419 ) ) ;
#39029 = CARTESIAN_POINT ( 'NONE',  ( 9.250000000000000000, -78.24999999999998579, -1.152201742116999973E-14 ) ) ;
#39030 = VECTOR ( 'NONE', #47915, 1000.000000000000000 ) ;
#39031 = CARTESIAN_POINT ( 'NONE',  ( 11.02792952375000013, -78.91278856042799816, -2.305147454016000186 ) ) ;
#39032 = ADVANCED_FACE ( 'NONE', ( #27036 ), #49501, .T. ) ;
#39033 = CARTESIAN_POINT ( 'NONE',  ( -6.043427764450786555, -76.88333333333332575, -10.48543666025110177 ) ) ;
#39034 = CARTESIAN_POINT ( 'NONE',  ( 1.250000000000000000, -78.25000000000000000, 0.000000000000000000 ) ) ;
#39035 = DIRECTION ( 'NONE',  ( 1.000000000000000000, 0.000000000000000000, 0.000000000000000000 ) ) ;
#39036 = CARTESIAN_POINT ( 'NONE',  ( 0.8726123492689907835, -82.02341677713879164, -1.234002077154575883 ) ) ;
#39037 = CARTESIAN_POINT ( 'NONE',  ( 0.08452963021239402741, -79.73065581606381613, -1.247426360802352141 ) ) ;
#39038 = CARTESIAN_POINT ( 'NONE',  ( -10.75000000000000355, -79.48958333333334281, 1.407171709420384609 ) ) ;
#39039 = CARTESIAN_POINT ( 'NONE',  ( 1.034214221880000141E-14, 0.2999999999999999334, 0.000000000000000000 ) ) ;
#39040 = CARTESIAN_POINT ( 'NONE',  ( -12.68624828429000040, -23.76426636002999970, 1.886933512377000133 ) ) ;
#39041 = ORIENTED_EDGE ( 'NONE', *, *, #31899, .T. ) ;
#39042 = ORIENTED_EDGE ( 'NONE', *, *, #36699, .T. ) ;
#39043 = CARTESIAN_POINT ( 'NONE',  ( -12.77568125274000010, -53.53490786090000597, -0.5296379231473000715 ) ) ;
#39044 = ORIENTED_EDGE ( 'NONE', *, *, #9490, .F. ) ;
#39045 = ORIENTED_EDGE ( 'NONE', *, *, #30539, .F. ) ;
#39046 = PLANE ( 'NONE',  #27346 ) ;
#39047 = CARTESIAN_POINT ( 'NONE',  ( 10.78933672403999999, -76.81123958467900081, -1.663003020634000073 ) ) ;
#39048 = CARTESIAN_POINT ( 'NONE',  ( -3.292576784871000140, -78.35493667140100627, -9.347695904456999827 ) ) ;
#39049 = CARTESIAN_POINT ( 'NONE',  ( 0.5449807741670494865, -78.22973173042375095, -9.235034757777352610 ) ) ;
#39050 = CARTESIAN_POINT ( 'NONE',  ( -5.394429334091999984, -79.78339274672698878, -9.834543342166998769 ) ) ;
#39051 = AXIS2_PLACEMENT_3D ( 'NONE', #2554, #57713, #16126 ) ;
#39052 = VERTEX_POINT ( 'NONE', #18210 ) ;
#39053 = ORIENTED_EDGE ( 'NONE', *, *, #48256, .F. ) ;
#39054 = CARTESIAN_POINT ( 'NONE',  ( -6.550240698926310223, -77.53778409855667064, 6.531065114973362284 ) ) ;
#39055 = DIRECTION ( 'NONE',  ( 0.000000000000000000, 0.000000000000000000, 1.000000000000000000 ) ) ;
#39056 = CARTESIAN_POINT ( 'NONE',  ( -12.79972228485999963, -60.59021513420999838, -2.019125729023000027 ) ) ;
#39057 = CARTESIAN_POINT ( 'NONE',  ( -0.5548610165507998904, -77.95059892722998995, -9.688283574444998436 ) ) ;
#39058 = PRODUCT_RELATED_PRODUCT_CATEGORY ( 'part', '', ( #8796 ) ) ;
#39059 = CARTESIAN_POINT ( 'NONE',  ( 7.624341766656999475, -60.06485146221000093, 10.42531125026000005 ) ) ;
#39060 = CARTESIAN_POINT ( 'NONE',  ( 10.75000000000000355, -76.73958333333331439, -1.407171709420407035 ) ) ;
#39061 = CARTESIAN_POINT ( 'NONE',  ( 1.791008777272000030, -80.29243406013898721, 11.11143388882000060 ) ) ;
#39062 = CARTESIAN_POINT ( 'NONE',  ( 1.623222485893000000, -80.54441198108999345, 0.5147482071316000773 ) ) ;
#39063 = AXIS2_PLACEMENT_3D ( 'NONE', #45456, #54309, #24169 ) ;
#39064 = CARTESIAN_POINT ( 'NONE',  ( 1.980464439859999981, -58.55472017426999543, 12.85144117154000121 ) ) ;
#39065 = CARTESIAN_POINT ( 'NONE',  ( -9.759527141425989427, -76.65258383443992329, 6.542760971238160472 ) ) ;
#39066 = APPLICATION_CONTEXT ( 'automotive_design' ) ;
#39067 = VERTEX_POINT ( 'NONE', #36201 ) ;
#39068 = CARTESIAN_POINT ( 'NONE',  ( -8.188285776285999518, -54.09506253957000155, 9.395726099541001020 ) ) ;
#39069 = CARTESIAN_POINT ( 'NONE',  ( -5.644471715163000169, -77.93073667140099303, 8.009852484315999277 ) ) ;
#39070 = AXIS2_PLACEMENT_3D ( 'NONE', #10756, #31994, #50034 ) ;
#39071 = CARTESIAN_POINT ( 'NONE',  ( 9.148490208346998998, -78.00753312129299388, 7.734416031130999514 ) ) ;
#39072 = CARTESIAN_POINT ( 'NONE',  ( -10.01676960212000012, -18.79061945240999876, -7.658895148207999881 ) ) ;
#39073 = EDGE_CURVE ( 'NONE', #47139, #21820, #32915, .T. ) ;
#39075 = CARTESIAN_POINT ( 'NONE',  ( -0.005119011380219999283, -17.06186137810999881, -12.43705489344000092 ) ) ;
#39074 = CARTESIAN_POINT ( 'NONE',  ( 7.705142895613999343, -57.04916621739000249, 10.24998526317999925 ) ) ;
#39076 = CARTESIAN_POINT ( 'NONE',  ( -7.596835002782709623, -78.85208333333333997, -5.838193839761696147 ) ) ;
#39077 = CARTESIAN_POINT ( 'NONE',  ( -11.02922838689999985, -80.07413114498598361, -2.420755946928999869 ) ) ;
#39078 = CYLINDRICAL_SURFACE ( 'NONE', #31370, 1.500000000000000000 ) ;
#39079 = CARTESIAN_POINT ( 'NONE',  ( 7.538328940029000336, -77.00676689867499647, -8.367052130149000178 ) ) ;
#39080 = CARTESIAN_POINT ( 'NONE',  ( 12.50680023853920630, -24.30414033429958209, 1.424451025645361302 ) ) ;
#39081 = CARTESIAN_POINT ( 'NONE',  ( 5.516100435859000228, -80.15765279019329625, 9.811525831467001524 ) ) ;
#39082 = EDGE_CURVE ( 'NONE', #25591, #52707, #12481, .T. ) ;
#39083 = ORIENTED_EDGE ( 'NONE', *, *, #51017, .T. ) ;
#39084 = DIRECTION ( 'NONE',  ( 0.000000000000000000, 1.000000000000000000, 0.000000000000000000 ) ) ;
#39085 = CARTESIAN_POINT ( 'NONE',  ( -12.50659871785105892, -24.97347219492468540, 0.3508073941911192817 ) ) ;
#39086 = CARTESIAN_POINT ( 'NONE',  ( -12.71658872085999903, -18.68415268018999953, 1.931087888240000217 ) ) ;
#39087 = CARTESIAN_POINT ( 'NONE',  ( 3.596145366532999876, -2.894607885732999986, 0.5996453614708999735 ) ) ;
#39088 = DIRECTION ( 'NONE',  ( 1.000000000000000000, 0.000000000000000000, 0.000000000000000000 ) ) ;
#39089 = CARTESIAN_POINT ( 'NONE',  ( -3.862434228255000157, -79.36513192999699129, 8.716192152569998797 ) ) ;
#39090 = CARTESIAN_POINT ( 'NONE',  ( -12.77657003520000067, -53.48789974419999993, 0.1588669551757000142 ) ) ;
#39091 = CARTESIAN_POINT ( 'NONE',  ( 2.062312494845999655, -60.02715659860000130, 12.83634740211000036 ) ) ;
#39092 = DIRECTION ( 'NONE',  ( 0.000000000000000000, 0.000000000000000000, -1.000000000000000000 ) ) ;
#39093 = CARTESIAN_POINT ( 'NONE',  ( 0.000000000000000000, -32.88214388149999934, 0.000000000000000000 ) ) ;
#39094 = FACE_OUTER_BOUND ( 'NONE', #37525, .T. ) ;
#39095 = CARTESIAN_POINT ( 'NONE',  ( -7.973554211391000734, -77.36784033438198094, -7.659671442301999811 ) ) ;
#39096 = CONICAL_SURFACE ( 'NONE', #36273, 2.949999999500999781, 0.7853981633972997312 ) ;
#39097 = CARTESIAN_POINT ( 'NONE',  ( 10.11784875172895148, -76.40690788625481389, -5.985750144463405142 ) ) ;
#39098 = CARTESIAN_POINT ( 'NONE',  ( 3.831242997621999713, -76.98791202109900667, 10.34520717408000046 ) ) ;
#39099 = EDGE_CURVE ( 'NONE', #21408, #11254, #37467, .T. ) ;
#39100 = CARTESIAN_POINT ( 'NONE',  ( 8.838834764832000701, -55.54999999966999980, -8.838834764832000701 ) ) ;
#39101 = CARTESIAN_POINT ( 'NONE',  ( 7.710118476742000126, -20.25022860572000027, 10.18499221090000084 ) ) ;
#39102 = DIRECTION ( 'NONE',  ( 0.000000000000000000, -1.000000000000000000, 0.000000000000000000 ) ) ;
#39103 = CARTESIAN_POINT ( 'NONE',  ( -1.500000000000000000, -79.00000000000000000, 0.000000000000000000 ) ) ;
#39104 = CARTESIAN_POINT ( 'NONE',  ( 5.539808784079867543, -77.43333333333333712, 9.611650271896852615 ) ) ;
#39105 = CARTESIAN_POINT ( 'NONE',  ( 0.4840504722130451465, -80.22894859189042904, -10.73925919085179359 ) ) ;
#39106 = CARTESIAN_POINT ( 'NONE',  ( -7.624341764923000753, -18.73514850530999709, -10.42531124853000080 ) ) ;
#39107 = CARTESIAN_POINT ( 'NONE',  ( 10.49326040991128828, -80.07116553579604101, -3.963973988046216146 ) ) ;
#39108 = CARTESIAN_POINT ( 'NONE',  ( 7.958763982157000427, -54.32301960771999916, 9.723170657500999070 ) ) ;
#39109 = CIRCLE ( 'NONE', #23054, 9.549999999999998934 ) ;
#39110 = CARTESIAN_POINT ( 'NONE',  ( 1.250000000000000000, -81.74999999999998579, 0.000000000000000000 ) ) ;
#39111 = DIRECTION ( 'NONE',  ( 0.000000000000000000, 1.000000000000000000, 0.000000000000000000 ) ) ;
#39112 = CARTESIAN_POINT ( 'NONE',  ( -0.5999999999999999778, -5.200000000000000178, 0.5999999999999999778 ) ) ;
#39113 = EDGE_LOOP ( 'NONE', ( #9719, #24014, #44787, #363, #168, #25897 ) ) ;
#39114 = ADVANCED_FACE ( 'NONE', ( #6947 ), #6656, .F. ) ;
#39115 = CARTESIAN_POINT ( 'NONE',  ( -1.081559480311999888, -0.7500000000000000000, 3.328697807033000000 ) ) ;
#39116 = EDGE_CURVE ( 'NONE', #46485, #8218, #33511, .T. ) ;
#39117 = ORIENTED_EDGE ( 'NONE', *, *, #57844, .F. ) ;
#39118 = ORIENTED_EDGE ( 'NONE', *, *, #37333, .T. ) ;
#39119 = FACE_OUTER_BOUND ( 'NONE', #16597, .T. ) ;
#39120 = ORIENTED_EDGE ( 'NONE', *, *, #11118, .F. ) ;
#39121 = CARTESIAN_POINT ( 'NONE',  ( 1.376968171896000070, -80.72674124465299883, -3.266332797073000282 ) ) ;
#39122 = CARTESIAN_POINT ( 'NONE',  ( -6.579782092783524661, -79.33575076626789269, 6.852906106304269329 ) ) ;
#39123 = ORIENTED_EDGE ( 'NONE', *, *, #5039, .F. ) ;
#39124 = CARTESIAN_POINT ( 'NONE',  ( 0.2746856994466179147, -82.74303240917123503, -1.219238289928273211 ) ) ;
#39125 = CARTESIAN_POINT ( 'NONE',  ( 8.082524092276891281, -79.70833333333332860, -4.658475568430806568 ) ) ;
#39126 = ORIENTED_EDGE ( 'NONE', *, *, #42688, .T. ) ;
#39127 = CARTESIAN_POINT ( 'NONE',  ( 12.50000000000000000, -23.24999999688999708, 1.750000000000000000 ) ) ;
#39128 = CARTESIAN_POINT ( 'NONE',  ( -8.615032359022308128, -80.04915988844547314, 6.429856405177485357 ) ) ;
#39129 = DIRECTION ( 'NONE',  ( 0.7026410690473250398, -0.1122098755728047209, -0.7026410690473250398 ) ) ;
#39130 = EDGE_CURVE ( 'NONE', #36944, #20252, #56789, .T. ) ;
#39131 = CARTESIAN_POINT ( 'NONE',  ( 0.000000000000000000, -49.87071424677999687, 0.000000000000000000 ) ) ;
#39132 = CARTESIAN_POINT ( 'NONE',  ( -1.963210506780999953, -76.44485224922898681, -11.00998129987999974 ) ) ;
#39133 = DIRECTION ( 'NONE',  ( 0.000000000000000000, 0.000000000000000000, 1.000000000000000000 ) ) ;
#39134 = CARTESIAN_POINT ( 'NONE',  ( -11.00000000000000711, -78.68958333333334565, 1.439896632895276696 ) ) ;
#39135 = AXIS2_PLACEMENT_3D ( 'NONE', #33197, #46533, #10498 ) ;
#39136 = CARTESIAN_POINT ( 'NONE',  ( -8.025391215536000544, -76.45193055640599766, -7.688479554171000707 ) ) ;
#39137 = FACE_OUTER_BOUND ( 'NONE', #29501, .T. ) ;
#39138 = CARTESIAN_POINT ( 'NONE',  ( 0.3292142484335000563, -79.36673629165399291, -1.292352404326999826 ) ) ;
#39139 = AXIS2_PLACEMENT_3D ( 'NONE', #22426, #45174, #54321 ) ;
#39140 = CARTESIAN_POINT ( 'NONE',  ( 0.000000000000000000, -74.70999999999999375, 0.000000000000000000 ) ) ;
#39141 = CARTESIAN_POINT ( 'NONE',  ( 2.613303202534924541, -2.902163255836463840, 1.941981267590990656 ) ) ;
#39142 = CARTESIAN_POINT ( 'NONE',  ( -0.3705230124191999930, -80.49350264934798815, -3.525290978833000022 ) ) ;
#39143 = CARTESIAN_POINT ( 'NONE',  ( 3.250000000000000000, -1.250000000000000000, 0.000000000000000000 ) ) ;
#39144 = CARTESIAN_POINT ( 'NONE',  ( -0.3097977128257069501, -80.97757901313826778, 10.75868109506080472 ) ) ;
#39145 = CARTESIAN_POINT ( 'NONE',  ( 3.432824520865000117, -83.87669503318799968, -0.8929043418966999823 ) ) ;
#39146 = CARTESIAN_POINT ( 'NONE',  ( -3.448863046786000197, -1.782744131007000021, -1.608907009436000068 ) ) ;
#39147 = CARTESIAN_POINT ( 'NONE',  ( 12.00000000000000000, -79.14999999999999147, 0.000000000000000000 ) ) ;
#39148 = EDGE_CURVE ( 'NONE', #35206, #39734, #11463, .T. ) ;
#39149 = CARTESIAN_POINT ( 'NONE',  ( -7.756281347497000489, -61.02006031080999549, -10.15825374577000062 ) ) ;
#39150 = VECTOR ( 'NONE', #29338, 1000.000000000000000 ) ;
#39151 = CARTESIAN_POINT ( 'NONE',  ( -9.134410136912352485, -79.24350122207665947, 7.854726423800818758 ) ) ;
#39152 = CARTESIAN_POINT ( 'NONE',  ( -1.200131629027000102, -80.74444067939001002, -0.3495483843597000373 ) ) ;
#39153 = B_SPLINE_CURVE_WITH_KNOTS ( 'NONE', 3,
 ( #11780, #43080, #48660, #52507, #57503, #12064 ),
 .UNSPECIFIED., .F., .F.,
 ( 4, 2, 4 ),
 ( 0.000000000000000000, 0.5000000000000000000, 1.000000000000000000 ),
 .UNSPECIFIED. ) ;
#39154 = CARTESIAN_POINT ( 'NONE',  ( 12.57042253521000141, -26.10094976978000147, 0.000000000000000000 ) ) ;
#39155 = CARTESIAN_POINT ( 'NONE',  ( 5.512103878356000131, -76.89219232727998588, 11.78783395355999986 ) ) ;
#39156 = CARTESIAN_POINT ( 'NONE',  ( -10.13785388426000011, -78.34083892477998745, -4.205702700205000255 ) ) ;
#39157 = CARTESIAN_POINT ( 'NONE',  ( 1.980584515752000119, -23.26485146623999967, -12.76303204602000108 ) ) ;
#39158 = CARTESIAN_POINT ( 'NONE',  ( -1.099509683757999845, -76.19937248742999714, -12.31320345612999922 ) ) ;
#39159 = ORIENTED_EDGE ( 'NONE', *, *, #16105, .T. ) ;
#39160 = CARTESIAN_POINT ( 'NONE',  ( -1.123310606857000016, -80.39374047146120006, -11.35014609800000152 ) ) ;
#39161 = CARTESIAN_POINT ( 'NONE',  ( 12.55486071739000131, -60.95393632975000031, 1.580832792523999775 ) ) ;
#39162 = CARTESIAN_POINT ( 'NONE',  ( 6.122063361877000176, -79.24616473471999711, -11.23243970840999850 ) ) ;
#39163 = CARTESIAN_POINT ( 'NONE',  ( 7.668936932643000581, -19.22847221992000044, -10.21380041495000057 ) ) ;
#39164 = CARTESIAN_POINT ( 'NONE',  ( -9.275907895452998986, -77.87139044835899426, 2.590510119660999866 ) ) ;
#39165 = CARTESIAN_POINT ( 'NONE',  ( -2.683124628265999956, -83.42080844866399048, -3.195452193269000318 ) ) ;
#39166 = CARTESIAN_POINT ( 'NONE',  ( -12.56594317984999876, -18.75000000536999778, 1.750000000000000000 ) ) ;
#39167 = CARTESIAN_POINT ( 'NONE',  ( -0.3603946542032999689, -79.38485486817801018, 1.573953487139999829 ) ) ;
#39168 = ORIENTED_EDGE ( 'NONE', *, *, #3634, .T. ) ;
#39169 = CARTESIAN_POINT ( 'NONE',  ( 4.601781879248937557, -78.93432654680742644, 8.115879808169474074 ) ) ;
#39170 = CARTESIAN_POINT ( 'NONE',  ( 1.262641813692434667, -78.92689010668476612, -3.687440721609341665 ) ) ;
#39171 = ORIENTED_EDGE ( 'NONE', *, *, #5160, .T. ) ;
#39172 = CARTESIAN_POINT ( 'NONE',  ( -8.032634178075001685, -78.43019927879299757, -7.427287829177999789 ) ) ;
#39173 = CARTESIAN_POINT ( 'NONE',  ( -7.452378523310481562, -55.25278097498677710, -8.090910852015047894 ) ) ;
#39174 = VECTOR ( 'NONE', #299, 1000.000000000000000 ) ;
#39175 = CARTESIAN_POINT ( 'NONE',  ( 1.785229341567000194, -80.23309620847798840, 11.07557821988999969 ) ) ;
#39176 = EDGE_LOOP ( 'NONE', ( #172, #19741, #51343, #15879, #56627 ) ) ;
#39177 = VERTEX_POINT ( 'NONE', #33796 ) ;
#39178 = ORIENTED_EDGE ( 'NONE', *, *, #25817, .F. ) ;
#39179 = CARTESIAN_POINT ( 'NONE',  ( 1.250000000000000000, -80.34999999999999432, 0.000000000000000000 ) ) ;
#39180 = DIRECTION ( 'NONE',  ( 1.155082973713999823E-13, 0.000000000000000000, 1.000000000000000000 ) ) ;
#39181 = CARTESIAN_POINT ( 'NONE',  ( 9.523132023602000729, -80.50917187374454898, 1.108936319727999997 ) ) ;
#39182 = ORIENTED_EDGE ( 'NONE', *, *, #7238, .T. ) ;
#39183 = CARTESIAN_POINT ( 'NONE',  ( 12.43641395959999940, -53.88198970716000247, -0.03481089025435999545 ) ) ;
#39184 = ORIENTED_EDGE ( 'NONE', *, *, #42515, .T. ) ;
#39185 = CARTESIAN_POINT ( 'NONE',  ( -12.26143800982999998, -79.05153930436631526, -0.2371146996492999870 ) ) ;
#39186 = CARTESIAN_POINT ( 'NONE',  ( 3.399999999999689493, -78.72609999968184979, -2.006589542798614012 ) ) ;
#39187 = CARTESIAN_POINT ( 'NONE',  ( 8.260145278118999457, -53.85964900942000355, 9.643338478971999805 ) ) ;
#39188 = EDGE_CURVE ( 'NONE', #28511, #30828, #51837, .T. ) ;
#39189 = DIRECTION ( 'NONE',  ( 0.7071067811865475727, 0.000000000000000000, 0.7071067811865475727 ) ) ;
#39190 = CARTESIAN_POINT ( 'NONE',  ( -1.199500263597274241, -78.34791666666666288, 0.9218200799623669228 ) ) ;
#39191 = CARTESIAN_POINT ( 'NONE',  ( 7.765002223030514017, -77.37977859133056313, -8.854379362200837988 ) ) ;
#39192 = CARTESIAN_POINT ( 'NONE',  ( 4.311778524607963625, -80.50626779744442274, -10.34858355512559314 ) ) ;
#39193 = CARTESIAN_POINT ( 'NONE',  ( -8.485281374238999419, -23.25000000000000000, 8.485281374238999419 ) ) ;
#39194 = CARTESIAN_POINT ( 'NONE',  ( 9.074254517363083750, -78.83453198432620468, -1.794298757601813010 ) ) ;
#39195 = CARTESIAN_POINT ( 'NONE',  ( -7.659225027811000786, -23.68266641665999828, 9.963489011784998794 ) ) ;
#39196 = CARTESIAN_POINT ( 'NONE',  ( 4.115854587004999843, -80.92957046129099297, -0.6828514729849000098 ) ) ;
#39197 = DIRECTION ( 'NONE',  ( 1.000000000000000000, 0.000000000000000000, 0.000000000000000000 ) ) ;
#39198 = CARTESIAN_POINT ( 'NONE',  ( -12.66315144086999922, -16.82197088188999601, -0.06064144874954999209 ) ) ;
#39199 = CARTESIAN_POINT ( 'NONE',  ( -11.00000000000000000, -78.09999999999999432, 2.733298954964999989E-14 ) ) ;
#39200 = CARTESIAN_POINT ( 'NONE',  ( 1.298131932841000147, -76.36488988309598369, 12.21218573294999921 ) ) ;
#39201 = CARTESIAN_POINT ( 'NONE',  ( -1.045756772073208829, -81.19753128763325378, 0.8139332635508695901 ) ) ;
#39202 = ADVANCED_FACE ( 'NONE', ( #42390 ), #38863, .T. ) ;
#39203 = CARTESIAN_POINT ( 'NONE',  ( -3.245126138204999844, -1.829671397435000069, -1.541643571398999990 ) ) ;
#39204 = DIRECTION ( 'NONE',  ( 0.9999999924279685537, 0.000000000000000000, 0.0001230612157836962969 ) ) ;
#39205 = AXIS2_PLACEMENT_3D ( 'NONE', #9098, #50431, #32387 ) ;
#39206 = B_SPLINE_CURVE_WITH_KNOTS ( 'NONE', 3,
 ( #27379, #45416, #27668, #37113 ),
 .UNSPECIFIED., .F., .F.,
 ( 4, 4 ),
 ( 0.000000000000000000, 1.000000000000000000 ),
 .UNSPECIFIED. ) ;
#39207 = CARTESIAN_POINT ( 'NONE',  ( 0.7440580446819816673, -81.08396281512723647, 1.316460893200364746 ) ) ;
#39208 = CARTESIAN_POINT ( 'NONE',  ( 12.70926857202000093, -60.20841990675999966, -1.933876778424000076 ) ) ;
#39209 = DIRECTION ( 'NONE',  ( 0.000000000000000000, 1.000000000000000000, 0.000000000000000000 ) ) ;
#39210 = B_SPLINE_CURVE_WITH_KNOTS ( 'NONE', 3,
 ( #47465, #52445, #47746, #10855, #7279, #34121, #2570, #20282, #38570, #25281, #2855, #15264, #1705, #20852, #24421, #56876, #12004, #29983, #56584, #19699, #38278, #15851, #55717, #28828, #42435, #33257, #6112, #33839, #37985, #16144, #51299, #56010, #15560, #46087, #41635, #18913, #31295, #4459, #31592, #5045, #18629, #36621, #50215, #33274, #29140, #38294, #41567, #42667, #50370, #23482, #55365, #41495, #37056, #55073, #50663, #10500, #24067, #37644, #28779, #19943, #37932, #2807, #42962, #2519, #11953, #34938, #47408, #4471, #52399, #29645, #34365, #16095, #40483, #26891, #43534, #3098, #38519, #56534, #47983, #20801, #43251, #12236, #29931, #34075, #38808, #21376, #44914, #22471, #12520, #6939, #56826, #52111, #15798, #47697, #7227, #51829, #48547, #52681, #52971, #33787, #25518, #11384, #7521, #29359, #21093, #25231, #39097, #57106, #43835, #16672, #34653, #8094, #30517, #30227, #48270, #7806, #3382, #25807, #57398, #16956, #36339, #41070, #657, #45512, #36921, #23055, #28055, #54365, #54071, #55224 ),
 .UNSPECIFIED., .F., .F.,
 ( 4, 2, 2, 2, 2, 2, 2, 1, 1, 1, 1, 1, 2, 2, 2, 2, 2, 1, 1, 1, 1, 1, 2, 2, 2, 2, 2, 1, 1, 1, 1, 2, 2, 2, 2, 2, 2, 2, 1, 1, 1, 1, 2, 2, 2, 2, 2, 2, 2, 1, 1, 1, 1, 1, 1, 2, 2, 2, 2, 2, 2, 1, 1, 1, 1, 2, 2, 2, 2, 2, 1, 1, 1, 2, 2, 2, 2, 1, 2, 2, 4 ),
 ( 0.000000000000000000, 0.06250000000016037172, 0.1250000000003207434, 0.1875000000004811151, 0.2187500000005612733, 0.2343750000006013245, 0.2421875000006213918, 0.2460937500006314671, 0.2480468750006364631, 0.2490234375006390166, 0.2495117187506402379, 0.2497558593756408762, 0.2498779296881412093, 0.2500000000006415424, 0.2812500000006000755, 0.2968750000005794809, 0.3046875000005691003, 0.3085937500005638823, 0.3105468750005613288, 0.3115234375005599965, 0.3120117187505592748, 0.3122558593755589418, 0.3123779296880587197, 0.3125000000005585532, 0.3437500000004944378, 0.3593750000004624079, 0.3671875000004463652, 0.3710937500004383716, 0.3730468750004343748, 0.3740234375004323764, 0.3745117187504313216, 0.3747558593754308220, 0.3750000000004302669, 0.4062500000003576028, 0.4218750000003212985, 0.4375000000002849387, 0.4687500000002122746, 0.4843750000001759703, 0.4921875000001578182, 0.4960937500001487144, 0.4980468750001442180, 0.4990234375001419420, 0.4995117187501407763, 0.5000000000001396661, 0.5624999999999947820, 0.6249999999998500089, 0.6874999999997051248, 0.7187499999996328492, 0.7343749999995966560, 0.7421874999995784483, 0.7460937499995694555, 0.7480468749995650146, 0.7490234374995626832, 0.7495117187495616839, 0.7497558593745610178, 0.7498779296870606847, 0.7499999999995603517, 0.7812499999996209699, 0.7968749999996512789, 0.8046874999996664890, 0.8085937499996740385, 0.8105468749996778133, 0.8115234374996798117, 0.8120117187496806999, 0.8122558593746812550, 0.8123779296871814770, 0.8124999999996815880, 0.8437499999997338795, 0.8593749999997600808, 0.8671874999997730704, 0.8710937499997796207, 0.8730468749997828404, 0.8740234374997843947, 0.8745117187497852829, 0.8749999999997860600, 0.9062499999998396838, 0.9218749999998664402, 0.9296874999998798739, 0.9335937499998865352, 0.9374999999998931965, 1.000000000000000000 ),
 .UNSPECIFIED. ) ;
#39211 = CARTESIAN_POINT ( 'NONE',  ( 3.113245456484129203, -78.46450137413576442, -10.55002948983070610 ) ) ;
#39212 = CARTESIAN_POINT ( 'NONE',  ( 3.710074744828999904, -2.127759542060999820, -0.1726258946814999695 ) ) ;
#39213 = AXIS2_PLACEMENT_3D ( 'NONE', #9686, #22970, #40980 ) ;
#39214 = CARTESIAN_POINT ( 'NONE',  ( -8.607099856842999941, -77.57054998477100582, -8.432888219828999610 ) ) ;
#39215 = DIRECTION ( 'NONE',  ( 0.000000000000000000, 1.000000000000000000, 0.000000000000000000 ) ) ;
#39216 = ADVANCED_FACE ( 'NONE', ( #2528, #19653 ), #20531, .F. ) ;
#39218 = CARTESIAN_POINT ( 'NONE',  ( -8.130813118010999929, -17.31476110167000115, 9.546856411653001473 ) ) ;
#39217 = CARTESIAN_POINT ( 'NONE',  ( -8.485281374238999419, -59.94999999967000548, -8.485281374238999419 ) ) ;
#39219 = CARTESIAN_POINT ( 'NONE',  ( 1.467208996055999748, -82.48761497235999229, 0.6014104092625999209 ) ) ;
#39220 = CARTESIAN_POINT ( 'NONE',  ( -6.837720798360027885, -79.52994970263227970, 8.297335093543503959 ) ) ;
#39221 = ORIENTED_EDGE ( 'NONE', *, *, #24128, .F. ) ;
#39222 = CARTESIAN_POINT ( 'NONE',  ( -9.134410136912348932, -78.84350122207662537, 7.854726423800818758 ) ) ;
#39223 = CARTESIAN_POINT ( 'NONE',  ( -3.764285624315000245, -79.65891715040700660, 11.55877412955000061 ) ) ;
#39224 = EDGE_CURVE ( 'NONE', #18080, #11813, #23783, .T. ) ;
#39225 = CARTESIAN_POINT ( 'NONE',  ( -5.860463241014358005, -79.17777220148535378, 7.502936674103677817 ) ) ;
#39226 = CARTESIAN_POINT ( 'NONE',  ( -7.566790551998485270, -80.00000000000000000, -5.513831221825833850 ) ) ;
#39227 = CARTESIAN_POINT ( 'NONE',  ( -7.765022563386000165, -60.89093562068000409, 9.830785949133000301 ) ) ;
#39228 = CARTESIAN_POINT ( 'NONE',  ( -3.544559805645000061, -1.685986014850999970, 1.535826592584000005 ) ) ;
#39229 = CARTESIAN_POINT ( 'NONE',  ( -8.038032936864000888, -79.82032020290799323, -5.764166645736000127 ) ) ;
#39230 = PLANE ( 'NONE',  #15440 ) ;
#39231 = CARTESIAN_POINT ( 'NONE',  ( -12.70305331329071485, -53.76853698820474392, -0.8727610012296372899 ) ) ;
#39232 = ORIENTED_EDGE ( 'NONE', *, *, #42360, .F. ) ;
#39233 = CARTESIAN_POINT ( 'NONE',  ( -12.70610308055483628, -54.34479009111368697, 1.580620443374196382 ) ) ;
#39234 = CARTESIAN_POINT ( 'NONE',  ( -3.431352783032999731, -1.204516015699999887, 2.086989923523999924 ) ) ;
#39235 = CARTESIAN_POINT ( 'NONE',  ( -9.337827476838000962, -79.84366001420200121, -2.776632127938000405 ) ) ;
#39236 = CARTESIAN_POINT ( 'NONE',  ( 1.250000000000000000, -79.75000000000000000, 0.000000000000000000 ) ) ;
#39237 = CARTESIAN_POINT ( 'NONE',  ( -1.500000000000000222, -78.41041666666669130, -0.1963495408493622363 ) ) ;
#39238 = CARTESIAN_POINT ( 'NONE',  ( 1.356773869401999955, -79.47112212912999496, -0.9668579442890000708 ) ) ;
#39239 = ORIENTED_EDGE ( 'NONE', *, *, #34951, .T. ) ;
#39240 = CARTESIAN_POINT ( 'NONE',  ( -12.56594317982999875, -55.55000000504000468, 1.750000000000000000 ) ) ;
#39241 = CARTESIAN_POINT ( 'NONE',  ( -12.00000000000000000, -60.04999999966999980, -1.250000000000000000 ) ) ;
#39242 = CARTESIAN_POINT ( 'NONE',  ( 3.911993909898488830, -82.39999677995871252, -0.8315195909956012432 ) ) ;
#39243 = CARTESIAN_POINT ( 'NONE',  ( -0.6295237254636286695, -78.41666666666665719, 1.092232985442819881 ) ) ;
#39244 = CARTESIAN_POINT ( 'NONE',  ( 12.71536175399091739, -54.67444297152277954, -1.781227265980894758 ) ) ;
#39245 = VERTEX_POINT ( 'NONE', #37359 ) ;
#39246 = ORIENTED_EDGE ( 'NONE', *, *, #25665, .F. ) ;
#39247 = CARTESIAN_POINT ( 'NONE',  ( 1.318177213333999953, -76.62543624521698860, 12.40076185704000089 ) ) ;
#39248 = CARTESIAN_POINT ( 'NONE',  ( 4.145023818608256860, -78.75651719028334696, -9.918724640339455334 ) ) ;
#39249 = B_SPLINE_CURVE_WITH_KNOTS ( 'NONE', 3,
 ( #9376, #40959, #45401, #550, #18527, #36519 ),
 .UNSPECIFIED., .F., .F.,
 ( 4, 1, 1, 4 ),
 ( 0.000000000000000000, 0.3333333311575783497, 0.6666666623152567306, 0.9999999934728349693 ),
 .UNSPECIFIED. ) ;
#39250 = CARTESIAN_POINT ( 'NONE',  ( 0.4280957282384999507, -78.29268648134998898, -1.355413529770999936 ) ) ;
#39251 = ORIENTED_EDGE ( 'NONE', *, *, #18963, .F. ) ;
#39252 = CARTESIAN_POINT ( 'NONE',  ( -6.013262726775999489, -77.61973084965400460, 7.348341287529000176 ) ) ;
#39253 = B_SPLINE_CURVE_WITH_KNOTS ( 'NONE', 3,
 ( #11532, #29510, #25090, #52827, #11243, #57253, #43114, #12382, #29222, #47271 ),
 .UNSPECIFIED., .F., .F.,
 ( 4, 2, 2, 2, 4 ),
 ( 0.000000000000000000, 0.2500000000000000000, 0.5000000000000000000, 0.7500000000000000000, 1.000000000000000000 ),
 .UNSPECIFIED. ) ;
#39254 = VECTOR ( 'NONE', #26227, 1000.000000000000000 ) ;
#39255 = CARTESIAN_POINT ( 'NONE',  ( 8.796335266379964324, -77.50208333333333144, 6.760013919724087827 ) ) ;
#39256 = CARTESIAN_POINT ( 'NONE',  ( -11.75000000000000355, -75.81041666666666856, -1.538071403320004249 ) ) ;
#39257 = AXIS2_PLACEMENT_3D ( 'NONE', #1939, #42075, #28767 ) ;
#39258 = CARTESIAN_POINT ( 'NONE',  ( -9.416026390438000604, -78.70544818976000556, 6.872484323511000248 ) ) ;
#39259 = CONICAL_SURFACE ( 'NONE', #15674, 13.94999999937999924, 0.7853981633972997312 ) ;
#39260 = CARTESIAN_POINT ( 'NONE',  ( -11.12496554189999820, -77.26019399548486888, -1.432917402686000097 ) ) ;
#39261 = FACE_OUTER_BOUND ( 'NONE', #14063, .T. ) ;
#39262 = CARTESIAN_POINT ( 'NONE',  ( 1.460959015002472494, -79.77083333333334281, 0.3926218265389233020 ) ) ;
#39263 = CARTESIAN_POINT ( 'NONE',  ( -7.408849624938999234, -79.46926788952099230, -8.421820339245000397 ) ) ;
#39264 = CARTESIAN_POINT ( 'NONE',  ( -0.7277978613523643503, -79.98136350393239979, 9.221261735625438050 ) ) ;
#39265 = CIRCLE ( 'NONE', #4384, 13.89999999999999858 ) ;
#39266 = ORIENTED_EDGE ( 'NONE', *, *, #4461, .T. ) ;
#39267 = CARTESIAN_POINT ( 'NONE',  ( 10.71485332735033502, -80.17911206518367351, -2.929766398920109705 ) ) ;
#39268 = ORIENTED_EDGE ( 'NONE', *, *, #52545, .F. ) ;
#39269 = CARTESIAN_POINT ( 'NONE',  ( -0.6687410688009000070, -80.00053993242899253, 11.24641019779000040 ) ) ;
#39270 = CARTESIAN_POINT ( 'NONE',  ( 9.249996844504634552, -77.35002626973081874, 0.002854433395025519210 ) ) ;
#39271 = CARTESIAN_POINT ( 'NONE',  ( -1.200597545982000192, -80.77594520594300320, -0.5467811674232999630 ) ) ;
#39272 = DIRECTION ( 'NONE',  ( -0.7071067812863980340, -6.386265919119980056E-09, 0.7071067810866970005 ) ) ;
#39273 = CARTESIAN_POINT ( 'NONE',  ( 12.05000000000000071, -75.80000000000001137, 0.000000000000000000 ) ) ;
#39274 = CARTESIAN_POINT ( 'NONE',  ( 1.505666248717000055, -78.80671151888600434, 0.1786365444185999962 ) ) ;
#39275 = LINE ( 'NONE', #25695, #27553 ) ;
#39276 = FACE_OUTER_BOUND ( 'NONE', #49078, .T. ) ;
#39277 = CARTESIAN_POINT ( 'NONE',  ( -2.421270742014151267, -77.70429338144477072, -9.009162903448457271 ) ) ;
#39278 = CARTESIAN_POINT ( 'NONE',  ( -12.60413670420000010, -18.69283319134000010, -1.799502287691000069 ) ) ;
#39279 = CARTESIAN_POINT ( 'NONE',  ( 1.000000000000000000, -81.99999999999998579, 7.000000000000000000 ) ) ;
#39280 = CARTESIAN_POINT ( 'NONE',  ( -0.6558374186847000242, -79.87278845086298418, 11.02940581592999969 ) ) ;
#39281 = EDGE_CURVE ( 'NONE', #23434, #28137, #194, .T. ) ;
#39282 = CARTESIAN_POINT ( 'NONE',  ( -6.173435753739000553, -76.93948667140098507, 6.984674784554999682 ) ) ;
#39283 = CARTESIAN_POINT ( 'NONE',  ( 8.838834764832000701, -60.04999999966999980, 8.838834764832000701 ) ) ;
#39284 = CARTESIAN_POINT ( 'NONE',  ( 1.960122366415000261, -79.68942003686028386, 3.682998213212000049 ) ) ;
#39285 = CARTESIAN_POINT ( 'NONE',  ( 8.596418555780418913, -77.80208333333332860, 6.606377239730356621 ) ) ;
#39286 = EDGE_LOOP ( 'NONE', ( #55451, #27466, #35238, #36289 ) ) ;
#39287 = FACE_OUTER_BOUND ( 'NONE', #38612, .T. ) ;
#39288 = CARTESIAN_POINT ( 'NONE',  ( -1.551612880221999946, -79.90986802222998620, -0.3269472641410000047 ) ) ;
#39289 = CARTESIAN_POINT ( 'NONE',  ( 7.919595949288999570, -55.64999999964999233, -9.050966799188000067 ) ) ;
#39290 = CARTESIAN_POINT ( 'NONE',  ( 11.36821324764999908, -77.79056806846899974, -3.778861202892000115 ) ) ;
#39291 = CARTESIAN_POINT ( 'NONE',  ( -12.74365836115054407, -18.47810168887382076, 1.980611005600014574 ) ) ;
#39292 = DIRECTION ( 'NONE',  ( 0.000000000000000000, -1.000000000000000000, 0.000000000000000000 ) ) ;
#39293 = CARTESIAN_POINT ( 'NONE',  ( -3.001381142052446549, -2.206320731719022543, 1.838231690380543348 ) ) ;
#39294 = CARTESIAN_POINT ( 'NONE',  ( -5.505695391233000002, -78.76725584965399207, -8.014431902511001127 ) ) ;
#39295 = CARTESIAN_POINT ( 'NONE',  ( -2.142155038640999987, -77.53611896097199008, 9.278014228403000274 ) ) ;
#39296 = LINE ( 'NONE', #36025, #1878 ) ;
#39297 = LINE ( 'NONE', #29847, #32816 ) ;
#39298 = CARTESIAN_POINT ( 'NONE',  ( 12.00000000000000000, -78.54999999999999716, 0.000000000000000000 ) ) ;
#39299 = CARTESIAN_POINT ( 'NONE',  ( -1.213379087956198310, -81.62537046322781009, 0.3916290527410095090 ) ) ;
#39300 = ORIENTED_EDGE ( 'NONE', *, *, #26943, .T. ) ;
#39301 = CARTESIAN_POINT ( 'NONE',  ( 10.99999999999999822, -18.25000000000000000, -0.1600933372615688799 ) ) ;
#39302 = DIRECTION ( 'NONE',  ( -1.000000000000000000, 0.000000000000000000, 0.000000000000000000 ) ) ;
#39303 = CARTESIAN_POINT ( 'NONE',  ( 4.260122498627000098, -79.67337695312400569, 11.50807400234999989 ) ) ;
#39304 = EDGE_CURVE ( 'NONE', #45130, #2960, #34641, .T. ) ;
#39305 = CARTESIAN_POINT ( 'NONE',  ( 2.322889840689456697, -78.69999999999998863, -4.022071228304650248 ) ) ;
#39306 = CARTESIAN_POINT ( 'NONE',  ( -1.374853770045000090, -81.30921723553998959, -0.7192078502473999713 ) ) ;
#39307 = CARTESIAN_POINT ( 'NONE',  ( -7.803863155890000236, -78.27012355001599531, 8.057160196619001624 ) ) ;
#39308 = CARTESIAN_POINT ( 'NONE',  ( 9.981840466370998755, -78.65397303944499185, 4.563647388395000171 ) ) ;
#39309 = CARTESIAN_POINT ( 'NONE',  ( 1.247385801071000166, -17.52277743742000027, -12.50301438876999960 ) ) ;
#39310 = CARTESIAN_POINT ( 'NONE',  ( 5.970850396337000099, -76.17430707708200543, -10.71897758064000072 ) ) ;
#39311 = CARTESIAN_POINT ( 'NONE',  ( 1.312204302215017826, -78.56237777671691447, 11.67681704195204517 ) ) ;
#39312 = CARTESIAN_POINT ( 'NONE',  ( -10.42531125070999920, -60.06485145371000556, 7.624341767111000756 ) ) ;
#39313 = ORIENTED_EDGE ( 'NONE', *, *, #19684, .F. ) ;
#39314 = CIRCLE ( 'NONE', #26111, 11.44999999999999929 ) ;
#39315 = CARTESIAN_POINT ( 'NONE',  ( -10.57985553746999940, -78.66399466736399404, -3.125442558719000008 ) ) ;
#39316 = CARTESIAN_POINT ( 'NONE',  ( 0.8664535991523154568, -79.91447041001134721, 0.9006602674240518080 ) ) ;
#39317 = CARTESIAN_POINT ( 'NONE',  ( -5.539808784079931492, -78.11666666666666003, 9.611650271896815312 ) ) ;
#39318 = CIRCLE ( 'NONE', #24232, 11.65000000000000036 ) ;
#39319 = AXIS2_PLACEMENT_3D ( 'NONE', #3526, #22101, #13244 ) ;
#39320 = CARTESIAN_POINT ( 'NONE',  ( 10.48730647577000141, -77.96533954523499688, -3.808884262352000061 ) ) ;
#39321 = CARTESIAN_POINT ( 'NONE',  ( 11.75000000000000000, -76.95000000000000284, 0.000000000000000000 ) ) ;
#39322 = CARTESIAN_POINT ( 'NONE',  ( 0.000000000000000000, -92.39999999999999147, 0.000000000000000000 ) ) ;
#39323 = VECTOR ( 'NONE', #35810, 1000.000000000000000 ) ;
#39324 = CARTESIAN_POINT ( 'NONE',  ( -1.389164232317718017, -81.88171006759844772, -0.5985393350652561395 ) ) ;
#39325 = EDGE_CURVE ( 'NONE', #51850, #53713, #14997, .T. ) ;
#39326 = CARTESIAN_POINT ( 'NONE',  ( -0.4417226670687336432, -79.69665877900507667, -1.169169109811868612 ) ) ;
#39327 = LINE ( 'NONE', #48772, #6626 ) ;
#39328 = CARTESIAN_POINT ( 'NONE',  ( 1.799490220168999954, -22.77129148951999937, 12.64502302235000109 ) ) ;
#39329 = CARTESIAN_POINT ( 'NONE',  ( 11.75000000000000000, -76.05000000000001137, 0.000000000000000000 ) ) ;
#39330 = ORIENTED_EDGE ( 'NONE', *, *, #9210, .F. ) ;
#39331 = ORIENTED_EDGE ( 'NONE', *, *, #55271, .T. ) ;
#39332 = CYLINDRICAL_SURFACE ( 'NONE', #19226, 1.500000000000000000 ) ;
#39333 = CARTESIAN_POINT ( 'NONE',  ( 9.467323119481999782, -77.38933998579800289, 1.196001045232000015 ) ) ;
#39334 = EDGE_LOOP ( 'NONE', ( #9037, #16828, #24079, #26522 ) ) ;
#39335 = CARTESIAN_POINT ( 'NONE',  ( -5.320285352961153791, -79.67214536383268353, 7.903715897855382089 ) ) ;
#39337 = EDGE_CURVE ( 'NONE', #33152, #8440, #1643, .T. ) ;
#39336 = VERTEX_POINT ( 'NONE', #38817 ) ;
#39338 = CARTESIAN_POINT ( 'NONE',  ( -9.888452460216527129, -81.00000000000000000, -4.376188563388549113 ) ) ;
#39339 = CARTESIAN_POINT ( 'NONE',  ( 10.89235442234000040, -77.32873010171299200, 0.7293703643125000191 ) ) ;
#39340 = CONTEXT_DEPENDENT_SHAPE_REPRESENTATION ( #10028, #42824 ) ;
#39341 = B_SPLINE_CURVE_WITH_KNOTS ( 'NONE', 3,
 ( #10928, #37773, #55794, #15344, #10050, #28909, #9752, #20073, #56084, #18902, #32164, #27738, #37187, #45785, #5320, #41919, #23328, #36894 ),
 .UNSPECIFIED., .F., .F.,
 ( 4, 2, 2, 2, 2, 2, 2, 2, 4 ),
 ( 0.000000000000000000, 0.1249999999999999722, 0.2500000000000000000, 0.3750000000000000000, 0.5000000000000001110, 0.6250000000000001110, 0.7500000000000000000, 0.8750000000000000000, 1.000000000000000000 ),
 .UNSPECIFIED. ) ;
#39342 = CARTESIAN_POINT ( 'NONE',  ( 8.449950666592000559, -78.90086332859900153, -4.961522297560000183 ) ) ;
#39343 = CARTESIAN_POINT ( 'NONE',  ( -1.173906744531483248, -78.21502352218460885, -9.176430860882623719 ) ) ;
#39344 = CARTESIAN_POINT ( 'NONE',  ( 8.733858618705999888, -78.39433925363499611, -7.038306768505999678 ) ) ;
#39345 = ORIENTED_EDGE ( 'NONE', *, *, #51577, .F. ) ;
#39346 = ORIENTED_EDGE ( 'NONE', *, *, #42083, .T. ) ;
#39347 = CARTESIAN_POINT ( 'NONE',  ( -4.496256502423060297, -77.51547528653394181, 8.084058354872142971 ) ) ;
#39348 = DIRECTION ( 'NONE',  ( 1.000000000000000000, 0.000000000000000000, 0.000000000000000000 ) ) ;
#39349 = CARTESIAN_POINT ( 'NONE',  ( 7.648026766735999793, -23.25000000582000226, -10.12290050089000104 ) ) ;
#39350 = AXIS2_PLACEMENT_3D ( 'NONE', #4801, #49387, #9813 ) ;
#39351 = CARTESIAN_POINT ( 'NONE',  ( -12.61117499584999813, -60.01550664522000034, -1.798980867982999943 ) ) ;
#39352 = CARTESIAN_POINT ( 'NONE',  ( 2.867548251969000095, -77.97902275635898661, -9.270807752789000489 ) ) ;
#39353 = CARTESIAN_POINT ( 'NONE',  ( 7.691893942719999266, -21.75453807238000081, 10.42272502862000039 ) ) ;
#39354 = CARTESIAN_POINT ( 'NONE',  ( -9.250000000000000000, -77.49999999999998579, -1.203901273580999948E-14 ) ) ;
#39355 = CARTESIAN_POINT ( 'NONE',  ( 10.10712711931551944, -54.33345760842059491, -7.860996423901147168 ) ) ;
#39356 = CARTESIAN_POINT ( 'NONE',  ( -10.49924843836999955, -80.33887287015198808, -4.054558598941000014 ) ) ;
#39357 = CARTESIAN_POINT ( 'NONE',  ( 12.55485633994999795, -17.84594908780999845, -1.580761757392000089 ) ) ;
#39358 = EDGE_CURVE ( 'NONE', #44782, #49641, #17537, .T. ) ;
#39359 = CARTESIAN_POINT ( 'NONE',  ( -0.7232461515322000656, -82.19001440484599641, -1.097480396689000104 ) ) ;
#39360 = CIRCLE ( 'NONE', #21445, 4.999999999999996447 ) ;
#39361 = ORIENTED_EDGE ( 'NONE', *, *, #32827, .T. ) ;
#39362 = EDGE_CURVE ( 'NONE', #32341, #39914, #54316, .T. ) ;
#39363 = AXIS2_PLACEMENT_3D ( 'NONE', #12002, #11717, #29694 ) ;
#39364 = CARTESIAN_POINT ( 'NONE',  ( -8.790679651930998872, -53.86186536156999694, 8.797972003268000663 ) ) ;
#39365 = CARTESIAN_POINT ( 'NONE',  ( 11.97742283006000186, -77.95327449044499701, 0.2395971301470999903 ) ) ;
#39366 = CARTESIAN_POINT ( 'NONE',  ( -10.15833271782000047, -17.78011549213000109, -7.756208840363000512 ) ) ;
#39368 = CARTESIAN_POINT ( 'NONE',  ( -9.722718241315000398, -60.04999999966999980, -7.954951288349001004 ) ) ;
#39367 = CARTESIAN_POINT ( 'NONE',  ( 5.684123266893727155, -78.42295138177613012, 7.396499574309489233 ) ) ;
#39369 = AXIS2_PLACEMENT_3D ( 'NONE', #18649, #13318, #41367 ) ;
#39370 = DIRECTION ( 'NONE',  ( -0.7071067811865474617, -0.7071067811865474617, 3.205717710189212192E-10 ) ) ;
#39371 = FILL_AREA_STYLE ('',( #43516 ) ) ;
#39372 = DIRECTION ( 'NONE',  ( -0.9999548435846228323, 0.000000000000000000, -0.009503199022040118363 ) ) ;
#39373 = CARTESIAN_POINT ( 'NONE',  ( -10.03906427447999938, -77.36083935769899256, -5.104033018226999729 ) ) ;
#39374 = CARTESIAN_POINT ( 'NONE',  ( -8.027667713925865201, -79.64209375582814232, -4.635885087717896091 ) ) ;
#39375 = CARTESIAN_POINT ( 'NONE',  ( 4.427954972153999691, -80.98098182763799002, -10.19376387942000051 ) ) ;
#39376 = ORIENTED_EDGE ( 'NONE', *, *, #57513, .T. ) ;
#39377 = CARTESIAN_POINT ( 'NONE',  ( 8.779106447692145210, -80.29927823582293911, 6.259569139016127437 ) ) ;
#39378 = DIRECTION ( 'NONE',  ( 0.9999548435846228323, 0.000000000000000000, 0.009503199022040218977 ) ) ;
#39379 = CARTESIAN_POINT ( 'NONE',  ( -12.60413652832999887, -18.69283065396999888, 1.799502287743000029 ) ) ;
#39380 = EDGE_CURVE ( 'NONE', #56557, #378, #6508, .T. ) ;
#39381 = CARTESIAN_POINT ( 'NONE',  ( -2.996400371072000191, -3.165668112399999679, 2.346782378936000057 ) ) ;
#39382 = B_SPLINE_CURVE_WITH_KNOTS ( 'NONE', 3,
 ( #4195, #40203, #4781, #17776, #22783, #19234, #46117, #32205, #37226, #50246, #5360, #55241, #32492, #18944, #9796, #14789, #50830, #50537, #36936, #32784, #10375, #54949, #23653, #27780, #41665, #1244, #45823, #5643, #23367, #41378, #961, #14500, #10092, #28070, #49564, #54283, #44831, #26503, #27394, #23271, #45429, #288, #58405, #27098, #9403, #18267, #45134, #32110, #41277, #4969, #22979, #862, #40988, #8809, #40093, #50440, #36260, #14398, #44527, #40696, #26801, #580, #18847, #54574, #36840, #49257, #9110, #58107, #4386, #50151, #18560, #14114 ),
 .UNSPECIFIED., .F., .F.,
 ( 4, 2, 2, 2, 1, 2, 2, 2, 2, 2, 2, 2, 2, 2, 2, 2, 2, 2, 2, 2, 2, 2, 2, 2, 2, 2, 2, 2, 2, 2, 2, 2, 1, 2, 2, 2, 4 ),
 ( 0.000000000000000000, 0.03125000000000001388, 0.06250000000000002776, 0.07812500000000001388, 0.09375000000000000000, 0.1093749999999999722, 0.1249999999999999722, 0.1562499999999999445, 0.1874999999999999445, 0.2187499999999999167, 0.2499999999999999167, 0.2812499999999998890, 0.3124999999999998890, 0.3437499999999999445, 0.3749999999999999445, 0.4062499999999999445, 0.4374999999999999445, 0.4687499999999999445, 0.4999999999999998890, 0.5312499999999998890, 0.5624999999999998890, 0.5937499999999998890, 0.6249999999999998890, 0.6562500000000000000, 0.6875000000000000000, 0.7187500000000000000, 0.7500000000000000000, 0.7812500000000000000, 0.8125000000000000000, 0.8437500000000000000, 0.8750000000000000000, 0.8906250000000001110, 0.9062500000000001110, 0.9218750000000001110, 0.9375000000000001110, 0.9687500000000001110, 1.000000000000000000 ),
 .UNSPECIFIED. ) ;
#39383 = CARTESIAN_POINT ( 'NONE',  ( 1.621664633118000021, -80.15957412722899278, -9.284183544346999994 ) ) ;
#39384 = CARTESIAN_POINT ( 'NONE',  ( -12.68702648024000190, -55.04922088160000015, 1.889939500033999797 ) ) ;
#39385 = CARTESIAN_POINT ( 'NONE',  ( 9.363982905857531236, -77.19999999999997442, 5.400558314209766841 ) ) ;
#39386 = FACE_OUTER_BOUND ( 'NONE', #50968, .T. ) ;
#39387 = CARTESIAN_POINT ( 'NONE',  ( 0.000000000000000000, -80.49999999999998579, -10.69999999999999929 ) ) ;
#39388 = CARTESIAN_POINT ( 'NONE',  ( -1.735035607296000038, -85.15982450217398991, -3.748086837743999755 ) ) ;
#39389 = DIRECTION ( 'NONE',  ( 0.000000000000000000, 0.000000000000000000, 1.000000000000000000 ) ) ;
#39390 = CARTESIAN_POINT ( 'NONE',  ( -8.485281374238999419, -60.04999999966999980, -8.485281374238999419 ) ) ;
#39391 = B_SPLINE_SURFACE_WITH_KNOTS ( 'NONE', 3, 3, ( 
 ( #8474, #44493, #49525, #18810, #28522, #6095, #9954, #41238, #10838, #37090, #24104, #32648, #1690, #19682, #46571, #42124, #55401, #36801, #10539, #15246, #543, #54819, #55108, #23233, #829, #14078, #18519, #19393, #10243, #32946, #36512, #50700, #1114, #37682, #55698 ),
 ( #54537, #32362, #27935, #32072, #37385, #23520, #33240, #14361, #50113, #51284, #45688, #28814, #46862, #6390, #45984, #24405, #9658, #27647, #5228, #50404, #14653, #5510, #41531, #14948, #19099, #28223, #46277, #5803, #23809, #41825, #1399, #50988, #51575, #43572, #20269 ),
 ( #20836, #11132, #3135, #34401, #29970, #29681, #34106, #25267, #38554, #38842, #56569, #47156, #29396, #48021, #52720, #12272, #39132, #15541, #24976, #6686, #7839, #24694, #38262, #19983, #16708, #56859, #21126, #30261, #52148, #57143, #48301, #16419, #34690, #7555, #33822 ),
 ( #11992, #37970, #42999, #56285, #25553, #51862, #47446, #42420, #52432, #11706, #2556, #20557, #6974, #16129, #47731, #1989, #55995, #42705, #33538, #29110, #43286, #2272, #7266, #15835, #11415, #2840, #43869, #49465, #26133, #4583, #54180, #18167, #13126, #30839, #12838 ) ),
 .UNSPECIFIED., .F., .F., .F.,
 ( 4, 4 ),
 ( 4, 1, 1, 1, 1, 1, 1, 1, 1, 1, 1, 1, 1, 1, 1, 1, 1, 1, 1, 1, 1, 1, 1, 1, 1, 1, 1, 1, 1, 1, 1, 1, 4 ),
 ( -0.5168282991433000850, 1.516828299142999992 ),
 ( -0.009208997693793000497, 0.005755623558620999794, 0.02072024481102999888, 0.03568486606345000478, 0.05064948731585999786, 0.06561410856827000482, 0.08057872982069000378, 0.09554335107309999686, 0.1105079723255000118, 0.1254725935778999990, 0.1404372148303000001, 0.1554018360827999767, 0.1703664573352000056, 0.1853310785876000066, 0.2002956998400000077, 0.2152603210924000088, 0.2302249423447999821, 0.2451895635972000109, 0.2601541848496000120, 0.2751188061020999887, 0.2900834273544999897, 0.3050480486068999908, 0.3200126698593000474, 0.3349772911116999929, 0.3499419123640999940, 0.3649065336164999951, 0.3798711548689999717, 0.3948357761214000283, 0.4098003973737999739, 0.4247650186261999750, 0.4397296398786000315, 0.4546942611309999771, 0.4696588823833999782 ),
 .UNSPECIFIED. ) ;
#39392 = CARTESIAN_POINT ( 'NONE',  ( -10.00926467875000014, -76.60660321907299419, 4.638537167971000130 ) ) ;
#39393 = CARTESIAN_POINT ( 'NONE',  ( -0.01871105017136468623, -81.97680572310699176, 1.249633071440004350 ) ) ;
#39394 = CARTESIAN_POINT ( 'NONE',  ( 10.18496935386999880, -57.04935285362000030, 7.710095619715000126 ) ) ;
#39395 = CARTESIAN_POINT ( 'NONE',  ( 6.479078291783999966, -79.25424805011499529, -7.022474634662000170 ) ) ;
#39396 = CARTESIAN_POINT ( 'NONE',  ( 9.611650271896820641, -77.39166666666666572, 5.539808784079911952 ) ) ;
#39397 = CARTESIAN_POINT ( 'NONE',  ( -5.625515643987146319, -80.18124105601512497, -9.161514280032365676 ) ) ;
#39398 = DIRECTION ( 'NONE',  ( 0.000000000000000000, 0.000000000000000000, -1.000000000000000000 ) ) ;
#39399 = CARTESIAN_POINT ( 'NONE',  ( 7.910459948463299362, -79.66262039076877954, 7.952749987741428939 ) ) ;
#39400 = CIRCLE ( 'NONE', #29034, 5.000000000000000888 ) ;
#39401 = CARTESIAN_POINT ( 'NONE',  ( 11.92746894621999942, -79.25868537235298561, 1.562891678063999867 ) ) ;
#39402 = CARTESIAN_POINT ( 'NONE',  ( 0.000000000000000000, -77.50000000000000000, 0.000000000000000000 ) ) ;
#39403 = DIRECTION ( 'NONE',  ( 0.000000000000000000, 1.000000000000000000, 0.000000000000000000 ) ) ;
#39404 = VECTOR ( 'NONE', #2106, 1000.000000000000000 ) ;
#39405 = CARTESIAN_POINT ( 'NONE',  ( 4.100000000000000533, -78.69999999999998863, 0.000000000000000000 ) ) ;
#39406 = EDGE_LOOP ( 'NONE', ( #32487, #56149, #11111, #49688 ) ) ;
#39407 = CARTESIAN_POINT ( 'NONE',  ( 7.836764916109974166, -61.10511429613130474, 9.850487231183253201 ) ) ;
#39408 = ORIENTED_EDGE ( 'NONE', *, *, #43404, .F. ) ;
#39409 = FILL_AREA_STYLE_COLOUR ( '', #5693 ) ;
#39411 = EDGE_CURVE ( 'NONE', #23438, #30600, #52540, .T. ) ;
#39410 = ORIENTED_EDGE ( 'NONE', *, *, #17071, .F. ) ;
#39412 = CARTESIAN_POINT ( 'NONE',  ( -3.250000000000002665, -1.489583333333333703, 0.4254240051736044581 ) ) ;
#39413 = AXIS2_PLACEMENT_3D ( 'NONE', #58050, #17031, #52471 ) ;
#39414 = CARTESIAN_POINT ( 'NONE',  ( -1.500000000000000888, -78.48958333333331439, 0.1963495408493559080 ) ) ;
#39415 = CARTESIAN_POINT ( 'NONE',  ( -2.658242603751999944, -81.86019317200199907, -2.348470574630999952 ) ) ;
#39416 = CARTESIAN_POINT ( 'NONE',  ( -1.025492391311069618, -79.28331459140689219, 9.446644090482800848 ) ) ;
#39417 = VERTEX_POINT ( 'NONE', #25376 ) ;
#39418 = CARTESIAN_POINT ( 'NONE',  ( 7.975755774848001245, -79.32330787033001229, 9.089596497509001338 ) ) ;
#39419 = B_SPLINE_CURVE_WITH_KNOTS ( 'NONE', 3,
 ( #14915, #29079, #1658, #19072, #11099, #33791 ),
 .UNSPECIFIED., .F., .F.,
 ( 4, 2, 4 ),
 ( 0.000000000000000000, 0.5000000000000000000, 1.000000000000000000 ),
 .UNSPECIFIED. ) ;
#39420 = ORIENTED_EDGE ( 'NONE', *, *, #45014, .T. ) ;
#39421 = DIRECTION ( 'NONE',  ( 0.7071067811865474617, 0.000000000000000000, 0.7071067811865474617 ) ) ;
#39422 = CARTESIAN_POINT ( 'NONE',  ( 1.500000000000000000, -79.14999999999999147, 0.000000000000000000 ) ) ;
#39423 = CARTESIAN_POINT ( 'NONE',  ( 0.000000000000000000, -80.69999999999998863, 0.000000000000000000 ) ) ;
#39424 = CARTESIAN_POINT ( 'NONE',  ( -6.937102608493817435, -80.03119389196088207, 8.211835529152839541 ) ) ;
#39425 = CARTESIAN_POINT ( 'NONE',  ( -9.312499999988999022, -77.13750000001088836, -2.050180145195999796E-09 ) ) ;
#39426 = CARTESIAN_POINT ( 'NONE',  ( -7.707166124622999881, -77.30197135713177659, -5.896629607976000109 ) ) ;
#39427 = CARTESIAN_POINT ( 'NONE',  ( 3.284677190815898484, -85.82402986354867380, 1.430105188728104881 ) ) ;
#39428 = CARTESIAN_POINT ( 'NONE',  ( 9.505949683906999681, -79.00000000000000000, 6.906476714433999575 ) ) ;
#39429 = CARTESIAN_POINT ( 'NONE',  ( -0.3439666625990999704, -79.97550662411998701, 1.306773950318999900 ) ) ;
#39430 = CARTESIAN_POINT ( 'NONE',  ( 5.402466744453000125, -76.15846601409100458, 9.843631583929999707 ) ) ;
#39431 = CARTESIAN_POINT ( 'NONE',  ( -1.250000000000000000, -82.49999999999998579, 0.000000000000000000 ) ) ;
#39432 = EDGE_CURVE ( 'NONE', #46115, #1066, #20953, .T. ) ;
#39433 = CARTESIAN_POINT ( 'NONE',  ( -1.139762735568999874, -81.58007094306199747, 3.969817958149999715 ) ) ;
#39434 = CARTESIAN_POINT ( 'NONE',  ( -10.29678529194292658, -80.12898668796422896, -3.869235002584780148 ) ) ;
#39435 = CARTESIAN_POINT ( 'NONE',  ( -1.258617623430583476, -3.007881555714398303, 2.995588677545779621 ) ) ;
#39436 = CARTESIAN_POINT ( 'NONE',  ( 2.970753672374999876, -79.60055496681158616, 1.938087954564000182 ) ) ;
#39437 = AXIS2_PLACEMENT_3D ( 'NONE', #8663, #3655, #17822 ) ;
#39438 = LINE ( 'NONE', #34413, #6372 ) ;
#39439 = CARTESIAN_POINT ( 'NONE',  ( 3.546563745408000123, -82.43369503318800184, -0.05579941425955000506 ) ) ;
#39440 = CARTESIAN_POINT ( 'NONE',  ( 3.521688171515000132, -3.583255539711999837, 0.7298424208991000084 ) ) ;
#39441 = CARTESIAN_POINT ( 'NONE',  ( -0.1647852606798474728, -79.86509396069870093, -1.263697374764313874 ) ) ;
#39442 = CARTESIAN_POINT ( 'NONE',  ( 9.393203674808258796, -80.20833333333331439, -5.413904038987190859 ) ) ;
#39443 = CARTESIAN_POINT ( 'NONE',  ( 5.838193839761669501, -78.22291666666666288, 7.596835002782726498 ) ) ;
#39444 = ADVANCED_FACE ( 'NONE', ( #51976 ), #36043, .T. ) ;
#39445 = CARTESIAN_POINT ( 'NONE',  ( -0.9200108141794000050, -81.74253175281400274, -0.9654823929056000065 ) ) ;
#39447 = EDGE_CURVE ( 'NONE', #47646, #11409, #16980, .T. ) ;
#39446 = CARTESIAN_POINT ( 'NONE',  ( -12.43646312222999839, -17.07951485557000026, -0.1257251053153000120 ) ) ;
#39448 = CARTESIAN_POINT ( 'NONE',  ( 12.61277705613999878, -23.19666672528000007, 1.798399175679999740 ) ) ;
#39449 = DIRECTION ( 'NONE',  ( -1.000000000000000000, 0.000000000000000000, 0.000000000000000000 ) ) ;
#39450 = AXIS2_PLACEMENT_3D ( 'NONE', #22654, #9663, #3554 ) ;
#39451 = CARTESIAN_POINT ( 'NONE',  ( 1.980610890452888295, -23.52073889484903546, -12.74374574606960486 ) ) ;
#39452 = CARTESIAN_POINT ( 'NONE',  ( -12.17235636505000151, -76.59542353800999592, -2.158157603104000177 ) ) ;
#39453 = EDGE_LOOP ( 'NONE', ( #35840, #4930, #18514, #46837 ) ) ;
#39454 = DIRECTION ( 'NONE',  ( -1.000000000000000000, 0.000000000000000000, 0.000000000000000000 ) ) ;
#39455 = CARTESIAN_POINT ( 'NONE',  ( 3.576074390006000137, -85.88547955769999476, -1.592170899227999925 ) ) ;
#39456 = CARTESIAN_POINT ( 'NONE',  ( 12.66008999775999833, -61.42705329315000284, 1.387101471715999956 ) ) ;
#39457 = CARTESIAN_POINT ( 'NONE',  ( -1.931043742978000077, -22.77795407709999864, -12.75763395695999947 ) ) ;
#39458 = CARTESIAN_POINT ( 'NONE',  ( -8.614692902062000002, -77.35976152403699757, 3.831263898871999807 ) ) ;
#39459 = CARTESIAN_POINT ( 'NONE',  ( -3.892240088685000377, -83.30055803339699594, -1.503509056668000055 ) ) ;
#39460 = CARTESIAN_POINT ( 'NONE',  ( -2.184012626508494481, -79.99174196189673580, 10.52796603406774700 ) ) ;
#39461 = CARTESIAN_POINT ( 'NONE',  ( -0.1806087918925000091, -80.48785071125600155, 1.406216040666999900 ) ) ;
#39462 = VERTEX_POINT ( 'NONE', #43974 ) ;
#39463 = CARTESIAN_POINT ( 'NONE',  ( 9.500000000000000000, -77.04999999999999716, 0.000000000000000000 ) ) ;
#39464 = CARTESIAN_POINT ( 'NONE',  ( 8.931020339874743641, -78.87206237794539732, 2.484699444477077357 ) ) ;
#39465 = EDGE_CURVE ( 'NONE', #46183, #43155, #35086, .T. ) ;
#39466 = CARTESIAN_POINT ( 'NONE',  ( 3.407095545933000569, -78.77851879815550262, -4.172488654716052899E-16 ) ) ;
#39467 = EDGE_LOOP ( 'NONE', ( #46845, #44703, #45893, #39044 ) ) ;
#39468 = CARTESIAN_POINT ( 'NONE',  ( -10.87240354821999944, -78.87967694811598562, -1.216000584195999767 ) ) ;
#39469 = CARTESIAN_POINT ( 'NONE',  ( 12.60413670417000098, -55.49283319101999723, 1.799502287691000069 ) ) ;
#39470 = CARTESIAN_POINT ( 'NONE',  ( -1.750000000001000089, -55.54999998977000075, 12.56594317853999954 ) ) ;
#39471 = ORIENTED_EDGE ( 'NONE', *, *, #55726, .T. ) ;
#39472 = ORIENTED_EDGE ( 'NONE', *, *, #45514, .F. ) ;
#39474 = EDGE_CURVE ( 'NONE', #43629, #22264, #48981, .T. ) ;
#39473 = ORIENTED_EDGE ( 'NONE', *, *, #4869, .F. ) ;
#39475 = CARTESIAN_POINT ( 'NONE',  ( 1.149310424350558080, -80.38227707828973223, 0.4913328182984957326 ) ) ;
#39476 = ADVANCED_FACE ( 'NONE', ( #3524 ), #35675, .F. ) ;
#39477 = DIRECTION ( 'NONE',  ( 0.7071067811865474617, 0.000000000000000000, -0.7071067811865474617 ) ) ;
#39478 = CARTESIAN_POINT ( 'NONE',  ( 8.414570695956999913, -60.64999999943950826, -8.414570695956999913 ) ) ;
#39479 = ORIENTED_EDGE ( 'NONE', *, *, #12618, .F. ) ;
#39480 = CARTESIAN_POINT ( 'NONE',  ( 0.000000000000000000, -74.64999999999999147, 0.000000000000000000 ) ) ;
#39482 = ORIENTED_EDGE ( 'NONE', *, *, #41797, .T. ) ;
#39481 = B_SPLINE_CURVE_WITH_KNOTS ( 'NONE', 3,
 ( #25104, #43704, #16258, #25963, #34523, #12396, #51991, #2688, #48145, #7676, #25677, #7388, #3260, #39255, #38392, #43987, #20681, #39547 ),
 .UNSPECIFIED., .F., .F.,
 ( 4, 2, 2, 2, 2, 2, 2, 2, 4 ),
 ( 0.000000000000000000, 0.1250000000000000278, 0.2500000000000000000, 0.3750000000000001110, 0.5000000000000001110, 0.6250000000000001110, 0.7500000000000002220, 0.8750000000000001110, 1.000000000000000000 ),
 .UNSPECIFIED. ) ;
#39483 = CARTESIAN_POINT ( 'NONE',  ( -0.9446365838440466955, -79.20834522158486379, -0.8548086173491427076 ) ) ;
#39484 = CARTESIAN_POINT ( 'NONE',  ( 3.851650068367000301, -78.96264283715740362, -2.273141396972203854 ) ) ;
#39485 = CARTESIAN_POINT ( 'NONE',  ( 7.633502222218000455, -55.59895684611999656, 10.36289759015999934 ) ) ;
#39486 = CIRCLE ( 'NONE', #37597, 5.000000000000000000 ) ;
#39487 = FACE_OUTER_BOUND ( 'NONE', #21327, .T. ) ;
#39488 = CARTESIAN_POINT ( 'NONE',  ( -5.751575620263249533, -79.64192708332932114, 7.482738016046601714 ) ) ;
#39489 = CARTESIAN_POINT ( 'NONE',  ( 12.70228545259539032, -61.62820680322044353, -1.205254117609577236 ) ) ;
#39490 = CARTESIAN_POINT ( 'NONE',  ( -1.508524907456192610, -77.84776514064024866, 0.03467181534751852950 ) ) ;
#39491 = CARTESIAN_POINT ( 'NONE',  ( 8.700421281190083178, -78.82251712223430218, -3.142473759474660344 ) ) ;
#39492 = CARTESIAN_POINT ( 'NONE',  ( -10.01676948373000009, -23.20938276584000093, 7.658894993369000481 ) ) ;
#39493 = CARTESIAN_POINT ( 'NONE',  ( 2.775698051716999792, -81.16380496681199475, 3.115375198333000473 ) ) ;
#39494 = CARTESIAN_POINT ( 'NONE',  ( -8.458823954585000138, -77.29848667140100815, -4.874260255650000317 ) ) ;
#39495 = CARTESIAN_POINT ( 'NONE',  ( -12.66008925484999992, -17.37289997915000228, 1.387046028394999908 ) ) ;
#39496 = DIRECTION ( 'NONE',  ( 0.7071067811865475727, 0.000000000000000000, 0.7071067811865475727 ) ) ;
#39497 = CARTESIAN_POINT ( 'NONE',  ( -10.51110168222999874, -75.95506250004599735, 6.351495789100000344 ) ) ;
#39498 = LINE ( 'NONE', #25915, #54372 ) ;
#39499 = CARTESIAN_POINT ( 'NONE',  ( -1.214170062781000148, -1.395588905189000029, -3.939698975434999362 ) ) ;
#39500 = CARTESIAN_POINT ( 'NONE',  ( -1.249999999999999778, -78.51041666666664298, -0.1636246173744686228 ) ) ;
#39501 = CARTESIAN_POINT ( 'NONE',  ( -1.177869840716120997, -80.29261637651916317, 1.006895591056990558 ) ) ;
#39502 = CARTESIAN_POINT ( 'NONE',  ( -9.376541175504000236, -77.45795096818498848, -0.1234390441450999854 ) ) ;
#39503 = CARTESIAN_POINT ( 'NONE',  ( 1.980464439859999981, -57.04527982639000072, -12.85144117157999943 ) ) ;
#39504 = CARTESIAN_POINT ( 'NONE',  ( 1.460959015002474048, -78.72916666666665719, -0.3926218265389178064 ) ) ;
#39505 = CARTESIAN_POINT ( 'NONE',  ( -3.515269593969000184, -2.480847686686999953, -0.5480397081700000284 ) ) ;
#39506 = CARTESIAN_POINT ( 'NONE',  ( -9.933360547807000174, -77.92342353357300055, -7.219704108085999827 ) ) ;
#39507 = CARTESIAN_POINT ( 'NONE',  ( 0.000000000000000000, -77.04999999999999716, 0.000000000000000000 ) ) ;
#39508 = AXIS2_PLACEMENT_3D ( 'NONE', #20224, #39084, #24929 ) ;
#39510 = CYLINDRICAL_SURFACE ( 'NONE', #25943, 1.000000000000000000 ) ;
#39509 = DIRECTION ( 'NONE',  ( 0.000000000000000000, 0.000000000000000000, 1.000000000000000000 ) ) ;
#39511 = CARTESIAN_POINT ( 'NONE',  ( -1.186490757027999887, -81.09779729262000103, -0.2694786029208000033 ) ) ;
#39512 = CARTESIAN_POINT ( 'NONE',  ( -7.601746409728754372, -79.53766441201359783, 7.600897104933312498 ) ) ;
#39513 = VERTEX_POINT ( 'NONE', #26240 ) ;
#39514 = CARTESIAN_POINT ( 'NONE',  ( -1.416666666666666741, -83.20000000000000284, 0.000000000000000000 ) ) ;
#39515 = CARTESIAN_POINT ( 'NONE',  ( 0.2413473483368999972, -79.63228351955899598, 12.15388238791999953 ) ) ;
#39516 = CARTESIAN_POINT ( 'NONE',  ( 3.573639641522492028, -79.09450849937717010, 8.866719865068596107 ) ) ;
#39517 = DIRECTION ( 'NONE',  ( 0.000000000000000000, 1.000000000000000000, 0.000000000000000000 ) ) ;
#39518 = CARTESIAN_POINT ( 'NONE',  ( 1.439896632895286466, -78.96458333333333712, 11.00000000000000711 ) ) ;
#39519 = CARTESIAN_POINT ( 'NONE',  ( 0.008649596124003998757, -1.093362276482000128, 3.863893329571999935 ) ) ;
#39520 = CARTESIAN_POINT ( 'NONE',  ( -5.407072851296999438, -80.19379678548699530, 7.853270924851000423 ) ) ;
#39521 = CARTESIAN_POINT ( 'NONE',  ( 12.66736977981000045, -24.23307288772000234, -1.690635117038000068 ) ) ;
#39522 = CARTESIAN_POINT ( 'NONE',  ( -12.00000000000000000, -55.54999999966999980, 0.000000000000000000 ) ) ;
#39523 = ORIENTED_EDGE ( 'NONE', *, *, #39073, .F. ) ;
#39524 = CARTESIAN_POINT ( 'NONE',  ( -12.71162569430491551, -54.56025712730872357, 1.720540999418351369 ) ) ;
#39525 = AXIS2_PLACEMENT_3D ( 'NONE', #56844, #26113, #34673 ) ;
#39526 = CARTESIAN_POINT ( 'NONE',  ( -7.678106106111999729, -79.80848667140099906, -5.817855318239999463 ) ) ;
#39527 = EDGE_CURVE ( 'NONE', #6877, #14569, #2143, .T. ) ;
#39528 = FACE_OUTER_BOUND ( 'NONE', #47278, .T. ) ;
#39529 = CARTESIAN_POINT ( 'NONE',  ( -10.18589226629999978, -55.51082276539999327, -7.641012305206999145 ) ) ;
#39530 = ADVANCED_FACE ( 'NONE', ( #39814 ), #43596, .F. ) ;
#39531 = CARTESIAN_POINT ( 'NONE',  ( 3.437861145763999815, -83.99067953870898862, 0.8750219220807000653 ) ) ;
#39532 = ORIENTED_EDGE ( 'NONE', *, *, #43576, .F. ) ;
#39533 = CARTESIAN_POINT ( 'NONE',  ( -12.52785477533552516, -55.00586572896404647, 1.668513102962560835 ) ) ;
#39534 = CARTESIAN_POINT ( 'NONE',  ( 9.431008682120035402, -61.60059307736660372, -8.251849285864723882 ) ) ;
#39535 = DIRECTION ( 'NONE',  ( 1.000000000000000000, 0.000000000000000000, 0.000000000000000000 ) ) ;
#39536 = CARTESIAN_POINT ( 'NONE',  ( -7.986982684638000762, -54.07364722701999682, -10.07612755991999975 ) ) ;
#39537 = EDGE_CURVE ( 'NONE', #46988, #36429, #40110, .T. ) ;
#39538 = CARTESIAN_POINT ( 'NONE',  ( -0.5483576180056000116, -79.45068147198898600, -9.751923335751000010 ) ) ;
#39539 = ORIENTED_EDGE ( 'NONE', *, *, #48016, .T. ) ;
#39540 = VERTEX_POINT ( 'NONE', #17386 ) ;
#39541 = CARTESIAN_POINT ( 'NONE',  ( 11.20283039713999962, -76.47574370419398804, 5.204271411707000361 ) ) ;
#39542 = CARTESIAN_POINT ( 'NONE',  ( -8.098901191184470605, -78.65749706134158714, -7.103902919008961092 ) ) ;
#39543 = CARTESIAN_POINT ( 'NONE',  ( -1.329574456303999952, -77.62855326413999535, 0.2546955586738999799 ) ) ;
#39544 = VERTEX_POINT ( 'NONE', #58123 ) ;
#39545 = B_SPLINE_CURVE_WITH_KNOTS ( 'NONE', 3,
 ( #14856, #6300, #32851, #15153 ),
 .UNSPECIFIED., .F., .F.,
 ( 4, 4 ),
 ( 0.000000000000000000, 1.000000000000000000 ),
 .UNSPECIFIED. ) ;
#39546 = CARTESIAN_POINT ( 'NONE',  ( -1.269916711065999904, -77.30448084965399858, -9.409822520238998678 ) ) ;
#39547 = CARTESIAN_POINT ( 'NONE',  ( 11.00000000000000000, -77.44999999999998863, 0.000000000000000000 ) ) ;
#39548 = CARTESIAN_POINT ( 'NONE',  ( -1.538071403319991814, -75.91458333333332575, -11.75000000000000355 ) ) ;
#39549 = CARTESIAN_POINT ( 'NONE',  ( -7.818192365797999699, -78.68694664278000062, 9.061685001942999307 ) ) ;
#39550 = CARTESIAN_POINT ( 'NONE',  ( -3.633103876187999681, -77.15124862347786916, 10.61219425078000000 ) ) ;
#39551 = CARTESIAN_POINT ( 'NONE',  ( -12.76303204525000012, -60.06485147653999945, -1.980584515753000208 ) ) ;
#39552 = CARTESIAN_POINT ( 'NONE',  ( -3.407883501310938978, -86.40321104920799655, 1.440947618426480670 ) ) ;
#39553 = CARTESIAN_POINT ( 'NONE',  ( -2.848564863371000122, -79.00625005849099125, -10.84913769893999991 ) ) ;
#39554 = ADVANCED_FACE ( 'NONE', ( #53706 ), #7661, .T. ) ;
#39555 = CARTESIAN_POINT ( 'NONE',  ( 3.434537346384257006, -79.94481355672635914, 8.588818010512337509 ) ) ;
#39556 = CARTESIAN_POINT ( 'NONE',  ( 8.274781782206300562, -17.02110650128472358, 9.689260013783508541 ) ) ;
#39557 = EDGE_LOOP ( 'NONE', ( #31585, #23577, #49049 ) ) ;
#39558 = CARTESIAN_POINT ( 'NONE',  ( -11.07910306079999962, -79.63533932610398836, -2.045094064781999954 ) ) ;
#39559 = CARTESIAN_POINT ( 'NONE',  ( 4.243585900913456221, -77.26294495438891374, -8.219156677414845902 ) ) ;
#39560 = CARTESIAN_POINT ( 'NONE',  ( -1.227075629532000001, -79.83906442605000109, -0.7101723588523999320 ) ) ;
#39561 = CARTESIAN_POINT ( 'NONE',  ( 7.601397897754999633, -23.24999999688999708, 10.07627163191000008 ) ) ;
#39562 = VECTOR ( 'NONE', #51181, 1000.000000000000000 ) ;
#39563 = CARTESIAN_POINT ( 'NONE',  ( 11.74981453461694869, -76.45368481813011385, 0.5897208236573105999 ) ) ;
#39564 = CARTESIAN_POINT ( 'NONE',  ( 1.618935784732136174, -60.72751168617237028, -12.52134385804463967 ) ) ;
#39565 = CARTESIAN_POINT ( 'NONE',  ( 3.520524516624752298, -3.098549438791605048, -0.03236223760434995406 ) ) ;
#39566 = AXIS2_PLACEMENT_3D ( 'NONE', #41881, #50463, #18867 ) ;
#39567 = DIRECTION ( 'NONE',  ( 0.000000000000000000, -1.000000000000000000, 0.000000000000000000 ) ) ;
#39568 = CARTESIAN_POINT ( 'NONE',  ( 4.823394776896443581, -78.11073669759603888, -11.06826222629441148 ) ) ;
#39569 = CARTESIAN_POINT ( 'NONE',  ( -7.601397897754999633, -60.04999999725999515, 10.07627163191000008 ) ) ;
#39570 = CARTESIAN_POINT ( 'NONE',  ( -4.428614322242999890, -79.90088080519498703, 10.12250943391000035 ) ) ;
#39571 = CARTESIAN_POINT ( 'NONE',  ( 10.35747158362999976, -18.68415522710999710, -7.626500902215000544 ) ) ;
#39572 = CARTESIAN_POINT ( 'NONE',  ( -0.9269137457058925778, -83.04216970360333505, 0.8380920112027951951 ) ) ;
#39573 = CARTESIAN_POINT ( 'NONE',  ( 4.047001421017999867, -82.42136181958099428, -0.2667492537523999951 ) ) ;
#39574 = FACE_OUTER_BOUND ( 'NONE', #15277, .T. ) ;
#39575 = VERTEX_POINT ( 'NONE', #53117 ) ;
#39576 = CARTESIAN_POINT ( 'NONE',  ( -7.667248634474823632, -77.19999999999998863, 7.744282795875710335 ) ) ;
#39577 = CARTESIAN_POINT ( 'NONE',  ( 0.2491193812340000147, -79.53091273156999819, -1.565693046525999943 ) ) ;
#39578 = CARTESIAN_POINT ( 'NONE',  ( 9.250000000000000000, -79.25028042812365925, 0.03259666451019458538 ) ) ;
#39579 = CARTESIAN_POINT ( 'NONE',  ( 10.18066396183999878, -78.29249513909199720, 6.314281093748000728 ) ) ;
#39580 = LINE ( 'NONE', #48179, #14612 ) ;
#39581 = CARTESIAN_POINT ( 'NONE',  ( -0.7572724432162000197, -83.18294061714399845, 1.483977110291999857 ) ) ;
#39582 = CARTESIAN_POINT ( 'NONE',  ( -10.57592698605000159, -78.61493240443898856, -5.530395178621999364 ) ) ;
#39583 = CARTESIAN_POINT ( 'NONE',  ( -0.8481231068849000021, -79.01200194988500414, 9.686304223355000076 ) ) ;
#39584 = CARTESIAN_POINT ( 'NONE',  ( 2.243017272178000177, -78.85064318342999456, -9.366006557871001448 ) ) ;
#39585 = CARTESIAN_POINT ( 'NONE',  ( 1.460729357743000056, -54.70908756765000192, -12.44211643236999976 ) ) ;
#39586 = CARTESIAN_POINT ( 'NONE',  ( 7.374560639698993114, -78.47708333333332575, -9.596002108778149520 ) ) ;
#39587 = CARTESIAN_POINT ( 'NONE',  ( -0.5731199659192217633, -86.07389998728977787, 4.609165628485452970 ) ) ;
#39588 = ORIENTED_EDGE ( 'NONE', *, *, #20521, .F. ) ;
#39589 = CARTESIAN_POINT ( 'NONE',  ( 0.5999999998848000171, -18.85000000520999919, -11.79999999988000070 ) ) ;
#39590 = CARTESIAN_POINT ( 'NONE',  ( -0.8522511841608177985, -2.205572306515419800, -3.165809400549076891 ) ) ;
#39591 = LINE ( 'NONE', #21011, #40014 ) ;
#39592 = CARTESIAN_POINT ( 'NONE',  ( 12.50000000000000000, -26.93717104351999936, 0.000000000000000000 ) ) ;
#39593 = CARTESIAN_POINT ( 'NONE',  ( 0.6062141276560999437, -82.48424635968999041, -1.551696954864999922 ) ) ;
#39594 = CARTESIAN_POINT ( 'NONE',  ( 2.854969924326999919, -78.18841452101000300, 10.84745395576000071 ) ) ;
#39595 = CARTESIAN_POINT ( 'NONE',  ( -10.13785388426000011, -78.46144477612099877, -4.205702700205000255 ) ) ;
#39596 = CARTESIAN_POINT ( 'NONE',  ( 0.6484536763431314466, -16.87597017290114820, 12.70397497891879190 ) ) ;
#39597 = CARTESIAN_POINT ( 'NONE',  ( 11.48358316434000059, -76.28750529199700736, 4.321443532648999941 ) ) ;
#39598 = DIRECTION ( 'NONE',  ( 0.000000000000000000, 1.000000000000000000, 0.000000000000000000 ) ) ;
#39599 = CARTESIAN_POINT ( 'NONE',  ( -4.100000000000000533, -81.79999999999998295, 0.000000000000000000 ) ) ;
#39600 = ORIENTED_EDGE ( 'NONE', *, *, #27194, .F. ) ;
#39601 = CARTESIAN_POINT ( 'NONE',  ( 6.766101950298000212, -78.96359444038398578, 8.713300108436000002 ) ) ;
#39602 = CARTESIAN_POINT ( 'NONE',  ( 0.3635088733166961794, -79.95197095518092567, 1.195828664671276576 ) ) ;
#39603 = CARTESIAN_POINT ( 'NONE',  ( 11.00000000000000355, -77.83958333333332291, -1.439896632895299566 ) ) ;
#39604 = CARTESIAN_POINT ( 'NONE',  ( -9.242272388666000538, -78.69574075788399625, 6.250760013846000440 ) ) ;
#39605 = LINE ( 'NONE', #44917, #31673 ) ;
#39606 = CYLINDRICAL_SURFACE ( 'NONE', #33155, 5.100000000000000533 ) ;
#39607 = LINE ( 'NONE', #31608, #23312 ) ;
#39608 = CARTESIAN_POINT ( 'NONE',  ( 10.66387363228065155, -76.91183802276627546, -5.042381349153009396 ) ) ;
#39609 = AXIS2_PLACEMENT_3D ( 'NONE', #17253, #35242, #8994 ) ;
#39610 = AXIS2_PLACEMENT_3D ( 'NONE', #49446, #40580, #52768 ) ;
#39611 = CARTESIAN_POINT ( 'NONE',  ( -5.413904038987206846, -79.41666666666665719, 9.393203674808249914 ) ) ;
#39612 = CARTESIAN_POINT ( 'NONE',  ( -12.71162862753614675, -61.03964265594247962, -1.720599174840216516 ) ) ;
#39613 = ADVANCED_FACE ( 'NONE', ( #57829 ), #26818, .F. ) ;
#39614 = DIRECTION ( 'NONE',  ( 0.000000000000000000, 1.000000000000000000, 0.000000000000000000 ) ) ;
#39615 = ORIENTED_EDGE ( 'NONE', *, *, #5230, .T. ) ;
#39616 = ORIENTED_EDGE ( 'NONE', *, *, #9082, .T. ) ;
#39617 = CARTESIAN_POINT ( 'NONE',  ( 10.54482503192156173, -78.83451348532614134, -2.089947448372381000 ) ) ;
#39618 = ORIENTED_EDGE ( 'NONE', *, *, #7759, .F. ) ;
#39619 = CARTESIAN_POINT ( 'NONE',  ( 7.345645686283435616, -79.55621302496926717, 6.245313084360852862 ) ) ;
#39620 = ORIENTED_EDGE ( 'NONE', *, *, #2276, .F. ) ;
#39621 = CARTESIAN_POINT ( 'NONE',  ( -9.369164850722000892, -18.75000000000000000, 7.601397897754999633 ) ) ;
#39622 = CARTESIAN_POINT ( 'NONE',  ( 7.007185918478000097, -76.89294861368399836, 8.371063940391000102 ) ) ;
#39623 = CARTESIAN_POINT ( 'NONE',  ( -7.575359187103000380, -78.57578998579799645, 6.037810896484000267 ) ) ;
#39624 = CARTESIAN_POINT ( 'NONE',  ( -7.666962656759157113, -78.14788324491564708, -5.230267631833246611 ) ) ;
#39625 = CARTESIAN_POINT ( 'NONE',  ( -1.472820794058999905, -78.31263022462898959, -10.90095403661999995 ) ) ;
#39626 = ADVANCED_FACE ( 'NONE', ( #40412 ), #37321, .F. ) ;
#39627 = ORIENTED_EDGE ( 'NONE', *, *, #44691, .T. ) ;
#39628 =( GEOMETRIC_REPRESENTATION_CONTEXT ( 3 ) GLOBAL_UNCERTAINTY_ASSIGNED_CONTEXT ( ( #38406 ) ) GLOBAL_UNIT_ASSIGNED_CONTEXT ( ( #19998, #51875, #16142 ) ) REPRESENTATION_CONTEXT ( 'NONE', 'WORKASPACE' ) );
#39629 = EDGE_LOOP ( 'NONE', ( #11396, #2332, #24449, #51957 ) ) ;
#39630 = CARTESIAN_POINT ( 'NONE',  ( -7.080981860525860760, -77.54444738242287372, 5.951650271570930073 ) ) ;
#39631 = CARTESIAN_POINT ( 'NONE',  ( -7.062685404271999978, -77.73978399679897677, 8.485436034813998774 ) ) ;
#39632 = CARTESIAN_POINT ( 'NONE',  ( -0.9218200799623775810, -77.92708333333332860, 1.199500263597266247 ) ) ;
#39633 = CARTESIAN_POINT ( 'NONE',  ( -8.680270256945998852, -77.23654793159298038, 3.860428508128000313 ) ) ;
#39634 = CARTESIAN_POINT ( 'NONE',  ( 7.612971414713999962, -23.32452529362999982, 10.53003223722999948 ) ) ;
#39635 = CARTESIAN_POINT ( 'NONE',  ( -3.989559569275991979, -79.49016193574067302, -8.633000817857986675 ) ) ;
#39636 = CARTESIAN_POINT ( 'NONE',  ( 8.266608573639034674, -53.82766203646255576, -9.697383820226121998 ) ) ;
#39637 = CARTESIAN_POINT ( 'NONE',  ( -7.179058446792000225, -80.00010590276899336, -8.667882172381000672 ) ) ;
#39638 = CARTESIAN_POINT ( 'NONE',  ( 12.82229880959000035, -18.57735182838000298, -2.065917129154000165 ) ) ;
#39639 = DIRECTION ( 'NONE',  ( 1.000000000000000000, 0.000000000000000000, 0.000000000000000000 ) ) ;
#39640 = CARTESIAN_POINT ( 'NONE',  ( -9.499653450934914645, -79.30027302004205580, 1.387647615217423080E-06 ) ) ;
#39641 = ORIENTED_EDGE ( 'NONE', *, *, #40364, .T. ) ;
#39642 = CARTESIAN_POINT ( 'NONE',  ( -7.248874762069000610, -79.65039421481900206, -9.668155108506001127 ) ) ;
#39643 = AXIS2_PLACEMENT_3D ( 'NONE', #34866, #52896, #8015 ) ;
#39644 = CARTESIAN_POINT ( 'NONE',  ( -7.646091287746999754, -55.09149945095000334, 10.13691902390999999 ) ) ;
#39645 = CARTESIAN_POINT ( 'NONE',  ( 2.228685126279000173, -78.06179175213999599, 11.77068507108999995 ) ) ;
#39646 = ADVANCED_FACE ( 'NONE', ( #14898 ), #20053, .T. ) ;
#39647 = CARTESIAN_POINT ( 'NONE',  ( -10.35410226330999883, -18.59601732823000120, -7.619716344073999892 ) ) ;
#39648 = CIRCLE ( 'NONE', #30246, 5.100000000000000533 ) ;
#39650 = CARTESIAN_POINT ( 'NONE',  ( -10.98362417419999915, -18.84999999999999787, 0.5999999999999999778 ) ) ;
#39649 = CARTESIAN_POINT ( 'NONE',  ( 7.682331425190000118, -59.56486430393999854, 10.04115011120000034 ) ) ;
#39651 = CARTESIAN_POINT ( 'NONE',  ( -4.784380313523538319, -78.88333333333333997, -8.300970689365453126 ) ) ;
#39652 = CARTESIAN_POINT ( 'NONE',  ( 10.07719973192999952, -58.54888345776999614, -7.718346056099999686 ) ) ;
#39653 = DIRECTION ( 'NONE',  ( -1.000000000000000000, 0.000000000000000000, 0.000000000000000000 ) ) ;
#39654 = CARTESIAN_POINT ( 'NONE',  ( 9.707899084501001141, -77.11571227068199619, 5.708822989341999943 ) ) ;
#39655 = CARTESIAN_POINT ( 'NONE',  ( -10.48543666025111420, -78.25833333333331154, 6.043427764450754580 ) ) ;
#39656 = FACE_OUTER_BOUND ( 'NONE', #10703, .T. ) ;
#39657 = ORIENTED_EDGE ( 'NONE', *, *, #53660, .T. ) ;
#39658 = CARTESIAN_POINT ( 'NONE',  ( 11.75000000000000000, -78.45000000000000284, 0.000000000000000000 ) ) ;
#39659 = FACE_OUTER_BOUND ( 'NONE', #49211, .T. ) ;
#39660 = CARTESIAN_POINT ( 'NONE',  ( 0.000000000000000000, -80.19999999999998863, 0.000000000000000000 ) ) ;
#39661 = CARTESIAN_POINT ( 'NONE',  ( 1.801839102376999957, -2.465322672876999910, 3.169418229746999938 ) ) ;
#39662 = CARTESIAN_POINT ( 'NONE',  ( -0.9512330062464999791, -78.08007375745999923, 11.17646036812999988 ) ) ;
#39663 = CARTESIAN_POINT ( 'NONE',  ( 10.20077725957859371, -76.87621043607762772, 3.463738954154604421 ) ) ;
#39664 = CARTESIAN_POINT ( 'NONE',  ( 5.007692372854583240, -77.26250000000000284, -9.832060106187633153 ) ) ;
#39665 = CARTESIAN_POINT ( 'NONE',  ( -1.582498447116000184, -60.95086122444999432, 12.55493832976000057 ) ) ;
#39666 = CARTESIAN_POINT ( 'NONE',  ( 3.165411199172027512, -3.229166666666666519, -0.8506806241676553304 ) ) ;
#39667 = CARTESIAN_POINT ( 'NONE',  ( 3.805616819021000463, -82.35352836652198505, -1.402374097307999889 ) ) ;
#39668 = FACE_OUTER_BOUND ( 'NONE', #36566, .T. ) ;
#39669 = CARTESIAN_POINT ( 'NONE',  ( 4.106769510331843342, -77.10559041576395600, -11.35196456917261543 ) ) ;
#39670 = AXIS2_PLACEMENT_3D ( 'NONE', #11108, #37659, #6660 ) ;
#39671 = CARTESIAN_POINT ( 'NONE',  ( -6.618456890295999706, -76.78327565549400902, -8.969427176287000592 ) ) ;
#39672 = CARTESIAN_POINT ( 'NONE',  ( 1.142430001277040308, -81.88337218985522270, 0.5072272210963466588 ) ) ;
#39673 = CARTESIAN_POINT ( 'NONE',  ( 1.659612711100000082, -78.08553037389999929, 0.1150004796074000080 ) ) ;
#39674 = CARTESIAN_POINT ( 'NONE',  ( 10.14948852603999896, -56.04899164556000102, 7.674614791885000287 ) ) ;
#39675 = CARTESIAN_POINT ( 'NONE',  ( 1.310679582531385279, -78.79166666666667140, 0.7554284705563519831 ) ) ;
#39676 = CARTESIAN_POINT ( 'NONE',  ( -12.55458806508999992, -60.96283916815999504, 1.575041344316999936 ) ) ;
#39677 = CARTESIAN_POINT ( 'NONE',  ( -0.7043158906892222904, -80.21985320402481534, -10.73277725065178245 ) ) ;
#39678 = CARTESIAN_POINT ( 'NONE',  ( -8.596418555780431348, -77.05208333333332860, -6.606377239730338857 ) ) ;
#39679 = CARTESIAN_POINT ( 'NONE',  ( -1.134730520616228144, -81.37330620173663931, -0.9788030900385257249 ) ) ;
#39680 = CARTESIAN_POINT ( 'NONE',  ( 11.66950233118999947, -79.29659029478199272, -2.920592611544999606 ) ) ;
#39681 = EDGE_CURVE ( 'NONE', #19958, #46028, #50941, .T. ) ;
#39682 = DIRECTION ( 'NONE',  ( 0.7071067811865475727, 0.000000000000000000, -0.7071067811865475727 ) ) ;
#39683 = CARTESIAN_POINT ( 'NONE',  ( 3.521285801175999985, -79.17310371897299603, 10.69740673549999954 ) ) ;
#39684 = CARTESIAN_POINT ( 'NONE',  ( -10.98464796637059671, -23.30469563149750556, -0.5810037832618578646 ) ) ;
#39685 = ORIENTED_EDGE ( 'NONE', *, *, #51577, .T. ) ;
#39686 = EDGE_CURVE ( 'NONE', #35836, #9708, #42404, .T. ) ;
#39687 = CARTESIAN_POINT ( 'NONE',  ( -1.583004792618638135, -24.45209241160721803, 12.70616254410927937 ) ) ;
#39688 = VECTOR ( 'NONE', #38839, 1000.000000000000000 ) ;
#39689 = ORIENTED_EDGE ( 'NONE', *, *, #40805, .F. ) ;
#39690 = SURFACE_SIDE_STYLE ('',( #22263 ) ) ;
#39691 = EDGE_LOOP ( 'NONE', ( #11612, #56118, #44544, #7580 ) ) ;
#39692 = CIRCLE ( 'NONE', #126, 12.50000000000000000 ) ;
#39693 = CARTESIAN_POINT ( 'NONE',  ( 0.000000000000000000, -75.15999999999999659, 0.000000000000000000 ) ) ;
#39694 = LINE ( 'NONE', #31699, #44729 ) ;
#39695 = CARTESIAN_POINT ( 'NONE',  ( -2.637902738039999750, -79.46783057900900360, 10.59324478783000067 ) ) ;
#39696 = CARTESIAN_POINT ( 'NONE',  ( 3.260490012720000053, -82.41024718738999866, -1.390626556135999836 ) ) ;
#39697 = CARTESIAN_POINT ( 'NONE',  ( 1.449316606189569034, -79.26277057543936166, 9.388788162982219632 ) ) ;
#39698 = VERTEX_POINT ( 'NONE', #36755 ) ;
#39699 = CARTESIAN_POINT ( 'NONE',  ( 2.604371601988999529, -77.49395168096407360, -10.72853197743999942 ) ) ;
#39701 = EDGE_CURVE ( 'NONE', #21244, #29877, #6047, .T. ) ;
#39700 = CARTESIAN_POINT ( 'NONE',  ( 10.99067476705999979, -78.63267194099999813, -5.319090318451999977 ) ) ;
#39702 = ORIENTED_EDGE ( 'NONE', *, *, #410, .T. ) ;
#39703 = CYLINDRICAL_SURFACE ( 'NONE', #29150, 11.00000000000000000 ) ;
#39704 = CARTESIAN_POINT ( 'NONE',  ( -9.723199429427999974, -17.52306056076000118, 7.958735708429999889 ) ) ;
#39705 = CARTESIAN_POINT ( 'NONE',  ( 0.5173218454072999739, -79.60896080275701081, 1.229208833401000067 ) ) ;
#39706 = CARTESIAN_POINT ( 'NONE',  ( 0.000000000000000000, -90.29999999999999716, 0.000000000000000000 ) ) ;
#39707 = CARTESIAN_POINT ( 'NONE',  ( -1.625803502918283128, -86.31452044229997966, -3.560909881631929785 ) ) ;
#39708 = CARTESIAN_POINT ( 'NONE',  ( 0.8759936321165389117, -85.93109222455437646, 3.362092887207752234 ) ) ;
#39709 = CARTESIAN_POINT ( 'NONE',  ( -10.68064082909000057, -77.45636465244999158, 7.608522161463999289 ) ) ;
#39710 = CARTESIAN_POINT ( 'NONE',  ( 7.139902610388999982, -77.41714066711000442, -10.43201753306000157 ) ) ;
#39711 = CARTESIAN_POINT ( 'NONE',  ( 7.285770374979999353, -76.21115555539499553, -7.844054078469000046 ) ) ;
#39712 = DIRECTION ( 'NONE',  ( 0.9999463328794432337, 0.000000000000000000, -0.01036008498777044214 ) ) ;
#39713 = AXIS2_PLACEMENT_3D ( 'NONE', #39402, #35831, #23140 ) ;
#39714 = CARTESIAN_POINT ( 'NONE',  ( 3.923097297260000005, -77.16568667140100501, -8.674161723994000539 ) ) ;
#39715 = CARTESIAN_POINT ( 'NONE',  ( 2.545068763118000454, -82.42182391443098766, -3.252898933875000065 ) ) ;
#39716 = CARTESIAN_POINT ( 'NONE',  ( -10.01235002620999914, -55.50151115525000023, 7.653559626076999578 ) ) ;
#39717 = CARTESIAN_POINT ( 'NONE',  ( -1.332907328585176687, -3.009958170327963867, 2.963254743748688025 ) ) ;
#39718 = CARTESIAN_POINT ( 'NONE',  ( -3.238159006571999843, -78.63855496681158286, 1.037165980353000005 ) ) ;
#39719 = CARTESIAN_POINT ( 'NONE',  ( -12.00000000000000000, -18.75000000000000000, -1.250000000000000000 ) ) ;
#39720 = CARTESIAN_POINT ( 'NONE',  ( -5.059370734576000395, -80.98961836681789350, -10.06538451635999998 ) ) ;
#39721 = CARTESIAN_POINT ( 'NONE',  ( -3.054513261463999818, -2.798870392637999860, -2.270689576097000284 ) ) ;
#39722 = CARTESIAN_POINT ( 'NONE',  ( 10.73701163424265026, -77.19999999999998863, -0.8148447674452932166 ) ) ;
#39723 = VERTEX_POINT ( 'NONE', #9321 ) ;
#39724 = CARTESIAN_POINT ( 'NONE',  ( -7.620012114232000755, -60.00560398617000146, -10.53562503196000044 ) ) ;
#39725 = CARTESIAN_POINT ( 'NONE',  ( 5.539808784079907511, -79.36666666666666003, -9.611650271896827746 ) ) ;
#39726 = CARTESIAN_POINT ( 'NONE',  ( -1.297058042903999953, -81.24056691320100754, -0.3101879797029999941 ) ) ;
#39727 = AXIS2_PLACEMENT_3D ( 'NONE', #46643, #6171, #24181 ) ;
#39728 = CARTESIAN_POINT ( 'NONE',  ( -12.43641395964999852, -17.08198970748000178, 0.03481089025432999862 ) ) ;
#39729 = CARTESIAN_POINT ( 'NONE',  ( -12.97295173694999981, -77.55824801881999520, -1.020668466325000079 ) ) ;
#39730 = EDGE_CURVE ( 'NONE', #15955, #52954, #56835, .T. ) ;
#39731 = AXIS2_PLACEMENT_3D ( 'NONE', #47924, #48483, #30159 ) ;
#39732 = DIRECTION ( 'NONE',  ( 0.000000000000000000, 1.000000000000000000, 0.000000000000000000 ) ) ;
#39733 = FACE_OUTER_BOUND ( 'NONE', #27037, .T. ) ;
#39734 = VERTEX_POINT ( 'NONE', #40905 ) ;
#39735 = CARTESIAN_POINT ( 'NONE',  ( -7.960542989054001595, -80.68744634177852504, 7.971132368775000643 ) ) ;
#39736 = CARTESIAN_POINT ( 'NONE',  ( -1.250000000000000000, -23.25000000000000000, 12.50000000000000000 ) ) ;
#39737 = CARTESIAN_POINT ( 'NONE',  ( 12.77302471396000172, -61.52230123271999673, 1.481949986260999941 ) ) ;
#39738 = CARTESIAN_POINT ( 'NONE',  ( 6.043427764450807871, -79.06666666666666288, -10.48543666025108756 ) ) ;
#39739 = CARTESIAN_POINT ( 'NONE',  ( 7.350012343602999820, -77.58715215706898505, -6.223385617129999936 ) ) ;
#39740 = CARTESIAN_POINT ( 'NONE',  ( 0.2926469569035999863, -85.11057975687899102, -4.161840105401999779 ) ) ;
#39741 = CARTESIAN_POINT ( 'NONE',  ( -2.424017749977676051, -79.99353046406088197, 10.47610573998703742 ) ) ;
#39742 = CARTESIAN_POINT ( 'NONE',  ( -1.191059436918999959, -79.14830987996700173, -0.7689280169367000983 ) ) ;
#39743 = ORIENTED_EDGE ( 'NONE', *, *, #36905, .F. ) ;
#39744 = DIRECTION ( 'NONE',  ( 0.000000000000000000, -1.000000000000000000, 0.000000000000000000 ) ) ;
#39745 = CARTESIAN_POINT ( 'NONE',  ( 10.71369944335146229, -78.92916666666664582, -2.879226727952112874 ) ) ;
#39746 = CARTESIAN_POINT ( 'NONE',  ( -2.040407335258644039, -78.82460961380570552, -3.421830084111916026 ) ) ;
#39747 = ORIENTED_EDGE ( 'NONE', *, *, #38950, .T. ) ;
#39748 = ORIENTED_EDGE ( 'NONE', *, *, #4478, .T. ) ;
#39749 = CARTESIAN_POINT ( 'NONE',  ( -10.76843015134999959, -79.79903360897698406, 1.073136842994000029 ) ) ;
#39750 = CARTESIAN_POINT ( 'NONE',  ( 0.000000000000000000, -86.09999999999999432, 0.000000000000000000 ) ) ;
#39751 = CARTESIAN_POINT ( 'NONE',  ( -7.226987988700000365, -79.87689231032499038, -8.725751546883000032 ) ) ;
#39752 = ORIENTED_EDGE ( 'NONE', *, *, #32194, .T. ) ;
#39753 = EDGE_CURVE ( 'NONE', #48636, #1742, #13446, .T. ) ;
#39754 = ORIENTED_EDGE ( 'NONE', *, *, #44361, .F. ) ;
#39755 = ORIENTED_EDGE ( 'NONE', *, *, #41580, .T. ) ;
#39756 = CYLINDRICAL_SURFACE ( 'NONE', #2179, 11.00000000000000000 ) ;
#39757 = CARTESIAN_POINT ( 'NONE',  ( -2.217000330786000450, -79.64323432020552218, 9.512392227823999846 ) ) ;
#39758 = ORIENTED_EDGE ( 'NONE', *, *, #16251, .T. ) ;
#39759 = EDGE_CURVE ( 'NONE', #25961, #56481, #14144, .T. ) ;
#39760 = VERTEX_POINT ( 'NONE', #47106 ) ;
#39761 = CARTESIAN_POINT ( 'NONE',  ( 0.7967880007212916338, -79.82850301384860359, -0.9953065419355184851 ) ) ;
#39762 = AXIS2_PLACEMENT_3D ( 'NONE', #55041, #18742, #36735 ) ;
#39763 = CARTESIAN_POINT ( 'NONE',  ( -3.620804144604786057, -78.99318692614357929, 0.06825924720741134710 ) ) ;
#39764 = AXIS2_PLACEMENT_3D ( 'NONE', #38311, #1741, #51041 ) ;
#39765 = CARTESIAN_POINT ( 'NONE',  ( 7.646788101807000082, -55.42771363232999704, 10.00831428589000005 ) ) ;
#39766 = PLANE ( 'NONE',  #45910 ) ;
#39767 = DIRECTION ( 'NONE',  ( 0.9903465037221068634, -0.1386138613754009652, 0.000000000000000000 ) ) ;
#39768 = CARTESIAN_POINT ( 'NONE',  ( -10.80752097171290416, -80.82844002948797879, 2.980286201706882743 ) ) ;
#39769 = CARTESIAN_POINT ( 'NONE',  ( 7.655542440077000244, -56.02180874340999850, -10.38645071868999992 ) ) ;
#39770 = CARTESIAN_POINT ( 'NONE',  ( 1.750000000000000000, -60.04999999657000131, -12.50000000000000000 ) ) ;
#39771 = CARTESIAN_POINT ( 'NONE',  ( -10.53495260691999924, -23.22711197486000145, 7.618387230241999930 ) ) ;
#39772 = CARTESIAN_POINT ( 'NONE',  ( -1.460959015002473826, -79.92083333333336270, -0.3926218265389207485 ) ) ;
#39773 = CARTESIAN_POINT ( 'NONE',  ( -3.770520861067999885, -78.43767549782629089, 1.207678794456000126 ) ) ;
#39774 = CARTESIAN_POINT ( 'NONE',  ( -2.546514579946999923, -77.15288667140099221, 9.424721798891001256 ) ) ;
#39775 = PRODUCT_DEFINITION ( 'UNKNOWN', '', #30046, #30961 ) ;
#39776 = DIRECTION ( 'NONE',  ( -0.7071067811864980568, 0.7071067811865969777, 1.168837541411996137E-09 ) ) ;
#39777 = CARTESIAN_POINT ( 'NONE',  ( -1.439896632895359962, -77.98541666666666572, 10.99999999999999645 ) ) ;
#39778 = CARTESIAN_POINT ( 'NONE',  ( 0.03250568004163000707, -75.87309702343600293, 11.74995503739000036 ) ) ;
#39779 = CARTESIAN_POINT ( 'NONE',  ( -8.150146600852348655, -60.21532333328943309, -7.387512494710285260 ) ) ;
#39780 = DIRECTION ( 'NONE',  ( 0.000000000000000000, 1.000000000000000000, 0.000000000000000000 ) ) ;
#39781 = CARTESIAN_POINT ( 'NONE',  ( 1.418826352046264949, -78.23560893958142515, -10.68831118249899426 ) ) ;
#39782 = CARTESIAN_POINT ( 'NONE',  ( 1.152612928993206332, -80.65700505819430077, 1.031344352619617766 ) ) ;
#39783 = CARTESIAN_POINT ( 'NONE',  ( -9.183761103090999356, -77.50442046432299037, 1.919071004230999966 ) ) ;
#39784 = CARTESIAN_POINT ( 'NONE',  ( -1.585290096527000259, -78.42326554362610125, -0.3067070840873000193 ) ) ;
#39785 = DIRECTION ( 'NONE',  ( 0.000000000000000000, -1.000000000000000000, 2.812564995716999917E-14 ) ) ;
#39786 = CARTESIAN_POINT ( 'NONE',  ( 3.791268666074999683, -77.37336614992500472, 10.23726759892000082 ) ) ;
#39787 = EDGE_CURVE ( 'NONE', #39760, #45960, #21957, .T. ) ;
#39788 = CARTESIAN_POINT ( 'NONE',  ( 7.972949129781999211, -77.12301250442499168, -9.187753233325999247 ) ) ;
#39789 = CARTESIAN_POINT ( 'NONE',  ( -1.500000000000000888, -80.98958333333332860, 0.1963495408493559080 ) ) ;
#39791 = CARTESIAN_POINT ( 'NONE',  ( 0.6775591888709999733, -77.90986211677478934, -1.132025780260999870 ) ) ;
#39790 = LINE ( 'NONE', #52517, #33579 ) ;
#39792 = CARTESIAN_POINT ( 'NONE',  ( 0.4426188121580000301, -81.79270613248999666, -1.400191678299000042 ) ) ;
#39793 = CARTESIAN_POINT ( 'NONE',  ( -9.134412046857288914, -79.55589225187523539, 5.669345810953543285 ) ) ;
#39794 = VERTEX_POINT ( 'NONE', #38214 ) ;
#39795 = EDGE_CURVE ( 'NONE', #2615, #31027, #56237, .T. ) ;
#39796 = CARTESIAN_POINT ( 'NONE',  ( 6.365665562422999635, -78.73050366622999263, 10.17242851768000023 ) ) ;
#39797 = CARTESIAN_POINT ( 'NONE',  ( 8.539931521643000067, -79.44584810362599114, -8.651281711199999336 ) ) ;
#39798 = CARTESIAN_POINT ( 'NONE',  ( -5.666459946039999807, -80.15558659221879623, -9.493356078915999419 ) ) ;
#39799 = CARTESIAN_POINT ( 'NONE',  ( 12.00000000000000000, -79.65624999999998579, 0.9424777960769732399 ) ) ;
#39800 = CARTESIAN_POINT ( 'NONE',  ( 9.611650271896820641, -78.89166666666666572, 5.539808784079911952 ) ) ;
#39801 = CIRCLE ( 'NONE', #21893, 9.000000000000000000 ) ;
#39802 = CARTESIAN_POINT ( 'NONE',  ( -2.719292624632000166, -1.072128508794999879, 2.510906049621999703 ) ) ;
#39803 = CARTESIAN_POINT ( 'NONE',  ( 9.494251020668999175, -78.90826789792399154, 1.836410959852999847 ) ) ;
#39804 = CARTESIAN_POINT ( 'NONE',  ( 12.66313299633999812, -25.17803434852999800, 0.06050769725596999438 ) ) ;
#39805 = CARTESIAN_POINT ( 'NONE',  ( -1.667961430005999945, -58.54888345776999614, 12.58335110162999904 ) ) ;
#39806 = VERTEX_POINT ( 'NONE', #15786 ) ;
#39807 = CARTESIAN_POINT ( 'NONE',  ( 8.485281374238999419, -23.25000000000000000, 8.485281374238999419 ) ) ;
#39808 = CARTESIAN_POINT ( 'NONE',  ( 8.583677312638442913, -24.97185920791718061, -9.102132574100766149 ) ) ;
#39809 = DIRECTION ( 'NONE',  ( -1.000000000000000000, 0.000000000000000000, 0.000000000000000000 ) ) ;
#39810 = CARTESIAN_POINT ( 'NONE',  ( -10.01234990226999955, -55.50150862742999891, -7.653559502261000347 ) ) ;
#39811 = CARTESIAN_POINT ( 'NONE',  ( -1.473365879748000040, -82.90842953870898668, 3.227033238383000047 ) ) ;
#39812 = CONICAL_SURFACE ( 'NONE', #35078, 2.149999999947999729, 0.7853981633972997312 ) ;
#39813 = ORIENTED_EDGE ( 'NONE', *, *, #49245, .F. ) ;
#39814 = FACE_OUTER_BOUND ( 'NONE', #35165, .T. ) ;
#39815 = FACE_OUTER_BOUND ( 'NONE', #40021, .T. ) ;
#39816 = CARTESIAN_POINT ( 'NONE',  ( 0.8506806241676642122, -1.145833333333333481, -3.165411199172024848 ) ) ;
#39817 = ORIENTED_EDGE ( 'NONE', *, *, #35451, .T. ) ;
#39818 = AXIS2_PLACEMENT_3D ( 'NONE', #47489, #55448, #15877 ) ;
#39819 = CARTESIAN_POINT ( 'NONE',  ( -10.47840693000000023, -55.01310507149000273, -7.622759963108999948 ) ) ;
#39820 = VECTOR ( 'NONE', #32834, 1000.000000000000000 ) ;
#39821 = SURFACE_SIDE_STYLE ('',( #44853 ) ) ;
#39822 = CARTESIAN_POINT ( 'NONE',  ( -8.448510849392999233, -79.22801525502798370, 4.901364000006999788 ) ) ;
#39823 = ORIENTED_EDGE ( 'NONE', *, *, #19172, .T. ) ;
#39824 = ORIENTED_EDGE ( 'NONE', *, *, #31373, .T. ) ;
#39826 = EDGE_CURVE ( 'NONE', #1567, #48012, #47460, .T. ) ;
#39825 = CARTESIAN_POINT ( 'NONE',  ( 12.14581882086999975, -76.92655382554799814, -2.250985356504000112 ) ) ;
#39827 = CARTESIAN_POINT ( 'NONE',  ( -9.532031226582633465, -78.63842284804186988, -4.970339354283964894 ) ) ;
#39828 = EDGE_CURVE ( 'NONE', #44485, #18159, #30424, .T. ) ;
#39829 = ORIENTED_EDGE ( 'NONE', *, *, #8641, .F. ) ;
#39830 = CARTESIAN_POINT ( 'NONE',  ( 5.807838419657000095, -77.36753084965400262, -7.511754867730999763 ) ) ;
#39831 = CARTESIAN_POINT ( 'NONE',  ( -3.536740297498699448, -78.25459137991194325, 9.036885296280029678 ) ) ;
#39832 = CARTESIAN_POINT ( 'NONE',  ( 0.5247358252921234811, -80.25970768809875722, -1.134507553617768671 ) ) ;
#39833 = CARTESIAN_POINT ( 'NONE',  ( 5.691226796558999546, -77.83365458999999476, 11.81421328157999895 ) ) ;
#39834 = CARTESIAN_POINT ( 'NONE',  ( -11.14038684213999630, -78.24070234355004061, 1.307628137226999998 ) ) ;
#39835 = CARTESIAN_POINT ( 'NONE',  ( 7.714303428875997959, -15.69705297113999443, 12.53545825868000385 ) ) ;
#39836 = CARTESIAN_POINT ( 'NONE',  ( 1.533375225220143134, -86.36264283715698298, 3.533266005812232269 ) ) ;
#39837 = CARTESIAN_POINT ( 'NONE',  ( -10.71602610194999805, -79.87781303454870852, 3.314346869870000489 ) ) ;
#39838 = CARTESIAN_POINT ( 'NONE',  ( 3.524287703716790343, -79.94398289640221833, 8.552247391394926623 ) ) ;
#39839 = DIRECTION ( 'NONE',  ( -1.000000000000000000, 0.000000000000000000, 0.000000000000000000 ) ) ;
#39840 = ORIENTED_EDGE ( 'NONE', *, *, #6908, .F. ) ;
#39841 = CARTESIAN_POINT ( 'NONE',  ( -6.574673376928999780, -79.04539988511800175, 9.148912741538998361 ) ) ;
#39842 = CARTESIAN_POINT ( 'NONE',  ( -12.19234209666000091, -76.06301006652999774, -1.697737568323999913 ) ) ;
#39843 = CARTESIAN_POINT ( 'NONE',  ( 0.3499829075702999837, -79.44216343900099275, -1.373881155581999858 ) ) ;
#39844 = AXIS2_PLACEMENT_3D ( 'NONE', #51948, #24488, #38062 ) ;
#39845 = FACE_OUTER_BOUND ( 'NONE', #19889, .T. ) ;
#39846 = CARTESIAN_POINT ( 'NONE',  ( 1.020992902784864986, -3.200861152918981656, 3.368731490719146127 ) ) ;
#39847 = EDGE_CURVE ( 'NONE', #25463, #28651, #31340, .T. ) ;
#39848 = CARTESIAN_POINT ( 'NONE',  ( -1.047405116191372443, -80.65287959514462557, -0.8248589924739977430 ) ) ;
#39849 = FACE_OUTER_BOUND ( 'NONE', #33232, .T. ) ;
#39850 = LINE ( 'NONE', #35406, #57185 ) ;
#39851 = CARTESIAN_POINT ( 'NONE',  ( 5.418544735220999442, -78.39158470334899675, 9.753510481391998610 ) ) ;
#39852 = CARTESIAN_POINT ( 'NONE',  ( 1.741786704463999857, -77.58258832859900167, -9.469768965712999531 ) ) ;
#39853 = CARTESIAN_POINT ( 'NONE',  ( 10.42272502862000039, -21.75453807238000081, -7.691893942719999266 ) ) ;
#39854 = CARTESIAN_POINT ( 'NONE',  ( -1.160500472347511636, -83.06980021841565076, 0.4644083125726469197 ) ) ;
#39855 = CARTESIAN_POINT ( 'NONE',  ( 6.322255100220510293, -76.28719745902344584, 11.39032443625401214 ) ) ;
#39856 = CIRCLE ( 'NONE', #3096, 11.05000000000000071 ) ;
#39857 = B_SPLINE_SURFACE_WITH_KNOTS ( 'NONE', 3, 3, ( 
 ( #29336, #11647, #20780, #6915 ),
 ( #20499, #24348, #20215, #7203 ),
 ( #29624, #47383, #51514, #19622 ),
 ( #46805, #38495, #42359, #37912 ),
 ( #10778, #1633, #56512, #15487 ),
 ( #43225, #24922, #47678, #33477 ),
 ( #2493, #16068, #1929, #15189 ),
 ( #11074, #34050, #6624, #52088 ) ),
 .UNSPECIFIED., .F., .F., .F.,
 ( 4, 1, 1, 1, 1, 4 ),
 ( 4, 4 ),
 ( -0.01200407347464999865, 0.000000000000000000, 0.3333333333333000081, 0.6666666666667000474, 1.000000000000000000, 1.011997855551999947 ),
 ( -0.3559705542741999906, 1.355970554273999928 ),
 .UNSPECIFIED. ) ;
#39858 = EDGE_LOOP ( 'NONE', ( #27996, #40404, #71, #43265, #2685 ) ) ;
#39859 = CARTESIAN_POINT ( 'NONE',  ( 0.5343721329914999929, -82.61129654213999629, -1.367806479096000061 ) ) ;
#39860 = CARTESIAN_POINT ( 'NONE',  ( -0.5035993198763999423, -79.55212327692998997, -1.271638408173999979 ) ) ;
#39861 = CARTESIAN_POINT ( 'NONE',  ( -0.4635254915624000271, -77.75000000000000000, 1.426584774443000025 ) ) ;
#39862 = FACE_OUTER_BOUND ( 'NONE', #1721, .T. ) ;
#39863 = CARTESIAN_POINT ( 'NONE',  ( 0.000000000000000000, -75.10000000032299283, -4.199999999676998996 ) ) ;
#39864 = CIRCLE ( 'NONE', #38028, 1.200000000000000622 ) ;
#39865 = CARTESIAN_POINT ( 'NONE',  ( 1.210004456578480880, -78.97461667811870711, -0.3996061539552085984 ) ) ;
#39866 = CARTESIAN_POINT ( 'NONE',  ( -1.828203654226000063, -77.96382883426899468, 11.79377691179999843 ) ) ;
#39867 = CARTESIAN_POINT ( 'NONE',  ( -3.039602602086000083, -79.22975194988498515, -9.236151215514999180 ) ) ;
#39868 = CARTESIAN_POINT ( 'NONE',  ( 1.459128634122999868, -77.28030449881099173, -9.409639786240999726 ) ) ;
#39869 = CARTESIAN_POINT ( 'NONE',  ( -1.814305421036000121, -54.51058030636000495, -12.78003582248999948 ) ) ;
#39870 = CARTESIAN_POINT ( 'NONE',  ( 10.85629140140682125, -75.98074698996606458, 4.494010003869360226 ) ) ;
#39871 = CARTESIAN_POINT ( 'NONE',  ( 4.606177061618020652, -86.02148118236286223, 0.5287147981160357224 ) ) ;
#39872 = ORIENTED_EDGE ( 'NONE', *, *, #34935, .F. ) ;
#39873 = ADVANCED_FACE ( 'NONE', ( #56522 ), #38902, .F. ) ;
#39874 = CONICAL_SURFACE ( 'NONE', #8775, 11.80312499993000053, 0.7853981633972997312 ) ;
#39875 = CARTESIAN_POINT ( 'NONE',  ( -1.460959015002474493, -79.37916666666664867, 0.3926218265389144757 ) ) ;
#39876 = CARTESIAN_POINT ( 'NONE',  ( -9.534922033296867383, -78.74983463097288450, -6.929927095622216981 ) ) ;
#39877 = CARTESIAN_POINT ( 'NONE',  ( 3.999999999999884981, -78.69999999999998863, -2.360693579763222694 ) ) ;
#39878 = CARTESIAN_POINT ( 'NONE',  ( -1.510823314100999903, -83.34742229952999537, -0.3534059060544000319 ) ) ;
#39879 = CARTESIAN_POINT ( 'NONE',  ( -9.871730464199000465, -79.89415484708798942, 4.797141237513000256 ) ) ;
#39880 = CARTESIAN_POINT ( 'NONE',  ( 1.689459950990167547, -17.70811746100764950, 12.71013585610350383 ) ) ;
#39881 = CARTESIAN_POINT ( 'NONE',  ( 9.325195487021998630, -76.70256541335099598, -7.974226357216999794 ) ) ;
#39882 = DIRECTION ( 'NONE',  ( 0.6489586447330936148, -0.04890182338522946343, 0.7592504784955924624 ) ) ;
#39883 = DIRECTION ( 'NONE',  ( -1.000000000000000000, 0.000000000000000000, 0.000000000000000000 ) ) ;
#39884 = ORIENTED_EDGE ( 'NONE', *, *, #16238, .F. ) ;
#39885 = CARTESIAN_POINT ( 'NONE',  ( -11.13698119474000059, -79.71223007984299613, -0.4714344481541999921 ) ) ;
#39886 = CARTESIAN_POINT ( 'NONE',  ( -4.211014631457025814, -77.41241489099887474, 8.267936520958334867 ) ) ;
#39887 = DIRECTION ( 'NONE',  ( 0.000000000000000000, -1.000000000000000000, 0.000000000000000000 ) ) ;
#39888 = CARTESIAN_POINT ( 'NONE',  ( 11.03731426084000056, -79.00475665554398574, 1.633797283747999929 ) ) ;
#39889 = DIRECTION ( 'NONE',  ( 0.000000000000000000, 0.7071067811866525998, -0.7071067811864425456 ) ) ;
#39890 = CIRCLE ( 'NONE', #2211, 2.600000000000000089 ) ;
#39891 = DIRECTION ( 'NONE',  ( 0.7071067811704841999, -1.939413340559955448E-07, -0.7071067812025843002 ) ) ;
#39892 = CARTESIAN_POINT ( 'NONE',  ( 12.27743704900000132, -78.07818225714999016, 0.2455986337158999888 ) ) ;
#39893 = VERTEX_POINT ( 'NONE', #38506 ) ;
#39894 = CARTESIAN_POINT ( 'NONE',  ( 9.243145382185367964, -17.08347263196495192, -8.441178780123935965 ) ) ;
#39895 = CARTESIAN_POINT ( 'NONE',  ( 8.018769647075153273, -79.51052682219849999, 7.624166446277075515 ) ) ;
#39896 = TOROIDAL_SURFACE ( 'NONE', #49359, 26.50000000000000000, 14.00000000000000000 ) ;
#39897 = DIRECTION ( 'NONE',  ( 0.000000000000000000, -1.000000000000000000, 0.000000000000000000 ) ) ;
#39898 = EDGE_LOOP ( 'NONE', ( #9296, #20033, #35287, #35502 ) ) ;
#39899 = ORIENTED_EDGE ( 'NONE', *, *, #52763, .F. ) ;
#39900 = CARTESIAN_POINT ( 'NONE',  ( -8.414570695956999913, -59.94999999967000548, 8.414570695956999913 ) ) ;
#39901 = CARTESIAN_POINT ( 'NONE',  ( 9.330693044838000105, -77.86253998579799429, -1.999643576009999757 ) ) ;
#39902 = ORIENTED_EDGE ( 'NONE', *, *, #23579, .F. ) ;
#39903 = CARTESIAN_POINT ( 'NONE',  ( -6.452442768351031255, -79.68423335831413112, 7.009317820372825913 ) ) ;
#39904 = ORIENTED_EDGE ( 'NONE', *, *, #43046, .T. ) ;
#39905 = CARTESIAN_POINT ( 'NONE',  ( 7.646944885436999684, -23.19635956544000166, 10.19022188674999896 ) ) ;
#39906 = CIRCLE ( 'NONE', #21998, 13.86363636363999952 ) ;
#39907 = CARTESIAN_POINT ( 'NONE',  ( -0.9355429176084000265, -78.02289305516799800, 10.99211052673000033 ) ) ;
#39908 = CONICAL_SURFACE ( 'NONE', #35174, 1.099999997148999986, 0.7853981633972997312 ) ;
#39909 = CARTESIAN_POINT ( 'NONE',  ( -3.028287605162000240, -79.22903998579799634, -9.201769410957998829 ) ) ;
#39910 = CARTESIAN_POINT ( 'NONE',  ( -8.666955468490126435, -78.12913193041232773, -3.288494062500119774 ) ) ;
#39911 = CARTESIAN_POINT ( 'NONE',  ( -0.2291600886666000092, -78.32170900562999805, -11.06898422383999936 ) ) ;
#39912 = CARTESIAN_POINT ( 'NONE',  ( 1.150218351780601056, -79.38243505016826873, 0.4888114725149512174 ) ) ;
#39913 = ORIENTED_EDGE ( 'NONE', *, *, #2918, .T. ) ;
#39914 = VERTEX_POINT ( 'NONE', #37921 ) ;
#39915 = CARTESIAN_POINT ( 'NONE',  ( -1.459284021221519234, -77.48767362326580610, 9.134122967561379980 ) ) ;
#39916 = CARTESIAN_POINT ( 'NONE',  ( 6.574300740938999077, -77.48530632747599611, -8.869200617850999890 ) ) ;
#39917 = CARTESIAN_POINT ( 'NONE',  ( -5.838193839761687265, -77.47291666666666288, -7.596835002782715840 ) ) ;
#39918 = CARTESIAN_POINT ( 'NONE',  ( 0.8618009059429999619, -78.52253077722298258, -9.665816497589000633 ) ) ;
#39919 = CARTESIAN_POINT ( 'NONE',  ( -1.894422427200999959, -76.61909451939000348, -12.98637956171999974 ) ) ;
#39920 = ADVANCED_FACE ( 'NONE', ( #16081 ), #46487, .T. ) ;
#39921 = CARTESIAN_POINT ( 'NONE',  ( 2.117002802198683753, -2.180884342491374639, -2.498681180296688176 ) ) ;
#39922 = CARTESIAN_POINT ( 'NONE',  ( -1.472167250137000005, -78.74622289817000365, -0.6938203229310999642 ) ) ;
#39923 = CARTESIAN_POINT ( 'NONE',  ( 8.693423296916000353, -80.18569232445499040, -7.148151291522000683 ) ) ;
#39924 = CARTESIAN_POINT ( 'NONE',  ( 12.72397198033999999, -18.77854962937000138, -1.930909771329999858 ) ) ;
#39925 = CARTESIAN_POINT ( 'NONE',  ( -9.389195554418000356, -24.71043214204999927, -8.194863653270999748 ) ) ;
#39926 = CARTESIAN_POINT ( 'NONE',  ( -2.421167930323333106, -78.60416666666664298, -9.009247259181917045 ) ) ;
#39927 = ORIENTED_EDGE ( 'NONE', *, *, #33943, .F. ) ;
#39928 = CARTESIAN_POINT ( 'NONE',  ( 8.704926853273999399, -78.81797727176099500, 7.993911894783999550 ) ) ;
#39929 = CARTESIAN_POINT ( 'NONE',  ( -7.634437838894000627, -55.05219468418000162, 10.30764259108000225 ) ) ;
#39930 = CARTESIAN_POINT ( 'NONE',  ( -7.614885234455580409, -78.03764472252724715, 7.587876194577269473 ) ) ;
#39931 = CARTESIAN_POINT ( 'NONE',  ( -11.86109855473999986, -78.64510676903400110, -1.682380905046999997 ) ) ;
#39932 = CARTESIAN_POINT ( 'NONE',  ( -7.961057357828999592, -17.46431744651999907, -9.783210913639999617 ) ) ;
#39933 = CARTESIAN_POINT ( 'NONE',  ( 7.691916945423999508, -57.04634220890999785, 10.42274798266000069 ) ) ;
#39934 = CARTESIAN_POINT ( 'NONE',  ( -0.5668640707507043297, -53.88340304925345947, 12.50470739224864936 ) ) ;
#39935 = CARTESIAN_POINT ( 'NONE',  ( -9.660486042390999728, -80.07923827687199037, 5.576357409276999633 ) ) ;
#39936 = B_SPLINE_CURVE_WITH_KNOTS ( 'NONE', 3,
 ( #21490, #31195, #16782, #12909, #30624, #13200, #34763, #48373, #21198, #39777, #48942, #57791, #40374, #44506, #8786, #35043, #58381, #39199 ),
 .UNSPECIFIED., .F., .F.,
 ( 4, 2, 2, 2, 2, 2, 2, 2, 4 ),
 ( 0.000000000000000000, 0.1249999999999999445, 0.2499999999999998890, 0.3749999999999999445, 0.5000000000000000000, 0.6250000000000000000, 0.7500000000000001110, 0.8750000000000000000, 1.000000000000000000 ),
 .UNSPECIFIED. ) ;
#39937 = DIRECTION ( 'NONE',  ( 1.000000000000000000, 0.000000000000000000, 0.000000000000000000 ) ) ;
#39938 = CARTESIAN_POINT ( 'NONE',  ( -11.16978667388999824, -77.33360301469699039, -1.438690452479999937 ) ) ;
#39939 = CARTESIAN_POINT ( 'NONE',  ( 0.8506806241676508895, -1.854166666666666741, 3.165411199172028400 ) ) ;
#39940 = CARTESIAN_POINT ( 'NONE',  ( -9.186543509187998779, -80.37243427822239994, -6.503932264059000268 ) ) ;
#39941 = ORIENTED_EDGE ( 'NONE', *, *, #26975, .F. ) ;
#39942 = CARTESIAN_POINT ( 'NONE',  ( -11.75000000000000000, -77.20000000000000284, -1.435311119447000145E-14 ) ) ;
#39943 = ADVANCED_FACE ( 'NONE', ( #11084 ), #29919, .F. ) ;
#39944 = CIRCLE ( 'NONE', #47530, 1.000000000000000000 ) ;
#39945 = CARTESIAN_POINT ( 'NONE',  ( 10.61050599188999932, -77.92876026662598576, -2.901234667509999809 ) ) ;
#39946 = DIRECTION ( 'NONE',  ( 0.000000000000000000, 0.000000000000000000, -1.000000000000000000 ) ) ;
#39947 = CARTESIAN_POINT ( 'NONE',  ( -3.434418375904999987, -2.158690377978999653, -1.223358650580000040 ) ) ;
#39948 = CARTESIAN_POINT ( 'NONE',  ( 6.201912463541000342, -78.37059474947899673, -9.171216270948999494 ) ) ;
#39949 = CARTESIAN_POINT ( 'NONE',  ( 5.694538069269999623E-14, -72.84999999994899156, -13.94999999994999840 ) ) ;
#39950 = CARTESIAN_POINT ( 'NONE',  ( 7.236935317891325603, -77.20000000000000284, 8.029755504972245106 ) ) ;
#39951 = CIRCLE ( 'NONE', #55051, 12.05000000000000071 ) ;
#39952 = CARTESIAN_POINT ( 'NONE',  ( -0.4260390295771080971, -1.986914419589991487, 3.249230163478797451 ) ) ;
#39953 = CARTESIAN_POINT ( 'NONE',  ( 0.000000000000000000, -82.50000000000000000, -1.000000000000000000 ) ) ;
#39954 = AXIS2_PLACEMENT_3D ( 'NONE', #40668, #32659, #10251 ) ;
#39955 = CARTESIAN_POINT ( 'NONE',  ( -1.733945428922999854, -82.98374735065199559, 3.797766467643000077 ) ) ;
#39956 = DIRECTION ( 'NONE',  ( -1.000000000000000000, 0.000000000000000000, 0.000000000000000000 ) ) ;
#39957 = EDGE_CURVE ( 'NONE', #11684, #51104, #7159, .T. ) ;
#39958 = CARTESIAN_POINT ( 'NONE',  ( -10.79518247106041251, -76.98995411785524823, -5.399136025279304363 ) ) ;
#39959 = EDGE_CURVE ( 'NONE', #17731, #23873, #57777, .T. ) ;
#39960 = CARTESIAN_POINT ( 'NONE',  ( 8.315675604772998497, -77.96769278298098982, -7.594965687514999786 ) ) ;
#39961 = CARTESIAN_POINT ( 'NONE',  ( 0.8603538941506917448, -81.91514795278682470, 0.9063378267799424570 ) ) ;
#39962 = CARTESIAN_POINT ( 'NONE',  ( 1.113300400990999917, -78.20452863244999264, 1.077154774809000015 ) ) ;
#39963 = CARTESIAN_POINT ( 'NONE',  ( -0.5065222552852000071, -77.20932084810999640, 9.658707080791000266 ) ) ;
#39964 = CARTESIAN_POINT ( 'NONE',  ( -1.001315002179000047, -17.31477588286000113, -12.50000000000000000 ) ) ;
#39965 = DIRECTION ( 'NONE',  ( 0.000000000000000000, 0.000000000000000000, -1.000000000000000000 ) ) ;
#39966 = CARTESIAN_POINT ( 'NONE',  ( -3.988375677951307541, -80.19515755555565306, -9.982611414254499493 ) ) ;
#39967 = CARTESIAN_POINT ( 'NONE',  ( -12.56594317989000054, -23.24999999414999863, -1.750000000001000089 ) ) ;
#39968 = CARTESIAN_POINT ( 'NONE',  ( 7.808727470805389537, -79.03618450172675125, -8.052663177511117709 ) ) ;
#39969 = ORIENTED_EDGE ( 'NONE', *, *, #21768, .T. ) ;
#39970 = CARTESIAN_POINT ( 'NONE',  ( 1.049808574365361347, -81.80446097931094585, -0.6784272128118777889 ) ) ;
#39971 = CYLINDRICAL_SURFACE ( 'NONE', #55789, 12.00000000000000000 ) ;
#39972 = CARTESIAN_POINT ( 'NONE',  ( 5.948804865077000237, -80.22133913145148654, 9.426875752653000262 ) ) ;
#39973 = CARTESIAN_POINT ( 'NONE',  ( 7.353725627631192197, -55.49344856148322691, 8.180687091746198902 ) ) ;
#39974 = EDGE_LOOP ( 'NONE', ( #45933, #28579, #55311, #47774 ) ) ;
#39975 = EDGE_LOOP ( 'NONE', ( #13650, #13403, #29605, #31103, #29006, #29796, #19464, #39823 ) ) ;
#39976 = CARTESIAN_POINT ( 'NONE',  ( -3.215437157339553487, -0.7500000000000000000, 1.430139912060602425 ) ) ;
#39977 = EDGE_CURVE ( 'NONE', #3036, #11190, #35994, .T. ) ;
#39978 = ORIENTED_EDGE ( 'NONE', *, *, #12177, .F. ) ;
#39979 = CARTESIAN_POINT ( 'NONE',  ( 10.10912542004786907, -55.32413588747969868, -7.634643956464879366 ) ) ;
#39980 = ORIENTED_EDGE ( 'NONE', *, *, #3473, .T. ) ;
#39981 = DIRECTION ( 'NONE',  ( 0.000000000000000000, 0.000000000000000000, 1.000000000000000000 ) ) ;
#39982 = CYLINDRICAL_SURFACE ( 'NONE', #48438, 10.25000000000000000 ) ;
#39983 = CARTESIAN_POINT ( 'NONE',  ( -8.243938165231000426, -79.69897570143299959, -7.330703780023000604 ) ) ;
#39984 = CARTESIAN_POINT ( 'NONE',  ( -9.596002108778161954, -76.35208333329295272, -7.374560639698982456 ) ) ;
#39985 = CARTESIAN_POINT ( 'NONE',  ( 0.5018391472701999589, -79.41170382117660154, -3.722840512358000176 ) ) ;
#39986 = CARTESIAN_POINT ( 'NONE',  ( -7.601074271102891800, -79.34838228251635428, 5.698502993689569252 ) ) ;
#39987 = ORIENTED_EDGE ( 'NONE', *, *, #39432, .T. ) ;
#39988 = CARTESIAN_POINT ( 'NONE',  ( -9.808193611224998776, -77.81204876761717060, 5.067887917229000116 ) ) ;
#39989 = CARTESIAN_POINT ( 'NONE',  ( -10.57271965826999960, -78.46022763255000143, -6.107801963966000613 ) ) ;
#39990 = ORIENTED_EDGE ( 'NONE', *, *, #32337, .T. ) ;
#39991 = EDGE_LOOP ( 'NONE', ( #10728, #38825, #52359, #38944 ) ) ;
#39992 = FACE_OUTER_BOUND ( 'NONE', #10894, .T. ) ;
#39993 = FACE_BOUND ( 'NONE', #915, .T. ) ;
#39994 = CARTESIAN_POINT ( 'NONE',  ( 1.137658753740000028, -79.55934817937600201, 0.6959227610743999870 ) ) ;
#39995 = CARTESIAN_POINT ( 'NONE',  ( 4.545264886168000729, -77.54575478459899784, 8.573871732259998879 ) ) ;
#39996 = CARTESIAN_POINT ( 'NONE',  ( -3.545429070608171696, -86.31452044229996545, 1.659291692407262930 ) ) ;
#39997 = CARTESIAN_POINT ( 'NONE',  ( 1.437416630538960405, -85.91103235223293666, 3.161135301328009906 ) ) ;
#39998 = CARTESIAN_POINT ( 'NONE',  ( -3.153993092687999766, -78.39994354880001026, 12.72742730875000028 ) ) ;
#39999 = CARTESIAN_POINT ( 'NONE',  ( -1.228039281160999918, -77.36163602614999490, -12.58161828305999919 ) ) ;
#40000 = CARTESIAN_POINT ( 'NONE',  ( 9.757498334186999855, -76.81312216313399688, 4.823034098846000539 ) ) ;
#40001 = CARTESIAN_POINT ( 'NONE',  ( -9.130570360603488922, -78.61295919940000942, -1.481171073185931109 ) ) ;
#40002 = CARTESIAN_POINT ( 'NONE',  ( -0.06039263125621000677, -80.01681542480598353, 4.129753795741000211 ) ) ;
#40003 = CARTESIAN_POINT ( 'NONE',  ( -10.38645071868999992, -59.57819125629999490, 7.655542440085000067 ) ) ;
#40004 = CARTESIAN_POINT ( 'NONE',  ( -2.301383562795737969, -3.038008897241404327, 2.294446131325794891 ) ) ;
#40005 = CARTESIAN_POINT ( 'NONE',  ( -3.178331792343999762, -80.25300264934799088, -1.569449204645999796 ) ) ;
#40006 = CARTESIAN_POINT ( 'NONE',  ( 11.22546153480763564, -77.52033577748665039, -4.386301564758395166 ) ) ;
#40007 = DIRECTION ( 'NONE',  ( 0.000000000000000000, 1.000000000000000000, 0.000000000000000000 ) ) ;
#40008 = CARTESIAN_POINT ( 'NONE',  ( 3.383845406481000406, -2.494828305427999826, -1.742318191517000070 ) ) ;
#40009 = CARTESIAN_POINT ( 'NONE',  ( -0.4078596229111138838, -80.15132319958321716, 1.208312492186587983 ) ) ;
#40010 = VERTEX_POINT ( 'NONE', #31291 ) ;
#40011 = DIRECTION ( 'NONE',  ( -1.000000000000000000, 0.000000000000000000, 0.000000000000000000 ) ) ;
#40012 = EDGE_CURVE ( 'NONE', #11615, #15713, #25451, .T. ) ;
#40013 = CARTESIAN_POINT ( 'NONE',  ( 11.00000000000000000, -77.44999999999998863, 0.000000000000000000 ) ) ;
#40014 = VECTOR ( 'NONE', #7723, 1000.000000000000000 ) ;
#40015 = CARTESIAN_POINT ( 'NONE',  ( -1.208084210770999922, -81.68708052363099625, 0.5648970606752000689 ) ) ;
#40016 = ADVANCED_FACE ( 'NONE', ( #7722 ), #21296, .F. ) ;
#40017 = CARTESIAN_POINT ( 'NONE',  ( 1.750000000000000000, -18.75000000000000000, -12.00000000000000000 ) ) ;
#40018 = CARTESIAN_POINT ( 'NONE',  ( -10.55511172854000002, -77.93295181317999720, 7.611100925114999249 ) ) ;
#40019 = CARTESIAN_POINT ( 'NONE',  ( -6.067803813374999855, -79.50066001420199768, 7.334714833394000877 ) ) ;
#40020 = CARTESIAN_POINT ( 'NONE',  ( 9.713030931998421380, -17.47705886690323140, 7.970419576809637974 ) ) ;
#40021 = EDGE_LOOP ( 'NONE', ( #2533, #7791, #17539, #57089, #7156, #57260 ) ) ;
#40022 = VECTOR ( 'NONE', #4552, 1000.000000000000000 ) ;
#40023 = CARTESIAN_POINT ( 'NONE',  ( -9.931063218460421282, -54.67724209132310875, 7.763994034062362992 ) ) ;
#40024 = CARTESIAN_POINT ( 'NONE',  ( 8.130813118348999780, -54.11476110100999648, -9.546856411313999757 ) ) ;
#40025 = EDGE_CURVE ( 'NONE', #1317, #10320, #54005, .T. ) ;
#40026 = CARTESIAN_POINT ( 'NONE',  ( -1.189940096281000059, -80.83713527995598724, -0.6468527390756999562 ) ) ;
#40027 = CARTESIAN_POINT ( 'NONE',  ( -9.596002108778160178, -78.95208333333330586, -7.374560639698984232 ) ) ;
#40028 = CARTESIAN_POINT ( 'NONE',  ( -1.922928979007999750, -77.56575641046499925, -9.325916353809999393 ) ) ;
#40029 = CARTESIAN_POINT ( 'NONE',  ( -3.413899980018999969, -86.06631758453399073, 2.398936571692999564 ) ) ;
#40030 = CARTESIAN_POINT ( 'NONE',  ( 1.092232985442820992, -82.29166666666665719, 0.6295237254636267821 ) ) ;
#40031 = CARTESIAN_POINT ( 'NONE',  ( -0.9676267263329999535, -80.53746333463699614, 1.036212325607999807 ) ) ;
#40032 = EDGE_LOOP ( 'NONE', ( #18436, #22626, #33621, #20324, #22691, #8916, #15236 ) ) ;
#40033 = CARTESIAN_POINT ( 'NONE',  ( -2.363548001580171309, -77.20752253318963199, -10.48685899165801416 ) ) ;
#40034 = CARTESIAN_POINT ( 'NONE',  ( 1.157617308350565644, -78.96545863123837705, 9.256449997036533262 ) ) ;
#40035 = CARTESIAN_POINT ( 'NONE',  ( -4.000000000000000000, -78.69999999915415856, 2.834003763004000336E-08 ) ) ;
#40036 = VERTEX_POINT ( 'NONE', #26573 ) ;
#40037 = ORIENTED_EDGE ( 'NONE', *, *, #52776, .F. ) ;
#40038 = CARTESIAN_POINT ( 'NONE',  ( -1.500000000366989328, -77.74999999999998579, 0.3141592638904139312 ) ) ;
#40039 = SURFACE_SIDE_STYLE ('',( #11747 ) ) ;
#40040 = CARTESIAN_POINT ( 'NONE',  ( 10.70231528814999855, -80.02182239623499527, 4.045645928379999923 ) ) ;
#40041 = VERTEX_POINT ( 'NONE', #57887 ) ;
#40042 = CARTESIAN_POINT ( 'NONE',  ( 4.484759669696999573, -77.53578839696798752, 11.18403784080000030 ) ) ;
#40043 = EDGE_CURVE ( 'NONE', #8704, #22042, #43633, .T. ) ;
#40044 = VERTEX_POINT ( 'NONE', #17443 ) ;
#40045 = ORIENTED_EDGE ( 'NONE', *, *, #24662, .F. ) ;
#40046 = DIRECTION ( 'NONE',  ( 0.000000000000000000, 1.000000000000000000, 0.000000000000000000 ) ) ;
#40047 = DIRECTION ( 'NONE',  ( -0.7071067811865954233, 0.7071067811864955033, 7.552239815522943575E-08 ) ) ;
#40048 = VECTOR ( 'NONE', #57531, 1000.000000000000000 ) ;
#40049 = VERTEX_POINT ( 'NONE', #35429 ) ;
#40050 = ORIENTED_EDGE ( 'NONE', *, *, #15855, .T. ) ;
#40051 = CARTESIAN_POINT ( 'NONE',  ( 1.268374697692444597, -79.90801042311336744, 0.1245783310639265173 ) ) ;
#40052 = CIRCLE ( 'NONE', #53255, 10.74999999999999822 ) ;
#40053 = CARTESIAN_POINT ( 'NONE',  ( 3.407095545933001457, -78.77851879815550262, -1.253608761936364502E-15 ) ) ;
#40054 = EDGE_CURVE ( 'NONE', #15436, #26860, #57127, .T. ) ;
#40055 = DIRECTION ( 'NONE',  ( 0.000000000000000000, -1.000000000000000000, 0.000000000000000000 ) ) ;
#40056 = CARTESIAN_POINT ( 'NONE',  ( -0.1577469407266123835, -18.24957415542316141, 11.00002392222777381 ) ) ;
#40057 = CARTESIAN_POINT ( 'NONE',  ( 11.75000000000000000, -77.45000000000000284, 1.043320980279999928E-14 ) ) ;
#40058 = CIRCLE ( 'NONE', #55167, 14.00000000000000000 ) ;
#40059 = CARTESIAN_POINT ( 'NONE',  ( -10.42531124908000173, -60.06485148440999922, -7.624341765471999821 ) ) ;
#40060 = CARTESIAN_POINT ( 'NONE',  ( -11.48784787867999846, -78.17288519146396197, -3.397854551190000461 ) ) ;
#40061 = CARTESIAN_POINT ( 'NONE',  ( 8.550487401031416468, -78.81900159872047595, -3.528449567620169702 ) ) ;
#40062 = CARTESIAN_POINT ( 'NONE',  ( -10.00844230537000001, -23.36891112553000127, 7.647097279392999880 ) ) ;
#40063 = CARTESIAN_POINT ( 'NONE',  ( 0.9218200799623741393, -80.07708333333333428, -1.199500263597268690 ) ) ;
#40064 = CARTESIAN_POINT ( 'NONE',  ( -1.152152900689999759, -81.33525264934799281, 4.012747624594999785 ) ) ;
#40065 = CARTESIAN_POINT ( 'NONE',  ( -4.471077175322999864, -77.90826001420199987, -8.802310476361999036 ) ) ;
#40066 = CARTESIAN_POINT ( 'NONE',  ( -1.500000000000000000, -83.34999999999999432, 0.000000000000000000 ) ) ;
#40067 = CARTESIAN_POINT ( 'NONE',  ( 0.000000000000000000, -81.99999999999998579, -7.000000000000000000 ) ) ;
#40068 = CARTESIAN_POINT ( 'NONE',  ( -1.666727925315000025, -23.19174481776000007, 12.50018462903999961 ) ) ;
#40069 = CARTESIAN_POINT ( 'NONE',  ( -12.50000000000000000, -55.54999999966999980, 0.000000000000000000 ) ) ;
#40070 = CARTESIAN_POINT ( 'NONE',  ( -2.858407197967999913, -79.99999999999998579, 8.797272775729998884 ) ) ;
#40071 = CARTESIAN_POINT ( 'NONE',  ( -3.387230649729000120, -1.584484372332999769, -1.285432911469999828 ) ) ;
#40072 = EDGE_CURVE ( 'NONE', #22104, #56774, #1260, .T. ) ;
#40073 = CARTESIAN_POINT ( 'NONE',  ( -2.858407197967999913, -79.75000000000000000, -8.797272775729998884 ) ) ;
#40075 = EDGE_CURVE ( 'NONE', #29038, #36778, #14469, .T. ) ;
#40074 = CARTESIAN_POINT ( 'NONE',  ( 1.505169111093489498, -81.09224709464676550, -0.1340111490899882907 ) ) ;
#40076 = CARTESIAN_POINT ( 'NONE',  ( -1.249999993052000047, -76.30000000069199473, -0.6999999993075000093 ) ) ;
#40077 = CARTESIAN_POINT ( 'NONE',  ( 1.980584515756000030, -55.53514849873000259, -12.76303204337999908 ) ) ;
#40078 = CARTESIAN_POINT ( 'NONE',  ( -7.601397897754999633, -55.55000000209000177, -10.07627163191000008 ) ) ;
#40079 = CARTESIAN_POINT ( 'NONE',  ( 6.261651594248000663, -77.70020226594600388, -8.942431733175999042 ) ) ;
#40080 = CARTESIAN_POINT ( 'NONE',  ( 2.284509925729999669, -77.73351832560599917, 12.06552085823000020 ) ) ;
#40081 = CARTESIAN_POINT ( 'NONE',  ( -0.3926218265389255779, -80.89583333333337123, 1.460959015002472494 ) ) ;
#40083 = CARTESIAN_POINT ( 'NONE',  ( 1.481171800329999844, -78.11983073899280328, 0.3241480609735999940 ) ) ;
#40082 = CARTESIAN_POINT ( 'NONE',  ( 0.9218200799623692543, -79.72291666666667709, 1.199500263597272687 ) ) ;
#40084 = CARTESIAN_POINT ( 'NONE',  ( 0.5132697287564000899, -81.91933951002999947, -1.623690596030999744 ) ) ;
#40085 = ORIENTED_EDGE ( 'NONE', *, *, #35001, .F. ) ;
#40086 = CARTESIAN_POINT ( 'NONE',  ( -0.7681833999686432657, -82.07291666666665719, -0.9995835529977258327 ) ) ;
#40087 = CARTESIAN_POINT ( 'NONE',  ( 7.584438660666999787, -79.44356212903799985, 9.203919974279001437 ) ) ;
#40088 = PRESENTATION_LAYER_ASSIGNMENT (  '', '', ( #23168 ) ) ;
#40089 = CARTESIAN_POINT ( 'NONE',  ( -9.167119855300001063, -80.12061390621509815, -6.180331023587999795 ) ) ;
#40090 = ADVANCED_FACE ( 'NONE', ( #4749 ), #27457, .T. ) ;
#40091 = B_SPLINE_CURVE_WITH_KNOTS ( 'NONE', 3,
 ( #42981, #39412, #2538, #25251, #7826, #43270, #16113, #16401, #34385, #52417, #25826, #43855, #57418, #16977, #23151, #21970, #57994, #177 ),
 .UNSPECIFIED., .F., .F.,
 ( 4, 2, 2, 2, 2, 2, 2, 2, 4 ),
 ( 0.000000000000000000, 0.1250000000000001110, 0.2500000000000001665, 0.3750000000000001665, 0.5000000000000001110, 0.6250000000000001110, 0.7500000000000001110, 0.8750000000000001110, 1.000000000000000000 ),
 .UNSPECIFIED. ) ;
#40092 = PLANE ( 'NONE',  #16284 ) ;
#40093 = CARTESIAN_POINT ( 'NONE',  ( 3.009949031611931947, -85.32916667478426120, -1.673658179043767458 ) ) ;
#40094 = CARTESIAN_POINT ( 'NONE',  ( 11.19180402071999936, -77.58921497497100006, 0.7494220128532999015 ) ) ;
#40095 = CARTESIAN_POINT ( 'NONE',  ( -12.76303204525000012, -60.06485147653999945, -1.980584515753000208 ) ) ;
#40096 = AXIS2_PLACEMENT_3D ( 'NONE', #11921, #29899, #58232 ) ;
#40097 = CARTESIAN_POINT ( 'NONE',  ( 9.078688998878000405, -79.10553623779898658, 3.126726393672000004 ) ) ;
#40098 = CARTESIAN_POINT ( 'NONE',  ( -1.214351151748000124, -1.533058083081000111, 3.496700174682000117 ) ) ;
#40099 = CARTESIAN_POINT ( 'NONE',  ( -2.865983266988000100, -79.30827256302897865, -9.351425617539000257 ) ) ;
#40100 = FACE_OUTER_BOUND ( 'NONE', #48685, .T. ) ;
#40101 = CARTESIAN_POINT ( 'NONE',  ( 1.980584515756000030, -18.73514849905999924, -12.76303204340999997 ) ) ;
#40102 = ORIENTED_EDGE ( 'NONE', *, *, #8548, .F. ) ;
#40103 = DIRECTION ( 'NONE',  ( 1.000000000000000000, 0.000000000000000000, 0.000000000000000000 ) ) ;
#40104 = CARTESIAN_POINT ( 'NONE',  ( -12.56594317982999875, -55.55000000504000468, 1.750000000000000000 ) ) ;
#40105 = CARTESIAN_POINT ( 'NONE',  ( 0.000000000000000000, -78.69999999999998863, 0.000000000000000000 ) ) ;
#40106 = CARTESIAN_POINT ( 'NONE',  ( -10.18491068058999893, -55.49283065365000311, -7.640030139739999449 ) ) ;
#40107 = CARTESIAN_POINT ( 'NONE',  ( -0.8981901762082999952, -79.96851006753000490, -1.403037214508999986 ) ) ;
#40108 = CARTESIAN_POINT ( 'NONE',  ( 9.369164850722000892, -18.75000000000000000, -7.601397897754999633 ) ) ;
#40109 = VERTEX_POINT ( 'NONE', #50505 ) ;
#40110 = LINE ( 'NONE', #22400, #18148 ) ;
#40111 = CARTESIAN_POINT ( 'NONE',  ( -11.75000000000000000, -77.70000000000000284, 0.000000000000000000 ) ) ;
#40112 = CARTESIAN_POINT ( 'NONE',  ( -2.062673488738000049, -23.32452529362999982, 12.82904091339000097 ) ) ;
#40113 = ORIENTED_EDGE ( 'NONE', *, *, #43777, .T. ) ;
#40114 = ORIENTED_EDGE ( 'NONE', *, *, #11634, .F. ) ;
#40115 = CARTESIAN_POINT ( 'NONE',  ( -12.80900240954000147, -58.55365779174999830, 1.930989144707000005 ) ) ;
#40116 = CARTESIAN_POINT ( 'NONE',  ( -7.624757993407000001, -54.99647951274999969, -10.47516388917000008 ) ) ;
#40117 = CARTESIAN_POINT ( 'NONE',  ( -0.5483576180056000116, -79.39037854631799007, -9.751923335751000010 ) ) ;
#40118 = VERTEX_POINT ( 'NONE', #32172 ) ;
#40119 = ORIENTED_EDGE ( 'NONE', *, *, #15903, .T. ) ;
#40120 = CARTESIAN_POINT ( 'NONE',  ( 3.079339082788000059, -77.26865414418398359, -11.84061610281999855 ) ) ;
#40121 = CARTESIAN_POINT ( 'NONE',  ( -10.75000000000000000, -78.60000000000000853, 0.000000000000000000 ) ) ;
#40122 = CARTESIAN_POINT ( 'NONE',  ( 0.9401231181983999985, -77.88411904209999648, -1.213240629208000243 ) ) ;
#40123 = ORIENTED_EDGE ( 'NONE', *, *, #9903, .F. ) ;
#40124 = CARTESIAN_POINT ( 'NONE',  ( -9.204193785523999694, -77.20990584965399250, -2.332437886131999871 ) ) ;
#40125 = ADVANCED_FACE ( 'NONE', ( #18039 ), #37195, .F. ) ;
#40126 = CARTESIAN_POINT ( 'NONE',  ( -8.073593340907574856, -78.39671052555694075, -5.384321531606748756 ) ) ;
#40127 = CARTESIAN_POINT ( 'NONE',  ( 1.157786043506160212, -80.31939170094496205, -0.4709745549768553086 ) ) ;
#40128 = DIRECTION ( 'NONE',  ( 0.000000000000000000, 0.000000000000000000, -1.000000000000000000 ) ) ;
#40129 = EDGE_CURVE ( 'NONE', #10450, #31238, #14175, .T. ) ;
#40130 = CARTESIAN_POINT ( 'NONE',  ( 11.08595418830999968, -76.98783056546687931, -1.708721840212999776 ) ) ;
#40131 = CARTESIAN_POINT ( 'NONE',  ( -13.13047446164998711, -22.78578169018998878, -0.8260994316375004365 ) ) ;
#40132 = CARTESIAN_POINT ( 'NONE',  ( -2.739132899390686049, -86.25171438276198899, 3.697400121254383887 ) ) ;
#40133 = CARTESIAN_POINT ( 'NONE',  ( -4.152600241220000044, -79.49650423252299447, -10.41988588363999924 ) ) ;
#40134 = VECTOR ( 'NONE', #5253, 1000.000000000000000 ) ;
#40135 = CARTESIAN_POINT ( 'NONE',  ( 6.953009658842218776, -79.90740165580891130, 6.100783007042114292 ) ) ;
#40136 = DIRECTION ( 'NONE',  ( 0.7071067811865475727, 0.000000000000000000, -0.7071067811865475727 ) ) ;
#40137 = ORIENTED_EDGE ( 'NONE', *, *, #36087, .F. ) ;
#40138 = CARTESIAN_POINT ( 'NONE',  ( 9.887211716164999942, -79.41060049144299171, 5.401109038458000278 ) ) ;
#40139 = CARTESIAN_POINT ( 'NONE',  ( 9.754023262367999436, -76.24978791229999331, -7.509630405475999915 ) ) ;
#40140 = CARTESIAN_POINT ( 'NONE',  ( -1.397510954313999854, -79.94980780150500266, -0.8088121278437000461 ) ) ;
#40141 = CARTESIAN_POINT ( 'NONE',  ( 0.5643133282633999714, -78.81822964757999728, -1.192525073705999805 ) ) ;
#40142 = CARTESIAN_POINT ( 'NONE',  ( -2.263164996904851289, -2.919503939068432530, -2.771219827481139042 ) ) ;
#40143 = CARTESIAN_POINT ( 'NONE',  ( -9.346058021984571695, -16.83471832412213232, 8.620905970628376380 ) ) ;
#40144 = CARTESIAN_POINT ( 'NONE',  ( 0.5999999999999999778, -18.84999999999999787, -10.98362417419999915 ) ) ;
#40145 = DIRECTION ( 'NONE',  ( 0.000000000000000000, 0.000000000000000000, -1.000000000000000000 ) ) ;
#40146 = CARTESIAN_POINT ( 'NONE',  ( 10.45148855949000044, -78.33539999468298731, 3.906137931512999817 ) ) ;
#40147 = CARTESIAN_POINT ( 'NONE',  ( 9.233773875527001351, -77.60363998579799727, -3.090294488178999988 ) ) ;
#40148 = CARTESIAN_POINT ( 'NONE',  ( -10.10912517723439841, -23.47586858184963532, -7.634643689412396128 ) ) ;
#40149 = CARTESIAN_POINT ( 'NONE',  ( -1.407171709420418138, -79.61458333333331439, -10.75000000000000000 ) ) ;
#40150 = DIRECTION ( 'NONE',  ( 0.000000000000000000, 0.000000000000000000, -1.000000000000000000 ) ) ;
#40151 = B_SPLINE_CURVE_WITH_KNOTS ( 'NONE', 3,
 ( #49933, #9477, #33642, #56100, #15645, #24213, #47256, #2088, #20086, #56386, #15058, #10943, #33052, #51100, #38078, #43103, #55511, #11802, #51682, #37787, #42520, #47552, #2373, #10651, #25079, #15936, #11520, #11230, #29209, #6788 ),
 .UNSPECIFIED., .F., .F.,
 ( 4, 2, 1, 1, 2, 2, 1, 2, 2, 2, 1, 1, 2, 2, 1, 2, 2, 4 ),
 ( 0.6954909650194412984, 0.7335545943920098733, 0.7430705017351519892, 0.7478284554067230472, 0.7490179438246158394, 0.7502074322425086317, 0.7525864090782941052, 0.7716182237645784481, 0.8477454825097158198, 0.8667772971960001627, 0.8715352508675713317, 0.8739142277033569162, 0.8745089719123033678, 0.8751037161212498194, 0.8762932045391426117, 0.8858091118822855048, 0.9238727412548570772, 1.000000000000000000 ),
 .UNSPECIFIED. ) ;
#40152 = ORIENTED_EDGE ( 'NONE', *, *, #30155, .F. ) ;
#40154 = EDGE_CURVE ( 'NONE', #28360, #30070, #14882, .T. ) ;
#40153 = CARTESIAN_POINT ( 'NONE',  ( 1.261625697157999992, -81.66390831549000495, -0.7514603626543999715 ) ) ;
#40155 = CARTESIAN_POINT ( 'NONE',  ( -11.44417895085270942, -77.82083333333333997, -3.075537641221545826 ) ) ;
#40156 = CARTESIAN_POINT ( 'NONE',  ( -12.00000000000000000, -18.75000000000000000, 0.000000000000000000 ) ) ;
#40157 = LINE ( 'NONE', #18027, #15449 ) ;
#40158 = FACE_OUTER_BOUND ( 'NONE', #30946, .T. ) ;
#40159 = CARTESIAN_POINT ( 'NONE',  ( 2.220279159302000149, -77.93669951884498914, 11.72628939184999908 ) ) ;
#40160 = CARTESIAN_POINT ( 'NONE',  ( 6.482950081930999531, -79.19664415034600324, -6.598019266050999754 ) ) ;
#40161 = CARTESIAN_POINT ( 'NONE',  ( -9.433548213854539455, -25.12797454612102754, -8.532643227186095913 ) ) ;
#40162 = CARTESIAN_POINT ( 'NONE',  ( 11.68767212001979594, -78.52916666666665435, -3.140974612311341563 ) ) ;
#40163 = CARTESIAN_POINT ( 'NONE',  ( -10.17265785211000129, -78.92724904577400480, 4.268344714933999917 ) ) ;
#40164 = FACE_OUTER_BOUND ( 'NONE', #16039, .T. ) ;
#40165 = ORIENTED_EDGE ( 'NONE', *, *, #3067, .F. ) ;
#40166 = CARTESIAN_POINT ( 'NONE',  ( -8.500869906239364227, -78.26250000000001705, 4.334382246026820873 ) ) ;
#40167 = CARTESIAN_POINT ( 'NONE',  ( -3.250000000000000000, -2.100000000000000089, 0.000000000000000000 ) ) ;
#40168 = CARTESIAN_POINT ( 'NONE',  ( -6.659468121095000193, -79.24723885956400693, 10.30708084445999972 ) ) ;
#40169 = CARTESIAN_POINT ( 'NONE',  ( -2.127490919130949454, -78.43735717367049176, -3.528455608958080525 ) ) ;
#40170 = ADVANCED_FACE ( 'NONE', ( #4456 ), #11621, .F. ) ;
#40171 = CARTESIAN_POINT ( 'NONE',  ( -1.519662023741000123, -82.86320165035199636, -0.6825586799200999977 ) ) ;
#40172 = CARTESIAN_POINT ( 'NONE',  ( 9.233664981878000333, -79.72560072109197904, 5.933249305785000871 ) ) ;
#40173 = EDGE_CURVE ( 'NONE', #9708, #41885, #22750, .T. ) ;
#40174 = LINE ( 'NONE', #21301, #43041 ) ;
#40175 = CARTESIAN_POINT ( 'NONE',  ( -7.771634306715999863, -77.01216573198799153, -9.645635764621999897 ) ) ;
#40176 = CARTESIAN_POINT ( 'NONE',  ( 3.150470485466851933, -78.55114870413540018, 11.31836463120567160 ) ) ;
#40177 = CARTESIAN_POINT ( 'NONE',  ( 26.50000000000000000, -39.30476017083000073, 1.155265119678999855E-13 ) ) ;
#40178 = ORIENTED_EDGE ( 'NONE', *, *, #31333, .T. ) ;
#40179 = CARTESIAN_POINT ( 'NONE',  ( 3.646964122112999807, -80.12495082227849252, 10.50067842184000000 ) ) ;
#40180 = CARTESIAN_POINT ( 'NONE',  ( -2.099388381696000023E-14, 0.000000000000000000, -12.69999999999999929 ) ) ;
#40181 = CARTESIAN_POINT ( 'NONE',  ( 9.370643039124985307, -75.80000000000003979, -7.368669060076848076 ) ) ;
#40182 = LINE ( 'NONE', #26890, #41040 ) ;
#40183 = APPLICATION_CONTEXT ( 'automotive_design' ) ;
#40184 = CARTESIAN_POINT ( 'NONE',  ( -9.663285910017000546, -79.20140313587198477, 5.577858467032999812 ) ) ;
#40185 = CARTESIAN_POINT ( 'NONE',  ( 8.035240866938423210, -76.30833333333333712, 7.229432123683737110 ) ) ;
#40186 = CARTESIAN_POINT ( 'NONE',  ( 0.000000000000000000, -76.39999999999999147, 0.000000000000000000 ) ) ;
#40187 = CARTESIAN_POINT ( 'NONE',  ( 9.687205842286999768, -78.02392362630298805, -7.546775612817000045 ) ) ;
#40188 = VECTOR ( 'NONE', #50143, 1000.000000000000114 ) ;
#40189 = ADVANCED_FACE ( 'NONE', ( #45495 ), #44596, .F. ) ;
#40190 = CIRCLE ( 'NONE', #2501, 0.2000000000000005107 ) ;
#40191 = CARTESIAN_POINT ( 'NONE',  ( -9.393203674808288994, -79.45833333333331439, 5.413904038987134015 ) ) ;
#40192 = CIRCLE ( 'NONE', #17572, 4.100000000000000533 ) ;
#40193 = DIRECTION ( 'NONE',  ( 1.000000000000000000, 0.000000000000000000, 0.000000000000000000 ) ) ;
#40194 = DIRECTION ( 'NONE',  ( -1.000000000000000000, 0.000000000000000000, 0.000000000000000000 ) ) ;
#40195 = ORIENTED_EDGE ( 'NONE', *, *, #13958, .T. ) ;
#40196 = VECTOR ( 'NONE', #8070, 1000.000000000000000 ) ;
#40197 = ORIENTED_EDGE ( 'NONE', *, *, #43625, .F. ) ;
#40198 = CARTESIAN_POINT ( 'NONE',  ( -9.723174507563001612, -61.27697503937000079, -7.958760295438001009 ) ) ;
#40199 = CARTESIAN_POINT ( 'NONE',  ( 6.844651340168000253, -76.88284666193300154, -6.485976721047999938 ) ) ;
#40200 = ORIENTED_EDGE ( 'NONE', *, *, #56315, .T. ) ;
#40201 = CARTESIAN_POINT ( 'NONE',  ( -7.421655993048999811, -78.47872433538000791, 9.763070719336001346 ) ) ;
#40202 = VERTEX_POINT ( 'NONE', #1212 ) ;
#40203 = CARTESIAN_POINT ( 'NONE',  ( 3.439647241017512069, -82.43854168378354075, -0.1699550553820542431 ) ) ;
#40204 = EDGE_CURVE ( 'NONE', #51850, #822, #52224, .T. ) ;
#40205 = ADVANCED_FACE ( 'NONE', ( #43098 ), #309, .T. ) ;
#40206 = CARTESIAN_POINT ( 'NONE',  ( -7.626500902235000545, -60.11584477251999203, 10.35747158364999976 ) ) ;
#40207 = CARTESIAN_POINT ( 'NONE',  ( -8.885605805125999623, -78.09673998579799559, 3.858414063430999796 ) ) ;
#40208 = CARTESIAN_POINT ( 'NONE',  ( -5.647686975130659981, -78.17275673027563698, -7.326454094270782313 ) ) ;
#40209 = CARTESIAN_POINT ( 'NONE',  ( 0.9578316561260999951, -78.83012074166400396, -11.17589679220000143 ) ) ;
#40210 = CARTESIAN_POINT ( 'NONE',  ( 1.114061420507061140, -79.38800613273430429, 0.5663899713086829601 ) ) ;
#40211 = ORIENTED_EDGE ( 'NONE', *, *, #30155, .T. ) ;
#40212 = ORIENTED_EDGE ( 'NONE', *, *, #24747, .T. ) ;
#40213 = CARTESIAN_POINT ( 'NONE',  ( 1.967341388825386339, -77.45803376817946173, 9.038427814231061674 ) ) ;
#40214 = CARTESIAN_POINT ( 'NONE',  ( -9.808193611224998776, -77.89219955680599128, 5.067887917229000116 ) ) ;
#40215 = CARTESIAN_POINT ( 'NONE',  ( -1.310679582531389498, -77.95833333333335702, 0.7554284705563444335 ) ) ;
#40216 = CARTESIAN_POINT ( 'NONE',  ( -7.456816947376000648, -78.83519289764198845, 6.210200510404999541 ) ) ;
#40217 = CARTESIAN_POINT ( 'NONE',  ( 12.23521718689999993, -76.14169869620000952, -4.290956967987999526 ) ) ;
#40218 = CARTESIAN_POINT ( 'NONE',  ( -8.376464375933499795, -79.43904992786433183, -4.482401383029819719 ) ) ;
#40219 = CARTESIAN_POINT ( 'NONE',  ( 12.80090744918999945, -56.03767312542999690, 1.980532734072999901 ) ) ;
#40220 = B_SPLINE_CURVE_WITH_KNOTS ( 'NONE', 3,
 ( #11728, #47753, #7288, #25288, #47474, #51308 ),
 .UNSPECIFIED., .F., .F.,
 ( 4, 2, 4 ),
 ( 0.000000000000000000, 0.5000000000000000000, 1.000000000000000000 ),
 .UNSPECIFIED. ) ;
#40221 = CARTESIAN_POINT ( 'NONE',  ( -4.017143116098000455, -80.39449815114798525, 10.51352533724000082 ) ) ;
#40222 = CARTESIAN_POINT ( 'NONE',  ( 12.43647099681000157, -17.08193128089000012, 0.03491583288331000234 ) ) ;
#40223 = CARTESIAN_POINT ( 'NONE',  ( 1.250000000000000222, -78.23958333333328596, -0.1636246173744659582 ) ) ;
#40224 = CARTESIAN_POINT ( 'NONE',  ( -1.243323288595322929, -79.18571856227184469, 9.501473710774742898 ) ) ;
#40225 = ORIENTED_EDGE ( 'NONE', *, *, #8627, .T. ) ;
#40226 = CARTESIAN_POINT ( 'NONE',  ( -5.117891248972000540, -79.85094018418639905, 10.91715234938999934 ) ) ;
#40227 = CARTESIAN_POINT ( 'NONE',  ( 1.549833839051000028, -76.27701249839499553, -11.26909137997999899 ) ) ;
#40228 = CARTESIAN_POINT ( 'NONE',  ( -6.833799251793511331, -78.02991085507407831, 8.298221944495866254 ) ) ;
#40229 = CARTESIAN_POINT ( 'NONE',  ( 3.249499231398999655, -78.78075334615299141, -11.53069031867000049 ) ) ;
#40230 = CARTESIAN_POINT ( 'NONE',  ( -10.08162962782999905, -17.28146287379999890, -7.981572332336000386 ) ) ;
#40231 = AXIS2_PLACEMENT_3D ( 'NONE', #52527, #30647, #3232 ) ;
#40233 = CARTESIAN_POINT ( 'NONE',  ( -1.890224871707000043, -18.25210751985000002, -12.68696160873999901 ) ) ;
#40232 = DIRECTION ( 'NONE',  ( 0.000000000000000000, -1.000000000000000000, 0.000000000000000000 ) ) ;
#40234 = DIRECTION ( 'NONE',  ( -0.9999999930530776293, 0.000000000000000000, -0.0001178721535688749008 ) ) ;
#40235 = CARTESIAN_POINT ( 'NONE',  ( 10.53101998745000145, -55.49360374314999689, -7.613962827161000035 ) ) ;
#40236 = FACE_OUTER_BOUND ( 'NONE', #40783, .T. ) ;
#40237 = CARTESIAN_POINT ( 'NONE',  ( 7.461283454533999659, -77.07449396308798839, -8.281536679888001018 ) ) ;
#40238 = CARTESIAN_POINT ( 'NONE',  ( -12.80088938717999980, -56.03743348177000172, 1.980532758767000301 ) ) ;
#40239 = CARTESIAN_POINT ( 'NONE',  ( 9.818658714980999846, -80.61406345225509540, 5.503422351864000639 ) ) ;
#40240 = CIRCLE ( 'NONE', #9145, 12.09999999999999964 ) ;
#40241 = ORIENTED_EDGE ( 'NONE', *, *, #7612, .T. ) ;
#40242 = CARTESIAN_POINT ( 'NONE',  ( 12.57042253521000141, -15.89905023022000030, 0.000000000000000000 ) ) ;
#40243 = CARTESIAN_POINT ( 'NONE',  ( 1.389926494652000022, -54.17618663712000426, 12.65988803918999928 ) ) ;
#40244 = FACE_OUTER_BOUND ( 'NONE', #29723, .T. ) ;
#40245 = CIRCLE ( 'NONE', #3491, 12.50000000000000000 ) ;
#40246 = CARTESIAN_POINT ( 'NONE',  ( 1.588974128205000058, -1.877812473829999940, -3.458412288513000199 ) ) ;
#40247 = CIRCLE ( 'NONE', #11987, 1.750000000000000666 ) ;
#40248 = CARTESIAN_POINT ( 'NONE',  ( 5.838193839761705917, -77.47708333333333997, -7.596835002782701629 ) ) ;
#40249 = EDGE_CURVE ( 'NONE', #33666, #4024, #33253, .T. ) ;
#40250 = CARTESIAN_POINT ( 'NONE',  ( -13.99999999961999819, -72.70000000038000110, 1.691901337660000028E-09 ) ) ;
#40251 = DIRECTION ( 'NONE',  ( -1.000000000000000000, 0.000000000000000000, 0.000000000000000000 ) ) ;
#40252 = CARTESIAN_POINT ( 'NONE',  ( 12.66313295597999833, -16.82196533882000011, -0.06049275240486999550 ) ) ;
#40253 = CARTESIAN_POINT ( 'NONE',  ( 2.242205298352999865, -85.40032450217400140, -3.468575908922999940 ) ) ;
#40254 = DIRECTION ( 'NONE',  ( 0.000000000000000000, -1.000000000000000000, 0.000000000000000000 ) ) ;
#40255 = CARTESIAN_POINT ( 'NONE',  ( 9.233489274360861643, -76.75868152203480577, 7.775098440744370620 ) ) ;
#40256 = CARTESIAN_POINT ( 'NONE',  ( -5.351850814891999875, -79.07833840369001166, 11.44861053826999964 ) ) ;
#40257 = CARTESIAN_POINT ( 'NONE',  ( 7.183928826236000376, -78.45794695701400201, -8.388570749380001246 ) ) ;
#40258 = CARTESIAN_POINT ( 'NONE',  ( 0.6820633866021539315, -81.92923038876949704, 1.047497107621460088 ) ) ;
#40259 = CARTESIAN_POINT ( 'NONE',  ( 1.343706126530000100, -78.02984880411999313, -0.9808119522502999343 ) ) ;
#40260 = CARTESIAN_POINT ( 'NONE',  ( 1.779623408287325015, -60.93630868986362259, 12.71471627660582193 ) ) ;
#40261 = CARTESIAN_POINT ( 'NONE',  ( 1.097245158776866569, -82.56172650200396390, 1.088114895880704092 ) ) ;
#40262 = DIRECTION ( 'NONE',  ( 0.9805806756909162258, 0.1961161351382035567, -2.366546780594040249E-11 ) ) ;
#40263 = CARTESIAN_POINT ( 'NONE',  ( 2.213099632718122045, -80.24184156219480712, -10.51960425961281587 ) ) ;
#40264 = CARTESIAN_POINT ( 'NONE',  ( 0.000000000000000000, -81.89999999962999766, -4.199999999630000147 ) ) ;
#40265 = CARTESIAN_POINT ( 'NONE',  ( -4.019865671108900251, -79.25407524574178808, 10.47197636312916735 ) ) ;
#40266 = EDGE_CURVE ( 'NONE', #13108, #35472, #49326, .T. ) ;
#40267 = CARTESIAN_POINT ( 'NONE',  ( 12.50000000000000000, -54.11640971901999819, -1.003652782195000093 ) ) ;
#40268 = ORIENTED_EDGE ( 'NONE', *, *, #23501, .T. ) ;
#40269 = CARTESIAN_POINT ( 'NONE',  ( 0.4820398299941640596, -81.75661953861411746, -1.153239258334429751 ) ) ;
#40270 = EDGE_CURVE ( 'NONE', #1025, #16006, #29491, .T. ) ;
#40271 = DIRECTION ( 'NONE',  ( 1.000000000000000000, 0.000000000000000000, 0.000000000000000000 ) ) ;
#40272 = CARTESIAN_POINT ( 'NONE',  ( 5.587778422887999419, -80.05792107344059616, -9.645275144704999803 ) ) ;
#40273 = CARTESIAN_POINT ( 'NONE',  ( 0.3271848554491016414, -80.14583333333330017, -1.217465845835393967 ) ) ;
#40274 = VERTEX_POINT ( 'NONE', #19490 ) ;
#40275 = ORIENTED_EDGE ( 'NONE', *, *, #53583, .T. ) ;
#40276 = CARTESIAN_POINT ( 'NONE',  ( -1.055696352445999908, -81.06023499620100381, -1.221768855801000253 ) ) ;
#40277 = ORIENTED_EDGE ( 'NONE', *, *, #26920, .F. ) ;
#40278 = CARTESIAN_POINT ( 'NONE',  ( 12.50000000000000000, -60.04999999966999980, 0.000000000000000000 ) ) ;
#40279 = VECTOR ( 'NONE', #31431, 1000.000000000000114 ) ;
#40280 = EDGE_LOOP ( 'NONE', ( #599, #56654 ) ) ;
#40281 = DIRECTION ( 'NONE',  ( 0.000000000000000000, -1.433672777923999722E-08, 0.9999999999999998890 ) ) ;
#40282 = LINE ( 'NONE', #9289, #37135 ) ;
#40283 = EDGE_CURVE ( 'NONE', #29318, #57022, #56403, .T. ) ;
#40284 = CARTESIAN_POINT ( 'NONE',  ( 9.221778727104000595, -79.34490324240999826, -6.054794091447999627 ) ) ;
#40285 = CARTESIAN_POINT ( 'NONE',  ( 1.933504092460000212, -23.40406847274999791, -12.70940235707999832 ) ) ;
#40286 = CARTESIAN_POINT ( 'NONE',  ( 3.542379078311999940, -81.33571061287598525, 1.250168379276000108 ) ) ;
#40287 = CARTESIAN_POINT ( 'NONE',  ( 1.488544850709269340, -79.26244586587921503, 9.382635476564523458 ) ) ;
#40288 = VERTEX_POINT ( 'NONE', #11515 ) ;
#40289 = DIRECTION ( 'NONE',  ( 0.7071067811863970265, -3.534300182982984496E-08, 0.7071067811866971198 ) ) ;
#40290 = CARTESIAN_POINT ( 'NONE',  ( 3.072533585156999703, -79.06378271215000098, -11.81724133653000131 ) ) ;
#40291 = EDGE_LOOP ( 'NONE', ( #37854, #27336, #6836, #46433 ) ) ;
#40292 = EDGE_LOOP ( 'NONE', ( #20387, #44727, #42255, #23863 ) ) ;
#40293 = CARTESIAN_POINT ( 'NONE',  ( 10.19999999921000011, -0.2000000007865999907, -1.811584077144999807E-09 ) ) ;
#40294 = CARTESIAN_POINT ( 'NONE',  ( 10.69999999997999929, -81.80000000002199556, -2.760617010408999913E-10 ) ) ;
#40295 = VECTOR ( 'NONE', #55011, 1000.000000000000000 ) ;
#40296 = CARTESIAN_POINT ( 'NONE',  ( -1.980611416589750817, -60.32597731777364203, -12.74335092665457303 ) ) ;
#40297 = CARTESIAN_POINT ( 'NONE',  ( 6.240531904507999883, -78.02895987979198367, 7.431451467605000083 ) ) ;
#40298 = AXIS2_PLACEMENT_3D ( 'NONE', #17048, #12330, #38900 ) ;
#40299 = CARTESIAN_POINT ( 'NONE',  ( 2.694001289665577392, -86.12610001270965654, -3.783547376761781322 ) ) ;
#40301 = EDGE_CURVE ( 'NONE', #1747, #10450, #55911, .T. ) ;
#40300 = CARTESIAN_POINT ( 'NONE',  ( 3.277027672054567908, -85.82457000994830310, 1.444457732302927733 ) ) ;
#40302 = CARTESIAN_POINT ( 'NONE',  ( 7.167851722631999323, -78.00376328549999982, -10.60335505485999974 ) ) ;
#40303 = CARTESIAN_POINT ( 'NONE',  ( -9.416026390438000604, -78.19420564057999457, 6.872484323511000248 ) ) ;
#40304 = EDGE_CURVE ( 'NONE', #50392, #14039, #5066, .T. ) ;
#40305 = CARTESIAN_POINT ( 'NONE',  ( 8.958556919380020744, -77.77414693750340291, -2.998186813234942072 ) ) ;
#40306 = CARTESIAN_POINT ( 'NONE',  ( 8.485281374238999419, -60.04999999966999980, -8.485281374238999419 ) ) ;
#40307 = CARTESIAN_POINT ( 'NONE',  ( -0.4143623072097000204, -80.85470891495099011, -3.941356880154000208 ) ) ;
#40308 = CARTESIAN_POINT ( 'NONE',  ( 12.60356226362999976, -19.24922971138999728, 1.750000000000000000 ) ) ;
#40309 = CARTESIAN_POINT ( 'NONE',  ( 0.000000000000000000, -46.09579702914000165, 0.000000000000000000 ) ) ;
#40310 = CARTESIAN_POINT ( 'NONE',  ( -3.410048246405999794, -78.60958598268121023, 0.4931512766838000439 ) ) ;
#40311 = DIRECTION ( 'NONE',  ( 0.000000000000000000, -1.000000000000000000, 0.000000000000000000 ) ) ;
#40312 = CARTESIAN_POINT ( 'NONE',  ( 0.1701061709968674784, -80.97413665117370840, 10.75656394733976029 ) ) ;
#40313 = CARTESIAN_POINT ( 'NONE',  ( -11.26045488449999965, -80.89932530880696504, 0.3336940576009999604 ) ) ;
#40314 = CARTESIAN_POINT ( 'NONE',  ( 3.702420020526000055, -2.551279764406999995, 0.8821385418971999792 ) ) ;
#40315 = CARTESIAN_POINT ( 'NONE',  ( 0.8766069548892785335, -79.43575010237100287, -0.9252077428013287808 ) ) ;
#40316 = ORIENTED_EDGE ( 'NONE', *, *, #20329, .T. ) ;
#40317 = CARTESIAN_POINT ( 'NONE',  ( 10.71369944335147828, -78.42916666666667425, -2.879226727952064913 ) ) ;
#40318 = LINE ( 'NONE', #49778, #50591 ) ;
#40319 = CARTESIAN_POINT ( 'NONE',  ( -0.2317941695893000198, -82.24449659242799271, -1.228320586388000013 ) ) ;
#40320 = CARTESIAN_POINT ( 'NONE',  ( -9.003615175678740812, -78.92666666666666231, -3.133420343058871627 ) ) ;
#40321 = CARTESIAN_POINT ( 'NONE',  ( -8.048032176077001054, -78.41399203484999703, 9.328081102756000220 ) ) ;
#40322 = CARTESIAN_POINT ( 'NONE',  ( -7.730443418336787609, -60.92191635792283222, -10.25197760567054317 ) ) ;
#40323 = CARTESIAN_POINT ( 'NONE',  ( 12.58338334669999981, -21.74800977511999989, -1.667961445601999992 ) ) ;
#40324 = ORIENTED_EDGE ( 'NONE', *, *, #42483, .T. ) ;
#40325 = CARTESIAN_POINT ( 'NONE',  ( -9.102117850481628025, -24.97186524166153276, -8.583692176905405091 ) ) ;
#40326 = B_SPLINE_CURVE_WITH_KNOTS ( 'NONE', 3,
 ( #43452, #42880, #47325, #6855, #2729, #24864, #43749, #11873, #39301, #3301 ),
 .UNSPECIFIED., .F., .F.,
 ( 4, 2, 2, 2, 4 ),
 ( 0.000000000000000000, 0.1250000000000000278, 0.2500000000000000555, 0.5000000000000000000, 1.000000000000000000 ),
 .UNSPECIFIED. ) ;
#40327 = CARTESIAN_POINT ( 'NONE',  ( -11.26138982850999959, -77.18296943548479305, -0.5357607033695001020 ) ) ;
#40328 = CONICAL_SURFACE ( 'NONE', #44081, 1.099999997157999232, 0.7853981633972997312 ) ;
#40329 = CARTESIAN_POINT ( 'NONE',  ( 0.7293115217919000637, -81.01790630965099638, -1.317947726832999988 ) ) ;
#40330 = CARTESIAN_POINT ( 'NONE',  ( 10.48543666025110355, -79.10833333333332007, -6.043427764450775008 ) ) ;
#40331 = CARTESIAN_POINT ( 'NONE',  ( -9.269208960685000775, -78.47531894259199703, -2.179940704506999616 ) ) ;
#40333 = CARTESIAN_POINT ( 'NONE',  ( -3.587712099295000012, -1.814945589986999952, 1.801380527025000067 ) ) ;
#40332 = CARTESIAN_POINT ( 'NONE',  ( 0.3110912592032999968, -82.61867690334500480, 4.118464764383999999 ) ) ;
#40334 = CARTESIAN_POINT ( 'NONE',  ( -2.062503053667999797, -57.04263462147999775, -12.92177931909999877 ) ) ;
#40335 = CARTESIAN_POINT ( 'NONE',  ( -0.7062052416310000691, -80.63092951705199596, -1.233256579520999763 ) ) ;
#40336 = EDGE_LOOP ( 'NONE', ( #11899, #18681, #9870, #8753 ) ) ;
#40337 = CARTESIAN_POINT ( 'NONE',  ( -4.710391155546546749, -77.18893069641463001, -9.663071856776335622 ) ) ;
#40338 = CARTESIAN_POINT ( 'NONE',  ( -11.75000000000000000, -78.20000000000000284, 1.702919296826999607E-14 ) ) ;
#40339 = AXIS2_PLACEMENT_3D ( 'NONE', #42750, #11175, #43039 ) ;
#40340 = CARTESIAN_POINT ( 'NONE',  ( -3.548349909811030045, -78.96264282632948550, 7.096699819622017458 ) ) ;
#40341 = B_SPLINE_CURVE_WITH_KNOTS ( 'NONE', 3,
 ( #39425, #21700, #30837, #16993 ),
 .UNSPECIFIED., .F., .F.,
 ( 4, 4 ),
 ( 0.000000000000000000, 1.000000000000000000 ),
 .UNSPECIFIED. ) ;
#40342 = ORIENTED_EDGE ( 'NONE', *, *, #13836, .T. ) ;
#40343 = ORIENTED_EDGE ( 'NONE', *, *, #8548, .T. ) ;
#40344 = CARTESIAN_POINT ( 'NONE',  ( 10.43959491470999978, -79.91030549489470047, -5.976816984917999953 ) ) ;
#40345 = DIRECTION ( 'NONE',  ( 0.9999999999998321343, 0.000000000000000000, 5.794540611356191117E-07 ) ) ;
#40346 = CARTESIAN_POINT ( 'NONE',  ( -7.987959636959824472, -80.44130578457811964, 7.262045713485346887 ) ) ;
#40347 = ORIENTED_EDGE ( 'NONE', *, *, #10820, .T. ) ;
#40348 = CARTESIAN_POINT ( 'NONE',  ( 4.400069678882000623, -77.34588318900199511, -11.21761009915999985 ) ) ;
#40349 = ORIENTED_EDGE ( 'NONE', *, *, #21338, .F. ) ;
#40350 = ORIENTED_EDGE ( 'NONE', *, *, #6832, .T. ) ;
#40351 = CARTESIAN_POINT ( 'NONE',  ( 7.664266801486627756, -60.54946977258676100, 7.892048199454674062 ) ) ;
#40352 = EDGE_CURVE ( 'NONE', #36547, #57912, #57849, .T. ) ;
#40353 = CARTESIAN_POINT ( 'NONE',  ( -3.140526010065456397, -76.50359585998626244, -11.68633867987707298 ) ) ;
#40354 = CARTESIAN_POINT ( 'NONE',  ( -4.373213035511999358, -79.83807026975351562, -8.733596771889999388 ) ) ;
#40355 = EDGE_LOOP ( 'NONE', ( #34150, #21750, #11398, #55390 ) ) ;
#40356 = CARTESIAN_POINT ( 'NONE',  ( -1.460777766812749734, -81.87926599238458891, 0.3927989208287778200 ) ) ;
#40357 = ORIENTED_EDGE ( 'NONE', *, *, #25865, .F. ) ;
#40358 = CARTESIAN_POINT ( 'NONE',  ( -1.263722992889853014, -80.63947858834744409, 0.1647592273877500069 ) ) ;
#40359 = CARTESIAN_POINT ( 'NONE',  ( 2.322889840689416285, -78.72610001270986402, -4.022071228304580082 ) ) ;
#40360 = CARTESIAN_POINT ( 'NONE',  ( -9.250000000000000000, -78.49999999999998579, 0.000000000000000000 ) ) ;
#40361 = DIRECTION ( 'NONE',  ( 0.000000000000000000, 1.000000000000000000, 0.000000000000000000 ) ) ;
#40362 = DIRECTION ( 'NONE',  ( 0.000000000000000000, 0.000000000000000000, -1.000000000000000000 ) ) ;
#40363 = CARTESIAN_POINT ( 'NONE',  ( 11.44417895085270054, -78.57083333333332575, 3.075537641221564922 ) ) ;
#40364 = EDGE_CURVE ( 'NONE', #1897, #53199, #22900, .T. ) ;
#40365 = CARTESIAN_POINT ( 'NONE',  ( 7.613962745591999592, -55.49360215019999742, -10.53101990617999917 ) ) ;
#40366 = DIRECTION ( 'NONE',  ( 0.000000000000000000, 1.000000000000000000, 0.000000000000000000 ) ) ;
#40367 = CARTESIAN_POINT ( 'NONE',  ( -10.19022265128000093, -23.19634105642999700, 7.646946115745000050 ) ) ;
#40368 = CARTESIAN_POINT ( 'NONE',  ( 0.000000000000000000, -87.20000000000000284, 0.000000000000000000 ) ) ;
#40369 = CARTESIAN_POINT ( 'NONE',  ( -1.439896632895359962, -78.48541666666665151, 10.99999999999999645 ) ) ;
#40370 = CARTESIAN_POINT ( 'NONE',  ( -3.128728754627999820, -81.81625264934800157, -2.764173162666000216 ) ) ;
#40371 = CARTESIAN_POINT ( 'NONE',  ( -7.364490753307999960, -77.76266001420199814, 6.575368940700000664 ) ) ;
#40372 = FACE_OUTER_BOUND ( 'NONE', #47714, .T. ) ;
#40373 = AXIS2_PLACEMENT_3D ( 'NONE', #11293, #42876, #6561 ) ;
#40374 = CARTESIAN_POINT ( 'NONE',  ( -6.760013919724099374, -78.02708333333333712, 8.796335266379958995 ) ) ;
#40375 = CARTESIAN_POINT ( 'NONE',  ( -1.582498447119000229, -24.15086122477999808, 12.55493832972999968 ) ) ;
#40376 = DIRECTION ( 'NONE',  ( -0.7071067811865474617, 0.7071067811865474617, 9.196891653921612702E-11 ) ) ;
#40377 = CARTESIAN_POINT ( 'NONE',  ( 2.575849577708000382, -83.78782518894399800, -2.439171769826999903 ) ) ;
#40378 = CARTESIAN_POINT ( 'NONE',  ( -2.982938763343999877, -2.003833096891999954, -1.417087710164999903 ) ) ;
#40379 = CARTESIAN_POINT ( 'NONE',  ( -1.369964363761594361, -82.06635564470731481, -0.4827857119653679030 ) ) ;
#40380 = CARTESIAN_POINT ( 'NONE',  ( -1.498818208256021745, -80.83919939903495333, 0.1937138382002916992 ) ) ;
#40381 = CARTESIAN_POINT ( 'NONE',  ( 12.77568181207000109, -62.06511628600999586, -0.5294980821349999367 ) ) ;
#40382 = CARTESIAN_POINT ( 'NONE',  ( -0.6549273519428999712, -79.31629276448599342, 1.475891481164999908 ) ) ;
#40383 = EDGE_CURVE ( 'NONE', #12786, #53705, #31814, .T. ) ;
#40384 = CARTESIAN_POINT ( 'NONE',  ( -3.535896000267000350, -77.42783883592798588, 10.32825277893000226 ) ) ;
#40385 = PRODUCT ( 'Battery', 'Battery', '', ( #46197 ) ) ;
#40386 = CARTESIAN_POINT ( 'NONE',  ( 4.527593368978999777, -77.28578839696798752, 11.29085598690000047 ) ) ;
#40387 = CARTESIAN_POINT ( 'NONE',  ( 0.5999999999999999778, -5.200000000000000178, -4.000000000000000000 ) ) ;
#40389 = CARTESIAN_POINT ( 'NONE',  ( 0.6485435286463999693, -79.01285795985199911, -1.370523042014000215 ) ) ;
#40388 = CARTESIAN_POINT ( 'NONE',  ( 1.500000000000000000, -79.65000000000000568, 0.000000000000000000 ) ) ;
#40390 = CARTESIAN_POINT ( 'NONE',  ( -1.388458563311000038, -81.66654517592999696, 0.7658850185041000680 ) ) ;
#40391 = EDGE_LOOP ( 'NONE', ( #45601, #3449, #43128, #15040 ) ) ;
#40392 = CARTESIAN_POINT ( 'NONE',  ( -0.7077633922091999263, -84.67496544543098480, 3.689232043295000096 ) ) ;
#40393 = CARTESIAN_POINT ( 'NONE',  ( -6.333362933179000009, -79.20385945140999695, -10.10566012912000033 ) ) ;
#40394 = CARTESIAN_POINT ( 'NONE',  ( -10.92553478716000015, -80.08564122021149956, -1.692710837394999945 ) ) ;
#40395 = CARTESIAN_POINT ( 'NONE',  ( -1.164828128805999992E-14, -72.79999999999999716, -13.89999999999999858 ) ) ;
#40396 = DIRECTION ( 'NONE',  ( 0.000000000000000000, 1.000000000000000000, 0.000000000000000000 ) ) ;
#40397 = CARTESIAN_POINT ( 'NONE',  ( 10.79417609527999922, -77.56197863196899789, -3.050225076229999832 ) ) ;
#40398 = CARTESIAN_POINT ( 'NONE',  ( -10.01676948373999920, -60.00938276551000428, 7.658894993385999328 ) ) ;
#40399 = CARTESIAN_POINT ( 'NONE',  ( -9.055195227533998192, -78.85919638534799958, -3.586521308946000186 ) ) ;
#40400 = CARTESIAN_POINT ( 'NONE',  ( 8.913248419499998576, -76.94780122596999661, -7.987006294937000206 ) ) ;
#40401 = CARTESIAN_POINT ( 'NONE',  ( -5.489373150238907151, -76.38659796104998634, -10.46729459822925534 ) ) ;
#40402 = CARTESIAN_POINT ( 'NONE',  ( 12.49989425040000057, -23.19225390461999936, -1.666425739591000044 ) ) ;
#40403 = CARTESIAN_POINT ( 'NONE',  ( -2.062673488410000200, -55.47547726255000100, 12.82904109059999875 ) ) ;
#40404 = ORIENTED_EDGE ( 'NONE', *, *, #17231, .F. ) ;
#40405 = DIRECTION ( 'NONE',  ( 0.000000000000000000, -1.000000000000000000, 0.000000000000000000 ) ) ;
#40406 = CARTESIAN_POINT ( 'NONE',  ( 5.809344757335999532, -79.51591332859899808, 7.547947145431999516 ) ) ;
#40407 = VECTOR ( 'NONE', #3844, 1000.000000000000000 ) ;
#40408 = CARTESIAN_POINT ( 'NONE',  ( 1.064406907239667577, -1.752651614945672565, -3.099959123880238199 ) ) ;
#40409 = CARTESIAN_POINT ( 'NONE',  ( -0.7554284705563483193, -81.48333333333334849, -1.310679582531387721 ) ) ;
#40410 = CARTESIAN_POINT ( 'NONE',  ( 0.2672206133491000224, -82.78817953870900226, 3.537394210971000152 ) ) ;
#40411 = EDGE_LOOP ( 'NONE', ( #8237, #22260, #56336, #31473 ) ) ;
#40412 = FACE_OUTER_BOUND ( 'NONE', #10439, .T. ) ;
#40413 = CARTESIAN_POINT ( 'NONE',  ( -11.75358435535890500, -77.70973593635036991, -1.536616025939224306 ) ) ;
#40414 = CARTESIAN_POINT ( 'NONE',  ( -1.668607604520085719, -55.00618368707833383, -12.52787843847536919 ) ) ;
#40415 = EDGE_LOOP ( 'NONE', ( #29667, #56325, #25399, #53126 ) ) ;
#40416 = ORIENTED_EDGE ( 'NONE', *, *, #7612, .F. ) ;
#40417 = MECHANICAL_DESIGN_GEOMETRIC_PRESENTATION_REPRESENTATION (  '', ( #21528 ), #9287 ) ;
#40418 = CARTESIAN_POINT ( 'NONE',  ( -9.996785040876998707, -54.64937852858999889, -7.758588586516999008 ) ) ;
#40419 = EDGE_CURVE ( 'NONE', #27418, #28917, #22629, .T. ) ;
#40420 =( LENGTH_UNIT ( ) NAMED_UNIT ( * ) SI_UNIT ( .MILLI., .METRE. ) );
#40421 = CARTESIAN_POINT ( 'NONE',  ( 5.496668217546000434, -80.00271666237398449, -8.073860231047000013 ) ) ;
#40422 = ORIENTED_EDGE ( 'NONE', *, *, #55095, .F. ) ;
#40423 = ORIENTED_EDGE ( 'NONE', *, *, #52390, .F. ) ;
#40424 = CARTESIAN_POINT ( 'NONE',  ( -3.182876184981000112, -77.29539847029199962, -11.93563171605999962 ) ) ;
#40425 = CARTESIAN_POINT ( 'NONE',  ( -0.5999999999999999778, -5.000000000000000000, -0.5999999999999999778 ) ) ;
#40426 = ADVANCED_FACE ( 'NONE', ( #44237 ), #19423, .F. ) ;
#40427 = CARTESIAN_POINT ( 'NONE',  ( -1.196135072002999955, -78.20959357977000082, 1.134084288239000093 ) ) ;
#40428 = ORIENTED_EDGE ( 'NONE', *, *, #4905, .F. ) ;
#40429 = CARTESIAN_POINT ( 'NONE',  ( 7.430757984336000099, -77.43352694988499252, 5.911115298933000695 ) ) ;
#40430 = CARTESIAN_POINT ( 'NONE',  ( 0.6031251352556811218, -80.26544605463739401, -1.094772290821791838 ) ) ;
#40431 = CARTESIAN_POINT ( 'NONE',  ( 5.623102978484999959, -77.33411282133998554, 11.84678905512000036 ) ) ;
#40432 = CYLINDRICAL_SURFACE ( 'NONE', #50460, 4.000000000000000000 ) ;
#40433 = CARTESIAN_POINT ( 'NONE',  ( -3.165820273081705327, -86.25171435493598437, 1.338596575002905409 ) ) ;
#40434 = CARTESIAN_POINT ( 'NONE',  ( 2.179295889402999897, -78.76112297147399488, 11.00312592022000047 ) ) ;
#40435 = B_SPLINE_CURVE_WITH_KNOTS ( 'NONE', 3,
 ( #12632, #43081, #2640, #24775, #53081, #20633, #57219, #29754, #43653, #43939, #38635, #42788, #56653, #56937, #33902, #2352, #16209, #34187 ),
 .UNSPECIFIED., .F., .F.,
 ( 4, 2, 2, 2, 2, 2, 2, 2, 4 ),
 ( 0.000000000000000000, 0.1250000000000000000, 0.2500000000000000000, 0.3750000000000000000, 0.5000000000000000000, 0.6250000000000000000, 0.7500000000000000000, 0.8750000000000000000, 1.000000000000000000 ),
 .UNSPECIFIED. ) ;
#40436 = CARTESIAN_POINT ( 'NONE',  ( 8.132368178600600572, -79.89002859466290829, 4.407339140889335205 ) ) ;
#40437 = ADVANCED_FACE ( 'NONE', ( #27084 ), #17069, .T. ) ;
#40438 = CARTESIAN_POINT ( 'NONE',  ( -4.097768037502161675, -80.35541789187665529, 10.32471114121541866 ) ) ;
#40439 = EDGE_LOOP ( 'NONE', ( #29103, #38460, #57165, #24525 ) ) ;
#40440 = DIRECTION ( 'NONE',  ( 0.000000000000000000, -1.000000000000000000, 0.000000000000000000 ) ) ;
#40441 = CARTESIAN_POINT ( 'NONE',  ( 2.878446107591830394, -77.25035309939079298, -8.790621935832806599 ) ) ;
#40442 = CARTESIAN_POINT ( 'NONE',  ( -0.2833792192578999947, -80.29709616517300219, 1.589625787444000071 ) ) ;
#40443 = VECTOR ( 'NONE', #13999, 1000.000000000000000 ) ;
#40444 = CARTESIAN_POINT ( 'NONE',  ( 1.154392285689999742, -78.86784227096099187, -0.6387050628028000387 ) ) ;
#40445 = CARTESIAN_POINT ( 'NONE',  ( 3.189660922236018603, -2.561412939622563112, -1.629070403506577724 ) ) ;
#40446 = VECTOR ( 'NONE', #41324, 1000.000000000000000 ) ;
#40447 = DIRECTION ( 'NONE',  ( 0.000000000000000000, 1.000000000000000000, 0.000000000000000000 ) ) ;
#40448 = CARTESIAN_POINT ( 'NONE',  ( -11.80208112487999905, -77.22397935580299588, -3.396125071686999952 ) ) ;
#40449 = CARTESIAN_POINT ( 'NONE',  ( -8.666912951892083328, -61.79291380850746407, -9.019442092672255384 ) ) ;
#40450 = CARTESIAN_POINT ( 'NONE',  ( 6.772004377195999680, -77.13018832859900442, -6.844728052047999611 ) ) ;
#40451 = CARTESIAN_POINT ( 'NONE',  ( 3.717789071696637304, -76.90015469873267762, 11.48706906119333304 ) ) ;
#40452 = CARTESIAN_POINT ( 'NONE',  ( -1.165193207555734078, -83.07060353884618564, 0.4526761131825299822 ) ) ;
#40453 = DIRECTION ( 'NONE',  ( 0.000000000000000000, 1.000000000000000000, 0.000000000000000000 ) ) ;
#40454 = CARTESIAN_POINT ( 'NONE',  ( -6.606377239730371720, -77.92708333333332860, 8.596418555780411808 ) ) ;
#40455 = VERTEX_POINT ( 'NONE', #17655 ) ;
#40456 = CARTESIAN_POINT ( 'NONE',  ( -0.5277720668919000380, -82.29534299292998867, 1.495277019118000039 ) ) ;
#40457 = CARTESIAN_POINT ( 'NONE',  ( 1.092255414008205028, -78.80861679417924393, -0.6293616401131961746 ) ) ;
#40458 = CARTESIAN_POINT ( 'NONE',  ( 1.250000000000000000, -79.84999999999999432, 0.000000000000000000 ) ) ;
#40459 = VECTOR ( 'NONE', #16731, 1000.000000000000000 ) ;
#40460 = DIRECTION ( 'NONE',  ( 0.000000000000000000, 1.000000000000000000, 0.000000000000000000 ) ) ;
#40461 = DIRECTION ( 'NONE',  ( -1.000000000000000000, 0.000000000000000000, 0.000000000000000000 ) ) ;
#40462 = AXIS2_PLACEMENT_3D ( 'NONE', #5442, #49756, #50043 ) ;
#40463 = CARTESIAN_POINT ( 'NONE',  ( -4.725986768004000638, -78.66919103528699964, -10.95903971673999955 ) ) ;
#40464 = CARTESIAN_POINT ( 'NONE',  ( -0.6471704932797999188, -77.95024805011499325, 9.701898969124000516 ) ) ;
#40465 = CARTESIAN_POINT ( 'NONE',  ( 1.477284502223000118, -54.07368499670000261, -12.77254812464999922 ) ) ;
#40466 = CARTESIAN_POINT ( 'NONE',  ( 8.313575899745858422, -76.01186070635600345, 8.302913058421760084 ) ) ;
#40467 = CARTESIAN_POINT ( 'NONE',  ( 1.984688374631000007, -80.16613885926460625, -10.73482082212999877 ) ) ;
#40468 = CARTESIAN_POINT ( 'NONE',  ( -0.5731199659188778162, -86.10000000000000853, 4.609165628485354382 ) ) ;
#40469 = ORIENTED_EDGE ( 'NONE', *, *, #11263, .T. ) ;
#40470 = CARTESIAN_POINT ( 'NONE',  ( -1.771468677314999907, -75.93649240829408598, 12.18184739844999420 ) ) ;
#40471 = CARTESIAN_POINT ( 'NONE',  ( -3.474812103689401965, -78.54828564506388489, -1.963390115445670991 ) ) ;
#40472 = CARTESIAN_POINT ( 'NONE',  ( 9.981840466370998755, -78.71427596511499303, 4.563647388395000171 ) ) ;
#40473 = CARTESIAN_POINT ( 'NONE',  ( -11.00000000000000000, -79.11041666666666572, -1.439896632895321327 ) ) ;
#40474 = CARTESIAN_POINT ( 'NONE',  ( 12.14319089506000005, -76.64257676113498974, 2.982765578692999853 ) ) ;
#40475 = FACE_OUTER_BOUND ( 'NONE', #13143, .T. ) ;
#40476 = CARTESIAN_POINT ( 'NONE',  ( -10.07979664880000037, -76.97175206120299151, 3.736335038366999761 ) ) ;
#40477 = ORIENTED_EDGE ( 'NONE', *, *, #8560, .T. ) ;
#40478 = EDGE_CURVE ( 'NONE', #20614, #17190, #32315, .T. ) ;
#40479 = CARTESIAN_POINT ( 'NONE',  ( 4.624113774747000249, -78.86790344678600206, -10.14259199460999916 ) ) ;
#40480 = CARTESIAN_POINT ( 'NONE',  ( 7.910248556510421025, -77.20622010308966310, -4.849172256848496509 ) ) ;
#40481 = CARTESIAN_POINT ( 'NONE',  ( 6.227934374241346660, -75.79999999999999716, -10.14191869714119676 ) ) ;
#40483 = CARTESIAN_POINT ( 'NONE',  ( 3.073856691126545915, -76.34527577747576288, -11.36762008860266171 ) ) ;
#40482 = CARTESIAN_POINT ( 'NONE',  ( -0.05337949040085999963, -80.77983644895500959, -1.318251307669999983 ) ) ;
#40484 = CARTESIAN_POINT ( 'NONE',  ( 5.365758882164000099, -78.14158470334899675, 9.658494679878000255 ) ) ;
#40485 = CARTESIAN_POINT ( 'NONE',  ( 4.392572548563236090, -76.34166666666665435, 9.875985572401184243 ) ) ;
#40486 = CARTESIAN_POINT ( 'NONE',  ( 0.6050660503295083315, -81.50719947809898258, -1.386332957043676428 ) ) ;
#40487 = AXIS2_PLACEMENT_3D ( 'NONE', #3083, #30210, #52955 ) ;
#40488 = DIRECTION ( 'NONE',  ( 0.000000000000000000, 1.000000000000000000, 0.000000000000000000 ) ) ;
#40489 = CARTESIAN_POINT ( 'NONE',  ( -1.210822168571097146, -79.88541666666665719, 9.249999999999992895 ) ) ;
#40490 = CARTESIAN_POINT ( 'NONE',  ( -6.272971974831352604, -79.62293377770998859, 9.114735501174530796 ) ) ;
#40491 = CARTESIAN_POINT ( 'NONE',  ( -12.43640309385000009, -24.91747517602999906, -0.05224034426415000154 ) ) ;
#40492 = EDGE_LOOP ( 'NONE', ( #44199, #42236, #6010, #44605, #45965, #46252, #46127, #26457, #11884, #32203, #44028 ) ) ;
#40493 = EDGE_LOOP ( 'NONE', ( #5082, #50755, #49816, #50365 ) ) ;
#40494 = CARTESIAN_POINT ( 'NONE',  ( 2.486604901413172808, -78.54583333333330586, -9.252740428348992907 ) ) ;
#40495 = EDGE_CURVE ( 'NONE', #15896, #10446, #54268, .T. ) ;
#40496 = CARTESIAN_POINT ( 'NONE',  ( -3.579650252175000436, -77.53493998579799040, 8.845718151729000667 ) ) ;
#40497 = CIRCLE ( 'NONE', #24457, 11.44999999999999929 ) ;
#40498 = VERTEX_POINT ( 'NONE', #13209 ) ;
#40499 = CARTESIAN_POINT ( 'NONE',  ( -7.255724684302470529, -79.80670072624305078, -6.257106228078864518 ) ) ;
#40500 = ORIENTED_EDGE ( 'NONE', *, *, #26750, .F. ) ;
#40501 = CARTESIAN_POINT ( 'NONE',  ( 7.645391636765999976, -23.21530450358000053, 10.18949673576000059 ) ) ;
#40502 = CARTESIAN_POINT ( 'NONE',  ( -4.570437647871999687, -78.05012939816998596, 10.04055945087000090 ) ) ;
#40503 = CIRCLE ( 'NONE', #44249, 2.799999999999999822 ) ;
#40504 = LINE ( 'NONE', #34393, #6105 ) ;
#40505 = CARTESIAN_POINT ( 'NONE',  ( -0.6521978219530000231, -78.07341332859900263, 9.777264943591001511 ) ) ;
#40506 = CARTESIAN_POINT ( 'NONE',  ( -5.862706933886596694, -78.17042577989984409, -7.154751683068700352 ) ) ;
#40507 = CARTESIAN_POINT ( 'NONE',  ( 10.05828973332000054, -78.91182977066900150, -4.964767691657000270 ) ) ;
#40508 = CARTESIAN_POINT ( 'NONE',  ( 3.699382908057097907, -81.00000000000004263, 10.19579882665893322 ) ) ;
#40509 = EDGE_CURVE ( 'NONE', #6488, #22487, #58391, .T. ) ;
#40510 = ORIENTED_EDGE ( 'NONE', *, *, #25781, .T. ) ;
#40511 = ORIENTED_EDGE ( 'NONE', *, *, #2589, .T. ) ;
#40512 = CARTESIAN_POINT ( 'NONE',  ( 6.771057570713677976, -77.40985474823717993, 6.320815176807171198 ) ) ;
#40513 = CARTESIAN_POINT ( 'NONE',  ( -11.00724581733999941, -77.86370633980098432, 0.8512868710715000287 ) ) ;
#40514 = EDGE_CURVE ( 'NONE', #48338, #19028, #21781, .T. ) ;
#40515 = DIRECTION ( 'NONE',  ( 0.7071067811865475727, 0.000000000000000000, -0.7071067811865475727 ) ) ;
#40516 = CARTESIAN_POINT ( 'NONE',  ( 8.898653440358000211, -78.60780226460998676, -3.871004561473999850 ) ) ;
#40517 = CARTESIAN_POINT ( 'NONE',  ( 11.97191554488999898, -76.11037712840000324, 4.552639408432999524 ) ) ;
#40518 = CARTESIAN_POINT ( 'NONE',  ( -8.539857470955180219, -79.43608207363838858, -4.162491799772078949 ) ) ;
#40519 = CARTESIAN_POINT ( 'NONE',  ( 9.164374456753368037, -53.58432317374141007, -8.803712804513708079 ) ) ;
#40520 = CARTESIAN_POINT ( 'NONE',  ( -4.417524307039417231, -79.38740258211193179, -8.447129840749521890 ) ) ;
#40521 = CARTESIAN_POINT ( 'NONE',  ( 12.83677071377000090, -18.77261389757000032, -2.062839858857999698 ) ) ;
#40522 = CARTESIAN_POINT ( 'NONE',  ( 0.9995835529977264988, -78.19791666666665719, -0.7681833999686417114 ) ) ;
#40523 = CARTESIAN_POINT ( 'NONE',  ( -10.84553603787253095, -76.66823218638354831, 4.520140657707524490 ) ) ;
#40524 = CARTESIAN_POINT ( 'NONE',  ( -2.293836348570999828, -84.30218271708000088, 2.760807823936999750 ) ) ;
#40525 = VERTEX_POINT ( 'NONE', #49846 ) ;
#40526 = CARTESIAN_POINT ( 'NONE',  ( 10.43594335123000150, -79.16914397480000787, 6.758781668662000364 ) ) ;
#40527 = CARTESIAN_POINT ( 'NONE',  ( 11.00455182153999978, -76.34027708591699479, 2.368156917827000107 ) ) ;
#40528 = CARTESIAN_POINT ( 'NONE',  ( -5.986584471844802025, -78.02217473519631596, 8.928664031516637678 ) ) ;
#40529 = CARTESIAN_POINT ( 'NONE',  ( 11.81379047889000056, -77.46494681281700423, 1.987564636421000008 ) ) ;
#40530 = CARTESIAN_POINT ( 'NONE',  ( -10.52682159591000044, -18.57432398260000284, 7.605688676868000542 ) ) ;
#40531 = DIRECTION ( 'NONE',  ( 0.000000000000000000, 0.1122098755727947705, -0.9936845293270585300 ) ) ;
#40532 = EDGE_CURVE ( 'NONE', #10595, #20949, #27380, .T. ) ;
#40533 = DIRECTION ( 'NONE',  ( -0.7071067812094172789, -2.924114042631071410E-07, -0.7071067811636172484 ) ) ;
#40534 = CARTESIAN_POINT ( 'NONE',  ( 4.048470932312206116, -80.94447786405585532, 9.958435342381811495 ) ) ;
#40535 = CARTESIAN_POINT ( 'NONE',  ( 0.7438124352902001357, -80.49061853915497977, 11.37744605582999924 ) ) ;
#40536 = CARTESIAN_POINT ( 'NONE',  ( 2.486604901413172364, -78.44583333333333997, -9.252740428348998236 ) ) ;
#40537 = CARTESIAN_POINT ( 'NONE',  ( -0.8202502003661999996, -77.51027545111699624, -11.11673469052999863 ) ) ;
#40538 = CARTESIAN_POINT ( 'NONE',  ( 3.250000000000000000, -1.750000000000000000, 0.000000000000000000 ) ) ;
#40539 = CARTESIAN_POINT ( 'NONE',  ( 4.185745002111000090, -80.73548588867527087, 10.32456989385000057 ) ) ;
#40540 = VERTEX_POINT ( 'NONE', #44816 ) ;
#40541 = LINE ( 'NONE', #44975, #30095 ) ;
#40542 = CARTESIAN_POINT ( 'NONE',  ( 0.5506765233279000693, -53.54045707723000191, 12.77514798307000099 ) ) ;
#40543 = CARTESIAN_POINT ( 'NONE',  ( -1.667260628937999867, -60.00942012442000362, -12.49858003896999925 ) ) ;
#40544 = CARTESIAN_POINT ( 'NONE',  ( -3.420922791951000352, -1.780913946619999910, 1.097631908065999973 ) ) ;
#40545 = CARTESIAN_POINT ( 'NONE',  ( 6.201912463541000342, -78.43838330275499970, -9.171216270948999494 ) ) ;
#40546 = CARTESIAN_POINT ( 'NONE',  ( -0.4631590389519466555, -79.50102817191933013, -1.469247881823791957 ) ) ;
#40547 = AXIS2_PLACEMENT_3D ( 'NONE', #4470, #17457, #35444 ) ;
#40548 = CARTESIAN_POINT ( 'NONE',  ( -3.165411199172024848, -1.520833333333333259, -0.8506806241676611036 ) ) ;
#40549 = CARTESIAN_POINT ( 'NONE',  ( 3.636872000734241883, -82.55416664812710792, 1.696597269464540814 ) ) ;
#40550 = CARTESIAN_POINT ( 'NONE',  ( -1.814305421036000121, -61.08941969298000174, 12.78003582256000215 ) ) ;
#40551 = CARTESIAN_POINT ( 'NONE',  ( -10.07627163191000008, -60.04999999725999515, -7.601397897754999633 ) ) ;
#40552 = EDGE_CURVE ( 'NONE', #52990, #18080, #39864, .T. ) ;
#40553 = CIRCLE ( 'NONE', #49960, 1.750000000000000000 ) ;
#40554 = CARTESIAN_POINT ( 'NONE',  ( 0.2926784520318999605, -85.14824735065198524, -4.164605519011000290 ) ) ;
#40555 = CARTESIAN_POINT ( 'NONE',  ( -11.75000000000000000, -76.04999999999999716, -3.652443742841000169E-09 ) ) ;
#40556 = ADVANCED_FACE ( 'NONE', ( #57799 ), #28580, .F. ) ;
#40557 = CARTESIAN_POINT ( 'NONE',  ( 2.615203195289000249, -78.85319526808000035, 12.68173180764000030 ) ) ;
#40558 = CARTESIAN_POINT ( 'NONE',  ( -6.940497389897999803, -77.13734811451699613, 8.722619821570999576 ) ) ;
#40559 = CARTESIAN_POINT ( 'NONE',  ( 1.356773869401999955, -79.41190580526000531, -0.9668579442890000708 ) ) ;
#40560 = CARTESIAN_POINT ( 'NONE',  ( 0.3904537433033999916, -78.53861805112998695, -1.499081755109000103 ) ) ;
#40561 = CARTESIAN_POINT ( 'NONE',  ( -1.689459951007934224, -61.09188253860865814, 12.71013585614315922 ) ) ;
#40562 = CARTESIAN_POINT ( 'NONE',  ( -1.214616973637322683, -83.19939165455916452, 0.8969727609832535142 ) ) ;
#40563 = CARTESIAN_POINT ( 'NONE',  ( 0.000000000000000000, -87.09999999999999432, 0.000000000000000000 ) ) ;
#40564 = CARTESIAN_POINT ( 'NONE',  ( 1.247385801071000166, -17.52277743742000027, -12.50301438876999960 ) ) ;
#40565 = LINE ( 'NONE', #13095, #40022 ) ;
#40566 = CARTESIAN_POINT ( 'NONE',  ( -0.4146376617620515237, -79.47196598975578752, -11.20935700980288452 ) ) ;
#40567 = CARTESIAN_POINT ( 'NONE',  ( 12.56594317982999875, -55.55000000504000468, -1.750000000000000000 ) ) ;
#40568 = ORIENTED_EDGE ( 'NONE', *, *, #51904, .F. ) ;
#40569 = CARTESIAN_POINT ( 'NONE',  ( 0.000000000000000000, -80.70000000000000284, 0.000000000000000000 ) ) ;
#40570 = CARTESIAN_POINT ( 'NONE',  ( -2.879226727952091114, -79.49583333333333712, 10.71369944335146940 ) ) ;
#40571 = CARTESIAN_POINT ( 'NONE',  ( 11.26184072110999779, -78.57390417293299834, 0.07002095171032998722 ) ) ;
#40572 = CARTESIAN_POINT ( 'NONE',  ( 8.171144579309718381, -55.45989902438863339, 7.364280830340200978 ) ) ;
#40573 = ORIENTED_EDGE ( 'NONE', *, *, #46589, .T. ) ;
#40574 = ORIENTED_EDGE ( 'NONE', *, *, #52223, .F. ) ;
#40575 = CIRCLE ( 'NONE', #6606, 4.100000000000000533 ) ;
#40576 = CARTESIAN_POINT ( 'NONE',  ( -3.499999997848071587, -0.7500000000000000000, 0.3665191617529296453 ) ) ;
#40577 = EDGE_LOOP ( 'NONE', ( #38674, #37075, #42863, #23677 ) ) ;
#40578 = DIRECTION ( 'NONE',  ( 0.000000000000000000, 0.000000000000000000, 1.000000000000000000 ) ) ;
#40579 = VERTEX_POINT ( 'NONE', #22966 ) ;
#40580 = DIRECTION ( 'NONE',  ( 0.7071067811865475727, 0.000000000000000000, -0.7071067811865475727 ) ) ;
#40581 = CARTESIAN_POINT ( 'NONE',  ( -10.55592303174000079, -79.87819379990754953, -3.904632140252999317 ) ) ;
#40582 = CARTESIAN_POINT ( 'NONE',  ( -1.460959015002474937, -78.47916666666664298, 0.3926218265389144757 ) ) ;
#40583 = CARTESIAN_POINT ( 'NONE',  ( -0.9781264271452000392, -24.94031143877000289, -12.65967462879000038 ) ) ;
#40584 = CARTESIAN_POINT ( 'NONE',  ( 2.387822949045000254, -81.33957009409999728, 2.679934097432000062 ) ) ;
#40585 = CARTESIAN_POINT ( 'NONE',  ( -7.785422980193717812, -79.35104354428872853, 5.443977945005203267 ) ) ;
#40586 = CARTESIAN_POINT ( 'NONE',  ( -1.776188306762000124, -77.46214197229863885, -10.89629776253999971 ) ) ;
#40587 = CARTESIAN_POINT ( 'NONE',  ( -3.320254015711999962, -78.14236234271000114, 11.17445779594999955 ) ) ;
#40588 = ADVANCED_FACE ( 'NONE', ( #12919, #49244, #22372, #8495 ), #41854, .T. ) ;
#40589 = ORIENTED_EDGE ( 'NONE', *, *, #19701, .T. ) ;
#40590 = EDGE_LOOP ( 'NONE', ( #51324, #31632, #49969, #4623 ) ) ;
#40591 = PLANE ( 'NONE',  #40462 ) ;
#40592 = ADVANCED_FACE ( 'NONE', ( #23539 ), #6120, .T. ) ;
#40593 = CARTESIAN_POINT ( 'NONE',  ( -0.6211595220380999871, -80.80550236970501032, -1.084739991049000096 ) ) ;
#40594 = AXIS2_PLACEMENT_3D ( 'NONE', #54657, #9492, #27477 ) ;
#40595 = CARTESIAN_POINT ( 'NONE',  ( -9.669247687117000112, -77.71629775937297779, -0.8224101967608999919 ) ) ;
#40596 = PLANE ( 'NONE',  #48309 ) ;
#40597 = CARTESIAN_POINT ( 'NONE',  ( 3.638642783662472624, -85.80035203905988794, 0.7847452661105541738 ) ) ;
#40598 = CARTESIAN_POINT ( 'NONE',  ( -8.012867221502000703, -78.34986579304998600, 9.287323121044000374 ) ) ;
#40599 = CARTESIAN_POINT ( 'NONE',  ( -7.915529793650001089, -78.26278494331999980, 9.174504061492999796 ) ) ;
#40600 = CARTESIAN_POINT ( 'NONE',  ( 1.505173492811999969, -76.66263051119899785, -10.77983693663999887 ) ) ;
#40601 = DIRECTION ( 'NONE',  ( -1.000000000000000000, 0.000000000000000000, 0.000000000000000000 ) ) ;
#40602 = CARTESIAN_POINT ( 'NONE',  ( -3.804546608024999887, -81.93696273528199470, 1.109691581360999990 ) ) ;
#40603 = CARTESIAN_POINT ( 'NONE',  ( -10.58783149161999937, -80.86163444153436330, -3.847989116766000084 ) ) ;
#40604 = CARTESIAN_POINT ( 'NONE',  ( -10.53003223724999948, -60.12452529330000317, 7.612971414731999786 ) ) ;
#40605 = CARTESIAN_POINT ( 'NONE',  ( 2.997702459963058175, -2.882598562504878448, 1.253802824134951921 ) ) ;
#40606 = CARTESIAN_POINT ( 'NONE',  ( 10.36935812844000004, -78.17876026662598576, -2.835297515976000327 ) ) ;
#40607 = CARTESIAN_POINT ( 'NONE',  ( -0.1120320062231000002, -77.84019403377490676, -1.328911429676000067 ) ) ;
#40608 = EDGE_CURVE ( 'NONE', #17178, #5420, #50428, .T. ) ;
#40609 = CARTESIAN_POINT ( 'NONE',  ( 0.000000000000000000, 4.040000000000000036, 0.000000000000000000 ) ) ;
#40610 = CARTESIAN_POINT ( 'NONE',  ( 10.78853149093999875, -80.62844613477429334, -3.242959171380999983 ) ) ;
#40611 = CARTESIAN_POINT ( 'NONE',  ( 0.2302091231002842686, -80.38984756532103404, -1.254262070711726906 ) ) ;
#40612 = ORIENTED_EDGE ( 'NONE', *, *, #21070, .F. ) ;
#40613 = CARTESIAN_POINT ( 'NONE',  ( -0.5999999999999999778, -23.15000000000000213, 10.98362417419999915 ) ) ;
#40614 = EDGE_CURVE ( 'NONE', #10884, #5875, #23982, .T. ) ;
#40615 = CARTESIAN_POINT ( 'NONE',  ( -8.796335266380001627, -79.14791666666667425, 6.760013919724038978 ) ) ;
#40616 = DIRECTION ( 'NONE',  ( 0.000000000000000000, -1.000000000000000000, 0.000000000000000000 ) ) ;
#40617 = VECTOR ( 'NONE', #11673, 1000.000000000000000 ) ;
#40618 = CARTESIAN_POINT ( 'NONE',  ( -9.385460185241999653, -79.85105627184799459, -2.646321958768000471 ) ) ;
#40619 = CARTESIAN_POINT ( 'NONE',  ( -12.96685733093999993, -77.02403958349000845, -1.095351912296000041 ) ) ;
#40620 = CARTESIAN_POINT ( 'NONE',  ( -8.597941394714000651, -79.60596001420199741, -4.085545016331000312 ) ) ;
#40621 = CARTESIAN_POINT ( 'NONE',  ( 12.80896991329000123, -20.24546192895000019, -1.930989179114000143 ) ) ;
#40622 = ORIENTED_EDGE ( 'NONE', *, *, #25087, .F. ) ;
#40623 = ADVANCED_FACE ( 'NONE', ( #42143 ), #5530, .F. ) ;
#40624 = CARTESIAN_POINT ( 'NONE',  ( -9.243123479229344852, -24.91653773630011059, -8.441201027682305735 ) ) ;
#40625 = CARTESIAN_POINT ( 'NONE',  ( 13.94764600793045517, -33.10361340872000113, 0.1325532415315603119 ) ) ;
#40626 = CARTESIAN_POINT ( 'NONE',  ( 1.398926169692999766, -81.05658412839899540, 0.1637023605030999973 ) ) ;
#40627 = CARTESIAN_POINT ( 'NONE',  ( 1.133919935544836166, -79.28431342984046637, -9.420845921445170745 ) ) ;
#40628 = AXIS2_PLACEMENT_3D ( 'NONE', #21018, #39598, #48757 ) ;
#40629 = CARTESIAN_POINT ( 'NONE',  ( -3.470329948268000120, -78.36162362607598197, 8.867197205552999506 ) ) ;
#40631 = CARTESIAN_POINT ( 'NONE',  ( 2.301364338783000285, -1.421557261823000129, -3.291430154679999998 ) ) ;
#40630 = CARTESIAN_POINT ( 'NONE',  ( -2.667996182181000098, -84.43400986860198998, 3.211137855840999755 ) ) ;
#40632 = CARTESIAN_POINT ( 'NONE',  ( -1.667916687331000070, -60.09848884406000025, -12.49168451100999988 ) ) ;
#40633 = CARTESIAN_POINT ( 'NONE',  ( -1.508831841893000236, -79.53945180266799753, 0.1495614418054999895 ) ) ;
#40634 = ORIENTED_EDGE ( 'NONE', *, *, #18845, .T. ) ;
#40635 = B_SPLINE_CURVE_WITH_KNOTS ( 'NONE', 3,
 ( #54001, #43975, #8526, #26520, #3525, #35676, #53707, #21526, #39534, #57539 ),
 .UNSPECIFIED., .F., .F.,
 ( 4, 2, 2, 2, 4 ),
 ( 0.000000000000000000, 0.2500000000000000000, 0.5000000000000000000, 0.7500000000000000000, 1.000000000000000000 ),
 .UNSPECIFIED. ) ;
#40636 = CARTESIAN_POINT ( 'NONE',  ( -0.2278969726611020374, -77.22338849210305511, -10.75220085459532449 ) ) ;
#40637 = CARTESIAN_POINT ( 'NONE',  ( 10.00716890277181470, -79.09696047196752033, 6.699252482690748245 ) ) ;
#40638 = AXIS2_PLACEMENT_3D ( 'NONE', #48464, #8007, #16584 ) ;
#40639 = VERTEX_POINT ( 'NONE', #10863 ) ;
#40640 = ORIENTED_EDGE ( 'NONE', *, *, #1134, .T. ) ;
#40641 = FACE_OUTER_BOUND ( 'NONE', #28803, .T. ) ;
#40642 = ADVANCED_FACE ( 'NONE', ( #50138 ), #32968, .F. ) ;
#40643 = DIRECTION ( 'NONE',  ( 0.000000000000000000, 1.000000000000000000, 0.000000000000000000 ) ) ;
#40644 = CARTESIAN_POINT ( 'NONE',  ( 0.000000000000000000, -75.15999999999999659, 0.000000000000000000 ) ) ;
#40645 = ORIENTED_EDGE ( 'NONE', *, *, #33195, .F. ) ;
#40646 = CARTESIAN_POINT ( 'NONE',  ( 11.95316821454999889, -78.43105580595199910, -1.522347302216999987 ) ) ;
#40647 = ORIENTED_EDGE ( 'NONE', *, *, #12904, .T. ) ;
#40648 = ORIENTED_EDGE ( 'NONE', *, *, #24040, .F. ) ;
#40649 = CARTESIAN_POINT ( 'NONE',  ( -2.996749445452521421, -2.632334343058801096, -1.256619453663492703 ) ) ;
#40650 = B_SPLINE_SURFACE_WITH_KNOTS ( 'NONE', 3, 3, ( 
 ( #24361, #19350, #42375, #15500 ),
 ( #33494, #51532, #46234, #48263 ),
 ( #39090, #21083, #52962, #7798 ),
 ( #25798, #26082, #11947, #42956 ),
 ( #16664, #43825, #29352, #7220 ),
 ( #3374, #15791, #2799, #12511 ),
 ( #57097, #16085, #16374, #21368 ),
 ( #20228, #39384, #38220, #47399 ),
 ( #25222, #38798, #7512, #8084 ),
 ( #24934, #57389, #16949, #3089 ),
 ( #25510, #44106, #47973, #43528 ) ),
 .UNSPECIFIED., .F., .F., .F.,
 ( 4, 1, 1, 1, 1, 1, 1, 1, 4 ),
 ( 4, 4 ),
 ( -0.01994574723506000249, 0.000000000000000000, 0.1666666666667000196, 0.3333333333333000081, 0.5000000000000000000, 0.6666666666667000474, 0.8333333333333000637, 1.000000000000000000, 1.020511277925000071 ),
 ( -0.3582002740308999900, 1.358574366093000085 ),
 .UNSPECIFIED. ) ;
#40651 = DIRECTION ( 'NONE',  ( 1.776356839400000238E-14, 1.000000000000000000, -1.894780628693999933E-13 ) ) ;
#40652 = CARTESIAN_POINT ( 'NONE',  ( -3.434862764218605591, -1.304367894840707365, 2.089124736184700737 ) ) ;
#40653 = ORIENTED_EDGE ( 'NONE', *, *, #56786, .F. ) ;
#40654 = CIRCLE ( 'NONE', #57577, 14.00000000000000000 ) ;
#40655 = ORIENTED_EDGE ( 'NONE', *, *, #51824, .F. ) ;
#40656 = CARTESIAN_POINT ( 'NONE',  ( 0.3448888686458475017, -80.00341931423071173, 1.227302044224852118 ) ) ;
#40657 = CARTESIAN_POINT ( 'NONE',  ( 3.962812355711000212, -78.85171438276199751, -1.463672932855430986E-15 ) ) ;
#40658 = CARTESIAN_POINT ( 'NONE',  ( 10.53562613913000057, -55.59442116235999976, 7.620013630307000518 ) ) ;
#40659 = CARTESIAN_POINT ( 'NONE',  ( -7.655555357453000198, -19.22204592323999961, -10.38646360831000059 ) ) ;
#40660 = DIRECTION ( 'NONE',  ( 1.000000000000000000, 0.000000000000000000, 0.000000000000000000 ) ) ;
#40661 = LINE ( 'NONE', #44496, #58196 ) ;
#40662 = CARTESIAN_POINT ( 'NONE',  ( -11.61454496413000115, -77.63029888298812864, 2.935712811417999557 ) ) ;
#40663 = CARTESIAN_POINT ( 'NONE',  ( 7.719754268718227230, -78.80359534466445837, -5.095877674619078590 ) ) ;
#40664 = CARTESIAN_POINT ( 'NONE',  ( -9.302993349864850714, -76.89708402442933277, -6.267052156691077514 ) ) ;
#40665 = CARTESIAN_POINT ( 'NONE',  ( -8.798028344861998917, -24.93813495683999903, 8.790623041439999952 ) ) ;
#40666 = VECTOR ( 'NONE', #38300, 1000.000000000000114 ) ;
#40667 = CARTESIAN_POINT ( 'NONE',  ( 2.421252246090693117, -77.74597346547214727, -9.009672662381980501 ) ) ;
#40668 = CARTESIAN_POINT ( 'NONE',  ( 0.000000000000000000, -76.14999999992500079, 0.000000000000000000 ) ) ;
#40669 = CARTESIAN_POINT ( 'NONE',  ( 2.459051015536999785, -79.03892549782628407, -3.318368392105000453 ) ) ;
#40670 = AXIS2_PLACEMENT_3D ( 'NONE', #35156, #44049, #50456 ) ;
#40671 = CARTESIAN_POINT ( 'NONE',  ( -9.405253678352000435, -77.73528667140098491, 2.617502431767999571 ) ) ;
#40672 = CARTESIAN_POINT ( 'NONE',  ( -3.708203932498999933, -76.29999999999999716, 11.41267819554000162 ) ) ;
#40673 = EDGE_CURVE ( 'NONE', #39462, #22214, #36538, .T. ) ;
#40674 = FACE_BOUND ( 'NONE', #30195, .T. ) ;
#40675 = CARTESIAN_POINT ( 'NONE',  ( 0.9781264271452999592, -24.94031143877000289, 12.65967462879000038 ) ) ;
#40676 = CARTESIAN_POINT ( 'NONE',  ( -12.50680023857786338, -61.10414033366070186, -1.424451025847738972 ) ) ;
#40677 = CARTESIAN_POINT ( 'NONE',  ( -1.165121112472999876, -1.482669754918000127, -3.780546559146999996 ) ) ;
#40678 = CARTESIAN_POINT ( 'NONE',  ( -1.250000000000001332, -80.98958333333331439, 0.1636246173744632659 ) ) ;
#40679 = CARTESIAN_POINT ( 'NONE',  ( 7.355581160863136070, -79.79837709061000339, -5.642938462726122317 ) ) ;
#40680 = CARTESIAN_POINT ( 'NONE',  ( 10.35845608624000036, -55.50221245779999890, 7.627487525399000212 ) ) ;
#40681 = CARTESIAN_POINT ( 'NONE',  ( 0.8412929767025426608, -81.02139373987667170, -1.256298128065854725 ) ) ;
#40682 = CARTESIAN_POINT ( 'NONE',  ( -0.9088528845057587402, -78.54008175705185124, 0.8581086277074990720 ) ) ;
#40683 = CARTESIAN_POINT ( 'NONE',  ( 10.36935812844000004, -78.07876026662599145, -2.835297515976000327 ) ) ;
#40684 = CARTESIAN_POINT ( 'NONE',  ( -12.51072239526000196, -26.30294702885999669, 0.7871079366006996647 ) ) ;
#40685 = CARTESIAN_POINT ( 'NONE',  ( -10.84231296956000001, -78.51729255600099577, 1.272641041331999956 ) ) ;
#40686 = CARTESIAN_POINT ( 'NONE',  ( 11.99915429782999965, -78.14045805696299851, 2.610761444098000261 ) ) ;
#40687 = CARTESIAN_POINT ( 'NONE',  ( -2.769480662737825227, -78.20484845553691855, -10.72687993797705985 ) ) ;
#40689 = CARTESIAN_POINT ( 'NONE',  ( -1.001490227998000027, -79.35438725917299507, -0.8734289068823000157 ) ) ;
#40688 = CARTESIAN_POINT ( 'NONE',  ( -1.460959015002474493, -79.87916666666664867, 0.3926218265389144757 ) ) ;
#40690 = DIRECTION ( 'NONE',  ( 0.000000000000000000, 1.000000000000000000, 0.000000000000000000 ) ) ;
#40691 = ORIENTED_EDGE ( 'NONE', *, *, #56640, .T. ) ;
#40692 = ADVANCED_FACE ( 'NONE', ( #51012 ), #28245, .F. ) ;
#40693 = CARTESIAN_POINT ( 'NONE',  ( 3.544514923079999935, -85.50899735065199536, 0.03711956419559000325 ) ) ;
#40694 = CARTESIAN_POINT ( 'NONE',  ( 7.404330972381000464, -80.89001299829502045, 8.210251132378001415 ) ) ;
#40695 = DIRECTION ( 'NONE',  ( 0.000000000000000000, 1.000000000000000000, 0.000000000000000000 ) ) ;
#40696 = CARTESIAN_POINT ( 'NONE',  ( 2.791771531253838923, -85.59895834061069309, 2.015565555989225377 ) ) ;
#40697 = LINE ( 'NONE', #16804, #41786 ) ;
#40698 = DIRECTION ( 'NONE',  ( 1.000000000000000000, 0.000000000000000000, 0.000000000000000000 ) ) ;
#40699 = CARTESIAN_POINT ( 'NONE',  ( -1.155570385622000096, -77.37333680668000113, -12.58848097821000067 ) ) ;
#40700 = DIRECTION ( 'NONE',  ( 0.7071067811865475727, 0.000000000000000000, -0.7071067811865475727 ) ) ;
#40701 = CARTESIAN_POINT ( 'NONE',  ( 12.78015149457000099, -24.30330660695999967, -1.806228889758999978 ) ) ;
#40702 = CARTESIAN_POINT ( 'NONE',  ( -7.655983890325164687, -55.09663439856309708, -10.06694524866255946 ) ) ;
#40703 = ORIENTED_EDGE ( 'NONE', *, *, #23172, .F. ) ;
#40704 = CARTESIAN_POINT ( 'NONE',  ( -1.217390015646170554, -53.98106975039858924, -12.70229597936710420 ) ) ;
#40705 = CARTESIAN_POINT ( 'NONE',  ( -0.9882926940093508250, -76.99166666656056179, -9.458333332648651393 ) ) ;
#40706 = CARTESIAN_POINT ( 'NONE',  ( 5.348541196722845115, -75.86208451537127928, -10.50221102791410033 ) ) ;
#40707 = ADVANCED_FACE ( 'NONE', ( #9978 ), #41562, .F. ) ;
#40708 = DIRECTION ( 'NONE',  ( 0.000000000000000000, 1.000000000000000000, 0.000000000000000000 ) ) ;
#40709 = EDGE_CURVE ( 'NONE', #5204, #51909, #19081, .T. ) ;
#40710 = CARTESIAN_POINT ( 'NONE',  ( -12.75763395696999858, -56.02204592290999585, -1.931043742978000077 ) ) ;
#40711 = DIRECTION ( 'NONE',  ( -1.000000000000000000, 0.000000000000000000, 0.000000000000000000 ) ) ;
#40712 = EDGE_LOOP ( 'NONE', ( #9930, #22340, #38252, #22993 ) ) ;
#40713 = CARTESIAN_POINT ( 'NONE',  ( -6.146531642657000027, -77.91423522357898435, 9.376936153619999104 ) ) ;
#40714 = CARTESIAN_POINT ( 'NONE',  ( 7.861032689965319342, -61.26660299192877801, -10.10708926017425924 ) ) ;
#40715 = ORIENTED_EDGE ( 'NONE', *, *, #36825, .T. ) ;
#40716 = AXIS2_PLACEMENT_3D ( 'NONE', #40644, #1097, #14058 ) ;
#40717 = EDGE_LOOP ( 'NONE', ( #16875, #3865, #22635 ) ) ;
#40718 = CARTESIAN_POINT ( 'NONE',  ( -7.645398650953000086, -55.58468617124000133, -10.18948982067999864 ) ) ;
#40719 = FILL_AREA_STYLE_COLOUR ( '', #19042 ) ;
#40720 = CARTESIAN_POINT ( 'NONE',  ( 8.985706068735000329, -79.54809944676298983, -3.828549499589000149 ) ) ;
#40721 = EDGE_LOOP ( 'NONE', ( #56899, #42400, #34737, #37006, #5328 ) ) ;
#40722 = CARTESIAN_POINT ( 'NONE',  ( -9.764287472051000449, -76.57194759300099918, 7.371956487538999347 ) ) ;
#40723 = CARTESIAN_POINT ( 'NONE',  ( -10.45242846958592331, -78.61880728566940491, -2.511674934066081555 ) ) ;
#40724 = CARTESIAN_POINT ( 'NONE',  ( -1.527202200078999983, -78.19870846077999715, 0.1530789007224999942 ) ) ;
#40725 = VERTEX_POINT ( 'NONE', #18406 ) ;
#40726 = EDGE_CURVE ( 'NONE', #5887, #51923, #55015, .T. ) ;
#40727 = CARTESIAN_POINT ( 'NONE',  ( -0.7479529023060000892, -77.68867305011499980, -9.465622776916999825 ) ) ;
#40728 = CARTESIAN_POINT ( 'NONE',  ( 1.250000000000000000, -80.34999999999999432, 0.000000000000000000 ) ) ;
#40729 = CARTESIAN_POINT ( 'NONE',  ( -3.153993092687999766, -78.38870099961999927, 12.72742730875000028 ) ) ;
#40730 = CARTESIAN_POINT ( 'NONE',  ( -7.374560639698971798, -78.87291666666666856, -9.596002108778163731 ) ) ;
#40731 = CARTESIAN_POINT ( 'NONE',  ( -2.557474545125634435, -86.40321104920798234, 3.452189813556158615 ) ) ;
#40732 = CARTESIAN_POINT ( 'NONE',  ( 2.867548251969000095, -77.89887176884063535, -9.270807752789000489 ) ) ;
#40733 = CARTESIAN_POINT ( 'NONE',  ( 5.960820980064980290, -79.91975476581831117, 7.102596592892035154 ) ) ;
#40734 = CARTESIAN_POINT ( 'NONE',  ( -3.204655417894513025, -78.85416664733885739, -2.415670736004921881 ) ) ;
#40735 = ORIENTED_EDGE ( 'NONE', *, *, #48767, .T. ) ;
#40736 = CARTESIAN_POINT ( 'NONE',  ( -6.294203684166999935, -77.18138806810267738, 7.343715272572999275 ) ) ;
#40737 = CARTESIAN_POINT ( 'NONE',  ( 2.922072168813211412, -77.25074815672523698, -8.776223896002093738 ) ) ;
#40738 = CARTESIAN_POINT ( 'NONE',  ( -1.137653363949000074, -79.79521086701498689, 1.002340751266999952 ) ) ;
#40739 = CARTESIAN_POINT ( 'NONE',  ( -2.945092855005243315, -3.303172867046446193, 1.926994060853980839 ) ) ;
#40740 = CARTESIAN_POINT ( 'NONE',  ( 7.660431276897000430, -59.99179487629999841, -10.01749742442000191 ) ) ;
#40741 = CARTESIAN_POINT ( 'NONE',  ( -12.27595451887999900, -76.19941089817999114, 0.3505736730271999391 ) ) ;
#40742 = CARTESIAN_POINT ( 'NONE',  ( 5.500000000000000000, -80.99999999999998579, 0.000000000000000000 ) ) ;
#40743 = CARTESIAN_POINT ( 'NONE',  ( 7.777253296891999845, -77.24328832859900729, 5.676678302143000288 ) ) ;
#40744 = CARTESIAN_POINT ( 'NONE',  ( -5.099558739856028922, -77.14031901058056917, -10.93429447588933634 ) ) ;
#40745 = CARTESIAN_POINT ( 'NONE',  ( 9.367799907751061639, -76.64748953336749082, -7.737080272526681846 ) ) ;
#40746 = ORIENTED_EDGE ( 'NONE', *, *, #42061, .T. ) ;
#40747 = CARTESIAN_POINT ( 'NONE',  ( -1.167634245779999969, -83.49552555368299522, -0.6204341648412000643 ) ) ;
#40748 = CARTESIAN_POINT ( 'NONE',  ( 4.000000000000000000, -74.80000000000001137, -0.5999999999999999778 ) ) ;
#40749 = CARTESIAN_POINT ( 'NONE',  ( -1.164828128805999992E-14, -72.75000000040999737, -13.94999999959000014 ) ) ;
#40750 = VECTOR ( 'NONE', #16351, 1000.000000000000000 ) ;
#40751 = CARTESIAN_POINT ( 'NONE',  ( 0.3864029911681999829, -77.12593457586999079, -11.74364478040999948 ) ) ;
#40752 = CARTESIAN_POINT ( 'NONE',  ( 1.250000000000000000, -55.54999999966999980, -12.00000000000000000 ) ) ;
#40753 = CARTESIAN_POINT ( 'NONE',  ( 9.752895431365999457, -78.77770829698199861, -6.878701514737999290 ) ) ;
#40754 = CARTESIAN_POINT ( 'NONE',  ( 8.219513559211000242, -78.80469415034599479, 5.194554602171000290 ) ) ;
#40755 = CARTESIAN_POINT ( 'NONE',  ( 4.510926502723999754, -77.54314704349698673, 8.509098192649000580 ) ) ;
#40756 = CARTESIAN_POINT ( 'NONE',  ( 2.738482428451646911, -76.05593295161513367, 11.42672558838834895 ) ) ;
#40757 = CARTESIAN_POINT ( 'NONE',  ( 10.95738943370000129, -79.19961247579199437, -1.279590238973999927 ) ) ;
#40758 = CARTESIAN_POINT ( 'NONE',  ( -0.5721033155199185538, -86.02148118236286223, 4.600989486740219014 ) ) ;
#40759 = ORIENTED_EDGE ( 'NONE', *, *, #15455, .F. ) ;
#40760 = EDGE_CURVE ( 'NONE', #47713, #19532, #39906, .T. ) ;
#40761 = CARTESIAN_POINT ( 'NONE',  ( -10.62397638184999948, -76.09214061310410671, -6.218250916117999516 ) ) ;
#40762 = CARTESIAN_POINT ( 'NONE',  ( 3.400000000000108269, -78.67390000031812747, -2.006589542798860926 ) ) ;
#40763 = EDGE_CURVE ( 'NONE', #18636, #41301, #55579, .T. ) ;
#40764 = CARTESIAN_POINT ( 'NONE',  ( 10.55657102546000026, -78.65809125644999256, -3.003801718854000047 ) ) ;
#40765 = CARTESIAN_POINT ( 'NONE',  ( -1.439896632895338202, -79.21458333333333712, -10.99999999999999822 ) ) ;
#40766 = CARTESIAN_POINT ( 'NONE',  ( -11.42547184184000031, -76.90670592927000371, -5.080618559187000116 ) ) ;
#40767 = CYLINDRICAL_SURFACE ( 'NONE', #1044, 1.750000000000001332 ) ;
#40768 = CARTESIAN_POINT ( 'NONE',  ( 0.3980000373821807047, -77.96875000003851142, 1.234183929323941831 ) ) ;
#40769 = ORIENTED_EDGE ( 'NONE', *, *, #7707, .T. ) ;
#40770 = CARTESIAN_POINT ( 'NONE',  ( -10.75919966670999983, -79.75272080125398588, 3.327699969971999572 ) ) ;
#40771 = CARTESIAN_POINT ( 'NONE',  ( 12.70619604133367098, -17.53855724477478972, 1.571828507159243271 ) ) ;
#40772 = CARTESIAN_POINT ( 'NONE',  ( 0.9382417441925061663, -75.80000000000001137, -11.80136876550232117 ) ) ;
#40773 = CARTESIAN_POINT ( 'NONE',  ( -0.03689285838845265952, -78.48547955770028750, 3.914326906660362315 ) ) ;
#40774 = VECTOR ( 'NONE', #22748, 1000.000000000000000 ) ;
#40775 = CARTESIAN_POINT ( 'NONE',  ( -0.8449747453178998446, -81.53464264722271082, 0.9222519907885509127 ) ) ;
#40776 = EDGE_CURVE ( 'NONE', #32275, #5785, #43639, .T. ) ;
#40777 = CARTESIAN_POINT ( 'NONE',  ( 10.73159385090000129, -78.47100192322299961, -3.053603293876000269 ) ) ;
#40778 = DIRECTION ( 'NONE',  ( 0.000000000000000000, -1.000000000000000000, 0.000000000000000000 ) ) ;
#40779 = LINE ( 'NONE', #53781, #13864 ) ;
#40780 = CARTESIAN_POINT ( 'NONE',  ( 6.606377239730313988, -79.32291666666665719, 8.596418555780454440 ) ) ;
#40781 = CARTESIAN_POINT ( 'NONE',  ( -1.842497806997727139, -79.58834702216799428, 10.91026042240053862 ) ) ;
#40782 = FACE_BOUND ( 'NONE', #49876, .T. ) ;
#40783 = EDGE_LOOP ( 'NONE', ( #56912, #35982, #33283, #31176 ) ) ;
#40784 = EDGE_LOOP ( 'NONE', ( #43623, #25533, #35691, #28039 ) ) ;
#40785 = CARTESIAN_POINT ( 'NONE',  ( -9.500000000000000000, -78.39999999999999147, 0.000000000000000000 ) ) ;
#40786 = CARTESIAN_POINT ( 'NONE',  ( 12.00000000000000000, -79.54999999999999716, 0.000000000000000000 ) ) ;
#40787 = CIRCLE ( 'NONE', #50243, 30.49999999999998934 ) ;
#40788 = ORIENTED_EDGE ( 'NONE', *, *, #2918, .F. ) ;
#40789 = CARTESIAN_POINT ( 'NONE',  ( 10.90625000000000000, -80.29374999999798490, -5.301077343649000152E-10 ) ) ;
#40790 = ORIENTED_EDGE ( 'NONE', *, *, #27348, .F. ) ;
#40791 = CARTESIAN_POINT ( 'NONE',  ( 8.588902834690999910, -25.13240111580999780, 9.317946123639000433 ) ) ;
#40792 = CARTESIAN_POINT ( 'NONE',  ( 10.12138908678999982, -77.42369350912798609, 4.388532480841000449 ) ) ;
#40793 = CARTESIAN_POINT ( 'NONE',  ( 8.180687091746211337, -55.49344856148323402, -7.353725627631179762 ) ) ;
#40794 = CARTESIAN_POINT ( 'NONE',  ( -9.610781959738998736, -78.61933998579799265, 1.214124111355000091 ) ) ;
#40795 = CARTESIAN_POINT ( 'NONE',  ( -5.812602142628422897, -78.17097178526422852, -7.195572196038425794 ) ) ;
#40796 = AXIS2_PLACEMENT_3D ( 'NONE', #51366, #50785, #23321 ) ;
#40797 = CARTESIAN_POINT ( 'NONE',  ( -9.066796825632000179, -78.81620026593400041, -6.603885667862000375 ) ) ;
#40798 = CARTESIAN_POINT ( 'NONE',  ( 0.8000647195480976581, -81.00000000000001421, 10.77406987238426872 ) ) ;
#40799 = ORIENTED_EDGE ( 'NONE', *, *, #41158, .F. ) ;
#40800 = LINE ( 'NONE', #14215, #49138 ) ;
#40801 = EDGE_LOOP ( 'NONE', ( #17851, #33513, #4379, #37746 ) ) ;
#40802 = CARTESIAN_POINT ( 'NONE',  ( -1.490426546943438124, -77.48793975142889678, 9.129111009367720797 ) ) ;
#40803 = CARTESIAN_POINT ( 'NONE',  ( -6.065106684382000068, -77.41173743516598904, 9.224892016835999797 ) ) ;
#40804 = CYLINDRICAL_SURFACE ( 'NONE', #55471, 0.6000000000000008660 ) ;
#40805 = EDGE_CURVE ( 'NONE', #13326, #27414, #42884, .T. ) ;
#40806 = CARTESIAN_POINT ( 'NONE',  ( -4.475245744599999576, -78.97731204328599119, -8.610626265545000990 ) ) ;
#40807 = VECTOR ( 'NONE', #28918, 1000.000000000000000 ) ;
#40808 = CARTESIAN_POINT ( 'NONE',  ( 11.50045843932000089, -76.73061308324000152, -3.738034289973000135 ) ) ;
#40809 = CARTESIAN_POINT ( 'NONE',  ( -5.127834196515462573, -79.47936672015556780, -7.997626843221576465 ) ) ;
#40810 = CARTESIAN_POINT ( 'NONE',  ( -1.573065832928000063, -78.69054132838999749, 0.4172852021023999991 ) ) ;
#40811 = CARTESIAN_POINT ( 'NONE',  ( 3.113304451009999863, -78.39783470746900207, -10.55022916317000181 ) ) ;
#40812 = CIRCLE ( 'NONE', #51204, 0.5000000000000004441 ) ;
#40813 = B_SPLINE_CURVE_WITH_KNOTS ( 'NONE', 3,
 ( #37619, #50643, #51513, #15486, #47382, #42646, #20213, #33178, #51225, #6914 ),
 .UNSPECIFIED., .F., .F.,
 ( 4, 2, 2, 2, 4 ),
 ( 0.000000000000000000, 0.2500000000000000000, 0.5000000000000000000, 0.7500000000000000000, 1.000000000000000000 ),
 .UNSPECIFIED. ) ;
#40814 = CARTESIAN_POINT ( 'NONE',  ( 7.195688986358000250, -79.24706562342598204, 8.240744890341000328 ) ) ;
#40815 = CARTESIAN_POINT ( 'NONE',  ( -0.6295237254636235624, -78.08333333333331439, -1.092232985442822990 ) ) ;
#40816 = CARTESIAN_POINT ( 'NONE',  ( 5.684557159767975598, -78.67708333333330017, -7.396918292183157106 ) ) ;
#40817 = CARTESIAN_POINT ( 'NONE',  ( -3.556697332079000518, -82.97942814914499365, 0.4833727558985000394 ) ) ;
#40818 = ORIENTED_EDGE ( 'NONE', *, *, #42083, .F. ) ;
#40819 = CARTESIAN_POINT ( 'NONE',  ( 7.619787310138999459, -79.61921597853599053, -9.677026921773000723 ) ) ;
#40820 = CARTESIAN_POINT ( 'NONE',  ( 2.940128815575000054, -76.49533191828599854, 10.98859724391999926 ) ) ;
#40821 = CARTESIAN_POINT ( 'NONE',  ( -7.602035473967630352, -78.03750729326660007, 7.600743598855997263 ) ) ;
#40822 = CARTESIAN_POINT ( 'NONE',  ( 10.99419336675999936, -78.91639992327199593, 4.758540471090999979 ) ) ;
#40823 = CARTESIAN_POINT ( 'NONE',  ( -3.250000000000000000, -3.500000000000000000, -1.188926645705999921E-13 ) ) ;
#40825 = FACE_OUTER_BOUND ( 'NONE', #49206, .T. ) ;
#40824 = DIRECTION ( 'NONE',  ( 0.000000000000000000, 1.000000000000000000, 1.322413929418000086E-13 ) ) ;
#40826 = CARTESIAN_POINT ( 'NONE',  ( 3.620209227050000145, -86.25171438276198899, -1.611820994701000043 ) ) ;
#40827 = CARTESIAN_POINT ( 'NONE',  ( 3.718021618522670213, -80.94702727586427216, 10.08698426341377008 ) ) ;
#40828 = CARTESIAN_POINT ( 'NONE',  ( -4.165479847964999927, -80.46200396371098407, 10.49531740235000044 ) ) ;
#40829 = CARTESIAN_POINT ( 'NONE',  ( 4.784380313523556083, -78.46666666666665435, -8.300970689365444244 ) ) ;
#40830 = CARTESIAN_POINT ( 'NONE',  ( -5.715586620248999772, -77.97329328214799204, -9.570092484259999921 ) ) ;
#40831 = CARTESIAN_POINT ( 'NONE',  ( -10.60034922676000058, -80.48104072104460727, -3.033110234585999709 ) ) ;
#40832 = ORIENTED_EDGE ( 'NONE', *, *, #32647, .T. ) ;
#40833 = CARTESIAN_POINT ( 'NONE',  ( 1.798954018885000172, -55.58469026579999905, 12.61117007300000026 ) ) ;
#40834 = CARTESIAN_POINT ( 'NONE',  ( 5.807838419656999207, -77.32737403538303056, -7.511754867730999763 ) ) ;
#40835 = CARTESIAN_POINT ( 'NONE',  ( 3.362739751829000312, -2.429750604645999790, -1.782634050134999981 ) ) ;
#40836 = EDGE_CURVE ( 'NONE', #18440, #20752, #32429, .T. ) ;
#40837 = CARTESIAN_POINT ( 'NONE',  ( 7.199825537761999961, -77.01785638038899151, 8.601198917431998936 ) ) ;
#40838 = CARTESIAN_POINT ( 'NONE',  ( -8.796335266379976758, -79.75208333333333144, -6.760013919724066511 ) ) ;
#40839 = AXIS2_PLACEMENT_3D ( 'NONE', #51810, #16938, #51520 ) ;
#40840 = DIRECTION ( 'NONE',  ( 0.000000000000000000, 1.000000000000000000, 0.000000000000000000 ) ) ;
#40841 = CARTESIAN_POINT ( 'NONE',  ( 12.80000000000000071, -0.1000000000000000056, 0.000000000000000000 ) ) ;
#40842 = CARTESIAN_POINT ( 'NONE',  ( -10.26995137457921992, -78.52463911791149087, -3.283750080291026219 ) ) ;
#40843 = CARTESIAN_POINT ( 'NONE',  ( 12.50000000000000000, -49.87071424677999687, 0.000000000000000000 ) ) ;
#40844 = CARTESIAN_POINT ( 'NONE',  ( 2.191310644209000014, -85.68044503318799343, 3.550807881941000055 ) ) ;
#40845 = CARTESIAN_POINT ( 'NONE',  ( -5.911015991908509903, -76.05000000000002558, 10.22919423390550442 ) ) ;
#40846 = CARTESIAN_POINT ( 'NONE',  ( -3.391782956974000118, -78.59828808732000027, -12.49646859905000085 ) ) ;
#40847 = B_SPLINE_SURFACE_WITH_KNOTS ( 'NONE', 3, 3, ( 
 ( #51145, #55853, #31936, #14227 ),
 ( #32225, #27800, #45846, #23387 ),
 ( #41398, #48132, #33366, #29511 ),
 ( #51694, #51403, #7664, #52259 ),
 ( #25663, #25091, #52542, #3248 ),
 ( #43693, #2952, #6801, #2675 ),
 ( #11244, #12099, #29791, #33940 ),
 ( #38668, #29223, #20952, #24810 ) ),
 .UNSPECIFIED., .F., .F., .F.,
 ( 4, 1, 1, 1, 1, 4 ),
 ( 4, 4 ),
 ( -0.01200407347463999970, 0.000000000000000000, 0.3333333333333000081, 0.6666666666667000474, 1.000000000000000000, 1.011997855551999947 ),
 ( -0.3559705542741999906, 1.355970554273999928 ),
 .UNSPECIFIED. ) ;
#40848 = ADVANCED_FACE ( 'NONE', ( #32828 ), #37268, .F. ) ;
#40849 = CARTESIAN_POINT ( 'NONE',  ( -10.89229298341999908, -77.19182080052098627, 2.369082973246999568 ) ) ;
#40850 = CARTESIAN_POINT ( 'NONE',  ( -1.529754383668999962, -81.30273936731998674, -0.6588408878327000062 ) ) ;
#40851 = CARTESIAN_POINT ( 'NONE',  ( -1.524425929186000062, -77.86280409478000308, -0.6660453670107999713 ) ) ;
#40852 = CARTESIAN_POINT ( 'NONE',  ( 2.632967082928999947, -77.24351440681299152, 9.306700570505000769 ) ) ;
#40853 = CARTESIAN_POINT ( 'NONE',  ( 0.3892601172833429768, -82.89574158191382480, -1.460010013733279433 ) ) ;
#40854 = CARTESIAN_POINT ( 'NONE',  ( -12.72554383682000001, -60.00159311597000311, 1.930239506950999884 ) ) ;
#40855 = CARTESIAN_POINT ( 'NONE',  ( 10.92207628522714202, -78.10253042142522872, 0.3426783470800407461 ) ) ;
#40856 = B_SPLINE_CURVE_WITH_KNOTS ( 'NONE', 3,
 ( #692, #32221, #9811, #50263, #5375, #2129, #30116, #47878, #52009, #16277, #20985, #34257, #6828, #33685, #7409, #47010, #25123, #56142 ),
 .UNSPECIFIED., .F., .F.,
 ( 4, 2, 2, 2, 2, 2, 2, 2, 4 ),
 ( 0.000000000000000000, 0.1250000000000000000, 0.2500000000000000000, 0.3750000000000000000, 0.5000000000000000000, 0.6250000000000000000, 0.7500000000000000000, 0.8750000000000000000, 1.000000000000000000 ),
 .UNSPECIFIED. ) ;
#40857 = CARTESIAN_POINT ( 'NONE',  ( 12.65375411746000012, -21.74977139047000207, -1.750000000000000000 ) ) ;
#40858 = CARTESIAN_POINT ( 'NONE',  ( 0.1449677685770666691, -78.01573408261680243, 1.266509336713319334 ) ) ;
#40859 = CIRCLE ( 'NONE', #30469, 0.5000000000000004441 ) ;
#40860 = CARTESIAN_POINT ( 'NONE',  ( -1.112877499973157436, -80.90331638296983385, -0.8763867746066754671 ) ) ;
#40861 = DIRECTION ( 'NONE',  ( -1.000000000000000000, 0.000000000000000000, 0.000000000000000000 ) ) ;
#40862 = CARTESIAN_POINT ( 'NONE',  ( 4.624113774747000249, -79.05017638237299593, -10.14259199460999916 ) ) ;
#40863 = DIRECTION ( 'NONE',  ( 0.000000000000000000, 1.000000000000000000, 0.000000000000000000 ) ) ;
#40864 = ORIENTED_EDGE ( 'NONE', *, *, #28627, .F. ) ;
#40865 = ORIENTED_EDGE ( 'NONE', *, *, #1247, .T. ) ;
#40866 = CARTESIAN_POINT ( 'NONE',  ( 1.579079316662999943, -81.25868548972499639, 0.3372275755211999737 ) ) ;
#40867 = ORIENTED_EDGE ( 'NONE', *, *, #16382, .F. ) ;
#40868 = CARTESIAN_POINT ( 'NONE',  ( 1.980584515752000119, -55.53514853344000102, 12.76303204600000107 ) ) ;
#40869 = ORIENTED_EDGE ( 'NONE', *, *, #50452, .F. ) ;
#40870 = CARTESIAN_POINT ( 'NONE',  ( -1.666698456700999920, -18.80818260160000222, 12.50018138921000066 ) ) ;
#40871 = DIRECTION ( 'NONE',  ( -1.000000000000000000, 0.000000000000000000, 0.000000000000000000 ) ) ;
#40872 = CARTESIAN_POINT ( 'NONE',  ( -2.697861840213120921, -81.86041665153629765, -2.140231034139926436 ) ) ;
#40873 = CARTESIAN_POINT ( 'NONE',  ( 1.801614160558000055, -23.38652261905000174, -12.59687422887999908 ) ) ;
#40874 = CARTESIAN_POINT ( 'NONE',  ( 2.359403609525000167, -79.53195424565778637, -3.184211391267000035 ) ) ;
#40875 = CARTESIAN_POINT ( 'NONE',  ( -10.75000000000000000, -78.00000000000000000, 2.252154972635999871E-14 ) ) ;
#40876 = CARTESIAN_POINT ( 'NONE',  ( -8.893690104282001130, -78.89047970819000000, -8.147993850101000746 ) ) ;
#40877 = ORIENTED_EDGE ( 'NONE', *, *, #4833, .T. ) ;
#40878 = ORIENTED_EDGE ( 'NONE', *, *, #43410, .T. ) ;
#40879 = CARTESIAN_POINT ( 'NONE',  ( -11.99999999979999821, -23.14999999072999870, 0.7999999997951999786 ) ) ;
#40880 = EDGE_CURVE ( 'NONE', #45004, #4724, #9875, .T. ) ;
#40881 = CARTESIAN_POINT ( 'NONE',  ( -1.154258600661999923, -79.80741129628098918, -0.6680293646364998672 ) ) ;
#40882 = CARTESIAN_POINT ( 'NONE',  ( -9.346518596363001308, -77.68787393024398114, 2.610229778083999808 ) ) ;
#40883 = FACE_OUTER_BOUND ( 'NONE', #15392, .T. ) ;
#40884 = CARTESIAN_POINT ( 'NONE',  ( -10.07719973192000040, -21.74888345808999901, 7.718346056094000041 ) ) ;
#40885 = CARTESIAN_POINT ( 'NONE',  ( -3.220107333416999840, -77.22669831202999546, 12.38709272308999942 ) ) ;
#40886 = EDGE_CURVE ( 'NONE', #53933, #45259, #15428, .T. ) ;
#40887 = CARTESIAN_POINT ( 'NONE',  ( 0.2307066564514000107, -79.28091273156999819, -1.449970716867000187 ) ) ;
#40888 = CONICAL_SURFACE ( 'NONE', #23933, 13.94999999993999928, 0.7853981633972997312 ) ;
#40889 = CARTESIAN_POINT ( 'NONE',  ( 7.000000000000000000, -80.99999999999998579, 0.000000000000000000 ) ) ;
#40890 = DIRECTION ( 'NONE',  ( 0.000000000000000000, 0.000000000000000000, -1.000000000000000000 ) ) ;
#40891 = CARTESIAN_POINT ( 'NONE',  ( -0.06101177358013000485, -79.81593595582098999, 4.172091831179000287 ) ) ;
#40892 = CARTESIAN_POINT ( 'NONE',  ( -6.474781754604000739, -80.27459204492750189, -9.218806710208998112 ) ) ;
#40893 = CARTESIAN_POINT ( 'NONE',  ( 12.60354432327999952, -22.75100837100999840, 1.750000000001000089 ) ) ;
#40894 = AXIS2_PLACEMENT_3D ( 'NONE', #43556, #56268, #37955 ) ;
#40895 = CARTESIAN_POINT ( 'NONE',  ( -9.614379562845476457, -78.25080762427336367, 6.833952463418961898 ) ) ;
#40896 = CARTESIAN_POINT ( 'NONE',  ( -3.405171369683000382, -81.64480496681198929, 0.9931618166635001188 ) ) ;
#40897 = CONICAL_SURFACE ( 'NONE', #31434, 1.099999997148999986, 0.7853981633972997312 ) ;
#40898 = CARTESIAN_POINT ( 'NONE',  ( 0.1443438050804999873, -78.08825715068029183, 1.325798245762999983 ) ) ;
#40899 = CARTESIAN_POINT ( 'NONE',  ( 0.000000000000000000, -76.89999999999999147, 0.000000000000000000 ) ) ;
#40900 = CARTESIAN_POINT ( 'NONE',  ( -2.895922040489999905, -80.22958303545810566, 10.88681414971999928 ) ) ;
#40901 = CARTESIAN_POINT ( 'NONE',  ( -3.804208684430999909, -3.354482064474000325, -0.1186911049137999996 ) ) ;
#40902 = CARTESIAN_POINT ( 'NONE',  ( 12.00000000000000000, -79.04999999999999716, 0.000000000000000000 ) ) ;
#40903 = ORIENTED_EDGE ( 'NONE', *, *, #49946, .T. ) ;
#40904 = CARTESIAN_POINT ( 'NONE',  ( -0.4820079653423386956, -23.51614597297864862, 10.98957811953314412 ) ) ;
#40905 = CARTESIAN_POINT ( 'NONE',  ( 9.500000000000000000, -77.14999999999999147, 0.000000000000000000 ) ) ;
#40906 = CARTESIAN_POINT ( 'NONE',  ( 0.000000000000000000, 0.000000000000000000, 0.000000000000000000 ) ) ;
#40907 = B_SPLINE_CURVE_WITH_KNOTS ( 'NONE', 3,
 ( #22756, #23627, #10064, #41352, #10349, #647, #50805, #360, #36330, #68, #28332, #54355, #46383, #5907, #18046, #45798, #54063, #41061 ),
 .UNSPECIFIED., .F., .F.,
 ( 4, 2, 2, 2, 2, 2, 2, 2, 4 ),
 ( 0.000000000000000000, 0.1250000000000000278, 0.2500000000000000555, 0.3750000000000000000, 0.5000000000000000000, 0.6250000000000000000, 0.7500000000000000000, 0.8750000000000001110, 1.000000000000000000 ),
 .UNSPECIFIED. ) ;
#40908 = CARTESIAN_POINT ( 'NONE',  ( 0.08638142328466999476, -81.13550306063599749, 1.330832257483999914 ) ) ;
#40909 = ADVANCED_FACE ( 'NONE', ( #24577 ), #47037, .F. ) ;
#40910 = CARTESIAN_POINT ( 'NONE',  ( 1.667936697358999965, -59.56462890159999546, 12.53241208775999915 ) ) ;
#40911 = CARTESIAN_POINT ( 'NONE',  ( -1.189541931187000134, -77.13504886542000349, -12.95855809378999979 ) ) ;
#40912 = CARTESIAN_POINT ( 'NONE',  ( -7.627497484503559910, -79.53793217095720536, 7.575070705985291752 ) ) ;
#40913 = CARTESIAN_POINT ( 'NONE',  ( 2.853743189566999534E-14, -82.05000000008600125, 0.000000000000000000 ) ) ;
#40914 = CARTESIAN_POINT ( 'NONE',  ( 11.71247802671000038, -76.72437053406000018, -3.008538372945000372 ) ) ;
#40915 = VERTEX_POINT ( 'NONE', #39592 ) ;
#40916 = CARTESIAN_POINT ( 'NONE',  ( 1.250000000000000000, -77.10000000000000853, -0.5000000000000000000 ) ) ;
#40917 = CYLINDRICAL_SURFACE ( 'NONE', #2268, 0.5999999999999999778 ) ;
#40918 = ADVANCED_FACE ( 'NONE', ( #7724 ), #57820, .T. ) ;
#40919 = CARTESIAN_POINT ( 'NONE',  ( 1.116962868089000027, -82.03575701190399627, 0.6857220190616999389 ) ) ;
#40920 = CARTESIAN_POINT ( 'NONE',  ( -1.405334850300460126, -17.68507052218669529, 12.50716844834726160 ) ) ;
#40921 = CARTESIAN_POINT ( 'NONE',  ( -9.411482030169999291, -79.02239977856800124, -0.1876179646513999877 ) ) ;
#40922 = ADVANCED_FACE ( 'NONE', ( #12442 ), #30435, .F. ) ;
#40924 = CARTESIAN_POINT ( 'NONE',  ( -3.754890333716000228, -1.346196431073999999, -1.424957469106999941 ) ) ;
#40923 = CARTESIAN_POINT ( 'NONE',  ( 3.596064725228000025, -85.38443645448099062, 2.031459853198999799 ) ) ;
#40925 = CARTESIAN_POINT ( 'NONE',  ( -1.250000000000000000, -82.49999999999998579, 0.000000000000000000 ) ) ;
#40926 = B_SPLINE_CURVE_WITH_KNOTS ( 'NONE', 3,
 ( #10671, #5351, #37218, #41371, #18937, #32777, #19813, #36927, #54659, #37806 ),
 .UNSPECIFIED., .F., .F.,
 ( 4, 2, 2, 2, 4 ),
 ( 0.000000000000000000, 0.2500000000000000000, 0.5000000000000000000, 0.7500000000000000000, 1.000000000000000000 ),
 .UNSPECIFIED. ) ;
#40927 = CARTESIAN_POINT ( 'NONE',  ( -1.304983203281999904, -80.14632141193500559, 0.1938670925079999940 ) ) ;
#40928 = ORIENTED_EDGE ( 'NONE', *, *, #43021, .F. ) ;
#40929 = CARTESIAN_POINT ( 'NONE',  ( -3.442070086358578695, -77.19916421208671409, -10.18408852963041156 ) ) ;
#40930 = CARTESIAN_POINT ( 'NONE',  ( -8.359900899578630415E-07, -76.12787248224110215, -11.82848710057588626 ) ) ;
#40931 = CARTESIAN_POINT ( 'NONE',  ( 3.992904449609001372, -78.77851881763731967, 7.985808899218034718 ) ) ;
#40932 = ORIENTED_EDGE ( 'NONE', *, *, #45102, .T. ) ;
#40933 = ORIENTED_EDGE ( 'NONE', *, *, #38818, .T. ) ;
#40934 = CARTESIAN_POINT ( 'NONE',  ( 9.203868716350999790, -79.66626286943098023, 5.914103205931999341 ) ) ;
#40935 = AXIS2_PLACEMENT_3D ( 'NONE', #27709, #4998, #36864 ) ;
#40936 = DIRECTION ( 'NONE',  ( 0.000000000000000000, 1.000000000000000000, 0.000000000000000000 ) ) ;
#40937 = CARTESIAN_POINT ( 'NONE',  ( -3.928999787110243336, -80.40462189993948527, 10.05523583907100260 ) ) ;
#40938 = EDGE_LOOP ( 'NONE', ( #45160, #54290, #52632, #40428 ) ) ;
#40939 = CARTESIAN_POINT ( 'NONE',  ( -11.55487901120999972, -78.21402128256200115, -3.417680896482000019 ) ) ;
#40940 = VERTEX_POINT ( 'NONE', #48192 ) ;
#40941 = ORIENTED_EDGE ( 'NONE', *, *, #27168, .F. ) ;
#40942 = CARTESIAN_POINT ( 'NONE',  ( 0.1872937409654373275, -2.730135739282324003, -3.245155438500901379 ) ) ;
#40943 = ADVANCED_FACE ( 'NONE', ( #56747 ), #27645, .F. ) ;
#40944 = LINE ( 'NONE', #532, #38934 ) ;
#40945 = LINE ( 'NONE', #50396, #18564 ) ;
#40946 = ORIENTED_EDGE ( 'NONE', *, *, #13607, .T. ) ;
#40947 = CARTESIAN_POINT ( 'NONE',  ( -9.019406120295011320, -53.80707871034554302, -8.666949038533088512 ) ) ;
#40948 = ORIENTED_EDGE ( 'NONE', *, *, #1233, .F. ) ;
#40949 = CARTESIAN_POINT ( 'NONE',  ( 3.999999999999675371, -78.69999999999998863, -2.360693579763098349 ) ) ;
#40950 = CARTESIAN_POINT ( 'NONE',  ( 10.18127254042999930, -55.41355771686999532, 7.633407132363999814 ) ) ;
#40951 = FACE_OUTER_BOUND ( 'NONE', #52385, .T. ) ;
#40952 = DIRECTION ( 'NONE',  ( -1.000000000000000000, 0.000000000000000000, 0.000000000000000000 ) ) ;
#40953 = EDGE_CURVE ( 'NONE', #31986, #25175, #25727, .T. ) ;
#40954 = B_SPLINE_CURVE_WITH_KNOTS ( 'NONE', 3,
 ( #57978, #9562, #26665, #23133, #40562, #48838, #18131, #45590, #36126, #5135, #4253, #3949, #54142, #13683, #50016, #4844, #13092, #17533, #31973, #27546, #35524, #17239, #13978, #40853, #445, #31089, #22551, #12806, #58274, #41141, #54442, #35226, #31680, #49126, #26378, #22250, #53257, #17837, #53553, #35825, #30805, #18424, #53854, #4549, #40261, #31386, #49427, #8978, #26963, #9269, #44993, #27254, #15445, #5415, #9856, #18712, #24304, #47054, #50600, #27838, #19579, #36706, #33439, #50306, #55302, #19880, #23713, #55893, #41435, #37873, #19002, #10435, #45883, #54721, #6583, #55010, #51475, #15144, #19294, #46767, #28715, #14558, #23423, #10149, #24595, #1301, #36994, #37286, #11032, #29015, #42318, #732, #51182, #14264, #5702, #32552, #6289, #1886, #28126, #1021, #32260, #46176, #41723, #14848, #32842, #50889, #28420 ),
 .UNSPECIFIED., .F., .F.,
 ( 4, 2, 2, 2, 2, 2, 1, 2, 2, 2, 2, 2, 2, 2, 2, 2, 2, 2, 2, 2, 2, 2, 2, 2, 2, 2, 2, 1, 2, 2, 2, 2, 2, 2, 2, 2, 2, 2, 2, 2, 2, 2, 2, 2, 2, 2, 2, 2, 1, 2, 2, 2, 2, 2, 4 ),
 ( 0.000000000000000000, 0.01562499999999999653, 0.03125000000000000000, 0.04687500000000000694, 0.06250000000000001388, 0.07812500000000002776, 0.09375000000000002776, 0.1093750000000000416, 0.1250000000000000555, 0.1406250000000000555, 0.1562500000000000555, 0.1718750000000000555, 0.1875000000000000278, 0.2031250000000000278, 0.2187500000000000278, 0.2343750000000000278, 0.2500000000000000555, 0.2656250000000000555, 0.2812500000000000555, 0.2968750000000000555, 0.3125000000000000555, 0.3281250000000000555, 0.3437500000000000555, 0.3750000000000000000, 0.4062500000000000000, 0.4375000000000000000, 0.4687500000000000000, 0.5000000000000000000, 0.5312500000000000000, 0.5625000000000000000, 0.5937500000000000000, 0.6250000000000000000, 0.6562500000000000000, 0.6718750000000000000, 0.6875000000000000000, 0.7031250000000000000, 0.7187500000000000000, 0.7343750000000000000, 0.7499999999999998890, 0.7656249999999998890, 0.7812499999999998890, 0.7968749999999998890, 0.8124999999999998890, 0.8281249999999998890, 0.8437499999999998890, 0.8593749999999998890, 0.8749999999999998890, 0.8906249999999998890, 0.9062499999999998890, 0.9218749999999998890, 0.9374999999999998890, 0.9531249999999998890, 0.9687499999999998890, 0.9843749999999998890, 1.000000000000000000 ),
 .UNSPECIFIED. ) ;
#40955 = DIRECTION ( 'NONE',  ( -1.000000000000000000, 0.000000000000000000, 0.000000000000000000 ) ) ;
#40956 = CARTESIAN_POINT ( 'NONE',  ( 10.46934363224000109, -77.44039367502212201, 5.823135730236001173 ) ) ;
#40957 = CARTESIAN_POINT ( 'NONE',  ( 6.650092250953310469, -78.78900554370888187, -6.429455470012980456 ) ) ;
#40958 = CARTESIAN_POINT ( 'NONE',  ( -5.629566154268999867, -77.14463501420200942, -7.542197886061999590 ) ) ;
#40959 = CARTESIAN_POINT ( 'NONE',  ( -14.00000000000000000, -9.337822431690000258, -5.544480866950999326E-06 ) ) ;
#40960 = DIRECTION ( 'NONE',  ( 0.000000000000000000, -1.000000000000000000, 0.000000000000000000 ) ) ;
#40961 = DIRECTION ( 'NONE',  ( 0.000000000000000000, 1.000000000000000000, 0.000000000000000000 ) ) ;
#40962 = CARTESIAN_POINT ( 'NONE',  ( -11.90928090972364295, -77.96396755025240566, -1.649882979053847176 ) ) ;
#40963 = CARTESIAN_POINT ( 'NONE',  ( -3.804558069882999938, -81.32753455456798974, 1.109648059985999913 ) ) ;
#40964 = CARTESIAN_POINT ( 'NONE',  ( 0.5999999999999999778, -5.000000000000000000, -4.000000000000000000 ) ) ;
#40965 = CARTESIAN_POINT ( 'NONE',  ( -12.43421868118999818, -17.56340276631999942, 1.197355605037999871 ) ) ;
#40966 = CARTESIAN_POINT ( 'NONE',  ( -8.838834764832000701, -55.54999999966999980, 8.838834764832000701 ) ) ;
#40967 = CARTESIAN_POINT ( 'NONE',  ( 1.886823409076000102, -23.76319684362000118, 12.68610076205999881 ) ) ;
#40968 = CARTESIAN_POINT ( 'NONE',  ( 0.07337134444413608014, -81.62075406677425349, 1.323144446007719965 ) ) ;
#40969 = CARTESIAN_POINT ( 'NONE',  ( -2.799999999999999822, -78.69999999999998863, 0.000000000000000000 ) ) ;
#40970 = CARTESIAN_POINT ( 'NONE',  ( -3.854343565295000218, -1.323241823148999963, -1.462699350379000007 ) ) ;
#40971 = DIRECTION ( 'NONE',  ( 1.000000000000000000, 0.000000000000000000, 0.000000000000000000 ) ) ;
#40972 = CARTESIAN_POINT ( 'NONE',  ( 10.42272502865000128, -57.04546192861999998, 7.691893942748999180 ) ) ;
#40973 = CARTESIAN_POINT ( 'NONE',  ( 0.7095316881522687469, -79.51322947404737818, -1.334021238738027249 ) ) ;
#40974 = CARTESIAN_POINT ( 'NONE',  ( -0.05678956088018663473, -78.47885428363976246, 1.248697955453646147 ) ) ;
#40975 = FACE_OUTER_BOUND ( 'NONE', #32575, .T. ) ;
#40976 = CARTESIAN_POINT ( 'NONE',  ( 3.481642061040000069, -3.298138707841000272, 0.1645893813865000055 ) ) ;
#40977 = CARTESIAN_POINT ( 'NONE',  ( -1.250000000000000000, -80.49999999999998579, 0.000000000000000000 ) ) ;
#40978 = CARTESIAN_POINT ( 'NONE',  ( 9.500000000000000000, -78.64999999999999147, 0.000000000000000000 ) ) ;
#40979 = CARTESIAN_POINT ( 'NONE',  ( 7.954951288349001004, -23.25000000000000000, 9.722718241315000398 ) ) ;
#40981 = CARTESIAN_POINT ( 'NONE',  ( 0.9976655664682999580, -78.61019790845699617, 1.007334501387000092 ) ) ;
#40980 = DIRECTION ( 'NONE',  ( -1.000000000000000000, 0.000000000000000000, 0.000000000000000000 ) ) ;
#40982 = CARTESIAN_POINT ( 'NONE',  ( 0.5386432692752000095, -83.11936459712099179, 1.615427185862999826 ) ) ;
#40983 = VERTEX_POINT ( 'NONE', #3016 ) ;
#40984 = CARTESIAN_POINT ( 'NONE',  ( -3.722285329556000111, -83.47246544543099844, 0.5059190862433999847 ) ) ;
#40985 = CARTESIAN_POINT ( 'NONE',  ( -9.932608425312000833, -79.57673028327599241, 6.601450038057999237 ) ) ;
#40986 = CARTESIAN_POINT ( 'NONE',  ( -6.853378677884999881, -80.64520419626960290, -8.675469944580999737 ) ) ;
#40987 = DIRECTION ( 'NONE',  ( 0.000000000000000000, -1.000000000000000000, -4.543461426100999533E-13 ) ) ;
#40988 = CARTESIAN_POINT ( 'NONE',  ( 1.884520266331757066, -85.21354167514409994, -2.882774053612764398 ) ) ;
#40989 = CARTESIAN_POINT ( 'NONE',  ( -10.96060824219999930, -77.31685154495198731, 2.383941600041999731 ) ) ;
#40990 = CARTESIAN_POINT ( 'NONE',  ( 1.750000000000000000, -60.04999999725999515, 12.50000000000000000 ) ) ;
#40991 = DIRECTION ( 'NONE',  ( 0.000000000000000000, 0.000000000000000000, -1.000000000000000000 ) ) ;
#40992 = CARTESIAN_POINT ( 'NONE',  ( -3.250880417296999614, -77.15131824283000128, 12.21627067396000044 ) ) ;
#40993 = FACE_OUTER_BOUND ( 'NONE', #11399, .T. ) ;
#40994 = CARTESIAN_POINT ( 'NONE',  ( -8.060180465563279384, -61.42064870639099894, 9.621709427725253505 ) ) ;
#40995 = CARTESIAN_POINT ( 'NONE',  ( 4.508375518195298248, -81.00000000000001421, -10.10122446274072772 ) ) ;
#40996 = VERTEX_POINT ( 'NONE', #48467 ) ;
#40997 = CARTESIAN_POINT ( 'NONE',  ( 0.1988171392200135945, -80.63513263419274324, -1.518600332402399777 ) ) ;
#40998 = CARTESIAN_POINT ( 'NONE',  ( 3.013969474723999564, -79.34431332859900010, -8.821166524726999469 ) ) ;
#40999 = CARTESIAN_POINT ( 'NONE',  ( 1.750000000000000000, -55.54999999966999980, -12.00000000000000000 ) ) ;
#41000 = DIRECTION ( 'NONE',  ( 1.000000000000000000, 0.000000000000000000, 0.000000000000000000 ) ) ;
#41001 = CARTESIAN_POINT ( 'NONE',  ( -12.64500484464999808, -59.57152778012000027, -1.799490225533999732 ) ) ;
#41002 = AXIS2_PLACEMENT_3D ( 'NONE', #28028, #27735, #1488 ) ;
#41003 = FACE_OUTER_BOUND ( 'NONE', #25824, .T. ) ;
#41004 = ORIENTED_EDGE ( 'NONE', *, *, #9898, .T. ) ;
#41005 = CARTESIAN_POINT ( 'NONE',  ( -1.333681084703000064, -77.87755051491399172, 11.13229884148000082 ) ) ;
#41006 = CARTESIAN_POINT ( 'NONE',  ( 0.000000000000000000, -4.000000000000000000, 0.000000000000000000 ) ) ;
#41007 = ORIENTED_EDGE ( 'NONE', *, *, #22813, .F. ) ;
#41008 = EDGE_CURVE ( 'NONE', #51194, #41515, #15400, .T. ) ;
#41009 = CARTESIAN_POINT ( 'NONE',  ( -1.167939344301158755, -80.57113232371381173, 0.4455473596557876781 ) ) ;
#41010 = AXIS2_PLACEMENT_3D ( 'NONE', #28920, #56384, #19492 ) ;
#41011 = CARTESIAN_POINT ( 'NONE',  ( -7.545891804452000251, -79.95556382368950210, 6.201630566990999682 ) ) ;
#41012 = ORIENTED_EDGE ( 'NONE', *, *, #6138, .T. ) ;
#41013 = CARTESIAN_POINT ( 'NONE',  ( -7.836763323982935958, -54.49488832206737499, 9.850488778788085042 ) ) ;
#41014 = DIRECTION ( 'NONE',  ( 0.000000000000000000, 1.000000000000000000, 0.000000000000000000 ) ) ;
#41015 = CARTESIAN_POINT ( 'NONE',  ( -0.5305471585600000095, -78.30357160033999264, -1.440242834216999945 ) ) ;
#41016 = ORIENTED_EDGE ( 'NONE', *, *, #29620, .T. ) ;
#41017 = CARTESIAN_POINT ( 'NONE',  ( -0.7479529023060000892, -77.74877694988499854, -9.465622776916999825 ) ) ;
#41018 = CARTESIAN_POINT ( 'NONE',  ( 2.269106295766999856E-14, -92.33215535459000023, -9.760776772971999193 ) ) ;
#41019 = CARTESIAN_POINT ( 'NONE',  ( 1.248546286058870969, -80.34460560522650496, -0.09467261385860081813 ) ) ;
#41020 = CARTESIAN_POINT ( 'NONE',  ( 12.47598273373999866, -77.80972615780000012, -3.494640443823999743 ) ) ;
#41021 = CARTESIAN_POINT ( 'NONE',  ( -3.548349909811000291, -78.43735717349129288, 5.104432642529999417E-09 ) ) ;
#41022 = ADVANCED_FACE ( 'NONE', ( #11591 ), #35799, .T. ) ;
#41023 = CARTESIAN_POINT ( 'NONE',  ( 9.177586578508210025, -79.86080595070167476, 1.207628619463350983 ) ) ;
#41024 = CARTESIAN_POINT ( 'NONE',  ( -1.749899258077674435, -23.38716848763002076, 12.55433901290729182 ) ) ;
#41025 = ORIENTED_EDGE ( 'NONE', *, *, #18621, .F. ) ;
#41026 = CARTESIAN_POINT ( 'NONE',  ( 8.300970689365438915, -77.59166666666666856, 4.784380313523563188 ) ) ;
#41027 = CARTESIAN_POINT ( 'NONE',  ( -1.771468677314999907, -75.93849150267999448, 12.18184739844999953 ) ) ;
#41028 = CARTESIAN_POINT ( 'NONE',  ( -1.312293291923000149, -79.89443611377700449, -0.7594922433479999180 ) ) ;
#41029 = B_SPLINE_SURFACE_WITH_KNOTS ( 'NONE', 3, 3, ( 
 ( #27103, #17376, #30649, #40402 ),
 ( #21799, #53106, #22689, #48972 ),
 ( #44533, #13529, #4691, #27239 ),
 ( #53991, #12934, #4391, #30359 ),
 ( #40701, #39521, #17974, #18273 ),
 ( #53693, #36265, #48400, #13231 ),
 ( #8815, #8513, #12655, #22391 ),
 ( #7937, #44245, #35966, #17087 ),
 ( #25939, #43964, #8227, #3514 ),
 ( #57526, #21515, #35070, #48683 ),
 ( #26229, #39804, #35363, #30932 ) ),
 .UNSPECIFIED., .F., .F., .F.,
 ( 4, 1, 1, 1, 1, 1, 1, 1, 4 ),
 ( 4, 4 ),
 ( -0.02001474922155999786, 0.000000000000000000, 0.1666666666667000196, 0.3333333333333000081, 0.5000000000000000000, 0.6666666666667000474, 0.8333333333333000637, 1.000000000000000000, 1.020283381528000133 ),
 ( -0.3582002740325999635, 1.358862457854000061 ),
 .UNSPECIFIED. ) ;
#41030 = CARTESIAN_POINT ( 'NONE',  ( -1.839417067126238203, -1.930490702502749345, -3.003034272496980961 ) ) ;
#41031 = CARTESIAN_POINT ( 'NONE',  ( 8.227501432806000992, -61.62538814575999879, -9.516269855012000178 ) ) ;
#41033 = EDGE_CURVE ( 'NONE', #38752, #48909, #4954, .T. ) ;
#41032 = CARTESIAN_POINT ( 'NONE',  ( 2.624826629463999694, -78.87516843985000037, 11.97953966613999910 ) ) ;
#41034 = CARTESIAN_POINT ( 'NONE',  ( -1.750000000001000089, -22.75100836360999779, 12.60354432389999957 ) ) ;
#41035 = CARTESIAN_POINT ( 'NONE',  ( -3.106054822367000146, -86.10000002299598520, 1.382903988153999952 ) ) ;
#41036 = CARTESIAN_POINT ( 'NONE',  ( 2.216541547539999879, -77.23606498579799506, 9.481530790117000507 ) ) ;
#41037 = CARTESIAN_POINT ( 'NONE',  ( 8.051245500302858460, -77.36714086066730545, 9.061184720839335682 ) ) ;
#41038 = DIRECTION ( 'NONE',  ( 0.000000000000000000, -1.000000000000000000, 0.000000000000000000 ) ) ;
#41039 = ADVANCED_FACE ( 'NONE', ( #51381 ), #35172, .F. ) ;
#41040 = VECTOR ( 'NONE', #52679, 1000.000000000000114 ) ;
#41041 = ORIENTED_EDGE ( 'NONE', *, *, #49593, .F. ) ;
#41042 = CARTESIAN_POINT ( 'NONE',  ( 1.318896022268000179, -83.24288869324199425, 0.6457249424517998992 ) ) ;
#41043 = CIRCLE ( 'NONE', #17473, 14.00000000000000000 ) ;
#41044 = CARTESIAN_POINT ( 'NONE',  ( -1.125831293927000099, -79.97334218465999811, 0.7473110439769999891 ) ) ;
#41045 = CARTESIAN_POINT ( 'NONE',  ( -0.3271848554491046945, -79.39583333333331439, 1.217465845835393301 ) ) ;
#41046 = CARTESIAN_POINT ( 'NONE',  ( 9.148490208346998998, -77.80416746146400442, 7.734416031130999514 ) ) ;
#41047 = CARTESIAN_POINT ( 'NONE',  ( 9.218641115533358743, -77.00000000000001421, -2.097425539381363446 ) ) ;
#41048 = VECTOR ( 'NONE', #26217, 1000.000000000000000 ) ;
#41049 = CARTESIAN_POINT ( 'NONE',  ( 11.75393452337000078, -77.31272526409898660, -2.068948229565000130 ) ) ;
#41050 = CARTESIAN_POINT ( 'NONE',  ( 4.316051676898999823, -78.84824415034599099, 8.712949996777000550 ) ) ;
#41051 = CARTESIAN_POINT ( 'NONE',  ( -5.310864497047000476, -77.62841853088399091, 8.034172531070000289 ) ) ;
#41052 = CARTESIAN_POINT ( 'NONE',  ( 0.8678127655509034755, -76.06901340928149580, 11.71984293853029691 ) ) ;
#41053 = CARTESIAN_POINT ( 'NONE',  ( -2.637902738039999750, -79.92101177224829200, 10.59324478783000067 ) ) ;
#41054 = CARTESIAN_POINT ( 'NONE',  ( 3.112536659741981016, -86.02148120184399716, -1.385790604991043118 ) ) ;
#41055 = EDGE_LOOP ( 'NONE', ( #6183, #32469, #51899, #24053 ) ) ;
#41056 = CARTESIAN_POINT ( 'NONE',  ( 12.21199139565999481, -76.31004809983465975, 1.550091862394999298 ) ) ;
#41057 = CARTESIAN_POINT ( 'NONE',  ( -0.03487147506507188438, -78.39678895079168797, -3.699835669024340579 ) ) ;
#41058 = CARTESIAN_POINT ( 'NONE',  ( 1.407171709420391936, -77.36458333333330017, 10.75000000000000178 ) ) ;
#41059 = CARTESIAN_POINT ( 'NONE',  ( 3.176617583302000281, -79.84208835542798965, 10.50586082162000068 ) ) ;
#41060 = CARTESIAN_POINT ( 'NONE',  ( -0.6454797251260506741, -17.11193487860159479, -12.50471521368209871 ) ) ;
#41061 = CARTESIAN_POINT ( 'NONE',  ( 12.00000000000000000, -77.64999999999999147, 0.000000000000000000 ) ) ;
#41062 = DIRECTION ( 'NONE',  ( 1.000000000000000000, 0.000000000000000000, 0.000000000000000000 ) ) ;
#41063 = CARTESIAN_POINT ( 'NONE',  ( 7.647094085193999469, -18.63104695440999947, -10.00844048070000092 ) ) ;
#41064 = CARTESIAN_POINT ( 'NONE',  ( 9.298479816476996618, -17.11187382770974352, 8.385858173856171049 ) ) ;
#41065 = ORIENTED_EDGE ( 'NONE', *, *, #47000, .F. ) ;
#41066 = CARTESIAN_POINT ( 'NONE',  ( -9.010285311145000975, -78.75895807477898813, -6.562724981485000164 ) ) ;
#41067 = DIRECTION ( 'NONE',  ( 0.000000000000000000, -1.000000000000000000, -5.033011044969999542E-14 ) ) ;
#41068 = CARTESIAN_POINT ( 'NONE',  ( -1.356476828458505590, -79.66581317784307714, -11.75740360620952352 ) ) ;
#41069 = CARTESIAN_POINT ( 'NONE',  ( -2.171317872500211799, -78.40681307385641219, 3.601143492177988570 ) ) ;
#41070 = CARTESIAN_POINT ( 'NONE',  ( 11.34395419804827299, -76.42888099978775074, -3.068742979946195160 ) ) ;
#41071 = CARTESIAN_POINT ( 'NONE',  ( -10.72788417900999924, -78.78770885299998383, 2.643935454766999982 ) ) ;
#41072 = CARTESIAN_POINT ( 'NONE',  ( -12.50386430447168351, -54.01495396579433361, -0.8574436029508151202 ) ) ;
#41073 = LINE ( 'NONE', #28058, #46900 ) ;
#41074 = FACE_OUTER_BOUND ( 'NONE', #54173, .T. ) ;
#41075 = CARTESIAN_POINT ( 'NONE',  ( 7.788616085187482163, -78.76231864851705211, 7.733387248865380315 ) ) ;
#41076 = CONICAL_SURFACE ( 'NONE', #50528, 1.546875000130000011, 0.7853981633972997312 ) ;
#41077 = DIRECTION ( 'NONE',  ( -0.7071067811865474617, 0.000000000000000000, 0.7071067811865474617 ) ) ;
#41078 = VERTEX_POINT ( 'NONE', #6490 ) ;
#41079 = EDGE_LOOP ( 'NONE', ( #25958, #43311, #44415, #11630 ) ) ;
#41080 = CARTESIAN_POINT ( 'NONE',  ( 9.963291278272981444, -78.81944231393819678, -4.036724254922090083 ) ) ;
#41081 = DIRECTION ( 'NONE',  ( -0.7071067811865475727, 0.000000000000000000, -0.7071067811865475727 ) ) ;
#41082 = VERTEX_POINT ( 'NONE', #32461 ) ;
#41083 = CARTESIAN_POINT ( 'NONE',  ( -9.831705185582000794, -76.21046601319852698, 5.330239850319000716 ) ) ;
#41084 = CARTESIAN_POINT ( 'NONE',  ( 7.758655887903000092, -24.15078616243999932, 9.996711280983999970 ) ) ;
#41085 = CARTESIAN_POINT ( 'NONE',  ( -10.95663201459999847, -78.13183842717499772, 1.286059498161999937 ) ) ;
#41086 = CARTESIAN_POINT ( 'NONE',  ( 9.029867227928999540, -62.13262194258000193, 9.038867509651000276 ) ) ;
#41088 = ADVANCED_FACE ( 'NONE', ( #1793 ), #42516, .F. ) ;
#41087 = CARTESIAN_POINT ( 'NONE',  ( 0.000000000000000000, -18.75000000000000000, 12.50000000000000000 ) ) ;
#41089 = CARTESIAN_POINT ( 'NONE',  ( -11.96294582457251110, -78.04565904830035095, 0.6386850134296362391 ) ) ;
#41090 = CARTESIAN_POINT ( 'NONE',  ( 10.49311453041000064, -80.05515156828879242, -3.963918880051000126 ) ) ;
#41091 = CARTESIAN_POINT ( 'NONE',  ( 9.536720110793080352, -80.99999999999998579, 5.361087519179783101 ) ) ;
#41092 = ORIENTED_EDGE ( 'NONE', *, *, #58202, .F. ) ;
#41093 = FACE_OUTER_BOUND ( 'NONE', #55988, .T. ) ;
#41094 = ORIENTED_EDGE ( 'NONE', *, *, #13103, .F. ) ;
#41095 = CARTESIAN_POINT ( 'NONE',  ( 2.852630567793418059, -77.45022947118953027, 8.799033844256978654 ) ) ;
#41096 = CARTESIAN_POINT ( 'NONE',  ( 6.574300740938999077, -77.60591217881798798, -8.869200617850999890 ) ) ;
#41097 = DIRECTION ( 'NONE',  ( 0.7071067811865474617, 0.000000000000000000, -0.7071067811865474617 ) ) ;
#41098 = CARTESIAN_POINT ( 'NONE',  ( 3.248345031021000029, -78.23829248593298757, 9.144340540792999406 ) ) ;
#41099 = CARTESIAN_POINT ( 'NONE',  ( -2.177178839649999809, -75.72006215493000525, 12.62074446832999897 ) ) ;
#41100 = CARTESIAN_POINT ( 'NONE',  ( 2.269106295766999856E-14, -92.56607767729998670, 0.000000000000000000 ) ) ;
#41101 = CARTESIAN_POINT ( 'NONE',  ( -0.9156221410628999635, -78.19294195445999662, 1.345473579290000110 ) ) ;
#41102 = FACE_OUTER_BOUND ( 'NONE', #15740, .T. ) ;
#41103 = CARTESIAN_POINT ( 'NONE',  ( 2.542269563431000190, -78.57284911944198313, -10.64070870773999822 ) ) ;
#41104 = CARTESIAN_POINT ( 'NONE',  ( -8.790688707546999936, -24.93813493249999880, -8.797962936834998970 ) ) ;
#41105 = EDGE_CURVE ( 'NONE', #19974, #17032, #19197, .T. ) ;
#41106 = CARTESIAN_POINT ( 'NONE',  ( -7.666647577129732660, -60.55042584425837049, 7.889735440113262221 ) ) ;
#41107 = CARTESIAN_POINT ( 'NONE',  ( 2.619065415988000023, -83.94143147127900306, 2.454433006111999660 ) ) ;
#41108 = ORIENTED_EDGE ( 'NONE', *, *, #3721, .F. ) ;
#41109 = CARTESIAN_POINT ( 'NONE',  ( -6.630296030920000305, -79.79479933005599435, 10.05508639755000111 ) ) ;
#41110 = CARTESIAN_POINT ( 'NONE',  ( 6.004377887672999847, -75.90363824613500299, 9.521041246372998756 ) ) ;
#41111 = CARTESIAN_POINT ( 'NONE',  ( -2.099635473158307786, -77.99077376007581108, 10.54287097477208412 ) ) ;
#41112 = CARTESIAN_POINT ( 'NONE',  ( 4.899854808515000215, -78.29242566852499863, -10.93194800986000104 ) ) ;
#41113 = CARTESIAN_POINT ( 'NONE',  ( -12.70253258979055389, -61.77063167632906726, 0.9890392131111367391 ) ) ;
#41114 = DIRECTION ( 'NONE',  ( 0.000000000000000000, 0.000000000000000000, 1.000000000000000000 ) ) ;
#41115 = CARTESIAN_POINT ( 'NONE',  ( 3.451879464910999840, -86.39318692756698681, -1.536875756006000016 ) ) ;
#41116 = CARTESIAN_POINT ( 'NONE',  ( -5.511117113485999752, -78.15441511928399621, -7.631433854063000233 ) ) ;
#41117 = CARTESIAN_POINT ( 'NONE',  ( 3.654181830570650824, -86.07389998728979208, -1.626946572303439753 ) ) ;
#41118 = CARTESIAN_POINT ( 'NONE',  ( -10.11369910513000114, -76.85660321907299419, 4.686934626122000402 ) ) ;
#41119 = CARTESIAN_POINT ( 'NONE',  ( -9.722718241315000398, -23.44678171330999916, 7.954951288349001004 ) ) ;
#41120 = CARTESIAN_POINT ( 'NONE',  ( -10.13082369059000065, -80.99114675511358996, -4.351272007672999820 ) ) ;
#41121 = ORIENTED_EDGE ( 'NONE', *, *, #14932, .T. ) ;
#41122 = CARTESIAN_POINT ( 'NONE',  ( -9.391369684923001060, -77.13822403538300421, 1.399863080762999923 ) ) ;
#41123 = CARTESIAN_POINT ( 'NONE',  ( 2.972945683522000060, -3.498054798046000169, -2.625398180863999897 ) ) ;
#41124 = CARTESIAN_POINT ( 'NONE',  ( 4.013660496580000903, -78.42022574075399177, -10.47417304634999979 ) ) ;
#41125 = CARTESIAN_POINT ( 'NONE',  ( -9.813193589766999736, -78.84650130276799018, -4.915816122623000162 ) ) ;
#41126 = CARTESIAN_POINT ( 'NONE',  ( 8.652376385601000308, -25.26264602966000083, -9.414489258817999584 ) ) ;
#41127 = FACE_OUTER_BOUND ( 'NONE', #4576, .T. ) ;
#41128 = EDGE_CURVE ( 'NONE', #53170, #31439, #52832, .T. ) ;
#41129 = CARTESIAN_POINT ( 'NONE',  ( 2.244456003428818125, -78.64167492799113290, -10.54596288039670959 ) ) ;
#41130 = CIRCLE ( 'NONE', #10968, 14.00000000000000000 ) ;
#41131 = CARTESIAN_POINT ( 'NONE',  ( -1.831734064479000113, -85.92094503318799070, 3.749003839799999849 ) ) ;
#41132 = CARTESIAN_POINT ( 'NONE',  ( -7.686941364994000381, -20.24527982330999976, -10.48774103564000093 ) ) ;
#41133 = VECTOR ( 'NONE', #10955, 1000.000000000000000 ) ;
#41134 = AXIS2_PLACEMENT_3D ( 'NONE', #26367, #53840, #53539 ) ;
#41135 = CARTESIAN_POINT ( 'NONE',  ( 8.870405106233999248, -53.73036971739000478, -8.878274241729000593 ) ) ;
#41136 = AXIS2_PLACEMENT_3D ( 'NONE', #8074, #26070, #52665 ) ;
#41137 = CARTESIAN_POINT ( 'NONE',  ( -10.03906427447999938, -77.31402055093700199, -5.104033018226999729 ) ) ;
#41138 = DIRECTION ( 'NONE',  ( 0.000000000000000000, -1.000000000000000000, 0.000000000000000000 ) ) ;
#41139 = CARTESIAN_POINT ( 'NONE',  ( -0.5337784322849999930, -79.61183811491999052, -1.207245797014000255 ) ) ;
#41140 = CARTESIAN_POINT ( 'NONE',  ( -0.8405563561534999950, -76.94822717842869508, -9.635375415708001157 ) ) ;
#41141 = CARTESIAN_POINT ( 'NONE',  ( -1.168951575717731561, -82.80464656011996283, -0.9568345469043921803 ) ) ;
#41142 = CARTESIAN_POINT ( 'NONE',  ( -10.75000000000000000, -80.50000000000000000, -1.711887504597999906E-14 ) ) ;
#41143 = CARTESIAN_POINT ( 'NONE',  ( -9.250000000000000000, -77.99999999999998579, 0.000000000000000000 ) ) ;
#41144 = CARTESIAN_POINT ( 'NONE',  ( -7.596835002782709623, -77.85208333333333997, -5.838193839761696147 ) ) ;
#41145 = VERTEX_POINT ( 'NONE', #19790 ) ;
#41146 = CARTESIAN_POINT ( 'NONE',  ( 1.206984821263439533, -81.82940592443240746, -0.3247830993265489186 ) ) ;
#41147 = CARTESIAN_POINT ( 'NONE',  ( 6.233047529871999615, -78.98050366622999263, 9.960502923565000444 ) ) ;
#41148 = CARTESIAN_POINT ( 'NONE',  ( 5.888733633253000477, -78.49219514392800079, -9.599841314972998418 ) ) ;
#41149 = DIRECTION ( 'NONE',  ( -0.7026410690473250398, 0.1122098755728047209, -0.7026410690473250398 ) ) ;
#41150 = ORIENTED_EDGE ( 'NONE', *, *, #9566, .T. ) ;
#41151 = ORIENTED_EDGE ( 'NONE', *, *, #22427, .F. ) ;
#41152 = DIRECTION ( 'NONE',  ( 0.000000000000000000, 1.000000000000000000, 0.000000000000000000 ) ) ;
#41153 = VERTEX_POINT ( 'NONE', #37783 ) ;
#41154 = DIRECTION ( 'NONE',  ( 1.000000000000000000, 0.000000000000000000, 0.000000000000000000 ) ) ;
#41155 = ORIENTED_EDGE ( 'NONE', *, *, #7953, .T. ) ;
#41156 = CARTESIAN_POINT ( 'NONE',  ( -1.929975092517999924, -18.79892743736000327, 12.72537404210999945 ) ) ;
#41157 = CARTESIAN_POINT ( 'NONE',  ( 2.228740036544774483, -80.74270832256439689, -2.625067772272801747 ) ) ;
#41158 = EDGE_CURVE ( 'NONE', #2598, #57897, #55210, .T. ) ;
#41159 = CARTESIAN_POINT ( 'NONE',  ( 6.068451062995785072, -78.28202394152809518, -6.981743368066175570 ) ) ;
#41160 = CARTESIAN_POINT ( 'NONE',  ( -1.250000000000000000, -79.00000000000000000, 0.000000000000000000 ) ) ;
#41161 = CARTESIAN_POINT ( 'NONE',  ( -7.638406141627999801, -78.40188750088999825, -9.335002989230998693 ) ) ;
#41162 = ORIENTED_EDGE ( 'NONE', *, *, #3583, .F. ) ;
#41164 = VERTEX_POINT ( 'NONE', #28327 ) ;
#41163 = EDGE_CURVE ( 'NONE', #43521, #18438, #1419, .T. ) ;
#41165 = DIRECTION ( 'NONE',  ( 0.000000000000000000, 1.000000000000000000, 0.000000000000000000 ) ) ;
#41166 = CARTESIAN_POINT ( 'NONE',  ( -12.56594317991999965, -60.04999999381999487, -1.750000000001000089 ) ) ;
#41167 = LINE ( 'NONE', #18738, #50681 ) ;
#41168 = CIRCLE ( 'NONE', #40231, 11.59999999999999964 ) ;
#41169 = CARTESIAN_POINT ( 'NONE',  ( 0.000000000000000000, -2.900000000000000355, 0.000000000000000000 ) ) ;
#41170 = CARTESIAN_POINT ( 'NONE',  ( -0.5548610165507998904, -77.82999307588899285, -9.688283574444998436 ) ) ;
#41171 = DIRECTION ( 'NONE',  ( 0.000000000000000000, 1.000000000000000000, 0.000000000000000000 ) ) ;
#41172 = CARTESIAN_POINT ( 'NONE',  ( -10.07722254369999959, -20.25199022618999933, 7.718368845809999712 ) ) ;
#41173 = AXIS2_PLACEMENT_3D ( 'NONE', #47527, #29187, #15914 ) ;
#41174 = CARTESIAN_POINT ( 'NONE',  ( -10.38133291898000188, -77.78174472164999997, 7.485792156039000389 ) ) ;
#41175 = CARTESIAN_POINT ( 'NONE',  ( -0.7081060581029999801, -80.22830095821998952, -1.286481228505000018 ) ) ;
#41176 = CARTESIAN_POINT ( 'NONE',  ( 9.091459715836720079, -77.32174693750340566, 2.567140442679551438 ) ) ;
#41177 = EDGE_CURVE ( 'NONE', #44267, #17252, #46378, .T. ) ;
#41178 = AXIS2_PLACEMENT_3D ( 'NONE', #4961, #27383, #32386 ) ;
#41179 = CARTESIAN_POINT ( 'NONE',  ( 0.000000000000000000, -18.84999999999999787, -12.00000000000000000 ) ) ;
#41180 = CARTESIAN_POINT ( 'NONE',  ( 4.116256581921999391, -80.89818977615198037, -0.6830113048311999835 ) ) ;
#41181 = TOROIDAL_SURFACE ( 'NONE', #46857, 13.50000000000000000, 0.5000000000000000000 ) ;
#41182 = CARTESIAN_POINT ( 'NONE',  ( -9.421357847594000745, -80.31228291220008941, -6.176342950743000770 ) ) ;
#41183 = CARTESIAN_POINT ( 'NONE',  ( -3.063214743671000218, -79.10658667140098999, -9.307899183505000451 ) ) ;
#41184 = DIRECTION ( 'NONE',  ( -1.000000000000000000, 0.000000000000000000, 0.000000000000000000 ) ) ;
#41185 = CARTESIAN_POINT ( 'NONE',  ( 10.38043817655364442, -76.18020833308295892, -5.983885801651409153 ) ) ;
#41186 = CARTESIAN_POINT ( 'NONE',  ( -0.6568659331174000471, -78.13786977406140011, 1.160647793301999853 ) ) ;
#41187 = LINE ( 'NONE', #27011, #761 ) ;
#41188 = CARTESIAN_POINT ( 'NONE',  ( 12.00000000000000000, -79.25000000000000000, 1.072514965728000067E-08 ) ) ;
#41189 = CARTESIAN_POINT ( 'NONE',  ( 1.781953555039999859, -3.015773310596999934, -3.363141973650999983 ) ) ;
#41190 = CARTESIAN_POINT ( 'NONE',  ( 10.00419727105263057, -77.19999999999998863, -4.081745277459294385 ) ) ;
#41191 = ORIENTED_EDGE ( 'NONE', *, *, #24298, .T. ) ;
#41192 = DIRECTION ( 'NONE',  ( 0.000000000000000000, -1.000000000000000000, 0.000000000000000000 ) ) ;
#41193 = CARTESIAN_POINT ( 'NONE',  ( 8.171144579307879852, -60.14010097496868212, -7.364280830342240236 ) ) ;
#41194 = CARTESIAN_POINT ( 'NONE',  ( -1.000000000000000000, -82.50000000000000000, 0.000000000000000000 ) ) ;
#41195 = CARTESIAN_POINT ( 'NONE',  ( 1.677867312386000176, -79.96794690487999446, -9.605949203754001076 ) ) ;
#41196 = CARTESIAN_POINT ( 'NONE',  ( -9.234979314279001983, -77.07954422446000819, -9.168119495123999485 ) ) ;
#41197 = CARTESIAN_POINT ( 'NONE',  ( -8.938323291245980684, -79.55317274765927493, 5.972287786095013651 ) ) ;
#41198 = FACE_OUTER_BOUND ( 'NONE', #51336, .T. ) ;
#41199 = FACE_OUTER_BOUND ( 'NONE', #56484, .T. ) ;
#41200 = VERTEX_POINT ( 'NONE', #15055 ) ;
#41201 = PLANE ( 'NONE',  #28768 ) ;
#41202 = CARTESIAN_POINT ( 'NONE',  ( 1.956384561158000190, -77.10404663294119132, 10.99260293793000010 ) ) ;
#41203 = CARTESIAN_POINT ( 'NONE',  ( 1.070496197449000153, -81.10360888163698689, 0.9153310235335999634 ) ) ;
#41204 = CARTESIAN_POINT ( 'NONE',  ( 7.653559626096999580, -23.29848884437999956, -10.01235002622999914 ) ) ;
#41205 = CARTESIAN_POINT ( 'NONE',  ( -0.1509935689429000305, -78.33319979694698532, 9.520902119764999227 ) ) ;
#41207 = CARTESIAN_POINT ( 'NONE',  ( -1.182840957218999955, -1.383876846447999798, -3.838043326965000279 ) ) ;
#41206 = CARTESIAN_POINT ( 'NONE',  ( 3.648109280413999844, -82.37817607281098731, 1.936498112586999998 ) ) ;
#41208 = CARTESIAN_POINT ( 'NONE',  ( -1.799475295154000065, -58.55083378327000077, -12.69619287811999797 ) ) ;
#41209 = CARTESIAN_POINT ( 'NONE',  ( -1.200597545982000192, -80.69206026912699770, -0.5467811674232999630 ) ) ;
#41210 = ORIENTED_EDGE ( 'NONE', *, *, #37643, .F. ) ;
#41211 = AXIS2_PLACEMENT_3D ( 'NONE', #22951, #40961, #2987 ) ;
#41212 = EDGE_CURVE ( 'NONE', #6548, #32058, #57024, .T. ) ;
#41213 = DIRECTION ( 'NONE',  ( -1.000000000000000000, -6.386283326366000088E-09, -1.411440692003999935E-10 ) ) ;
#41214 = CARTESIAN_POINT ( 'NONE',  ( 0.3926218265389221362, -79.04583333333334849, -1.460959015002473160 ) ) ;
#41215 = CONICAL_SURFACE ( 'NONE', #35400, 0.6999999997694995590, 0.7853981633972997312 ) ;
#41216 = ORIENTED_EDGE ( 'NONE', *, *, #4006, .T. ) ;
#41217 = DIRECTION ( 'NONE',  ( 0.000000000000000000, -1.000000000000000000, 0.000000000000000000 ) ) ;
#41218 = PRESENTATION_STYLE_ASSIGNMENT (( #32339 ) ) ;
#41219 = LINE ( 'NONE', #808, #57687 ) ;
#41220 = VECTOR ( 'NONE', #35393, 1000.000000000000000 ) ;
#41221 = EDGE_LOOP ( 'NONE', ( #31415, #22327, #56677, #25759 ) ) ;
#41222 = CARTESIAN_POINT ( 'NONE',  ( -7.660291894363999710, -78.62096101391799152, 9.301381605274000819 ) ) ;
#41223 = AXIS2_PLACEMENT_3D ( 'NONE', #40563, #9563, #22552 ) ;
#41224 = ORIENTED_EDGE ( 'NONE', *, *, #33890, .F. ) ;
#41225 = ORIENTED_EDGE ( 'NONE', *, *, #40532, .T. ) ;
#41226 = CARTESIAN_POINT ( 'NONE',  ( -2.991231916151877002, -2.632707418491854856, -1.269656187733815056 ) ) ;
#41227 = CARTESIAN_POINT ( 'NONE',  ( -6.014612645882658093, -76.48278618361135273, -10.41488065623265946 ) ) ;
#41228 = CARTESIAN_POINT ( 'NONE',  ( 9.151322089608749266, -79.17128379080990896, 2.562544536898030412 ) ) ;
#41229 = EDGE_LOOP ( 'NONE', ( #34517, #41953, #49364, #8692, #46838 ) ) ;
#41230 = CARTESIAN_POINT ( 'NONE',  ( 0.8836238660468611616, -82.78814780667313755, -0.8835844391709938295 ) ) ;
#41232 = EDGE_CURVE ( 'NONE', #53789, #31838, #51959, .T. ) ;
#41231 = ORIENTED_EDGE ( 'NONE', *, *, #13476, .T. ) ;
#41233 = CARTESIAN_POINT ( 'NONE',  ( 1.618935784642568265, -18.07248831326923977, 12.52134385800272121 ) ) ;
#41234 = CARTESIAN_POINT ( 'NONE',  ( 8.240271889161402186, -78.05562457600899506, -5.125597231812675680 ) ) ;
#41235 = DIRECTION ( 'NONE',  ( 0.9936845293270585300, -0.1122098755727947705, 0.000000000000000000 ) ) ;
#41236 = CARTESIAN_POINT ( 'NONE',  ( -1.249999996278000181, -76.50000000037098857, -0.4999999996289999915 ) ) ;
#41237 = CARTESIAN_POINT ( 'NONE',  ( -13.63885489310999510, -19.21421830981000056, 7.254376133916000668 ) ) ;
#41238 = CARTESIAN_POINT ( 'NONE',  ( 5.177752511601999785, -76.53501262057798726, 9.912858493839999952 ) ) ;
#41239 = PLANE ( 'NONE',  #23000 ) ;
#41240 = CARTESIAN_POINT ( 'NONE',  ( -3.250000000000000000, -3.000000000000000000, 0.000000000000000000 ) ) ;
#41241 = CARTESIAN_POINT ( 'NONE',  ( -7.641012305241000391, -60.08917723397000543, -10.18589226633000067 ) ) ;
#41242 = ADVANCED_FACE ( 'NONE', ( #53382 ), #42053, .F. ) ;
#41243 = CARTESIAN_POINT ( 'NONE',  ( 7.846823748142760735, -78.80564564162774843, -4.898151885573968300 ) ) ;
#41244 = CARTESIAN_POINT ( 'NONE',  ( 10.43984081968398492, -76.48826064512984146, 5.458517345968248335 ) ) ;
#41245 = CARTESIAN_POINT ( 'NONE',  ( 0.5705388283887262713, -23.34010097528690508, -10.98520465578131677 ) ) ;
#41246 = CARTESIAN_POINT ( 'NONE',  ( -1.248430190247999949, -79.13035038635399587, 0.06262635289305999720 ) ) ;
#41247 = EDGE_CURVE ( 'NONE', #9865, #34390, #7045, .T. ) ;
#41248 = CARTESIAN_POINT ( 'NONE',  ( -5.640425023195567711, -80.18229393084122592, -9.443705758514129300 ) ) ;
#41249 = CARTESIAN_POINT ( 'NONE',  ( 11.55970134427844975, -78.22637299551007573, 3.502838489863109750 ) ) ;
#41250 = VECTOR ( 'NONE', #536, 1000.000000000000000 ) ;
#41251 = CARTESIAN_POINT ( 'NONE',  ( 0.5296260211451999655, -78.80228455456848735, -3.927530026132000529 ) ) ;
#41252 = CARTESIAN_POINT ( 'NONE',  ( 0.7029086986541999149, -77.56231332859900363, 9.627002478265000107 ) ) ;
#41253 = CARTESIAN_POINT ( 'NONE',  ( -9.254388464354001087, -79.90752053325199711, 5.469807505829999528 ) ) ;
#41254 = CARTESIAN_POINT ( 'NONE',  ( 0.000000000000000000, -90.35000000009100063, -9.649999999909001147 ) ) ;
#41255 = CARTESIAN_POINT ( 'NONE',  ( -1.933504092460000212, -23.40406847274999791, 12.70940235707999832 ) ) ;
#41256 = CARTESIAN_POINT ( 'NONE',  ( -0.9808057187987175851, -81.80885307972523890, -0.8911311466870025511 ) ) ;
#41257 = CARTESIAN_POINT ( 'NONE',  ( -0.6349925544693003632, -78.01682879507401935, 1.107199314832773451 ) ) ;
#41258 = CARTESIAN_POINT ( 'NONE',  ( 3.784441966891999964, -1.714444768728000001, -0.1949150922344000114 ) ) ;
#41259 = CARTESIAN_POINT ( 'NONE',  ( 0.000000000000000000, -74.70999999999999375, 0.000000000000000000 ) ) ;
#41260 = CARTESIAN_POINT ( 'NONE',  ( 8.027497949466866345, -79.80879597959544469, -4.635833453492248957 ) ) ;
#41261 = AXIS2_PLACEMENT_3D ( 'NONE', #11042, #42615, #2181 ) ;
#41262 = CARTESIAN_POINT ( 'NONE',  ( 10.24998526315000014, -58.55083378327000077, 7.705142895592000052 ) ) ;
#41263 = CARTESIAN_POINT ( 'NONE',  ( -0.02856026855508699350, -79.72578953835795801, 1.512310964717682449 ) ) ;
#41264 = CARTESIAN_POINT ( 'NONE',  ( -0.5999999999999999778, -18.84999999999000053, -11.79999999999999893 ) ) ;
#41265 = AXIS2_PLACEMENT_3D ( 'NONE', #2852, #56581, #48884 ) ;
#41266 = CARTESIAN_POINT ( 'NONE',  ( -3.398324506668000122, -2.562221200086999939, -0.7749863891880000022 ) ) ;
#41267 = CARTESIAN_POINT ( 'NONE',  ( -2.402886566874598451, -77.34315645986228560, 10.56757644837470700 ) ) ;
#41268 = FACE_OUTER_BOUND ( 'NONE', #14214, .T. ) ;
#41269 = ADVANCED_FACE ( 'NONE', ( #7293, #15866 ), #16447, .F. ) ;
#41271 = CARTESIAN_POINT ( 'NONE',  ( 0.7144648680787000217, -78.51673172604100159, -1.337341431498000111 ) ) ;
#41270 = LINE ( 'NONE', #8800, #38303 ) ;
#41272 = CARTESIAN_POINT ( 'NONE',  ( -1.436129866501999919, -82.17181889680999518, 0.6722556991877999266 ) ) ;
#41273 = ORIENTED_EDGE ( 'NONE', *, *, #26831, .T. ) ;
#41274 = CARTESIAN_POINT ( 'NONE',  ( 1.964367198619000110, -82.87507450217398741, 3.004155151946999780 ) ) ;
#41275 = CARTESIAN_POINT ( 'NONE',  ( 7.666466404017000968, -80.02291679501679766, 7.955254905497999296 ) ) ;
#41276 = CARTESIAN_POINT ( 'NONE',  ( -9.260506811358984791, -80.00000000000000000, -0.7327802946142877305 ) ) ;
#41277 = CARTESIAN_POINT ( 'NONE',  ( -1.308541769128729326, -84.98229167586391952, -3.186053244962748110 ) ) ;
#41278 = DIRECTION ( 'NONE',  ( 0.000000000000000000, -1.000000000000000000, 0.000000000000000000 ) ) ;
#41279 = FACE_OUTER_BOUND ( 'NONE', #32335, .T. ) ;
#41280 = CARTESIAN_POINT ( 'NONE',  ( -1.228039281160999918, -77.87287857533000590, -12.58161828305999919 ) ) ;
#41281 = CARTESIAN_POINT ( 'NONE',  ( 1.692299031616999905, -79.40949596206999672, -9.745343228177999251 ) ) ;
#41282 = CARTESIAN_POINT ( 'NONE',  ( -0.9736830274145173991, -76.99999999999998579, 9.250386169343817855 ) ) ;
#41283 = ORIENTED_EDGE ( 'NONE', *, *, #7759, .T. ) ;
#41284 = EDGE_CURVE ( 'NONE', #11183, #27162, #33852, .T. ) ;
#41285 = CARTESIAN_POINT ( 'NONE',  ( 1.930860503447785925, -55.02582494032501614, -12.72930866328045418 ) ) ;
#41286 = CARTESIAN_POINT ( 'NONE',  ( -7.919595949288999570, -59.94999999969000015, -8.768124086712999699 ) ) ;
#41287 = CARTESIAN_POINT ( 'NONE',  ( -2.753235971857820097, -75.80574547360328097, -11.46018561868001306 ) ) ;
#41288 = ADVANCED_FACE ( 'NONE', ( #25582 ), #29427, .F. ) ;
#41289 = CARTESIAN_POINT ( 'NONE',  ( 1.500000000000001110, -78.63958333333334849, -0.1963495408493590721 ) ) ;
#41290 = CARTESIAN_POINT ( 'NONE',  ( -12.50386430450149433, -17.21495396633332575, -0.8574436033227620380 ) ) ;
#41291 = B_SPLINE_CURVE_WITH_KNOTS ( 'NONE', 3,
 ( #19086, #55092, #39407, #34956, #43266, #25823, #56549, #16110 ),
 .UNSPECIFIED., .F., .F.,
 ( 4, 2, 2, 4 ),
 ( 0.000000000000000000, 0.4999999999999996669, 0.7499999999999997780, 1.000000000000000000 ),
 .UNSPECIFIED. ) ;
#41292 = DIRECTION ( 'NONE',  ( 0.9936845293270585300, 0.1122098755727947705, 0.000000000000000000 ) ) ;
#41293 = ORIENTED_EDGE ( 'NONE', *, *, #49269, .F. ) ;
#41294 = CARTESIAN_POINT ( 'NONE',  ( -3.162453476786999840, -78.43086335765900685, -11.86569286591000072 ) ) ;
#41295 = CARTESIAN_POINT ( 'NONE',  ( -6.151115499150000332, -77.13436266505908634, -9.032717438718000480 ) ) ;
#41296 = CARTESIAN_POINT ( 'NONE',  ( -1.931087888049999979, -18.68415522710999710, 12.71658889741000031 ) ) ;
#41297 = ORIENTED_EDGE ( 'NONE', *, *, #30759, .F. ) ;
#41298 = ORIENTED_EDGE ( 'NONE', *, *, #6663, .T. ) ;
#41299 = CARTESIAN_POINT ( 'NONE',  ( -1.144396127583604317, -80.56701752473904321, 0.5034462585138648194 ) ) ;
#41300 = CARTESIAN_POINT ( 'NONE',  ( 9.647254834573999460, -80.24781774801149936, -1.526580663425000095 ) ) ;
#41301 = VERTEX_POINT ( 'NONE', #17020 ) ;
#41302 = DIRECTION ( 'NONE',  ( -0.7071067811865474617, 0.000000000000000000, -0.7071067811865474617 ) ) ;
#41303 = CARTESIAN_POINT ( 'NONE',  ( 9.175573575508092716, -25.22695822358256024, -8.792784719773246493 ) ) ;
#41304 = CARTESIAN_POINT ( 'NONE',  ( 1.532709587175000054, -78.46086630968000009, 0.08112354839639000781 ) ) ;
#41305 = ORIENTED_EDGE ( 'NONE', *, *, #17291, .T. ) ;
#41306 = CARTESIAN_POINT ( 'NONE',  ( 4.574312611392000072, -77.40494805011499579, 8.320643751074999983 ) ) ;
#41307 = CARTESIAN_POINT ( 'NONE',  ( 0.000000000000000000, -52.69905023022000279, 0.000000000000000000 ) ) ;
#41308 = STYLED_ITEM ( 'NONE', ( #34899 ), #16630 ) ;
#41309 = CARTESIAN_POINT ( 'NONE',  ( 10.36597025940959327, -18.22476146848570977, -7.635927901519359295 ) ) ;
#41310 = PLANE ( 'NONE',  #13803 ) ;
#41311 = CARTESIAN_POINT ( 'NONE',  ( -9.596002108778161954, -78.85208333333332575, -7.374560639698982456 ) ) ;
#41312 = CARTESIAN_POINT ( 'NONE',  ( 8.949233952815241366, -79.87044664050942799, 2.340432196254297548 ) ) ;
#41313 = CARTESIAN_POINT ( 'NONE',  ( -1.407839100258019949, -79.32013530975854110, 0.5457514781034552565 ) ) ;
#41314 = CARTESIAN_POINT ( 'NONE',  ( -1.161982140497694216, -79.89479165893936852, 3.880497637639665154 ) ) ;
#41315 = ORIENTED_EDGE ( 'NONE', *, *, #56415, .T. ) ;
#41316 = CARTESIAN_POINT ( 'NONE',  ( -5.838193839761721016, -77.72708333333332575, 7.596835002782687418 ) ) ;
#41317 = B_SPLINE_CURVE_WITH_KNOTS ( 'NONE', 3,
 ( #10837, #42123, #31853, #28813, #47155, #13562, #19982, #46570, #323, #46861, #6389, #6685, #50987, #22719, #24404, #15245, #42419, #1689, #24693, #33537, #19392, #5802, #49894, #1988, #45170, #19681, #54317, #37969, #4720, #51574, #6094, #10538, #37681, #51283, #33239, #11131, #37384, #55994, #25, #15540, #40732, #29109, #35996, #9438, #1398, #49600, #54021, #9148, #27132, #18301, #36294, #13857, #27429, #45464, #23808, #41824, #55400, #14947, #32945, #28521, #7838, #39426, #43571, #43285, #11705 ),
 .UNSPECIFIED., .F., .F.,
 ( 4, 1, 1, 1, 1, 1, 1, 1, 1, 1, 1, 1, 1, 1, 1, 1, 1, 1, 1, 1, 1, 1, 1, 1, 1, 1, 1, 1, 1, 1, 1, 1, 1, 1, 1, 1, 1, 1, 1, 1, 1, 1, 1, 1, 1, 1, 1, 1, 1, 1, 1, 1, 1, 1, 1, 1, 1, 1, 1, 1, 1, 1, 4 ),
 ( 0.000000000000000000, 0.01249973505302583512, 0.02874974388395608663, 0.04499975271488634160, 0.06124976154581659310, 0.07749977037674685154, 0.09374977920767710304, 0.1099997880386073545, 0.1262497968695376060, 0.1424998057004678575, 0.1587498145313981091, 0.1749998233623283606, 0.1912498321932586398, 0.2074998410241888636, 0.2237498498551191428, 0.2399998586860493666, 0.2562498675169795903, 0.2724998763479098973, 0.2887498851788401488, 0.3049998940097703448, 0.3212499028407005963, 0.3374999116716309033, 0.3537499205025611548, 0.3699999293334913508, 0.3862499381644216023, 0.4024999469953519093, 0.4187499558262821608, 0.4349999646572124123, 0.4512499734881426083, 0.4674999823190729153, 0.4837499911500031669, 0.4999999999809334184, 0.5162500088118636699, 0.5325000176427939769, 0.5487500264737241729, 0.5650000353046543689, 0.5812500441355847869, 0.5975000529665149829, 0.6137500617974452899, 0.6300000706283754859, 0.6462500794593056819, 0.6625000882902359889, 0.6787500971211661849, 0.6950001059520964919, 0.7112501147830267989, 0.7275001236139569949, 0.7437501324448873019, 0.7600001412758174979, 0.7762501501067478049, 0.7925001589376780009, 0.8087501677686081969, 0.8250001765995385039, 0.8412501854304688109, 0.8575001942613991179, 0.8737502030923293139, 0.8900002119232595099, 0.9062502207541898169, 0.9225002295851200129, 0.9387502384160503199, 0.9550002472469805159, 0.9712502560779107119, 0.9875002649088411300, 1.000000000000000000 ),
 .UNSPECIFIED. ) ;
#41318 = CARTESIAN_POINT ( 'NONE',  ( -6.024415200221000077, -76.39836206569999888, 10.73507988388000101 ) ) ;
#41319 = CARTESIAN_POINT ( 'NONE',  ( -0.6603457068528999496, -80.88092951705199596, -1.153171400786999978 ) ) ;
#41320 = B_SPLINE_CURVE_WITH_KNOTS ( 'NONE', 3,
 ( #27177, #46103, #36633, #31898, #10359, #50521, #37212, #54651, #945, #14190, #32478, #32187, #4764, #50229, #1229, #28343, #46394, #32769, #49646, #9776, #22765, #36047, #18927, #10074, #50816, #19219, #5919, #40775, #27765, #13609, #23925, #45808, #78, #5342, #368, #18055, #18349, #49941, #27473, #24515, #16239, #28640, #6798, #37797, #47561, #51399, #46979, #34218, #20380, #11241, #42530, #2099, #28934, #20098, #29218, #29785, #29508, #46691, #7089, #11529, #24806, #52253, #24225, #42818, #42242, #15655, #43110, #2670, #25088, #20665, #38373, #19803, #51973, #10953, #38662, #38087, #19505, #6210, #1808, #55520, #41944, #56682, #15946, #1515, #2384, #56110, #33651, #55818, #33935, #11811, #37499, #15372, #6506 ),
 .UNSPECIFIED., .F., .F.,
 ( 4, 2, 2, 2, 1, 1, 1, 2, 2, 2, 2, 2, 1, 1, 1, 2, 2, 2, 2, 2, 1, 1, 1, 2, 2, 2, 2, 2, 1, 1, 1, 2, 2, 2, 2, 2, 1, 1, 2, 2, 2, 2, 2, 1, 1, 2, 2, 2, 2, 1, 1, 1, 2, 2, 2, 4 ),
 ( 0.000000000000000000, 0.06249999999995189959, 0.09374999999992783550, 0.1093749999999160671, 0.1171874999999104328, 0.1210937499999074074, 0.1230468749999059086, 0.1240234374999054229, 0.1249999999999049372, 0.1874999999999221179, 0.2187499999999307221, 0.2343749999999348022, 0.2421874999999368283, 0.2460937499999380496, 0.2480468749999386879, 0.2490234374999390210, 0.2499999999999393818, 0.3124999999999485412, 0.3437499999999534261, 0.3593749999999558686, 0.3671874999999573119, 0.3710937499999578115, 0.3730468749999580336, 0.3740234374999581446, 0.3749999999999582001, 0.4375000000000022204, 0.4687500000000242584, 0.4843750000000353051, 0.4921875000000405787, 0.4960937500000432432, 0.4980468750000443534, 0.4990234375000447420, 0.5000000000000450751, 0.5625000000000640599, 0.5937500000000734968, 0.6093750000000782707, 0.6171875000000806022, 0.6210937500000814904, 0.6230468750000819345, 0.6250000000000823785, 0.6875000000000668354, 0.7187500000000590639, 0.7343750000000549560, 0.7421875000000529576, 0.7460937500000521805, 0.7480468750000518474, 0.7500000000000514033, 0.8125000000000446310, 0.8437500000000413003, 0.8593750000000397460, 0.8671875000000386358, 0.8710937500000378586, 0.8730468750000374145, 0.8750000000000368594, 0.9375000000000184297, 1.000000000000000000 ),
 .UNSPECIFIED. ) ;
#41321 = CARTESIAN_POINT ( 'NONE',  ( 1.062462549644097143, -1.998698511921152665, -3.356897962585378092 ) ) ;
#41322 = CARTESIAN_POINT ( 'NONE',  ( 12.71798280854999952, -18.70221404512000163, 1.931086388455000025 ) ) ;
#41323 = CARTESIAN_POINT ( 'NONE',  ( 3.086017585447000222, -79.16257562062001796, -11.86910201801999953 ) ) ;
#41324 = DIRECTION ( 'NONE',  ( 0.000000000000000000, -1.000000000000000000, 0.000000000000000000 ) ) ;
#41325 = CARTESIAN_POINT ( 'NONE',  ( -10.18499221075000172, -58.54977139891999371, -7.710118476601000026 ) ) ;
#41326 = CARTESIAN_POINT ( 'NONE',  ( 3.229284361504000334, -79.90857183731299074, 10.68004289648999894 ) ) ;
#41327 = CARTESIAN_POINT ( 'NONE',  ( 3.018310159408800875, -2.820852371859394747, -1.203481977088054489 ) ) ;
#41328 = DIRECTION ( 'NONE',  ( -0.7071067811865475727, 0.000000000000000000, 0.7071067811865475727 ) ) ;
#41329 = CARTESIAN_POINT ( 'NONE',  ( -10.10912542009497983, -18.52413588830296476, 7.634643956514072904 ) ) ;
#41330 = B_SPLINE_SURFACE_WITH_KNOTS ( 'NONE', 3, 3, ( 
 ( #8162, #17304, #48331, #7870, #26163, #29428, #7006, #52179, #25583, #2590, #2871, #43605, #20869, #22615, #44461, #22312, #4012, #4908, #30867, #17901, #9626, #54506, #13745, #31149, #31450, #22907, #222, #35290, #40919, #53320, #22018, #508, #35889, #49189, #45654 ),
 ( #18484, #40026, #36477, #14043, #18200, #53616, #40626, #41203, #4616, #36192, #45064, #13454, #45358, #32037, #5196, #27614, #54210, #12865, #58338, #31745, #13154, #48903, #49790, #50081, #9336, #58039, #23198, #27325, #8443, #793, #53921, #9041, #8741, #26438, #17599 ),
 ( #35588, #26732, #44763, #4312, #40329, #49492, #27027, #29075, #24068, #1951, #47120, #14328, #51538, #5477, #37057, #28485, #50951, #10501, #19068, #42085, #55366, #14910, #51248, #9918, #5766, #27899, #45946, #32907, #37933, #50371, #6647, #46536, #32613, #37350, #55074 ),
 ( #23483, #19944, #10799, #6353, #6058, #1654, #19644, #37645, #15208, #55660, #41496, #33200, #33502, #32324, #1080, #28780, #18775, #46826, #23774, #24369, #14621, #55957, #50664, #41789, #42381, #15508, #10207, #11095, #24658, #42668, #36767, #54784, #28186, #46240, #1361 ) ),
 .UNSPECIFIED., .F., .F., .F.,
 ( 4, 4 ),
 ( 4, 1, 1, 1, 1, 1, 1, 1, 1, 1, 1, 1, 1, 1, 1, 1, 1, 1, 1, 1, 1, 1, 1, 1, 1, 1, 1, 1, 1, 1, 1, 1, 4 ),
 ( -0.05371687727927999811, 1.053716877278999986 ),
 ( -0.01895676948048000132, 0.01184798092530000083, 0.04265273133108000297, 0.07345748173685999471, 0.1042622321426000115, 0.1350669825483999942, 0.1658717329542000185, 0.1966764833600000151, 0.2274812337658000116, 0.2582859841715000049, 0.2890907345773000015, 0.3198954849830999980, 0.3507002353889000501, 0.3815049857946999912, 0.4123097362003999566, 0.4431144866061999532, 0.4739192370120000053, 0.5047239874178000019, 0.5355287378235999984, 0.5663334882294001060, 0.5971382386350999605, 0.6279429890408999571, 0.6587477394467000646, 0.6895524898524999502, 0.7203572402583000578, 0.7511619906639999122, 0.7819667410698000198, 0.8127714914756000164, 0.8435762418813999020, 0.8743809922872000095, 0.9051857426928999750, 0.9359904930987000826, 0.9667952435044999682 ),
 .UNSPECIFIED. ) ;
#41331 = VERTEX_POINT ( 'NONE', #16734 ) ;
#41332 = CARTESIAN_POINT ( 'NONE',  ( 1.204186364734999959, -82.23249872513999037, -0.6131120777826000179 ) ) ;
#41333 = CARTESIAN_POINT ( 'NONE',  ( 0.6528909987539758264, -78.76693641361094933, -1.116013679407363401 ) ) ;
#41334 = CARTESIAN_POINT ( 'NONE',  ( 0.7681833999686413783, -79.32291666666668561, 0.9995835529977274980 ) ) ;
#41335 = CARTESIAN_POINT ( 'NONE',  ( 0.1636246173744642929, -78.86458333333332860, 1.250000000000000888 ) ) ;
#41336 = CARTESIAN_POINT ( 'NONE',  ( 7.722022491113547993, -76.99999999999998579, 5.250591757671347004 ) ) ;
#41337 = CARTESIAN_POINT ( 'NONE',  ( 0.6304340365998000184, -82.61450768115200560, 1.542015542100000136 ) ) ;
#41338 = CARTESIAN_POINT ( 'NONE',  ( 1.714448272638999793, -77.21325110754499121, -11.65560625356000024 ) ) ;
#41339 = CARTESIAN_POINT ( 'NONE',  ( -1.186507705731999929, -78.88609509508398787, -9.667052097962999468 ) ) ;
#41341 = EDGE_CURVE ( 'NONE', #1253, #30942, #26714, .T. ) ;
#41340 = CIRCLE ( 'NONE', #51722, 2.000000000000001776 ) ;
#41342 = CARTESIAN_POINT ( 'NONE',  ( 9.089779753456481259, -76.00420051561397372, 7.445294846272284772 ) ) ;
#41343 = CARTESIAN_POINT ( 'NONE',  ( -8.150086036219999386, -78.90001270277200263, 7.434906319739000402 ) ) ;
#41344 = CARTESIAN_POINT ( 'NONE',  ( -3.131568623105725369, -86.10000000000019327, 1.324114027861367449 ) ) ;
#41345 = ORIENTED_EDGE ( 'NONE', *, *, #38472, .T. ) ;
#41346 = DIRECTION ( 'NONE',  ( -1.000000000000000000, 0.000000000000000000, 0.000000000000000000 ) ) ;
#41347 = EDGE_CURVE ( 'NONE', #3955, #8688, #51890, .T. ) ;
#41348 = CARTESIAN_POINT ( 'NONE',  ( 3.548349909810999847, -78.43735717367049176, -2.094141712711119485 ) ) ;
#41349 = CARTESIAN_POINT ( 'NONE',  ( -13.86363636363000218, -46.43897132165000130, -1.277887489420000009E-05 ) ) ;
#41350 = CARTESIAN_POINT ( 'NONE',  ( -10.57157196544999955, -79.97318600897997953, 2.324769239444999691 ) ) ;
#41351 = CARTESIAN_POINT ( 'NONE',  ( -5.539808784079904846, -79.18333333333332291, -9.611650271896831299 ) ) ;
#41352 = CARTESIAN_POINT ( 'NONE',  ( -10.48543666025111776, -77.85833333333330586, 6.043427764450754580 ) ) ;
#41353 = DIRECTION ( 'NONE',  ( 0.000000000000000000, 1.000000000000000000, 0.000000000000000000 ) ) ;
#41354 = CARTESIAN_POINT ( 'NONE',  ( 10.15323015673999940, -17.76919784905000199, -7.760928569209999850 ) ) ;
#41355 = LINE ( 'NONE', #9769, #42836 ) ;
#41356 = ORIENTED_EDGE ( 'NONE', *, *, #24622, .T. ) ;
#41357 = CARTESIAN_POINT ( 'NONE',  ( -7.255688098778000139, -79.14026687680399164, 8.462245020330000145 ) ) ;
#41358 = DIRECTION ( 'NONE',  ( -1.000000000000000000, 0.000000000000000000, 0.000000000000000000 ) ) ;
#41359 = CARTESIAN_POINT ( 'NONE',  ( 2.813789756862229652, -79.85416666666667140, 10.47020627418440064 ) ) ;
#41360 = CARTESIAN_POINT ( 'NONE',  ( -3.699342699771063447, -78.39678895079168797, -0.06973942363209935380 ) ) ;
#41361 = CARTESIAN_POINT ( 'NONE',  ( -5.471496541426451365, -76.86542272010237298, 10.76143312585065459 ) ) ;
#41362 = EDGE_CURVE ( 'NONE', #4024, #38980, #7005, .T. ) ;
#41363 = CARTESIAN_POINT ( 'NONE',  ( -0.5999999999999999778, -5.000000000000000000, -0.5999999999999999778 ) ) ;
#41364 = B_SPLINE_CURVE_WITH_KNOTS ( 'NONE', 3,
 ( #38149, #56171, #20446, #51752, #11302, #47627, #25152, #2733, #11878, #29856, #47911, #41313, #46936, #14724, #55776, #19174, #23590, #51651, #10911, #32722, #10614, #51352, #18879, #5873, #56069, #42488, #1764, #37171, #19462, #28887, #46642, #23306, #6461, #898, #50476, #24474, #23882, #55182, #33608, #15324, #2058, #28009, #20059, #38045, #6170, #41604, #28595, #29178, #51065, #24180, #33017, #1473, #33317, #15613, #11202, #47225, #42195, #36875, #46349, #19758, #1184, #54886, #14436, #32431, #41898, #55477, #50773, #37458, #37755, #15024, #10027, #46056, #5579, #10318, #28296, #21483, #21192, #47519, #20335, #30618, #16487, #7618, #17055, #12053, #48366, #35036, #2341, #39490, #11490, #53071, #57491, #12621, #56927, #7048, #30034, #43348 ),
 .UNSPECIFIED., .F., .F.,
 ( 4, 2, 2, 2, 2, 2, 1, 2, 2, 2, 2, 2, 2, 2, 2, 2, 2, 2, 2, 2, 2, 2, 2, 2, 2, 2, 2, 2, 2, 2, 2, 2, 2, 2, 2, 2, 2, 2, 2, 2, 2, 2, 1, 2, 2, 2, 2, 2, 4 ),
 ( 0.000000000000000000, 0.01562499999999996531, 0.03124999999999993061, 0.04687499999999990979, 0.06249999999999988898, 0.07812499999999986122, 0.09374999999999984734, 0.1093749999999998196, 0.1249999999999998335, 0.1406249999999998335, 0.1562499999999998057, 0.1718749999999998057, 0.1874999999999998057, 0.2031249999999998057, 0.2187499999999997780, 0.2343749999999997780, 0.2499999999999997780, 0.2812499999999998335, 0.3124999999999998335, 0.3437499999999998890, 0.3749999999999999445, 0.4062500000000000000, 0.4375000000000000000, 0.4687500000000000555, 0.5000000000000001110, 0.5312500000000001110, 0.5625000000000002220, 0.5937500000000002220, 0.6250000000000002220, 0.6562500000000003331, 0.6875000000000003331, 0.7187500000000004441, 0.7500000000000004441, 0.7656250000000005551, 0.7812500000000004441, 0.7968750000000004441, 0.8125000000000004441, 0.8281250000000003331, 0.8437500000000003331, 0.8593750000000003331, 0.8750000000000002220, 0.8906250000000002220, 0.9062500000000002220, 0.9218750000000002220, 0.9375000000000001110, 0.9531250000000001110, 0.9687500000000001110, 0.9843750000000000000, 1.000000000000000000 ),
 .UNSPECIFIED. ) ;
#41365 = CARTESIAN_POINT ( 'NONE',  ( -12.50659830543690099, -53.82653383338065112, -0.3508384617699890073 ) ) ;
#41366 = CARTESIAN_POINT ( 'NONE',  ( -7.958763980599000476, -17.52301961032999955, -9.723170659105999647 ) ) ;
#41367 = DIRECTION ( 'NONE',  ( -0.9999999999998321343, 0.000000000000000000, -5.794540613806191565E-07 ) ) ;
#41368 = DIRECTION ( 'NONE',  ( 0.000000000000000000, 0.7071067811866525998, -0.7071067811864425456 ) ) ;
#41369 = CARTESIAN_POINT ( 'NONE',  ( 6.084059575412256393, -78.62185687685334301, -9.135208697462157801 ) ) ;
#41370 = EDGE_CURVE ( 'NONE', #34387, #50040, #23865, .T. ) ;
#41371 = CARTESIAN_POINT ( 'NONE',  ( -8.536051545334721879, -79.70833333333069959, -3.797199644221384229 ) ) ;
#41372 = VERTEX_POINT ( 'NONE', #30290 ) ;
#41373 = ORIENTED_EDGE ( 'NONE', *, *, #34354, .F. ) ;
#41374 = CARTESIAN_POINT ( 'NONE',  ( -9.927618387633998509, -77.89028998579800600, -1.374747298418999897 ) ) ;
#41375 = CARTESIAN_POINT ( 'NONE',  ( 7.561064631405968406, -78.78706913947456769, -7.641704783336303208 ) ) ;
#41376 = EDGE_LOOP ( 'NONE', ( #7642, #41387, #47843, #26109, #46229, #29564 ) ) ;
#41377 = CARTESIAN_POINT ( 'NONE',  ( 9.552813797205702784, -80.26770833350961709, -5.504922207147467716 ) ) ;
#41378 = CARTESIAN_POINT ( 'NONE',  ( 3.227959076126192262, -83.86458334601041997, -1.201676990424012326 ) ) ;
#41379 = AXIS2_PLACEMENT_3D ( 'NONE', #26205, #16494, #47526 ) ;
#41380 = CARTESIAN_POINT ( 'NONE',  ( 10.18114973714999927, -60.19009320380000361, 7.633087466122999487 ) ) ;
#41381 = DIRECTION ( 'NONE',  ( 0.5721800012456795814, 0.8201280669349721997, 0.000000000000000000 ) ) ;
#41382 = CARTESIAN_POINT ( 'NONE',  ( 11.70610040787851780, -78.31695220253838841, 2.546999134027124967 ) ) ;
#41383 = CARTESIAN_POINT ( 'NONE',  ( -1.472820794058999905, -78.38041877790499257, -10.90095403661999995 ) ) ;
#41384 = CARTESIAN_POINT ( 'NONE',  ( 2.883152686262326458, -1.811972400245676962, -1.558099060999823537 ) ) ;
#41385 = ORIENTED_EDGE ( 'NONE', *, *, #44501, .T. ) ;
#41386 = CARTESIAN_POINT ( 'NONE',  ( 10.75000000000000000, -77.75000000000000000, 0.000000000000000000 ) ) ;
#41387 = ORIENTED_EDGE ( 'NONE', *, *, #37975, .F. ) ;
#41388 = CARTESIAN_POINT ( 'NONE',  ( 9.132654035730695341, -77.36284952363988054, 1.468098543608952422 ) ) ;
#41389 = CARTESIAN_POINT ( 'NONE',  ( -5.876696946710000091, -77.51048305282198214, -9.346046374399000101 ) ) ;
#41390 = CARTESIAN_POINT ( 'NONE',  ( 10.10565965566643065, -76.04999999999999716, 4.494725398156579566 ) ) ;
#41391 = CARTESIAN_POINT ( 'NONE',  ( 1.412851607863000014, -78.70172720777699737, -0.7817060856327000540 ) ) ;
#41392 = CARTESIAN_POINT ( 'NONE',  ( -3.140974612311352221, -77.50416666666666288, -11.68767212001979061 ) ) ;
#41393 = CIRCLE ( 'NONE', #52691, 12.57042253521000141 ) ;
#41394 = DIRECTION ( 'NONE',  ( 0.000000000000000000, -1.000000000000000000, 0.000000000000000000 ) ) ;
#41395 = CARTESIAN_POINT ( 'NONE',  ( -1.566959183383000109, -78.24862352424000278, 0.4396611996733000294 ) ) ;
#41396 = DIRECTION ( 'NONE',  ( 0.000000000000000000, 1.000000000000000000, 0.000000000000000000 ) ) ;
#41397 = CARTESIAN_POINT ( 'NONE',  ( 10.84079038992999955, -79.66845093841598668, -1.471421101766999806 ) ) ;
#41398 = CARTESIAN_POINT ( 'NONE',  ( 2.062597299672999540, -59.58485473249000108, -12.87022657274000004 ) ) ;
#41399 = B_SPLINE_CURVE_WITH_KNOTS ( 'NONE', 3,
 ( #11679, #2815, #29654, #47706 ),
 .UNSPECIFIED., .F., .F.,
 ( 4, 4 ),
 ( 0.000000000000000000, 1.000000000000000000 ),
 .UNSPECIFIED. ) ;
#41400 = CARTESIAN_POINT ( 'NONE',  ( 12.71798269383000068, -55.50221245779999890, -1.931086388578000079 ) ) ;
#41401 = CARTESIAN_POINT ( 'NONE',  ( -1.490802228383000028, -82.73892731861099037, 3.265157211617999877 ) ) ;
#41402 = VERTEX_POINT ( 'NONE', #24725 ) ;
#41403 = DIRECTION ( 'NONE',  ( -0.7071067811865475727, 0.000000000000000000, 0.7071067811865475727 ) ) ;
#41404 = CARTESIAN_POINT ( 'NONE',  ( -10.63167128756999880, -76.62632357022098972, 2.002204529075000128 ) ) ;
#41405 = CARTESIAN_POINT ( 'NONE',  ( 10.53071379481334979, -77.86619273895507831, 2.161785647016301493 ) ) ;
#41406 = CARTESIAN_POINT ( 'NONE',  ( -10.86788298907000083, -77.66845141377899608, -5.040355520269000245 ) ) ;
#41407 = CARTESIAN_POINT ( 'NONE',  ( -10.31444587878999997, -17.69924218095000157, 7.758886158107999975 ) ) ;
#41409 = DIRECTION ( 'NONE',  ( 0.7071067811865475727, 0.000000000000000000, 0.7071067811865475727 ) ) ;
#41408 = DIRECTION ( 'NONE',  ( -1.000000000000000000, 0.000000000000000000, 0.000000000000000000 ) ) ;
#41410 = CARTESIAN_POINT ( 'NONE',  ( 2.537261334626276010, -2.939104093472465706, -2.439294570458690803 ) ) ;
#41411 = FACE_OUTER_BOUND ( 'NONE', #6376, .T. ) ;
#41412 = CARTESIAN_POINT ( 'NONE',  ( 3.106054555984663956, -86.10000000000019327, -1.382904586457956553 ) ) ;
#41413 = CARTESIAN_POINT ( 'NONE',  ( -7.664623337597000763, -77.45580276511299189, -8.093710500358000104 ) ) ;
#41414 = CARTESIAN_POINT ( 'NONE',  ( 3.912590402935000267, -82.39999999999999147, -0.8316467632710000668 ) ) ;
#41415 = CARTESIAN_POINT ( 'NONE',  ( 9.718307120666999310, -80.68179051666800206, 5.447174627686000470 ) ) ;
#41416 = ORIENTED_EDGE ( 'NONE', *, *, #27992, .T. ) ;
#41417 = CARTESIAN_POINT ( 'NONE',  ( 2.858407197969000002, -77.00000000000000000, 8.797272775729998884 ) ) ;
#41418 = CARTESIAN_POINT ( 'NONE',  ( 2.712110641633999730, -3.620707716005000076, 2.894388207016999726 ) ) ;
#41419 = PRODUCT_DEFINITION_FORMATION_WITH_SPECIFIED_SOURCE ( 'ANY', '', #41849, .NOT_KNOWN. ) ;
#41420 = CARTESIAN_POINT ( 'NONE',  ( 10.75916580684000046, -77.97112838545299951, 3.171507801093999657 ) ) ;
#41421 = CARTESIAN_POINT ( 'NONE',  ( -5.755176823513999729, -78.28877243311998768, 9.345691860246999383 ) ) ;
#41422 = CARTESIAN_POINT ( 'NONE',  ( 8.798028344861998917, -24.93813495683999903, -8.790623041439999952 ) ) ;
#41423 = DIRECTION ( 'NONE',  ( -0.07798810159653808693, 0.04890177473153878990, 0.9957542229071758566 ) ) ;
#41424 = CARTESIAN_POINT ( 'NONE',  ( -1.749722766158645193, -23.47588992886881343, -12.54673760678556782 ) ) ;
#41425 = CARTESIAN_POINT ( 'NONE',  ( 0.000000000000000000, -74.99999999999998579, -4.299999999999978506 ) ) ;
#41426 = CARTESIAN_POINT ( 'NONE',  ( -3.349446900146999972, -83.02867953870898532, 2.487518992154000408 ) ) ;
#41427 = VECTOR ( 'NONE', #30549, 999.9999999999998863 ) ;
#41428 = CARTESIAN_POINT ( 'NONE',  ( -10.48771805367000098, -20.24439828562999821, -7.686918321060999482 ) ) ;
#41429 = EDGE_CURVE ( 'NONE', #28511, #24529, #38584, .T. ) ;
#41430 = CARTESIAN_POINT ( 'NONE',  ( 10.01676221090000141, -55.59058563439999290, -7.658899961832999814 ) ) ;
#41431 = CARTESIAN_POINT ( 'NONE',  ( 2.618044012240999585, -78.32284911944198313, -10.95786383906999895 ) ) ;
#41432 = CARTESIAN_POINT ( 'NONE',  ( -0.4240539849974000464, -80.10665717147000464, 1.611036072322000079 ) ) ;
#41433 = CARTESIAN_POINT ( 'NONE',  ( -0.1527015615469000109, -77.84095328623999421, 1.349110360386999830 ) ) ;
#41434 = CARTESIAN_POINT ( 'NONE',  ( -10.48543666025109111, -79.34166666666665435, -6.043427764450793660 ) ) ;
#41435 = CARTESIAN_POINT ( 'NONE',  ( 0.3510616317362846295, -81.89369634218427052, -1.470620435669331760 ) ) ;
#41436 = B_SPLINE_CURVE_WITH_KNOTS ( 'NONE', 3,
 ( #46358, #5882, #5309, #41325, #23890, #2350 ),
 .UNSPECIFIED., .F., .F.,
 ( 4, 1, 1, 4 ),
 ( 0.000000000000000000, 0.3333333333333000081, 0.6666666666667000474, 1.000000000000000000 ),
 .UNSPECIFIED. ) ;
#41437 = DIRECTION ( 'NONE',  ( 0.000000000000000000, -1.000000000000000000, -1.767388436867000098E-14 ) ) ;
#41438 = CARTESIAN_POINT ( 'NONE',  ( 0.000000000000000000, -86.29999999996098836, 0.000000000000000000 ) ) ;
#41439 = CARTESIAN_POINT ( 'NONE',  ( -4.784380313523538319, -77.88333333333332575, -8.300970689365453126 ) ) ;
#41440 = VECTOR ( 'NONE', #45617, 1000.000000000000000 ) ;
#41441 = EDGE_LOOP ( 'NONE', ( #28277, #48503, #47642, #49743, #55249, #6866 ) ) ;
#41442 = CARTESIAN_POINT ( 'NONE',  ( -1.624989163556999772E-14, -74.80000000000001137, -11.19999999999998863 ) ) ;
#41443 = EDGE_CURVE ( 'NONE', #50397, #4032, #47223, .T. ) ;
#41444 = CARTESIAN_POINT ( 'NONE',  ( -10.69024338110999928, -78.91399466736399404, -3.158052726529999799 ) ) ;
#41445 = LINE ( 'NONE', #1029, #1670 ) ;
#41446 = ORIENTED_EDGE ( 'NONE', *, *, #29345, .F. ) ;
#41447 = VERTEX_POINT ( 'NONE', #40625 ) ;
#41448 = CARTESIAN_POINT ( 'NONE',  ( 0.9527810478389000526, -81.41904148856198731, 1.049889353731999986 ) ) ;
#41449 = ORIENTED_EDGE ( 'NONE', *, *, #20861, .F. ) ;
#41450 = ORIENTED_EDGE ( 'NONE', *, *, #33377, .F. ) ;
#41451 = DIRECTION ( 'NONE',  ( 0.7071067811865475727, 0.000000000000000000, -0.7071067811865475727 ) ) ;
#41452 = CYLINDRICAL_SURFACE ( 'NONE', #7552, 11.00000000000000000 ) ;
#41453 = CARTESIAN_POINT ( 'NONE',  ( -2.345309999012545443, -80.39583332391796944, -2.522288602443209182 ) ) ;
#41454 = FACE_OUTER_BOUND ( 'NONE', #5549, .T. ) ;
#41455 = CARTESIAN_POINT ( 'NONE',  ( 7.275474750695519077, -78.29713309960814627, -5.714788711246518105 ) ) ;
#41456 = CARTESIAN_POINT ( 'NONE',  ( -10.47020627418439354, -78.02083333333335702, -2.813789756862263847 ) ) ;
#41457 = ORIENTED_EDGE ( 'NONE', *, *, #45118, .F. ) ;
#41458 = VERTEX_POINT ( 'NONE', #13153 ) ;
#41459 = CARTESIAN_POINT ( 'NONE',  ( -12.50686284816388749, -17.69510763146807264, -1.423064270789318631 ) ) ;
#41460 = CARTESIAN_POINT ( 'NONE',  ( -1.250000000000000000, -78.60000000000000853, 0.000000000000000000 ) ) ;
#41461 = EDGE_CURVE ( 'NONE', #22736, #33739, #221, .T. ) ;
#41462 = CARTESIAN_POINT ( 'NONE',  ( -0.5135400118900182997, -61.97868533827725912, -12.70453250103373044 ) ) ;
#41463 = CARTESIAN_POINT ( 'NONE',  ( -5.351292223237999579, -77.69132919765699796, 8.095330809056001442 ) ) ;
#41464 = CARTESIAN_POINT ( 'NONE',  ( 2.299999999999999822, -76.00000000000000000, 0.000000000000000000 ) ) ;
#41465 = CARTESIAN_POINT ( 'NONE',  ( 2.338897668117772888, -85.88596255424737080, 3.133429492702677344 ) ) ;
#41466 = CARTESIAN_POINT ( 'NONE',  ( 7.379132703266000348, -77.09176059790999602, -10.64946278274999969 ) ) ;
#41467 = CARTESIAN_POINT ( 'NONE',  ( 1.446151133417000079, -79.40723116178999419, 0.2550274018384999786 ) ) ;
#41468 = FACE_OUTER_BOUND ( 'NONE', #58149, .T. ) ;
#41469 = B_SPLINE_CURVE_WITH_KNOTS ( 'NONE', 3,
 ( #18214, #35903, #54223, #36491, #40038, #31759 ),
 .UNSPECIFIED., .F., .F.,
 ( 4, 2, 4 ),
 ( 0.000000000000000000, 0.5000000000000001110, 1.000000000000000000 ),
 .UNSPECIFIED. ) ;
#41470 = CARTESIAN_POINT ( 'NONE',  ( -3.200164631505999946, -78.92298487743470048, -2.681188903621000374 ) ) ;
#41472 = AXIS2_PLACEMENT_3D ( 'NONE', #6651, #42089, #33506 ) ;
#41471 = CARTESIAN_POINT ( 'NONE',  ( 3.862060628231000159, -80.61325977223638972, 10.58270681924999934 ) ) ;
#41473 = CARTESIAN_POINT ( 'NONE',  ( -10.48543666025111420, -76.75833333333331154, 6.043427764450754580 ) ) ;
#41474 = CARTESIAN_POINT ( 'NONE',  ( 3.000494659939939801, -2.882409298795182373, 1.247127308777857824 ) ) ;
#41475 = CARTESIAN_POINT ( 'NONE',  ( 1.666530149241000069, -79.72707046129099240, 3.131649709249999969 ) ) ;
#41476 = CONICAL_SURFACE ( 'NONE', #28269, 10.59999999995999964, 0.7853981633972997312 ) ;
#41477 = CARTESIAN_POINT ( 'NONE',  ( 0.8912423865758999364, -78.03864452729919776, 0.9921004264782997684 ) ) ;
#41478 = DIRECTION ( 'NONE',  ( 1.000000000000000000, 0.000000000000000000, 0.000000000000000000 ) ) ;
#41479 = DIRECTION ( 'NONE',  ( 1.000000000000000000, 0.000000000000000000, 0.000000000000000000 ) ) ;
#41480 = CARTESIAN_POINT ( 'NONE',  ( 2.639686428813980079, -77.20000000000000284, -10.63845845605472107 ) ) ;
#41481 = ORIENTED_EDGE ( 'NONE', *, *, #46522, .T. ) ;
#41482 = CARTESIAN_POINT ( 'NONE',  ( -2.799999999999999822, -76.00000000000000000, 0.000000000000000000 ) ) ;
#41483 = CARTESIAN_POINT ( 'NONE',  ( 7.997114030225745296, -60.48581381149598002, -7.553727747507254620 ) ) ;
#41484 = DIRECTION ( 'NONE',  ( 0.000000000000000000, -1.000000000000000000, 0.000000000000000000 ) ) ;
#41485 = CARTESIAN_POINT ( 'NONE',  ( -9.270924421324000519, -79.35427108146299702, -3.023218246060999981 ) ) ;
#41486 = CARTESIAN_POINT ( 'NONE',  ( 5.579996517577999526, -77.28773409592999144, 11.75597208960999929 ) ) ;
#41487 = CARTESIAN_POINT ( 'NONE',  ( 7.085755085285039279, -79.41772239509739961, 8.085164613341476070 ) ) ;
#41488 = CARTESIAN_POINT ( 'NONE',  ( -2.362630825376999866, -79.54861332859900358, -9.447900677770000755 ) ) ;
#41489 = CARTESIAN_POINT ( 'NONE',  ( 9.685201957684167695, -78.49578785308447948, 6.650675367548727124 ) ) ;
#41490 = ADVANCED_FACE ( 'NONE', ( #507 ), #31743, .F. ) ;
#41491 = DIRECTION ( 'NONE',  ( -1.000000000000000000, 0.000000000000000000, 0.000000000000000000 ) ) ;
#41492 = CARTESIAN_POINT ( 'NONE',  ( -9.929563311754000310, -77.63992477412999449, 5.339448599216000346 ) ) ;
#41493 = CIRCLE ( 'NONE', #19804, 4.999999999999996447 ) ;
#41494 = EDGE_CURVE ( 'NONE', #28795, #15888, #31449, .T. ) ;
#41495 = CARTESIAN_POINT ( 'NONE',  ( -4.165135875058396664, -76.29562521202450398, -10.99247644781376287 ) ) ;
#41496 = CARTESIAN_POINT ( 'NONE',  ( -1.265869145960000219, -81.35542651680599135, 0.9852510953920999848 ) ) ;
#41497 = CARTESIAN_POINT ( 'NONE',  ( 7.654537165468999760, -23.28056535155999995, -10.01332852689000141 ) ) ;
#41498 = CARTESIAN_POINT ( 'NONE',  ( -7.831519877845000366, -78.56761851250499262, -5.222881475815000840 ) ) ;
#41500 = CARTESIAN_POINT ( 'NONE',  ( -1.180494763713999973, -0.7538550533857000246, 3.461421590595000097 ) ) ;
#41499 = CARTESIAN_POINT ( 'NONE',  ( 3.490791149790999803, -85.02754468068998506, -1.876264172078000225 ) ) ;
#41501 = CARTESIAN_POINT ( 'NONE',  ( -9.554796630153999715, -79.63025194988500743, -0.02401403847836000235 ) ) ;
#41502 = CARTESIAN_POINT ( 'NONE',  ( 0.000000000000000000, -0.1000000007601000024, 0.000000000000000000 ) ) ;
#41503 = CARTESIAN_POINT ( 'NONE',  ( 1.299878529918000014, -80.39438452883999275, -0.2255693107841999778 ) ) ;
#41504 = CARTESIAN_POINT ( 'NONE',  ( -8.593369277392113759, -77.15225396531909041, -6.609291488178449470 ) ) ;
#41505 = CYLINDRICAL_SURFACE ( 'NONE', #9669, 0.5999999999999999778 ) ;
#41506 = CARTESIAN_POINT ( 'NONE',  ( -3.999999999999848566, -78.72610001270986402, 7.999999999999648281 ) ) ;
#41507 = VERTEX_POINT ( 'NONE', #44180 ) ;
#41508 = EDGE_LOOP ( 'NONE', ( #14339, #11538, #2766, #1170 ) ) ;
#41509 = CARTESIAN_POINT ( 'NONE',  ( 7.652056849482000267, -79.45402974060098700, 9.281873293285000770 ) ) ;
#41510 = FACE_OUTER_BOUND ( 'NONE', #24820, .T. ) ;
#41511 = EDGE_CURVE ( 'NONE', #18212, #28960, #53574, .T. ) ;
#41512 = CARTESIAN_POINT ( 'NONE',  ( -1.033815393572557806, -80.38261156915623928, 10.74597751898181741 ) ) ;
#41513 = ORIENTED_EDGE ( 'NONE', *, *, #52861, .F. ) ;
#41514 = CARTESIAN_POINT ( 'NONE',  ( -10.82689242272999941, -77.65796654052100223, -5.021344731552000340 ) ) ;
#41515 = VERTEX_POINT ( 'NONE', #27025 ) ;
#41516 = VERTEX_POINT ( 'NONE', #54209 ) ;
#41517 = CONICAL_SURFACE ( 'NONE', #56610, 12.74999999937999995, 0.7853981633972997312 ) ;
#41518 = VECTOR ( 'NONE', #38580, 1000.000000000000000 ) ;
#41519 = ORIENTED_EDGE ( 'NONE', *, *, #12890, .F. ) ;
#41520 = CARTESIAN_POINT ( 'NONE',  ( -3.405565740252999518, -81.61342682855999442, 0.9933187896184001442 ) ) ;
#41521 = DIRECTION ( 'NONE',  ( -1.000000000000000000, 0.000000000000000000, 0.000000000000000000 ) ) ;
#41522 = ORIENTED_EDGE ( 'NONE', *, *, #3805, .F. ) ;
#41523 = CARTESIAN_POINT ( 'NONE',  ( 1.249623181998916532, -82.84938247290897095, -0.01959429098678184752 ) ) ;
#41524 = ORIENTED_EDGE ( 'NONE', *, *, #45970, .T. ) ;
#41525 = CARTESIAN_POINT ( 'NONE',  ( 1.211040244683831313, -79.23558525598221536, -9.190809572653749981 ) ) ;
#41526 = CARTESIAN_POINT ( 'NONE',  ( -2.183148623211547346, -77.74296245559024499, 9.455563964093084195 ) ) ;
#41527 = CARTESIAN_POINT ( 'NONE',  ( 2.301294140410000022, -78.85171438276198330, -3.984678389768961271 ) ) ;
#41528 = CARTESIAN_POINT ( 'NONE',  ( 12.50000000000000000, -23.25000000000000000, 1.250000000000000000 ) ) ;
#41529 = LINE ( 'NONE', #39551, #43787 ) ;
#41530 = B_SPLINE_CURVE_WITH_KNOTS ( 'NONE', 3,
 ( #24443, #33281, #51321, #15287, #28850, #38007, #41377, #960, #36354, #40789 ),
 .UNSPECIFIED., .F., .F.,
 ( 4, 2, 2, 2, 4 ),
 ( 0.1666666723472590150, 0.3750000042604442752, 0.5833333361736294798, 0.7916666680868147399, 1.000000000000000000 ),
 .UNSPECIFIED. ) ;
#41531 = CARTESIAN_POINT ( 'NONE',  ( -9.831705185582000794, -76.22657204401799902, 5.330239850318999828 ) ) ;
#41532 = CARTESIAN_POINT ( 'NONE',  ( -7.958776492183998741, -24.47699850274999989, 9.723157982400998378 ) ) ;
#41533 = CARTESIAN_POINT ( 'NONE',  ( 2.084841536542000107, -76.18354795607999108, 11.03345659225000119 ) ) ;
#41534 = CARTESIAN_POINT ( 'NONE',  ( 7.033247818498722381, -78.79382002255685791, -6.010734345524098465 ) ) ;
#41535 = CARTESIAN_POINT ( 'NONE',  ( 7.472976412552629455, -76.51966548243302668, 9.068880097928863293 ) ) ;
#41536 = AXIS2_PLACEMENT_3D ( 'NONE', #24420, #42434, #33551 ) ;
#41537 = CARTESIAN_POINT ( 'NONE',  ( -12.76303204525000012, -60.06485147653999945, -1.980584515753000208 ) ) ;
#41538 = FACE_OUTER_BOUND ( 'NONE', #14280, .T. ) ;
#41539 = CARTESIAN_POINT ( 'NONE',  ( -8.367750842354992002, -80.15659319994234977, -7.184025905134648227 ) ) ;
#41540 = CARTESIAN_POINT ( 'NONE',  ( -6.771615370240408716, -78.03068079904456056, -9.996688553910448860 ) ) ;
#41541 = CARTESIAN_POINT ( 'NONE',  ( -3.812522663964000191, -78.36136788790179253, 0.5513559584095000243 ) ) ;
#41542 = EDGE_CURVE ( 'NONE', #50457, #32490, #35586, .T. ) ;
#41543 = CARTESIAN_POINT ( 'NONE',  ( -12.66761570929000058, -17.77632520104999969, 1.696752301450999978 ) ) ;
#41544 = CARTESIAN_POINT ( 'NONE',  ( 1.009560447666660865, -82.90050067395594624, 0.7369711323571810357 ) ) ;
#41545 = CARTESIAN_POINT ( 'NONE',  ( 0.000000000000000000, -76.39999999999899671, 0.000000000000000000 ) ) ;
#41546 = CARTESIAN_POINT ( 'NONE',  ( -12.69999999929000012, 7.141125103605999188E-10, -6.699862062809000450E-09 ) ) ;
#41547 = CARTESIAN_POINT ( 'NONE',  ( -11.68767212001980127, -79.37916666666666288, 3.140974612311317138 ) ) ;
#41548 = CARTESIAN_POINT ( 'NONE',  ( -10.35398566683000077, -60.20788276206999967, -7.619388279096000360 ) ) ;
#41549 = DIRECTION ( 'NONE',  ( 1.000000000000000000, 0.000000000000000000, 0.000000000000000000 ) ) ;
#41550 = CARTESIAN_POINT ( 'NONE',  ( 1.291106326275375693, -79.64481427576352246, 0.8295474976191916650 ) ) ;
#41551 = CIRCLE ( 'NONE', #36951, 1.750000000000000444 ) ;
#41552 = DIRECTION ( 'NONE',  ( 0.000000000000000000, -1.000000000000000000, 0.000000000000000000 ) ) ;
#41553 = CARTESIAN_POINT ( 'NONE',  ( 12.51072239526000196, -15.69705297114000331, 0.7871079366006996647 ) ) ;
#41554 = CARTESIAN_POINT ( 'NONE',  ( 12.68703394091000014, -23.75066116476999767, 1.889962945498999902 ) ) ;
#41555 = CARTESIAN_POINT ( 'NONE',  ( 0.1636246173744697330, -80.63541666666665719, -1.249999999999999778 ) ) ;
#41556 = CARTESIAN_POINT ( 'NONE',  ( 0.3960817336853000303, -77.00102680916499764, -12.03780325391999995 ) ) ;
#41557 = CARTESIAN_POINT ( 'NONE',  ( -1.980584515756000030, -55.53514849873000259, 12.76303204337999908 ) ) ;
#41559 = CARTESIAN_POINT ( 'NONE',  ( -1.575772165402021807, -24.46154542800653431, -12.70597445617581478 ) ) ;
#41558 = CARTESIAN_POINT ( 'NONE',  ( 1.199500263597271799, -80.19791666666667140, -0.9218200799623701425 ) ) ;
#41560 = CARTESIAN_POINT ( 'NONE',  ( 6.559616885195999281, -75.99841620946999399, 10.30072712123999956 ) ) ;
#41561 = EDGE_LOOP ( 'NONE', ( #37379, #41957, #44198, #33378 ) ) ;
#41562 = B_SPLINE_SURFACE_WITH_KNOTS ( 'NONE', 3, 3, ( 
 ( #27956, #23256, #46881, #7218, #40976, #54841, #37114, #55129, #567, #54561, #46299, #14102, #45715, #5251, #14674, #5824, #41266, #18834, #14384, #32384, #32671, #23831, #50724, #10265, #41847, #1425, #34353, #43238, #48823, #25508, #3934, #53535, #17516, #12508, #3086 ),
 ( #21936, #53242, #52391, #30790, #57666, #21081, #26363, #43823, #38795, #8081, #25796, #57387, #39087, #17223, #35212, #25218, #57093, #12791, #29922, #39661, #8364, #44382, #16662, #20792, #39947, #11945, #57962, #35507, #13076, #12224, #31073, #2795, #49112, #56815, #16372 ),
 ( #47972, #21365, #7509, #43525, #30214, #34643, #52959, #52671, #48260, #39381, #30507, #7795, #3370, #34927, #16946, #48535, #26078, #44102, #3652, #21654, #35806, #40835, #13667, #36110, #9254, #18695, #430, #13371, #23408, #31957, #40246, #9547, #36979, #8961, #54704 ),
 ( #49413, #44979, #44684, #41418, #26946, #41123, #49709, #5119, #45867, #54992, #717, #1002, #45277, #31663, #31368, #14541, #4534, #5400, #23116, #27238, #36689, #22534, #4236, #18987, #53836, #32534, #8661, #32244, #54126, #26647, #22234, #27820, #58259, #17819, #40544 ) ),
 .UNSPECIFIED., .F., .F., .F.,
 ( 4, 4 ),
 ( 4, 1, 1, 1, 1, 1, 1, 1, 1, 1, 1, 1, 1, 1, 1, 1, 1, 1, 1, 1, 1, 1, 1, 1, 1, 1, 1, 1, 1, 1, 1, 1, 4 ),
 ( -0.3708084972812999980, 1.370808497280999960 ),
 ( 0.03450073181895999680, 0.06526418889335999785, 0.09602764596774999994, 0.1267911030420999785, 0.1575545601164999865, 0.1883180171909000222, 0.2190814742653000025, 0.2498449313396999827, 0.2806083884140999629, 0.3113718454884999987, 0.3421353025628999789, 0.3728987596373000146, 0.4036622167116999949, 0.4344256737861000306, 0.4651891308605000108, 0.4959525879348999911, 0.5267160450093000268, 0.5574795020837000070, 0.5882429591580999872, 0.6190064162324999675, 0.6497698733068999477, 0.6805333303813000390, 0.7112967874557000192, 0.7420602445300999994, 0.7728237016044999796, 0.8035871586789000709, 0.8343506157532999401, 0.8651140728276000003, 0.8958775299019999805, 0.9266409869763999607, 0.9574044440508000520, 0.9881679011251999212, 1.018931358199999915 ),
 .UNSPECIFIED. ) ;
#41563 = CARTESIAN_POINT ( 'NONE',  ( 0.2829668327839999775, -83.11171544543098832, 3.745838405360000234 ) ) ;
#41564 = CARTESIAN_POINT ( 'NONE',  ( 2.381660037360000537, -80.91833076151569060, -11.15416238136999993 ) ) ;
#41565 = ADVANCED_FACE ( 'NONE', ( #31147 ), #18198, .F. ) ;
#41567 = CARTESIAN_POINT ( 'NONE',  ( -4.559477187396880460, -76.29284459774818572, -10.82903768629202013 ) ) ;
#41566 = CARTESIAN_POINT ( 'NONE',  ( 8.315784280752016144, -78.31395558942278967, -4.050953114190261495 ) ) ;
#41568 = CARTESIAN_POINT ( 'NONE',  ( -1.199500263597270022, -81.55208333333334281, -0.9218200799623730290 ) ) ;
#41569 = CARTESIAN_POINT ( 'NONE',  ( 10.75916580684000046, -78.17449404528099421, 3.171507801093999657 ) ) ;
#41570 = DIRECTION ( 'NONE',  ( 0.7071067811865475727, 0.000000000000000000, 0.7071067811865475727 ) ) ;
#41571 = CARTESIAN_POINT ( 'NONE',  ( -1.553298277364999924, -78.78095298048599204, 9.504760619105999453 ) ) ;
#41572 = CARTESIAN_POINT ( 'NONE',  ( -2.958306647813000012, -1.246290208250999898, 2.731603797012999824 ) ) ;
#41573 = DIRECTION ( 'NONE',  ( 0.000000000000000000, 0.000000000000000000, 1.000000000000000000 ) ) ;
#41574 = CARTESIAN_POINT ( 'NONE',  ( 9.237675586264554539, -81.00000000000000000, -5.974098161736779211 ) ) ;
#41575 = ORIENTED_EDGE ( 'NONE', *, *, #11187, .T. ) ;
#41576 = FACE_OUTER_BOUND ( 'NONE', #283, .T. ) ;
#41577 = CARTESIAN_POINT ( 'NONE',  ( -7.591546392047000325, -79.74471332859900485, -5.752267283136999865 ) ) ;
#41578 = DIRECTION ( 'NONE',  ( 0.000000000000000000, 1.000000000000000000, 0.000000000000000000 ) ) ;
#41579 = ORIENTED_EDGE ( 'NONE', *, *, #32965, .F. ) ;
#41580 = EDGE_CURVE ( 'NONE', #30569, #33154, #40859, .T. ) ;
#41581 = CARTESIAN_POINT ( 'NONE',  ( 3.250000000000000000, -1.750000000000000000, 0.000000000000000000 ) ) ;
#41582 = VERTEX_POINT ( 'NONE', #8740 ) ;
#41583 = AXIS2_PLACEMENT_3D ( 'NONE', #33585, #42465, #32701 ) ;
#41584 = B_SPLINE_CURVE_WITH_KNOTS ( 'NONE', 3,
 ( #46645, #51655, #15328, #42198, #29181, #20338, #51356, #28892, #47228, #14441, #32436, #55186, #1768, #46061, #19761, #23594, #1188, #37758 ),
 .UNSPECIFIED., .F., .F.,
 ( 4, 2, 2, 2, 2, 2, 2, 2, 4 ),
 ( 0.000000000000000000, 0.1250000000000000000, 0.2499999999999999722, 0.3750000000000000000, 0.5000000000000000000, 0.6250000000000000000, 0.7500000000000000000, 0.8750000000000000000, 1.000000000000000000 ),
 .UNSPECIFIED. ) ;
#41585 = CARTESIAN_POINT ( 'NONE',  ( -11.77559907170000031, -78.34947541138799920, -3.482965070681999897 ) ) ;
#41586 = CARTESIAN_POINT ( 'NONE',  ( -4.716706279917999289, -77.08271516049769900, -9.880723834468000177 ) ) ;
#41587 = CARTESIAN_POINT ( 'NONE',  ( 0.000000000000000000, -75.10000000284179578, -7.200000000000000178 ) ) ;
#41588 = ORIENTED_EDGE ( 'NONE', *, *, #20120, .F. ) ;
#41589 = VERTEX_POINT ( 'NONE', #17900 ) ;
#41590 = B_SPLINE_CURVE_WITH_KNOTS ( 'NONE', 3,
 ( #36400, #45574, #31665, #31960, #45279, #48324, #44174, #9549, #52742, #13963, #49711, #34997, #22827, #40838, #18408, #12294, #7864, #21439 ),
 .UNSPECIFIED., .F., .F.,
 ( 4, 2, 2, 2, 2, 2, 2, 2, 4 ),
 ( 0.000000000000000000, 0.1250000000000000000, 0.2500000000000000000, 0.3750000000000000000, 0.5000000000000000000, 0.6250000000000000000, 0.7500000000000000000, 0.8750000000000000000, 1.000000000000000000 ),
 .UNSPECIFIED. ) ;
#41591 = CARTESIAN_POINT ( 'NONE',  ( -10.01752115540999988, -55.60828330164999755, -7.660412752583999563 ) ) ;
#41592 = CARTESIAN_POINT ( 'NONE',  ( 9.534323188421000239, -79.13213671798298776, -1.008198710029000189 ) ) ;
#41593 = VERTEX_POINT ( 'NONE', #26731 ) ;
#41594 = CARTESIAN_POINT ( 'NONE',  ( 12.55458938217999965, -54.63720883353000346, 1.575070636625000242 ) ) ;
#41595 = CARTESIAN_POINT ( 'NONE',  ( 5.825949712413000192, -79.90361206703849462, 9.232191225927998346 ) ) ;
#41596 = AXIS2_PLACEMENT_3D ( 'NONE', #32491, #14205, #27779 ) ;
#41597 = FACE_OUTER_BOUND ( 'NONE', #30309, .T. ) ;
#41598 = CARTESIAN_POINT ( 'NONE',  ( 9.136202122873999798, -77.40200194988500471, 2.585973524422000125 ) ) ;
#41599 = CIRCLE ( 'NONE', #52931, 9.700000000000001066 ) ;
#41600 = CARTESIAN_POINT ( 'NONE',  ( 3.521763997193422036, -82.70470561765866080, -0.7485769115635626525 ) ) ;
#41601 = LINE ( 'NONE', #10908, #47802 ) ;
#41602 = CARTESIAN_POINT ( 'NONE',  ( 1.589609816838088552, -86.17851881763699851, 3.662844055364134377 ) ) ;
#41603 = CARTESIAN_POINT ( 'NONE',  ( 9.537698866016000920, -77.04321742767268688, 2.758499149798000261 ) ) ;
#41604 = CARTESIAN_POINT ( 'NONE',  ( 0.8611387563286860836, -78.67764650869405330, 1.274486801945468262 ) ) ;
#41605 = CARTESIAN_POINT ( 'NONE',  ( -1.001315002179000047, -24.68522411714000242, 12.50000000000000000 ) ) ;
#41606 = ORIENTED_EDGE ( 'NONE', *, *, #3957, .T. ) ;
#41607 = CARTESIAN_POINT ( 'NONE',  ( 12.21199139566000014, -76.27738052755999831, 1.550091862394999964 ) ) ;
#41608 = ADVANCED_FACE ( 'NONE', ( #26161 ), #40917, .F. ) ;
#41609 = LINE ( 'NONE', #55781, #9706 ) ;
#41610 = CARTESIAN_POINT ( 'NONE',  ( 7.636246406707999590, -60.56323123069000047, -10.30460653227000023 ) ) ;
#41611 = CARTESIAN_POINT ( 'NONE',  ( 0.4482635754052999855, -78.64524269524000033, -12.25553529036999834 ) ) ;
#41612 = CARTESIAN_POINT ( 'NONE',  ( 11.13784153760999907, -76.35071295976199224, 5.174080857020999957 ) ) ;
#41613 = CARTESIAN_POINT ( 'NONE',  ( 13.89999999994000035, -80.79999999994112159, 2.316525911784000115E-09 ) ) ;
#41614 = EDGE_CURVE ( 'NONE', #34245, #46717, #57743, .T. ) ;
#41615 = CARTESIAN_POINT ( 'NONE',  ( 12.50745077490000057, -24.99994448286999926, 2.662071812989000278E-09 ) ) ;
#41616 = CARTESIAN_POINT ( 'NONE',  ( -11.26810403927533244, -78.02092148738429955, 4.317468151549603839 ) ) ;
#41617 = FACE_OUTER_BOUND ( 'NONE', #46701, .T. ) ;
#41618 = B_SPLINE_CURVE_WITH_KNOTS ( 'NONE', 3,
 ( #1661, #6654, #11390, #1959, #42092, #42969, #38815, #2526, #42675, #11102, #43258, #19952, #20528, #2243, #15805, #37940, #34082, #2814, #19651, #15514, #51545, #55667, #7527, #51835, #29938, #38526, #52406, #47415, #20808, #11961, #37653, #16388, #56541, #51255, #56832, #20241, #6945, #42388, #16102, #56255, #34373, #47991, #15216, #10806, #28787, #46833, #6359, #55963, #33509, #29082, #47127, #24667, #48555, #49128, #3952, #8679, #7813, #35526, #53555, #12808, #17241, #52977, #26097, #16679, #48277, #40263, #13094, #58276, #35827, #31091, #30524, #8382, #57405, #26668, #13389, #39105, #44700, #30807, #25814, #4255, #8101, #57980, #43541, #39677, #22252, #17839, #3671, #21671, #52688, #3105, #53856, #16963, #34660, #49429, #31388, #25524, #21100, #35228, #39966, #57113, #17535, #12243, #30234, #43842, #21954, #21384, #57684, #3389, #39397, #34945, #12526, #48840, #44122, #53259, #26380, #44399, #19296, #1023, #46179, #13980, #27257, #36996, #50308, #45296, #54723, #14850, #36709, #9858, #447, #10151, #14266, #5704, #37288, #1303, #32263, #26965, #31976, #27840, #4847, #8980, #45885, #55304, #9564, #5417 ),
 .UNSPECIFIED., .F., .F.,
 ( 4, 2, 2, 2, 2, 2, 2, 1, 1, 1, 1, 1, 2, 2, 2, 2, 1, 2, 2, 2, 2, 1, 1, 1, 2, 2, 2, 2, 2, 1, 1, 1, 1, 1, 2, 2, 2, 2, 2, 1, 1, 1, 1, 2, 2, 2, 2, 1, 1, 1, 2, 2, 2, 1, 1, 1, 1, 2, 2, 2, 2, 1, 1, 1, 1, 1, 2, 2, 2, 2, 2, 1, 1, 1, 1, 1, 2, 2, 2, 2, 2, 1, 1, 1, 1, 1, 2, 2, 2, 2, 2, 4 ),
 ( 0.000000000000000000, 0.06250000000004092560, 0.1250000000000818512, 0.1875000000001227907, 0.2187500000001432188, 0.2343750000001534051, 0.2421875000001585121, 0.2460937500001610101, 0.2480468750001622313, 0.2490234375001628142, 0.2495117187501630918, 0.2497558593751632583, 0.2498779296876633416, 0.2500000000001634248, 0.2656250000001660339, 0.2734375000001672551, 0.2773437500001679212, 0.2792968750001681988, 0.2812500000001684763, 0.2968750000001711964, 0.3046875000001724731, 0.3085937500001730283, 0.3105468750001733613, 0.3115234375001734723, 0.3120117187501735279, 0.3125000000001736389, 0.3437500000001835754, 0.3593750000001884604, 0.3671875000001909584, 0.3710937500001921796, 0.3730468750001927902, 0.3740234375001931788, 0.3745117187501933453, 0.3747558593751934009, 0.3748779296876934009, 0.3750000000001934009, 0.4062500000001655343, 0.4218750000001516010, 0.4296875000001446621, 0.4335937500001411649, 0.4355468750001393885, 0.4365234375001385003, 0.4370117187501380562, 0.4372558593751378342, 0.4375000000001376121, 0.4687500000001073586, 0.4843750000000923150, 0.4921875000000847655, 0.4960937500000809908, 0.4980468750000791034, 0.4990234375000781042, 0.5000000000000771605, 0.5312500000000467404, 0.5468750000000315303, 0.5546875000000239808, 0.5585937500000202061, 0.5605468750000182077, 0.5615234375000173195, 0.5625000000000164313, 0.5937499999999860112, 0.6093749999999708011, 0.6171874999999632516, 0.6210937499999593658, 0.6230468749999575895, 0.6240234374999565903, 0.6245117187499561462, 0.6247558593749559241, 0.6249999999999555911, 0.6562499999999220623, 0.6718749999999052980, 0.6796874999998968603, 0.6835937499998927525, 0.6855468749998905320, 0.6865234374998895328, 0.6870117187498890887, 0.6872558593748887557, 0.6873779296873886446, 0.6874999999998885336, 0.7187499999998622213, 0.7343749999998491207, 0.7421874999998425704, 0.7460937499998392397, 0.7480468749998375744, 0.7490234374998366862, 0.7495117187498362421, 0.7497558593748360201, 0.7498779296873361311, 0.7499999999998361311, 0.8124999999998770983, 0.8749999999999180655, 0.9374999999999589217, 1.000000000000000000 ),
 .UNSPECIFIED. ) ;
#41619 = AXIS2_PLACEMENT_3D ( 'NONE', #4853, #31686, #50024 ) ;
#41620 = EDGE_LOOP ( 'NONE', ( #43383, #56975, #2665, #32532, #28791, #2747 ) ) ;
#41621 = CARTESIAN_POINT ( 'NONE',  ( 0.5113695407423999306, -82.86409087623900405, 1.250788716666000111 ) ) ;
#41622 = CARTESIAN_POINT ( 'NONE',  ( -0.5026956014243000315, -77.27223151488298925, 9.585737870937999006 ) ) ;
#41623 = CARTESIAN_POINT ( 'NONE',  ( 10.10713367717059796, -24.46653151341558896, 7.860990029285546576 ) ) ;
#41624 = FACE_OUTER_BOUND ( 'NONE', #3609, .T. ) ;
#41625 = CARTESIAN_POINT ( 'NONE',  ( -2.132401835864000006, -3.457796016549000040, -3.041072444219000470 ) ) ;
#41626 = CARTESIAN_POINT ( 'NONE',  ( -11.57073820100000106, -77.55688910291300431, 2.924640136927000089 ) ) ;
#41627 = CARTESIAN_POINT ( 'NONE',  ( -9.275907895452998986, -77.68526618914199844, 2.590510119660999866 ) ) ;
#41628 = CARTESIAN_POINT ( 'NONE',  ( 4.220281262689746349, -76.04518811977419546, 10.96961518909428435 ) ) ;
#41629 = CARTESIAN_POINT ( 'NONE',  ( -1.074445222347000017, -83.11889217614600511, -0.5709172427956999973 ) ) ;
#41630 = CARTESIAN_POINT ( 'NONE',  ( 3.922208058606658998, -86.10000000000017906, 0.4502061935813617133 ) ) ;
#41631 = EDGE_LOOP ( 'NONE', ( #11106, #25831, #6882, #13752, #52061, #6948 ) ) ;
#41632 = CARTESIAN_POINT ( 'NONE',  ( 7.648026768024999811, -18.75000001589999954, -10.12290050218000026 ) ) ;
#41633 = CARTESIAN_POINT ( 'NONE',  ( 11.89593388229870463, -79.14596860729264449, 1.243669055771579046 ) ) ;
#41635 = CARTESIAN_POINT ( 'NONE',  ( -6.536760041025257095, -76.27796683842150571, -9.763812029757714228 ) ) ;
#41634 = DIRECTION ( 'NONE',  ( 0.000000000000000000, 1.000000000000000000, 0.000000000000000000 ) ) ;
#41636 = AXIS2_PLACEMENT_3D ( 'NONE', #34979, #17277, #27585 ) ;
#41637 = CARTESIAN_POINT ( 'NONE',  ( -10.96673197750000206, -78.49365534745898287, -0.4413686857046000278 ) ) ;
#41638 = CARTESIAN_POINT ( 'NONE',  ( 8.796335266379964324, -79.29791666666666572, -6.760013919724084275 ) ) ;
#41639 = CARTESIAN_POINT ( 'NONE',  ( -12.48473257364000055, -76.86897319096500780, 0.6967103256584999960 ) ) ;
#41640 = CARTESIAN_POINT ( 'NONE',  ( -0.006340012436140875923, -79.22516103717930491, -1.262873609533169628 ) ) ;
#41641 = CARTESIAN_POINT ( 'NONE',  ( 10.47513558174000003, -18.19636614430000066, -7.624778818008999259 ) ) ;
#41642 = CARTESIAN_POINT ( 'NONE',  ( -0.5999999999999999778, -18.84999999999000053, -11.79999999999999893 ) ) ;
#41643 = ORIENTED_EDGE ( 'NONE', *, *, #22297, .F. ) ;
#41644 = AXIS2_PLACEMENT_3D ( 'NONE', #27408, #4985, #22992 ) ;
#41645 = CARTESIAN_POINT ( 'NONE',  ( -0.2300833467695000134, -78.39998243216399487, -11.11357981391999949 ) ) ;
#41646 = DIRECTION ( 'NONE',  ( 0.000000000000000000, -1.000000000000000000, 0.000000000000000000 ) ) ;
#41647 = CARTESIAN_POINT ( 'NONE',  ( -11.02119874838501801, -79.57957167422193834, -4.309175828380967133 ) ) ;
#41648 = CARTESIAN_POINT ( 'NONE',  ( 2.148673218084974135, -78.39678895079168797, 3.720415760332554278 ) ) ;
#41649 = B_SPLINE_CURVE_WITH_KNOTS ( 'NONE', 3,
 ( #17452, #43465, #57321, #31300, #30149, #21874 ),
 .UNSPECIFIED., .F., .F.,
 ( 4, 2, 4 ),
 ( 0.000000000000000000, 0.5000000000000000000, 1.000000000000000000 ),
 .UNSPECIFIED. ) ;
#41650 = CARTESIAN_POINT ( 'NONE',  ( 4.591369065251983628, -77.29683506230675505, 11.11224176324230228 ) ) ;
#41651 = CARTESIAN_POINT ( 'NONE',  ( 0.000000000000000000, -87.59999999999999432, 0.000000000000000000 ) ) ;
#41652 = ADVANCED_FACE ( 'NONE', ( #26437 ), #15180, .F. ) ;
#41653 = CARTESIAN_POINT ( 'NONE',  ( -7.919595949288999570, -59.94999999040999938, 9.050966798898000931 ) ) ;
#41654 = EDGE_CURVE ( 'NONE', #32058, #45010, #28144, .T. ) ;
#41655 = CARTESIAN_POINT ( 'NONE',  ( -0.5543002251722001228, -79.23645473738000078, -1.308779764949999924 ) ) ;
#41656 = LINE ( 'NONE', #31905, #54711 ) ;
#41657 = CARTESIAN_POINT ( 'NONE',  ( -7.508608642448520776, -79.01514983751106058, -8.005536529047017069 ) ) ;
#41658 = FACE_OUTER_BOUND ( 'NONE', #26749, .T. ) ;
#41659 = VERTEX_POINT ( 'NONE', #31379 ) ;
#41660 = ORIENTED_EDGE ( 'NONE', *, *, #27537, .T. ) ;
#41661 = CARTESIAN_POINT ( 'NONE',  ( 0.3023719455682368218, -77.77249999999999375, 9.537307262745171599 ) ) ;
#41662 = CARTESIAN_POINT ( 'NONE',  ( 6.218583900441460699, -78.77425322109141348, -8.769005864712987375 ) ) ;
#41663 = ORIENTED_EDGE ( 'NONE', *, *, #58241, .T. ) ;
#41664 = CARTESIAN_POINT ( 'NONE',  ( -5.007180289739999068, -76.66194096900252930, 10.00009952528999868 ) ) ;
#41665 = CARTESIAN_POINT ( 'NONE',  ( 0.2803209884194523549, -83.59479168018397388, -3.431695889835921776 ) ) ;
#41666 = ADVANCED_FACE ( 'NONE', ( #4245 ), #48545, .F. ) ;
#41667 = CARTESIAN_POINT ( 'NONE',  ( 0.1963495408493571848, -80.26458333333334849, 1.500000000000000666 ) ) ;
#41668 = CARTESIAN_POINT ( 'NONE',  ( 10.52682159652000138, -60.22567232035000018, 7.605689092069000345 ) ) ;
#41669 = CARTESIAN_POINT ( 'NONE',  ( -12.17523484611175100, -76.55441792555106417, -0.7718671096416708233 ) ) ;
#41670 = CARTESIAN_POINT ( 'NONE',  ( 10.42518013479882022, -77.25890890101139519, -5.902164117432179502 ) ) ;
#41671 = CARTESIAN_POINT ( 'NONE',  ( -7.408849624938999234, -79.33369078296900057, -8.421820339245000397 ) ) ;
#41672 = ORIENTED_EDGE ( 'NONE', *, *, #3355, .T. ) ;
#41673 = DIRECTION ( 'NONE',  ( 0.000000000000000000, 1.000000000000000000, 0.000000000000000000 ) ) ;
#41674 = VERTEX_POINT ( 'NONE', #36920 ) ;
#41675 = CARTESIAN_POINT ( 'NONE',  ( 9.129142538877060176, -77.36303958135555092, 1.489769077664636843 ) ) ;
#41676 = CARTESIAN_POINT ( 'NONE',  ( -1.108343018679999847, -79.28756650451100541, -0.7155276831893999656 ) ) ;
#41677 = AXIS2_PLACEMENT_3D ( 'NONE', #32798, #15100, #50846 ) ;
#41678 = DIRECTION ( 'NONE',  ( -1.000000000000000000, 0.000000000000000000, 0.000000000000000000 ) ) ;
#41679 = CIRCLE ( 'NONE', #20817, 3.000000000000000000 ) ;
#41680 = CARTESIAN_POINT ( 'NONE',  ( -9.282419925074000489, -77.41400144119299398, -2.829762163499999872 ) ) ;
#41681 = CARTESIAN_POINT ( 'NONE',  ( -8.666925696772263876, -17.00708316157611577, 9.019429295400886559 ) ) ;
#41682 = DIRECTION ( 'NONE',  ( 0.7071067811865475727, 0.000000000000000000, 0.7071067811865475727 ) ) ;
#41683 = CARTESIAN_POINT ( 'NONE',  ( 1.619712389308999967, -79.02816550114999927, 0.1587296492880999887 ) ) ;
#41684 = CARTESIAN_POINT ( 'NONE',  ( 0.6656042537174000628, -82.13207046129099353, -4.118670586540000400 ) ) ;
#41685 = EDGE_CURVE ( 'NONE', #29148, #53060, #4133, .T. ) ;
#41686 = CARTESIAN_POINT ( 'NONE',  ( 0.9061038674864000386, -78.79758795410299399, 10.90260483175000061 ) ) ;
#41687 = CARTESIAN_POINT ( 'NONE',  ( 12.70610460585974621, -61.25512899773330133, 1.580683093980798315 ) ) ;
#41688 = B_SPLINE_CURVE_WITH_KNOTS ( 'NONE', 3,
 ( #47592, #43721, #52285, #3274, #25976, #33967, #16557, #52857, #11842, #16847, #48437, #29823, #12123, #12411, #56995, #7403, #17127, #30109 ),
 .UNSPECIFIED., .F., .F.,
 ( 4, 2, 2, 2, 2, 2, 2, 2, 4 ),
 ( 0.000000000000000000, 0.1250000000000000833, 0.2500000000000001110, 0.3750000000000000000, 0.4999999999999999445, 0.6249999999999998890, 0.7499999999999997780, 0.8749999999999998890, 1.000000000000000000 ),
 .UNSPECIFIED. ) ;
#41689 = DIRECTION ( 'NONE',  ( 2.044033345360999863E-13, 0.000000000000000000, -1.000000000000000000 ) ) ;
#41690 = CARTESIAN_POINT ( 'NONE',  ( -1.507731777991000000, -84.78318437814699848, -3.257374696832999739 ) ) ;
#41691 = ORIENTED_EDGE ( 'NONE', *, *, #6625, .T. ) ;
#41692 = CARTESIAN_POINT ( 'NONE',  ( 7.374560639698994002, -79.57708333333330586, -9.596002108778151296 ) ) ;
#41693 = CARTESIAN_POINT ( 'NONE',  ( 0.1615182143923999947, -76.15048332335200598, 11.61153150973999892 ) ) ;
#41694 = CARTESIAN_POINT ( 'NONE',  ( -0.1351391521504822224, -77.97607996944202569, 10.74916312770440818 ) ) ;
#41695 = CARTESIAN_POINT ( 'NONE',  ( -0.7928179559538000021, -78.68583547745299711, -11.95355612866999984 ) ) ;
#41696 = CARTESIAN_POINT ( 'NONE',  ( -7.657744736620999859, -18.33080421803999727, 9.966195456754999071 ) ) ;
#41697 = CONICAL_SURFACE ( 'NONE', #1224, 10.59999999997999787, 0.7853981633972997312 ) ;
#41698 = FACE_OUTER_BOUND ( 'NONE', #21932, .T. ) ;
#41699 = CARTESIAN_POINT ( 'NONE',  ( 1.483582653850644473, -3.409532918301972249, -3.194058075009992947 ) ) ;
#41700 = CARTESIAN_POINT ( 'NONE',  ( -9.601739433208001273, -79.20275584965399673, -1.533141744029000053 ) ) ;
#41701 = CARTESIAN_POINT ( 'NONE',  ( -6.279067761433998918, -78.01229597363898449, 7.013166371532999932 ) ) ;
#41702 = CARTESIAN_POINT ( 'NONE',  ( -6.128066803784989247, -85.83735717367099483, -5.039913953694903803 ) ) ;
#41703 = CARTESIAN_POINT ( 'NONE',  ( -6.550114462690999950, -77.03327565549399480, -8.876808543633000426 ) ) ;
#41704 = CARTESIAN_POINT ( 'NONE',  ( -8.987350104473000201, -77.09032746636262345, 8.369597699504998545 ) ) ;
#41705 = CARTESIAN_POINT ( 'NONE',  ( 9.617955526353000550, -80.74951758108093713, 5.390926903509000390 ) ) ;
#41706 = B_SPLINE_CURVE_WITH_KNOTS ( 'NONE', 3,
 ( #38372, #28339, #1806, #56394, #10660, #42816 ),
 .UNSPECIFIED., .F., .F.,
 ( 4, 1, 1, 4 ),
 ( 0.000000000000000000, 0.3333333333333000081, 0.6666666666667000474, 0.9999998688569559091 ),
 .UNSPECIFIED. ) ;
#41707 = EDGE_LOOP ( 'NONE', ( #57197, #3678 ) ) ;
#41708 = CARTESIAN_POINT ( 'NONE',  ( -2.061613410425999771, -60.00570014443000133, -12.83797036857999885 ) ) ;
#41709 = CARTESIAN_POINT ( 'NONE',  ( 5.387639657779031310, -80.43347167844690659, 9.329096843696712327 ) ) ;
#41710 = CARTESIAN_POINT ( 'NONE',  ( -10.58728162385000005, -77.67152861243299355, 3.705074683290000337 ) ) ;
#41711 = CARTESIAN_POINT ( 'NONE',  ( 9.304500756975000897, -79.01505542876398636, -5.821536072646999571 ) ) ;
#41712 = CARTESIAN_POINT ( 'NONE',  ( -12.76303204294999993, -23.26485150694999859, 1.980584515756000030 ) ) ;
#41713 = DIRECTION ( 'NONE',  ( -1.000000000000000000, 0.000000000000000000, 0.000000000000000000 ) ) ;
#41714 = DIRECTION ( 'NONE',  ( -1.000000000000000000, 0.000000000000000000, 0.000000000000000000 ) ) ;
#41715 = CARTESIAN_POINT ( 'NONE',  ( 9.722718241315000398, -55.54999999966999980, 7.954951288349001004 ) ) ;
#41716 = CARTESIAN_POINT ( 'NONE',  ( -3.884332861548999816, -84.59819503318799150, 1.523817745045000116 ) ) ;
#41717 = CARTESIAN_POINT ( 'NONE',  ( 0.3926218265389159190, -80.35416666666668561, 1.460959015002474715 ) ) ;
#41718 = CARTESIAN_POINT ( 'NONE',  ( 10.18114972180999978, -55.40990354248999950, -7.633087078966999783 ) ) ;
#41719 = CARTESIAN_POINT ( 'NONE',  ( -2.318770996637999904, -77.66809300996099807, 11.02076520135999971 ) ) ;
#41720 = CARTESIAN_POINT ( 'NONE',  ( -1.387963714323000142, -79.66454266569999731, 0.9213108730841000904 ) ) ;
#41721 = CARTESIAN_POINT ( 'NONE',  ( -10.42531125068999920, -23.26485145404000221, 7.624341767093000044 ) ) ;
#41722 = CARTESIAN_POINT ( 'NONE',  ( -6.043427764450786555, -79.38333333333332575, -10.48543666025110177 ) ) ;
#41723 = CARTESIAN_POINT ( 'NONE',  ( -0.3338606378991729740, -81.35724788051247458, -1.472545958893958673 ) ) ;
#41724 = VECTOR ( 'NONE', #39776, 1000.000000000000000 ) ;
#41725 = CARTESIAN_POINT ( 'NONE',  ( 0.000000000000000000, -76.00000000000000000, 0.000000000000000000 ) ) ;
#41726 = CARTESIAN_POINT ( 'NONE',  ( 5.330173052271000245, -78.18464638465644612, 9.594439332582000546 ) ) ;
#41727 = CARTESIAN_POINT ( 'NONE',  ( 1.131032139596482189, -79.81496092797256381, -0.5356056669552815563 ) ) ;
#41728 = CARTESIAN_POINT ( 'NONE',  ( 1.249734714957977388, -80.86107366444541356, 0.1638716315211910246 ) ) ;
#41729 = ORIENTED_EDGE ( 'NONE', *, *, #45605, .T. ) ;
#41730 = CARTESIAN_POINT ( 'NONE',  ( 0.4310498522562998258, -81.75308031528319930, -1.176456706122102069 ) ) ;
#41731 = VECTOR ( 'NONE', #2694, 1000.000000000000000 ) ;
#41732 = CARTESIAN_POINT ( 'NONE',  ( -4.084105282113999813, -79.55368493481499570, -10.24801534084000032 ) ) ;
#41733 = CYLINDRICAL_SURFACE ( 'NONE', #13904, 1.500000000000000000 ) ;
#41734 = ORIENTED_EDGE ( 'NONE', *, *, #15574, .T. ) ;
#41735 = ORIENTED_EDGE ( 'NONE', *, *, #8883, .T. ) ;
#41737 = B_SPLINE_CURVE_WITH_KNOTS ( 'NONE', 3,
 ( #36250, #14676, #1138, #49849, #19418, #32674, #9684, #28248, #5252, #14974, #54842, #54270, #18547, #41267, #31806, #9393, #50430, #9980, #27960, #19125, #46010, #5532, #23542, #32972, #46597, #22968, #37118, #50727, #42147, #29420, #11157, #2579, #2012, #55729, #52960, #26079, #20010, #43022, #29131, #33561, #30508, #20291, #42732, #2295, #24428, #15860, #6710, #24719, #6999, #33267, #51599, #51307, #10866, #38285, #34129, #15272, #44104, #56307, #37992, #47178, #6415, #47473, #28837, #16153, #25001, #20580, #33847, #51884, #11441, #38578, #56594, #12509, #46886, #48536, #8082, #3653, #1716, #19709, #37707, #42444, #15567, #56018, #14874, #55329 ),
 .UNSPECIFIED., .F., .F.,
 ( 4, 2, 1, 2, 2, 2, 2, 2, 2, 2, 1, 2, 2, 2, 2, 2, 2, 2, 1, 2, 2, 2, 2, 2, 2, 2, 1, 2, 2, 2, 2, 2, 2, 2, 1, 2, 2, 2, 2, 2, 2, 2, 1, 2, 4 ),
 ( 0.000000000000000000, 0.01562500000000001735, 0.03125000000000003469, 0.04687500000000006245, 0.06250000000000008327, 0.09375000000000012490, 0.1250000000000001665, 0.1562500000000001943, 0.1875000000000002776, 0.2031250000000002776, 0.2187500000000003053, 0.2343750000000003053, 0.2500000000000003331, 0.2812500000000003886, 0.3125000000000003886, 0.3437500000000003886, 0.3750000000000004441, 0.3906250000000004441, 0.4062500000000004441, 0.4218750000000004441, 0.4375000000000004996, 0.4687500000000004996, 0.5000000000000005551, 0.5312500000000005551, 0.5625000000000006661, 0.5781250000000006661, 0.5937500000000006661, 0.6093750000000006661, 0.6250000000000006661, 0.6562500000000006661, 0.6875000000000005551, 0.7187500000000004441, 0.7500000000000003331, 0.7656250000000004441, 0.7812500000000004441, 0.7968750000000004441, 0.8125000000000004441, 0.8437500000000003331, 0.8750000000000003331, 0.9062500000000002220, 0.9375000000000001110, 0.9531250000000001110, 0.9687500000000000000, 0.9843750000000000000, 1.000000000000000000 ),
 .UNSPECIFIED. ) ;
#41736 = CARTESIAN_POINT ( 'NONE',  ( 0.2289205461632000116, -81.96478034575399363, 1.399162150599000176 ) ) ;
#41738 = ORIENTED_EDGE ( 'NONE', *, *, #49680, .T. ) ;
#41739 = ORIENTED_EDGE ( 'NONE', *, *, #9213, .F. ) ;
#41740 = CARTESIAN_POINT ( 'NONE',  ( -1.460959015002474937, -81.97916666667948959, 0.3926218265389144757 ) ) ;
#41741 = AXIS2_PLACEMENT_3D ( 'NONE', #45074, #23207, #17910 ) ;
#41742 = CARTESIAN_POINT ( 'NONE',  ( -1.493489583059197878, -77.75651041671019925, -0.1963495429841721485 ) ) ;
#41743 = SHAPE_DEFINITION_REPRESENTATION ( #17763, #7439 ) ;
#41744 = EDGE_CURVE ( 'NONE', #39513, #41458, #11965, .T. ) ;
#41745 = CARTESIAN_POINT ( 'NONE',  ( 1.651882416763933437, -81.20520832075965245, 3.020993344137217207 ) ) ;
#41746 = AXIS2_PLACEMENT_3D ( 'NONE', #31289, #49629, #49334 ) ;
#41747 = CARTESIAN_POINT ( 'NONE',  ( -3.133069020688000084, -79.42036001420198943, -9.520158728599000142 ) ) ;
#41748 = CARTESIAN_POINT ( 'NONE',  ( 3.554000211758443051, -78.25642266958941207, -8.539967886276961906 ) ) ;
#41749 = DIRECTION ( 'NONE',  ( -1.000000000000000000, 0.000000000000000000, 0.000000000000000000 ) ) ;
#41750 = ORIENTED_EDGE ( 'NONE', *, *, #280, .T. ) ;
#41751 = ORIENTED_EDGE ( 'NONE', *, *, #21169, .F. ) ;
#41752 = CARTESIAN_POINT ( 'NONE',  ( -7.972207510795373153, -77.55765093248844266, 4.695355910174569658 ) ) ;
#41753 = CARTESIAN_POINT ( 'NONE',  ( 6.586108526242999694, -80.07391735373440156, 8.810401493720998900 ) ) ;
#41754 = CARTESIAN_POINT ( 'NONE',  ( -1.199500263597274685, -79.44791666666668561, 0.9218200799623673669 ) ) ;
#41755 = DIRECTION ( 'NONE',  ( 0.9999999924279685537, 0.000000000000000000, 0.0001230612157836962969 ) ) ;
#41756 = CARTESIAN_POINT ( 'NONE',  ( 5.927986824875999261, -77.94714365981798210, -7.683077610609999830 ) ) ;
#41757 = DIRECTION ( 'NONE',  ( 1.000000000000000000, 0.000000000000000000, 0.000000000000000000 ) ) ;
#41758 = CARTESIAN_POINT ( 'NONE',  ( -10.21380041493000057, -22.77152778045000048, 7.668936932623999780 ) ) ;
#41759 = CARTESIAN_POINT ( 'NONE',  ( -1.570796326794937636, -76.78541666666666288, 11.99999999999999467 ) ) ;
#41760 = EDGE_CURVE ( 'NONE', #38246, #37150, #22039, .T. ) ;
#41761 = CARTESIAN_POINT ( 'NONE',  ( -9.444256657865821580, -77.54794693750339718, 0.2255349141366999877 ) ) ;
#41762 = CARTESIAN_POINT ( 'NONE',  ( 0.2689332326338723100, -76.57310917009351670, 11.74710904988357640 ) ) ;
#41763 = CARTESIAN_POINT ( 'NONE',  ( 3.795871755532000513, -79.40398657535959615, -1.738093195592000040 ) ) ;
#41765 = AXIS2_PLACEMENT_3D ( 'NONE', #15629, #33625, #20638 ) ;
#41764 = CARTESIAN_POINT ( 'NONE',  ( 3.228614917279000185, -80.91423663227269003, -10.79283437469000084 ) ) ;
#41766 = CARTESIAN_POINT ( 'NONE',  ( -5.485200302047999799, -78.64776001420199236, -7.984597978739000901 ) ) ;
#41767 = CARTESIAN_POINT ( 'NONE',  ( 10.48543666025108045, -77.19166666666664867, 6.043427764450817641 ) ) ;
#41768 = CARTESIAN_POINT ( 'NONE',  ( -2.658223501415000189, -81.88530496681200077, -2.348490597694000037 ) ) ;
#41769 = CARTESIAN_POINT ( 'NONE',  ( -1.327706488546999797, -79.18557347086598952, -0.1249263990498000187 ) ) ;
#41770 = CARTESIAN_POINT ( 'NONE',  ( -2.421446639644671883, -79.49607851752138288, 9.010234589867415878 ) ) ;
#41771 = CARTESIAN_POINT ( 'NONE',  ( -12.76303204294000082, -18.73514849292999784, -1.980584515756000030 ) ) ;
#41772 = ADVANCED_FACE ( 'NONE', ( #14661 ), #32404, .T. ) ;
#41773 = CARTESIAN_POINT ( 'NONE',  ( 2.534829140202000008, -2.134334759237999979, 2.839140403360000509 ) ) ;
#41774 = CARTESIAN_POINT ( 'NONE',  ( -9.599999999916001059, -87.30000000008399752, 6.531558194539000517E-10 ) ) ;
#41775 = ORIENTED_EDGE ( 'NONE', *, *, #15217, .T. ) ;
#41776 = CARTESIAN_POINT ( 'NONE',  ( -11.55514622821841542, -78.81666666666667709, -2.460715419382146774 ) ) ;
#41777 = CARTESIAN_POINT ( 'NONE',  ( 8.188331488387794010, -60.02841244177609070, -7.345153731672020569 ) ) ;
#41778 = CIRCLE ( 'NONE', #31378, 0.8000000000000011546 ) ;
#41779 = EDGE_CURVE ( 'NONE', #10966, #27787, #5684, .T. ) ;
#41780 = CARTESIAN_POINT ( 'NONE',  ( 2.879226727952084897, -79.05416666666667425, 10.71369944335147117 ) ) ;
#41781 = CARTESIAN_POINT ( 'NONE',  ( 1.667936688463999895, -56.03513569577999931, 12.53239398060000021 ) ) ;
#41782 = CARTESIAN_POINT ( 'NONE',  ( 1.750000000000000000, -21.75064714178000003, -12.65372179279999898 ) ) ;
#41783 = CARTESIAN_POINT ( 'NONE',  ( 7.588639323636114931, -79.41262821244031045, 7.614128156161688032 ) ) ;
#41784 = AXIS2_PLACEMENT_3D ( 'NONE', #36031, #46085, #5610 ) ;
#41785 = CARTESIAN_POINT ( 'NONE',  ( -2.410095898663000114, -79.33801332859898992, 9.435914216412999878 ) ) ;
#41786 = VECTOR ( 'NONE', #52813, 1000.000000000000114 ) ;
#41787 = DIRECTION ( 'NONE',  ( 0.000000000000000000, 1.000000000000000000, 0.000000000000000000 ) ) ;
#41788 = CARTESIAN_POINT ( 'NONE',  ( 9.921600000191999058, -77.46856652213799066, 5.354231256300999497 ) ) ;
#41789 = CARTESIAN_POINT ( 'NONE',  ( -1.187247102542000166, -81.96674830889799068, -1.078697698851999842 ) ) ;
#41790 = DIRECTION ( 'NONE',  ( 0.000000000000000000, 0.000000000000000000, -1.000000000000000000 ) ) ;
#41791 = CARTESIAN_POINT ( 'NONE',  ( 7.038692338534999315, -77.82859895515098003, 6.250440358128999563 ) ) ;
#41793 = DIRECTION ( 'NONE',  ( -0.7071067811865969777, -0.7071067811864980568, 8.468117720049969248E-09 ) ) ;
#41792 = CARTESIAN_POINT ( 'NONE',  ( 0.2985038077467999651, -82.50228596008699355, 3.951822424672999823 ) ) ;
#41794 = CARTESIAN_POINT ( 'NONE',  ( 6.479078291783999966, -79.31435194988499404, -7.022474634662000170 ) ) ;
#41795 = CARTESIAN_POINT ( 'NONE',  ( -12.04999999926000243, -79.29999999926000953, -5.384918809984000181E-09 ) ) ;
#41796 = CARTESIAN_POINT ( 'NONE',  ( -0.9462876233756999378, -80.09670878855399678, 0.9192961133846000443 ) ) ;
#41797 = EDGE_CURVE ( 'NONE', #37205, #27512, #57861, .T. ) ;
#41798 = CARTESIAN_POINT ( 'NONE',  ( -10.75000000000000000, -80.59999999999999432, 0.000000000000000000 ) ) ;
#41799 = CARTESIAN_POINT ( 'NONE',  ( -5.800000004703999679, -81.00000000470399186, 2.775962718112000159E-08 ) ) ;
#41800 = EDGE_LOOP ( 'NONE', ( #50222, #20392, #53563, #23039 ) ) ;
#41801 = CARTESIAN_POINT ( 'NONE',  ( -2.112861425255000203, -79.24484432466799433, -11.84242215301999934 ) ) ;
#41802 = DIRECTION ( 'NONE',  ( 0.000000000000000000, -0.7071067811866525998, -0.7071067811864425456 ) ) ;
#41803 = B_SPLINE_CURVE_WITH_KNOTS ( 'NONE', 3,
 ( #20889, #16184, #34453, #53343, #7604, #43335, #25604, #17325, #21751, #8184, #35311, #57480, #44202, #12041, #25319, #53055, #12608, #52485, #47784, #12888, #43627 ),
 .UNSPECIFIED., .F., .F.,
 ( 4, 2, 2, 2, 2, 2, 2, 2, 2, 1, 4 ),
 ( 0.000000000000000000, 0.1249999999999999722, 0.2499999999999999445, 0.3750000000000000000, 0.5000000000000001110, 0.5625000000000001110, 0.6250000000000001110, 0.7500000000000001110, 0.8125000000000001110, 0.8750000000000001110, 1.000000000000000000 ),
 .UNSPECIFIED. ) ;
#41804 = DIRECTION ( 'NONE',  ( 1.000000000000000000, 0.000000000000000000, 0.000000000000000000 ) ) ;
#41805 = ORIENTED_EDGE ( 'NONE', *, *, #18771, .F. ) ;
#41806 = DIRECTION ( 'NONE',  ( 3.655298286142000429E-11, 1.000000000000000000, -1.590757977788000024E-09 ) ) ;
#41807 = EDGE_LOOP ( 'NONE', ( #12313, #5911, #35535, #38316, #48707, #26809, #29233, #52238, #2324 ) ) ;
#41808 = ORIENTED_EDGE ( 'NONE', *, *, #28852, .F. ) ;
#41809 = CARTESIAN_POINT ( 'NONE',  ( 7.995796640822063317, -60.48684619742046920, 7.555116226629825071 ) ) ;
#41810 = ORIENTED_EDGE ( 'NONE', *, *, #4758, .T. ) ;
#41811 = AXIS2_PLACEMENT_3D ( 'NONE', #2982, #56425, #42850 ) ;
#41812 = CARTESIAN_POINT ( 'NONE',  ( 2.111974152998999710, -79.20841833893540240, -2.850284762170999908 ) ) ;
#41813 = CARTESIAN_POINT ( 'NONE',  ( -12.76303204522000101, -23.26485147686999966, -1.980584515753000208 ) ) ;
#41814 = VERTEX_POINT ( 'NONE', #9667 ) ;
#41815 = CARTESIAN_POINT ( 'NONE',  ( 1.204475114971339522, -82.82837777568340698, -0.3367243055637897942 ) ) ;
#41816 = CARTESIAN_POINT ( 'NONE',  ( -7.718346056121999865, -57.05111654290000445, 10.07719973194999952 ) ) ;
#41817 = ORIENTED_EDGE ( 'NONE', *, *, #31153, .F. ) ;
#41818 = CARTESIAN_POINT ( 'NONE',  ( 0.6056591908766266741, -79.23038445115356865, -9.249560979224405344 ) ) ;
#41819 = CARTESIAN_POINT ( 'NONE',  ( -0.2201363562291999698, -79.36327907013999550, -1.483758735329000045 ) ) ;
#41820 = CARTESIAN_POINT ( 'NONE',  ( -10.98928341260028674, -79.80000000000001137, -4.685202055221748374 ) ) ;
#41821 = VECTOR ( 'NONE', #32099, 1000.000000000000000 ) ;
#41822 = DIRECTION ( 'NONE',  ( 0.000000000000000000, 0.000000000000000000, -1.000000000000000000 ) ) ;
#41823 = CARTESIAN_POINT ( 'NONE',  ( -9.356372444455999471, -78.89426924292401111, 7.928823137711024316 ) ) ;
#41824 = CARTESIAN_POINT ( 'NONE',  ( 9.131029190779001325, -77.47251433190575653, -3.285576857342999535 ) ) ;
#41825 = CARTESIAN_POINT ( 'NONE',  ( 10.12567350656000009, -76.05099845009399928, 4.748118780173999909 ) ) ;
#41826 = CARTESIAN_POINT ( 'NONE',  ( -9.199999999968001774, -80.60000000003199716, 3.388760884947000060E-10 ) ) ;
#41827 = AXIS2_PLACEMENT_3D ( 'NONE', #12658, #7941, #26810 ) ;
#41828 = ADVANCED_FACE ( 'NONE', ( #27656 ), #45698, .F. ) ;
#41829 = FACE_OUTER_BOUND ( 'NONE', #6607, .T. ) ;
#41830 = CARTESIAN_POINT ( 'NONE',  ( 7.640030264173999441, -60.10716680829000325, -10.18491080495000034 ) ) ;
#41831 = CARTESIAN_POINT ( 'NONE',  ( -3.762297919178509531, -78.69173512211914101, -8.453695876167582668 ) ) ;
#41832 = EDGE_CURVE ( 'NONE', #43717, #58122, #7776, .T. ) ;
#41833 = CARTESIAN_POINT ( 'NONE',  ( 9.381339102657999973, -77.31428501420199950, -0.7531566933248999840 ) ) ;
#41834 = CARTESIAN_POINT ( 'NONE',  ( 1.329937235669000017, -79.37841350325899725, -0.09921221311570001256 ) ) ;
#41835 = CARTESIAN_POINT ( 'NONE',  ( -7.609649279793637255, -80.16460715866527664, -7.942784592428623114 ) ) ;
#41836 = CARTESIAN_POINT ( 'NONE',  ( -4.784380313523580064, -77.21666666666669698, 8.300970689365431809 ) ) ;
#41837 = CARTESIAN_POINT ( 'NONE',  ( -0.06054963955015999627, -79.64017549782629146, 4.129750263999999227 ) ) ;
#41838 = CARTESIAN_POINT ( 'NONE',  ( -7.200293548019001122, -77.63511332859900449, 6.428765836700999436 ) ) ;
#41839 = DIRECTION ( 'NONE',  ( 1.000000000000000000, 0.000000000000000000, 0.000000000000000000 ) ) ;
#41840 = CARTESIAN_POINT ( 'NONE',  ( 1.124534988792357471, -82.88598862276096213, 0.5462022235247268043 ) ) ;
#41841 = CARTESIAN_POINT ( 'NONE',  ( 8.803297119250066416, -77.11875000000000568, -3.648104604236618087 ) ) ;
#41842 = CARTESIAN_POINT ( 'NONE',  ( -1.250652913346715689, -78.08346917523292063, 0.2616640092690510899 ) ) ;
#41843 = CARTESIAN_POINT ( 'NONE',  ( 0.000000000000000000, -49.87071424677999687, 0.000000000000000000 ) ) ;
#41844 = ADVANCED_FACE ( 'NONE', ( #24703 ), #38987, .T. ) ;
#41845 = CARTESIAN_POINT ( 'NONE',  ( 12.70395504299397693, -24.60679290123844609, -1.447100708825584947 ) ) ;
#41846 = CARTESIAN_POINT ( 'NONE',  ( -1.460729357738999923, -24.09091243203000232, -12.44211643240000065 ) ) ;
#41847 = CARTESIAN_POINT ( 'NONE',  ( -3.283483138947000057, -2.071609528251000309, -1.169594691854000112 ) ) ;
#41848 = CARTESIAN_POINT ( 'NONE',  ( 12.70956478397999945, -23.40497526616000101, 1.933781249744999986 ) ) ;
#41849 = PRODUCT ( 'Push Button Connector', 'Push Button Connector', '', ( #51493 ) ) ;
#41850 = CARTESIAN_POINT ( 'NONE',  ( 12.09396573961999799, -77.10954407085999662, -2.128801122353999986 ) ) ;
#41851 = CARTESIAN_POINT ( 'NONE',  ( -0.5999999998848000171, -18.85000000520999919, 11.79999999988000070 ) ) ;
#41852 = CARTESIAN_POINT ( 'NONE',  ( -1.208267226912113079, -24.82590682154043904, -12.70228502423716854 ) ) ;
#41853 = CARTESIAN_POINT ( 'NONE',  ( -6.294415428860999917, -76.25044869620001009, -10.46488830663000158 ) ) ;
#41854 =( BOUNDED_SURFACE ( )  B_SPLINE_SURFACE ( 3, 3, ( 
 ( #4066, #48952, #45123, #40684 ),
 ( #26491, #57508, #17953, #276 ),
 ( #18254, #36247, #35051, #53086 ),
 ( #44515, #9094, #12640, #30632 ),
 ( #3777, #48665, #8210, #35945 ),
 ( #53972, #31503, #14971, #18545 ),
 ( #41553, #46594, #37703, #19414 ) ),
 .UNSPECIFIED., .F., .F., .F. ) 
 B_SPLINE_SURFACE_WITH_KNOTS ( ( 4, 3, 4 ),
 ( 4, 4 ),
 ( 0.000000000000000000, 1.000000000000000000, 2.000000000000000000 ),
 ( 0.000000000000000000, 1.000000000000000000 ),
 .UNSPECIFIED. ) 
 GEOMETRIC_REPRESENTATION_ITEM ( )  RATIONAL_B_SPLINE_SURFACE ( (
 ( 1.196373642248999891, 1.184225762575999985, 1.184225762575999985, 1.196373642248999891),
 ( 0.9447739570234999773, 0.9351807998836999536, 0.9351807998836999536, 0.9447739570234999773),
 ( 0.9447739570234999773, 0.9351807998836999536, 0.9351807998836999536, 0.9447739570234999773),
 ( 1.196373642248999891, 1.184225762575999985, 1.184225762575999985, 1.196373642248999891),
 ( 0.9447739570234999773, 0.9351807998836999536, 0.9351807998836999536, 0.9447739570234999773),
 ( 0.9447739570234999773, 0.9351807998836999536, 0.9351807998836999536, 0.9447739570234999773),
 ( 1.196373642248999891, 1.184225762575999985, 1.184225762575999985, 1.196373642248999891) ) ) 
 REPRESENTATION_ITEM ( '' )  SURFACE ( )  );
#41855 = ORIENTED_EDGE ( 'NONE', *, *, #25909, .T. ) ;
#41856 = CARTESIAN_POINT ( 'NONE',  ( 0.2985269866015999862, -83.11171544543098832, 3.951819513428000086 ) ) ;
#41857 = CIRCLE ( 'NONE', #30504, 13.86363636363999952 ) ;
#41858 = CARTESIAN_POINT ( 'NONE',  ( 8.557023385002000992, -79.94353216860270095, 6.619562533252000947 ) ) ;
#41859 = CARTESIAN_POINT ( 'NONE',  ( 7.565568292094223324, -78.30138424788611928, -5.321967902146258034 ) ) ;
#41860 = CARTESIAN_POINT ( 'NONE',  ( 10.10448976474820704, -54.34884052575311841, 7.864761218125428499 ) ) ;
#41861 = CARTESIAN_POINT ( 'NONE',  ( -5.859445663532000914, -77.82042158625800710, 9.564779511708000115 ) ) ;
#41862 = CARTESIAN_POINT ( 'NONE',  ( 12.43570956081999945, -53.92016029949000000, -0.4384071701244000030 ) ) ;
#41863 = CARTESIAN_POINT ( 'NONE',  ( 7.600999290758999827, -78.69568149309900207, 5.914221820906000460 ) ) ;
#41864 = FACE_OUTER_BOUND ( 'NONE', #229, .T. ) ;
#41865 = PLANE ( 'NONE',  #51056 ) ;
#41866 = CARTESIAN_POINT ( 'NONE',  ( -7.341957592364786400, -76.13333333332644770, 8.159497658145225429 ) ) ;
#41867 = EDGE_CURVE ( 'NONE', #44850, #45023, #28884, .T. ) ;
#41868 = EDGE_LOOP ( 'NONE', ( #15680, #29386, #54805, #49911 ) ) ;
#41869 = DIRECTION ( 'NONE',  ( 0.7071067811865975328, 0.7071067811864976127, -1.669585032811993884E-09 ) ) ;
#41870 = DIRECTION ( 'NONE',  ( 0.000000000000000000, -1.000000000000000000, 0.000000000000000000 ) ) ;
#41871 = ORIENTED_EDGE ( 'NONE', *, *, #2708, .T. ) ;
#41872 = CARTESIAN_POINT ( 'NONE',  ( 1.324344358081999795, -78.89373633638300021, 0.1571239973995999795 ) ) ;
#41873 = CARTESIAN_POINT ( 'NONE',  ( 8.923648882468999233, -79.87442432477398313, -7.337453855139000503 ) ) ;
#41874 = VERTEX_POINT ( 'NONE', #2281 ) ;
#41875 = CARTESIAN_POINT ( 'NONE',  ( -11.92228046151999976, -78.74294670917899452, 2.416973144693999931 ) ) ;
#41876 = CARTESIAN_POINT ( 'NONE',  ( -10.93752463681999920, -77.51070342825998694, -2.465225665228000018 ) ) ;
#41877 = CARTESIAN_POINT ( 'NONE',  ( 9.848022987154569918, -61.62869493570521939, -8.114799025198223603 ) ) ;
#41878 = ORIENTED_EDGE ( 'NONE', *, *, #19264, .T. ) ;
#41879 = EDGE_CURVE ( 'NONE', #11806, #9508, #15518, .T. ) ;
#41880 = ORIENTED_EDGE ( 'NONE', *, *, #29098, .F. ) ;
#41881 = CARTESIAN_POINT ( 'NONE',  ( 0.000000000000000000, -6.049999999381999949, 0.000000000000000000 ) ) ;
#41882 = SURFACE_STYLE_FILL_AREA ( #55168 ) ;
#41883 = CARTESIAN_POINT ( 'NONE',  ( -2.116314338179000387, -80.11792711497950847, -9.535298106756000536 ) ) ;
#41884 = VECTOR ( 'NONE', #25840, 1000.000000000000114 ) ;
#41885 = VERTEX_POINT ( 'NONE', #51000 ) ;
#41886 = CARTESIAN_POINT ( 'NONE',  ( 8.485281374238999419, -18.75000000000000000, -8.485281374238999419 ) ) ;
#41887 = CARTESIAN_POINT ( 'NONE',  ( 8.894916816479799593, -25.22809132934175835, -9.073484344813371294 ) ) ;
#41888 = ORIENTED_EDGE ( 'NONE', *, *, #53135, .F. ) ;
#41889 = CARTESIAN_POINT ( 'NONE',  ( 10.75000000000000000, -80.84999999999999432, -1.053639850055999980E-14 ) ) ;
#41890 = CARTESIAN_POINT ( 'NONE',  ( -9.204193785523999694, -77.02959415034598578, -2.332437886131999871 ) ) ;
#41891 = TOROIDAL_SURFACE ( 'NONE', #8892, 13.50000000000000000, 0.5000000000000000000 ) ;
#41892 = PLANE ( 'NONE',  #13823 ) ;
#41893 = CARTESIAN_POINT ( 'NONE',  ( 0.5999999999999999778, -5.000000000000000000, 0.5999999999999999778 ) ) ;
#41894 = CARTESIAN_POINT ( 'NONE',  ( -10.07979664880000037, -76.57175206120300004, 3.736335038366999761 ) ) ;
#41895 = EDGE_CURVE ( 'NONE', #32127, #4183, #10497, .T. ) ;
#41896 = CIRCLE ( 'NONE', #31541, 12.50000000000000000 ) ;
#41897 = CARTESIAN_POINT ( 'NONE',  ( 7.201514106410999538, -76.91319389792408856, -6.116891697219999813 ) ) ;
#41898 = CARTESIAN_POINT ( 'NONE',  ( 0.9708803083217455443, -78.16900954117737399, 1.156142391821560755 ) ) ;
#41899 = CARTESIAN_POINT ( 'NONE',  ( -1.733997378023031111, -23.52383216769542074, 12.54437956612010296 ) ) ;
#41900 = ORIENTED_EDGE ( 'NONE', *, *, #8799, .F. ) ;
#41901 = ADVANCED_FACE ( 'NONE', ( #27878, #5173 ), #18751, .T. ) ;
#41902 = CARTESIAN_POINT ( 'NONE',  ( 10.54796701376999835, -75.77576924646000123, 6.346365727669000201 ) ) ;
#41903 = CARTESIAN_POINT ( 'NONE',  ( -0.6744830649036911430, -82.24320892454605314, -1.051876958025935949 ) ) ;
#41904 = VECTOR ( 'NONE', #33055, 1000.000000000000114 ) ;
#41905 = CARTESIAN_POINT ( 'NONE',  ( 2.364202589570008950, -2.032802416630155484, -2.609243845418832031 ) ) ;
#41906 = CARTESIAN_POINT ( 'NONE',  ( 12.87024489160000051, -19.21538333566000034, 2.062597265787999845 ) ) ;
#41907 = CARTESIAN_POINT ( 'NONE',  ( -1.307210027570999911, -79.16850156920999382, -12.19386267984000050 ) ) ;
#41908 = CARTESIAN_POINT ( 'NONE',  ( 9.406806676749999596, -76.76054034281098382, -7.895227358184000899 ) ) ;
#41909 = CARTESIAN_POINT ( 'NONE',  ( -3.308356911591993743, -85.80681307385599155, 1.472975398279013692 ) ) ;
#41910 = CARTESIAN_POINT ( 'NONE',  ( 9.713032445803841952, -61.32293762623243083, -7.970418356083900591 ) ) ;
#41911 = CARTESIAN_POINT ( 'NONE',  ( -11.02814366974847893, -78.08318630897967694, -4.893295640579582439 ) ) ;
#41912 = CARTESIAN_POINT ( 'NONE',  ( -0.4146318973826840226, -79.37205812977910568, -11.20920117498000046 ) ) ;
#41913 = B_SPLINE_CURVE_WITH_KNOTS ( 'NONE', 3,
 ( #331, #27139, #54326, #36005, #22728, #49011, #3842, #13571, #49609, #53433, #26271, #13866, #22133, #9157, #17721, #40739, #18310, #31561, #36302, #35402, #18013, #3556, #49902, #39846, #57862, #31861, #53148, #9449, #54030, #26848, #44006, #39565, #44880, #57567, #44285, #17130, #48727, #8270, #21840, #17416, #12976, #30973, #36, #8558, #40142, #26549, #4431, #44578, #49307, #4134, #58154, #35707, #22431, #53736, #13272, #31264, #8857, #40445, #18604, #54893, #32151, #23886, #33320, #37175, #36881, #23314, #1478, #55188, #14729, #50190, #54614, #1190, #32438, #14443, #28015, #19180, #14152, #23018, #50483, #50777, #621, #24184, #36592, #10034, #9737, #51358, #27725, #5303, #5014, #1769, #45769, #19468, #46062, #41905, #42201, #41321, #6174, #904, #32728, #18888, #41030, #10322, #5583, #23595, #19762, #46647, #27436 ),
 .UNSPECIFIED., .F., .F.,
 ( 4, 2, 2, 2, 2, 2, 1, 2, 2, 2, 2, 2, 2, 2, 2, 2, 2, 2, 2, 2, 2, 2, 2, 2, 2, 2, 2, 1, 2, 2, 2, 2, 2, 2, 2, 2, 2, 2, 2, 2, 2, 2, 2, 2, 2, 2, 2, 2, 1, 2, 2, 2, 2, 2, 4 ),
 ( 0.000000000000000000, 0.01562500000000000694, 0.03125000000000001388, 0.04687500000000002082, 0.06250000000000002776, 0.07812500000000002776, 0.09375000000000004163, 0.1093750000000000555, 0.1250000000000000555, 0.1406250000000000555, 0.1562500000000000555, 0.1718750000000000555, 0.1875000000000000278, 0.2031250000000000000, 0.2187499999999999722, 0.2343749999999999722, 0.2499999999999999445, 0.2656249999999999445, 0.2812499999999999445, 0.2968749999999999445, 0.3124999999999999445, 0.3281250000000000000, 0.3437500000000000000, 0.3750000000000000000, 0.4062499999999999445, 0.4374999999999998890, 0.4687499999999998890, 0.4999999999999998335, 0.5312499999999997780, 0.5624999999999997780, 0.5937499999999997780, 0.6249999999999997780, 0.6562499999999998890, 0.6718749999999998890, 0.6874999999999998890, 0.7031249999999998890, 0.7187499999999998890, 0.7343749999999998890, 0.7499999999999998890, 0.7656249999999998890, 0.7812499999999998890, 0.7968749999999998890, 0.8124999999999998890, 0.8281249999999998890, 0.8437499999999998890, 0.8593749999999998890, 0.8749999999999998890, 0.8906250000000000000, 0.9062500000000000000, 0.9218750000000000000, 0.9375000000000000000, 0.9531250000000000000, 0.9687500000000000000, 0.9843750000000000000, 1.000000000000000000 ),
 .UNSPECIFIED. ) ;
#41914 = ADVANCED_FACE ( 'NONE', ( #5459 ), #3186, .T. ) ;
#41915 = ORIENTED_EDGE ( 'NONE', *, *, #11253, .F. ) ;
#41916 = CARTESIAN_POINT ( 'NONE',  ( -1.259088972310000054, -82.99040930645999481, 0.4905773767712000577 ) ) ;
#41917 = CARTESIAN_POINT ( 'NONE',  ( -10.26699006316252749, -77.84166666666666856, -5.917523019358070790 ) ) ;
#41918 = CARTESIAN_POINT ( 'NONE',  ( 10.36597333712761326, -23.77522429014145544, 7.635925938716360051 ) ) ;
#41919 = CARTESIAN_POINT ( 'NONE',  ( 1.217465845835393967, -82.77083333333332860, 0.3271848554491025851 ) ) ;
#41920 = CARTESIAN_POINT ( 'NONE',  ( -3.483093260015999615, -1.774671397434999909, 0.8806644628490999382 ) ) ;
#41921 = CARTESIAN_POINT ( 'NONE',  ( 6.958153983328000614, -78.68285191714500115, -9.837675768602998971 ) ) ;
#41922 = CARTESIAN_POINT ( 'NONE',  ( 2.268344470944000157, -78.91451892421298453, -9.471763527590001175 ) ) ;
#41924 = DIRECTION ( 'NONE',  ( -1.000000000000000000, 0.000000000000000000, 0.000000000000000000 ) ) ;
#41923 = CARTESIAN_POINT ( 'NONE',  ( -6.982274206190579591, -76.12553274448890761, 9.454767744417145181 ) ) ;
#41925 = CARTESIAN_POINT ( 'NONE',  ( 7.624341766639000539, -23.26485146254000114, 10.42531125024000005 ) ) ;
#41926 = CARTESIAN_POINT ( 'NONE',  ( -2.409209601448396576, -85.88547957940600952, 3.252055376540686105 ) ) ;
#41927 = ORIENTED_EDGE ( 'NONE', *, *, #8622, .T. ) ;
#41928 = DIRECTION ( 'NONE',  ( -0.3090169943750105674, 0.000000000000000000, 0.9510565162951329921 ) ) ;
#41929 = CONICAL_SURFACE ( 'NONE', #55110, 11.80312499993000053, 0.7853981633972997312 ) ;
#41930 = CARTESIAN_POINT ( 'NONE',  ( -2.038544480927606983, -78.70000000000000284, -3.380937442862391951 ) ) ;
#41931 = CYLINDRICAL_SURFACE ( 'NONE', #41010, 1.500000000000000000 ) ;
#41932 = CARTESIAN_POINT ( 'NONE',  ( 1.684372618195999927, -78.35319357579599853, 10.84559388857000073 ) ) ;
#41933 = CIRCLE ( 'NONE', #25936, 30.50000000000000355 ) ;
#41934 = DIRECTION ( 'NONE',  ( 1.000000000000000000, 0.000000000000000000, 0.000000000000000000 ) ) ;
#41935 = CARTESIAN_POINT ( 'NONE',  ( 7.743925494623000283, -79.84195935437298886, -5.791931050047999463 ) ) ;
#41936 = CARTESIAN_POINT ( 'NONE',  ( 7.753900686131000697, -17.71068035545000185, -10.31980286348999876 ) ) ;
#41937 = CARTESIAN_POINT ( 'NONE',  ( 12.99510751537000353, -52.49705297113997204, -6.911973076623003642 ) ) ;
#41938 = VERTEX_POINT ( 'NONE', #23461 ) ;
#41939 = CARTESIAN_POINT ( 'NONE',  ( 12.71466563516855786, -17.86210710705555726, 1.778810201872595975 ) ) ;
#41940 = CARTESIAN_POINT ( 'NONE',  ( 10.74999999999999645, -79.76041666666667140, 1.407171709420451666 ) ) ;
#41941 = CARTESIAN_POINT ( 'NONE',  ( -0.4635254915625000027, -82.00000000000000000, -1.426584774443000025 ) ) ;
#41942 = CARTESIAN_POINT ( 'NONE',  ( 10.79453853465248159, -77.66598170563767667, -5.411409766425476775 ) ) ;
#41944 = CARTESIAN_POINT ( 'NONE',  ( 1.068867549261173000, -81.39395485511519723, 0.6488671464486228668 ) ) ;
#41943 = CARTESIAN_POINT ( 'NONE',  ( -1.166489638287000030, -82.11937728024399519, 0.6163185517979000716 ) ) ;
#41945 = CARTESIAN_POINT ( 'NONE',  ( 11.21680614116372610, -78.60040301369775761, 0.06974094738193595266 ) ) ;
#41946 = CARTESIAN_POINT ( 'NONE',  ( -9.185997767857138285, -77.00000000000001421, 1.529051226933332952 ) ) ;
#41947 = CARTESIAN_POINT ( 'NONE',  ( 3.521688171515000132, -3.513922206379000102, 0.7298424208991000084 ) ) ;
#41948 = ADVANCED_FACE ( 'NONE', ( #58318 ), #1058, .T. ) ;
#41949 = AXIS2_PLACEMENT_3D ( 'NONE', #50808, #10352, #47259 ) ;
#41950 = CARTESIAN_POINT ( 'NONE',  ( -11.00000000000000000, -79.59999999999999432, 0.000000000000000000 ) ) ;
#41951 = CARTESIAN_POINT ( 'NONE',  ( -9.813348458551734765, -78.98705748317810560, -4.915893702512511787 ) ) ;
#41952 = CARTESIAN_POINT ( 'NONE',  ( -6.043427764450832740, -77.21666666666666856, 10.48543666025107512 ) ) ;
#41953 = ORIENTED_EDGE ( 'NONE', *, *, #45034, .T. ) ;
#41954 = ORIENTED_EDGE ( 'NONE', *, *, #51653, .F. ) ;
#41955 = CARTESIAN_POINT ( 'NONE',  ( 6.055527902613000002, -77.71999999999999886, 7.319875806370000682 ) ) ;
#41956 = CARTESIAN_POINT ( 'NONE',  ( 7.609106138680006737, -78.78758249396523183, -7.593667575104682932 ) ) ;
#41957 = ORIENTED_EDGE ( 'NONE', *, *, #30115, .F. ) ;
#41958 = FACE_OUTER_BOUND ( 'NONE', #42736, .T. ) ;
#41959 = CARTESIAN_POINT ( 'NONE',  ( -9.486322910027237043, -79.39542840225620068, 0.5339199459016039651 ) ) ;
#41960 = CARTESIAN_POINT ( 'NONE',  ( 8.790688707576000738, -61.73813493216999859, 8.797962936864001549 ) ) ;
#41961 = CARTESIAN_POINT ( 'NONE',  ( -1.035649530420586162, -76.66761614046610873, -12.15563870979175576 ) ) ;
#41962 = CARTESIAN_POINT ( 'NONE',  ( -0.08519494393186054226, -78.42546946423334475, 11.97968001115087056 ) ) ;
#41963 = CARTESIAN_POINT ( 'NONE',  ( 8.822637088635000069, -80.13686059729418787, 6.926713255916000733 ) ) ;
#41964 = ORIENTED_EDGE ( 'NONE', *, *, #23172, .T. ) ;
#41965 = CARTESIAN_POINT ( 'NONE',  ( -10.18248259416120938, -24.29095036201641022, 7.792398156871034764 ) ) ;
#41966 = EDGE_LOOP ( 'NONE', ( #37711, #30741, #45969 ) ) ;
#41967 = EDGE_CURVE ( 'NONE', #21583, #18023, #18964, .T. ) ;
#41968 = CARTESIAN_POINT ( 'NONE',  ( 8.792064078896341783, -77.37518554897279444, 2.874290267169839819 ) ) ;
#41969 = LINE ( 'NONE', #2408, #2758 ) ;
#41970 = AXIS2_PLACEMENT_3D ( 'NONE', #44359, #8345, #26341 ) ;
#41971 = CARTESIAN_POINT ( 'NONE',  ( 2.500000000000000000, -80.69999999999998863, 0.000000000000000000 ) ) ;
#41972 = CARTESIAN_POINT ( 'NONE',  ( 1.449215700157000075, -78.20560097396669619, -0.7120307440141999678 ) ) ;
#41973 = AXIS2_PLACEMENT_3D ( 'NONE', #45570, #5117, #41924 ) ;
#41974 = CARTESIAN_POINT ( 'NONE',  ( 10.75000000000000000, -80.75000000000000000, 3.489821576044999869E-14 ) ) ;
#41975 = CARTESIAN_POINT ( 'NONE',  ( -3.140974612311352221, -78.50416666666664867, -11.68767212001979061 ) ) ;
#41976 = CARTESIAN_POINT ( 'NONE',  ( -0.6794254437148999903, -78.86112079180999501, -1.478865823597000029 ) ) ;
#41977 = CARTESIAN_POINT ( 'NONE',  ( 1.959975192012000100, -79.72707046129099240, 3.683075126482999728 ) ) ;
#41978 = FACE_OUTER_BOUND ( 'NONE', #40492, .T. ) ;
#41979 = DIRECTION ( 'NONE',  ( 0.000000000000000000, 0.000000000000000000, -1.000000000000000000 ) ) ;
#41980 = CARTESIAN_POINT ( 'NONE',  ( 12.74366183109916939, -60.32185227198593935, 1.980611001123821158 ) ) ;
#41981 = CARTESIAN_POINT ( 'NONE',  ( -4.100000000000000533, -78.69999999999998863, 0.000000000000000000 ) ) ;
#41982 = EDGE_CURVE ( 'NONE', #52202, #4102, #22593, .T. ) ;
#41983 = CARTESIAN_POINT ( 'NONE',  ( -3.515158122207999725, -83.18657311260999165, 0.4777273718585999807 ) ) ;
#41984 = ORIENTED_EDGE ( 'NONE', *, *, #30468, .F. ) ;
#41985 = CARTESIAN_POINT ( 'NONE',  ( -9.596002108778160178, -79.45208333333332007, -7.374560639698984232 ) ) ;
#41986 = CARTESIAN_POINT ( 'NONE',  ( -1.425428639595999858, -80.85725624887999174, 0.6946581327067000711 ) ) ;
#41987 = CARTESIAN_POINT ( 'NONE',  ( -2.105778458517339580, -77.99082079685921087, 10.54164563490564177 ) ) ;
#41988 = EDGE_CURVE ( 'NONE', #33230, #48634, #26672, .T. ) ;
#41989 = CARTESIAN_POINT ( 'NONE',  ( 2.697636866285999968, -77.77696867547399506, -11.67213861177999945 ) ) ;
#41990 = CARTESIAN_POINT ( 'NONE',  ( -9.723199427802001082, -54.32306055813000256, 7.958735710007999842 ) ) ;
#41991 = CARTESIAN_POINT ( 'NONE',  ( -1.250185882460489672, -77.76609322504926070, -0.2498302737146554653 ) ) ;
#41992 = CARTESIAN_POINT ( 'NONE',  ( 3.209891797385462375, -2.966244217981962805, -1.450742976519075800 ) ) ;
#41993 = CARTESIAN_POINT ( 'NONE',  ( 10.49291542331330085, -80.86792101652982012, 2.341975711254098425 ) ) ;
#41994 = CARTESIAN_POINT ( 'NONE',  ( 4.000000000000000000, -5.200000000000000178, -0.5999999999999999778 ) ) ;
#41995 = CARTESIAN_POINT ( 'NONE',  ( -6.908074975177627586, -86.09999999999999432, -5.681417088837195983 ) ) ;
#41996 = CARTESIAN_POINT ( 'NONE',  ( -5.762797186001000327, -77.87760228854999411, 9.407013499219999630 ) ) ;
#41997 = CARTESIAN_POINT ( 'NONE',  ( -3.699256142337000064, -77.04934472805763335, 11.71059914860999918 ) ) ;
#41998 = CARTESIAN_POINT ( 'NONE',  ( -3.250000000000000000, -2.100000000000000089, 0.000000000000000000 ) ) ;
#41999 = ORIENTED_EDGE ( 'NONE', *, *, #11708, .F. ) ;
#42000 = FACE_OUTER_BOUND ( 'NONE', #32132, .T. ) ;
#42001 = CARTESIAN_POINT ( 'NONE',  ( 1.466594960155999994, -60.88158199018999994, -12.44238958335999889 ) ) ;
#42002 = CARTESIAN_POINT ( 'NONE',  ( 8.547245099307286154, -80.40224407770602966, 6.556889745432177286 ) ) ;
#42003 = CARTESIAN_POINT ( 'NONE',  ( 9.668944085725000193, -77.05840859066300652, 5.685915129398999568 ) ) ;
#42004 = CARTESIAN_POINT ( 'NONE',  ( 1.684372618195999927, -78.23258772445399245, 10.84559388857000073 ) ) ;
#42005 = CARTESIAN_POINT ( 'NONE',  ( 7.658900562714999971, -23.20940503079999928, -10.01676248781999945 ) ) ;
#42006 = CARTESIAN_POINT ( 'NONE',  ( -1.945056384218381451, -85.94583335130319313, 3.510275759367116777 ) ) ;
#42007 = CARTESIAN_POINT ( 'NONE',  ( 8.485281374238999419, -59.94999999967000548, -8.485281374238999419 ) ) ;
#42008 = DIRECTION ( 'NONE',  ( -6.203993618971000339E-09, -1.000000000000000000, -6.182589629265999685E-10 ) ) ;
#42009 = B_SPLINE_SURFACE_WITH_KNOTS ( 'NONE', 3, 3, ( 
 ( #58258, #39086, #39379, #57665 ),
 ( #49412, #57092, #25507, #3650 ),
 ( #44101, #25795, #43524, #3085 ),
 ( #53241, #7794, #52670, #17222 ),
 ( #30506, #21653, #16659, #8080 ),
 ( #35211, #48822, #12223, #26361 ),
 ( #3369, #8660, #12790, #30213 ),
 ( #44381, #16945, #26646, #44682 ) ),
 .UNSPECIFIED., .F., .F., .F.,
 ( 4, 1, 1, 1, 1, 4 ),
 ( 4, 4 ),
 ( -0.01200407345745999922, 0.000000000000000000, 0.3333333333333000081, 0.6666666666667000474, 1.000000000000000000, 1.011997855551999947 ),
 ( -0.3559705542741000150, 1.355970554273999928 ),
 .UNSPECIFIED. ) ;
#42010 = CARTESIAN_POINT ( 'NONE',  ( -0.7861470525832999767, -84.35769503318799423, 4.097808574246000646 ) ) ;
#42011 = EDGE_CURVE ( 'NONE', #1755, #9471, #9604, .T. ) ;
#42012 = CARTESIAN_POINT ( 'NONE',  ( -1.199500263597270022, -79.55208333333332860, -0.9218200799623730290 ) ) ;
#42013 = CARTESIAN_POINT ( 'NONE',  ( 7.660411364605000273, -55.60826384781999820, -10.01752038681999935 ) ) ;
#42014 = AXIS2_PLACEMENT_3D ( 'NONE', #39507, #44230, #22072 ) ;
#42015 = DIRECTION ( 'NONE',  ( 1.000000000000000000, 0.000000000000000000, 0.000000000000000000 ) ) ;
#42016 = CARTESIAN_POINT ( 'NONE',  ( -0.7048934085577001074, -80.97905750928998714, -1.509431780672999990 ) ) ;
#42017 = CARTESIAN_POINT ( 'NONE',  ( -1.314590664899999872, -77.98943747231999168, -0.5743650807226000632 ) ) ;
#42018 = CARTESIAN_POINT ( 'NONE',  ( -10.48543666025111420, -77.75833333333331154, 6.043427764450754580 ) ) ;
#42019 = CARTESIAN_POINT ( 'NONE',  ( 0.000000000000000000, -78.69999999999998863, 0.000000000000000000 ) ) ;
#42020 = CARTESIAN_POINT ( 'NONE',  ( -9.199999999999999289, -79.79999999999999716, 0.000000000000000000 ) ) ;
#42021 = VERTEX_POINT ( 'NONE', #38494 ) ;
#42022 = CARTESIAN_POINT ( 'NONE',  ( 9.500000000000000000, -78.04999999999999716, 0.000000000000000000 ) ) ;
#42023 = EDGE_CURVE ( 'NONE', #22487, #36041, #50659, .T. ) ;
#42024 = CARTESIAN_POINT ( 'NONE',  ( -10.36597025940859673, -55.02476146821044978, 7.635927901479407254 ) ) ;
#42025 = EDGE_LOOP ( 'NONE', ( #17769, #6019, #45424, #17984, #37008 ) ) ;
#42026 = ADVANCED_FACE ( 'NONE', ( #33476 ), #36172, .F. ) ;
#42027 = CARTESIAN_POINT ( 'NONE',  ( -0.4710266599135919940, -81.69439008557912985, -1.157763597771598540 ) ) ;
#42028 = CARTESIAN_POINT ( 'NONE',  ( 5.887377288745000214, -80.28906619586439319, 9.329533489291000237 ) ) ;
#42029 = DIRECTION ( 'NONE',  ( -0.7071067811865474617, 0.7071067811865474617, 7.319413740254484567E-10 ) ) ;
#42030 = VERTEX_POINT ( 'NONE', #19621 ) ;
#42031 = ORIENTED_EDGE ( 'NONE', *, *, #31416, .T. ) ;
#42032 = CARTESIAN_POINT ( 'NONE',  ( -1.393296160724000199, -81.61749198208599410, -0.2622693059933000059 ) ) ;
#42033 = ORIENTED_EDGE ( 'NONE', *, *, #22014, .T. ) ;
#42034 = EDGE_LOOP ( 'NONE', ( #39026, #39251, #16288, #27629 ) ) ;
#42035 = CARTESIAN_POINT ( 'NONE',  ( -1.199500263597274685, -81.94791666667777008, 0.9218200799623673669 ) ) ;
#42036 = CARTESIAN_POINT ( 'NONE',  ( -10.11462645678665417, -55.41287635801736400, -7.639895286212103009 ) ) ;
#42037 = DIRECTION ( 'NONE',  ( 0.000000000000000000, 0.000000000000000000, 1.000000000000000000 ) ) ;
#42038 = CARTESIAN_POINT ( 'NONE',  ( 0.6616675926900500437, -79.77916665965761922, 3.378914762188844900 ) ) ;
#42039 = CARTESIAN_POINT ( 'NONE',  ( 4.634228027295999475, -78.15741001420200007, 8.886345528036001085 ) ) ;
#42040 = CARTESIAN_POINT ( 'NONE',  ( 7.019650986448177754, -78.29361464504475521, -6.023984796694146659 ) ) ;
#42041 = DIRECTION ( 'NONE',  ( -0.7071067811864970576, 3.544461081833985722E-08, 0.7071067811865970887 ) ) ;
#42042 = ORIENTED_EDGE ( 'NONE', *, *, #31484, .F. ) ;
#42043 = ORIENTED_EDGE ( 'NONE', *, *, #47769, .T. ) ;
#42044 = DIRECTION ( 'NONE',  ( 1.000000000000000000, 0.000000000000000000, 0.000000000000000000 ) ) ;
#42045 = CARTESIAN_POINT ( 'NONE',  ( -12.71466317164989590, -24.13795986741163802, 1.778778223973440209 ) ) ;
#42046 = CARTESIAN_POINT ( 'NONE',  ( -0.7554284705563544255, -79.41666666666667140, 1.310679582531384169 ) ) ;
#42047 = CARTESIAN_POINT ( 'NONE',  ( 10.99999999987063326, -76.04999999999999716, -1.151917307345635244 ) ) ;
#42048 = CARTESIAN_POINT ( 'NONE',  ( 3.248345031021000029, -78.11768663459099571, 9.144340540792999406 ) ) ;
#42049 = B_SPLINE_CURVE_WITH_KNOTS ( 'NONE', 3,
 ( #46549, #6075, #55970, #1668, #19658, #15225, #37948, #15521, #26102, #11967, #29658, #48281, #35234, #38820, #16107, #6950 ),
 .UNSPECIFIED., .F., .F.,
 ( 4, 2, 2, 2, 2, 2, 2, 4 ),
 ( 0.000000000000000000, 0.1785697310289149631, 0.2678545965433721809, 0.3571394620578294266, 0.4464243275722866722, 0.5357091930867439178, 0.6249940586012011634, 0.7142789241156584090 ),
 .UNSPECIFIED. ) ;
#42050 = CARTESIAN_POINT ( 'NONE',  ( 0.000000000000000000, -0.7781249991808000255, 0.000000000000000000 ) ) ;
#42051 = CARTESIAN_POINT ( 'NONE',  ( 3.513334747297280902, -85.82276510432375005, 1.485566327356647731 ) ) ;
#42052 = CARTESIAN_POINT ( 'NONE',  ( 3.370554742410902804, -77.44759005475501112, -11.56126178251549064 ) ) ;
#42053 = B_SPLINE_SURFACE_WITH_KNOTS ( 'NONE', 3, 3, ( 
 ( #26224, #58104, #36258, #30926, #40694, #13816, #54280, #22078, #21793, #22977, #12929, #40986, #36550, #49857, #13223, #578, #3792, #45426, #54571, #44239, #18557, #9106, #27392, #22682, #14111, #39798, #40089, #40394, #32108, #8507, #50149, #4683, #13522, #49562, #27095 ),
 ( #17667, #286, #53982, #31514, #26501, #44525, #58403, #31217, #53684, #26799, #31816, #17966, #4080, #57811, #45132, #17370, #18264, #35357, #35654, #9401, #49255, #8807, #4967, #44828, #4382, #22383, #35957, #14684, #28256, #2018, #20016, #5833, #37999, #55437, #41858 ),
 ( #56025, #5540, #6421, #24136, #46310, #55735, #37713, #10872, #23550, #19132, #32684, #15573, #46602, #14979, #27681, #28843, #15279, #23840, #32977, #33568, #33272, #14396, #51313, #46893, #51023, #9691, #1435, #24435, #5261, #42450, #54849, #45726, #23268, #41275, #55138 ),
 ( #860, #18844, #36837, #32394, #10572, #50438, #6129, #9990, #27968, #41564, #19426, #46019, #1145, #37127, #42154, #28554, #1724, #19716, #50735, #37417, #10275, #2301, #52747, #43603, #39160, #38871, #43313, #34429, #47758, #7869, #20587, #51606, #56314, #57167, #3442 ) ),
 .UNSPECIFIED., .F., .F., .F.,
 ( 4, 4 ),
 ( 4, 1, 1, 1, 1, 1, 1, 1, 1, 1, 1, 1, 1, 1, 1, 1, 1, 1, 1, 1, 1, 1, 1, 1, 1, 1, 1, 1, 1, 1, 1, 1, 4 ),
 ( -0.1772706441294000235, 1.177270644128999955 ),
 ( 0.3451371257638000123, 0.3660028545997999760, 0.3868685834356999642, 0.4077343122716999835, 0.4286000411075999716, 0.4494657699435999909, 0.4703314987795000346, 0.4911972276154999983, 0.5120629564514999066, 0.5329286852874000058, 0.5537944141233999140, 0.5746601429593000132, 0.5955258717953000325, 0.6163916006312000206, 0.6372573294671999289, 0.6581230583032000592, 0.6789887871390999363, 0.6998545159750999556, 0.7207202448110000548, 0.7415859736469999630, 0.7624517024829000622, 0.7833174313188999704, 0.8041831601548999897, 0.8250488889907999779, 0.8459146178267999971, 0.8667803466626999853, 0.8876460754987000046, 0.9085118043345999927, 0.9293775331706000120, 0.9502432620066000313, 0.9711089908424999084, 0.9919747196785000387, 1.012840448513999903 ),
 .UNSPECIFIED. ) ;
#42054 = CARTESIAN_POINT ( 'NONE',  ( -0.7285569484545000307, -79.65971054856998990, -1.138057995564000002 ) ) ;
#42055 = PRESENTATION_LAYER_ASSIGNMENT (  '', '', ( #24135 ) ) ;
#42056 = CARTESIAN_POINT ( 'NONE',  ( -7.483407197968000801, -77.00000000000000000, 5.437013583706000297 ) ) ;
#42057 = CARTESIAN_POINT ( 'NONE',  ( 1.621761508983999844, -80.72674124465299883, -3.847011800229999778 ) ) ;
#42058 = CARTESIAN_POINT ( 'NONE',  ( 0.7142021645403204833, -79.58595579008107279, 1.332894191355008529 ) ) ;
#42059 = B_SPLINE_CURVE_WITH_KNOTS ( 'NONE', 3,
 ( #48978, #25947, #21233, #56964, #53394, #16527, #30365, #43688, #8520, #26514, #34800, #34506, #25657, #8233, #3242 ),
 .UNSPECIFIED., .F., .F.,
 ( 4, 1, 1, 1, 1, 1, 1, 1, 1, 1, 1, 1, 4 ),
 ( 0.000000000000000000, 0.08333611588665000569, 0.1666676715620999949, 0.2500039875833999781, 0.3333306964953999807, 0.4166666792817999565, 0.4999999999924999994, 0.5833333197091999933, 0.6666692694150000431, 0.7499959719902999922, 0.8333323089881000678, 0.9166638425153998959, 1.000000000000000000 ),
 .UNSPECIFIED. ) ;
#42061 = EDGE_CURVE ( 'NONE', #29374, #58355, #40813, .T. ) ;
#42060 = CARTESIAN_POINT ( 'NONE',  ( -8.963686800021001488, -79.03971001420200082, 3.673354096997999640 ) ) ;
#42062 = CARTESIAN_POINT ( 'NONE',  ( -1.750000000001000089, -22.75077028492999887, -12.60356226393999890 ) ) ;
#42063 = CARTESIAN_POINT ( 'NONE',  ( -7.636247231030999671, -18.23676232879999759, -10.30460520062000107 ) ) ;
#42064 = VECTOR ( 'NONE', #35056, 1000.000000000000000 ) ;
#42066 = CARTESIAN_POINT ( 'NONE',  ( 1.886823409076000102, -18.23680315638000238, -12.68610076205999881 ) ) ;
#42065 = CYLINDRICAL_SURFACE ( 'NONE', #42919, 3.250000000000000000 ) ;
#42067 = DIRECTION ( 'NONE',  ( 0.000000000000000000, -1.000000000000000000, 0.000000000000000000 ) ) ;
#42068 = DIRECTION ( 'NONE',  ( -0.9999999924279685537, 0.000000000000000000, -0.0001230612157848962919 ) ) ;
#42069 = CARTESIAN_POINT ( 'NONE',  ( -9.495603837127998048, -78.36858404876599593, -6.055366803880999349 ) ) ;
#42070 = CONICAL_SURFACE ( 'NONE', #18507, 11.96250000010999948, 0.7853981633972997312 ) ;
#42071 = CARTESIAN_POINT ( 'NONE',  ( 5.812955055244049873, -77.19999999999998863, -9.242863774950786038 ) ) ;
#42072 = ORIENTED_EDGE ( 'NONE', *, *, #16481, .T. ) ;
#42073 = CARTESIAN_POINT ( 'NONE',  ( 9.502896619541301604, -61.54094210160239697, 8.179425867541981532 ) ) ;
#42074 = DIRECTION ( 'NONE',  ( 0.000000000000000000, -1.000000000000000000, 0.000000000000000000 ) ) ;
#42075 = DIRECTION ( 'NONE',  ( 0.7071067811865475727, 0.000000000000000000, -0.7071067811865475727 ) ) ;
#42076 = CARTESIAN_POINT ( 'NONE',  ( 1.167836049095117623, -78.37932260450160982, 0.4458657978228700025 ) ) ;
#42077 = CARTESIAN_POINT ( 'NONE',  ( -6.811155457859999984, -79.33047884747199419, 6.825426861229999531 ) ) ;
#42078 = CARTESIAN_POINT ( 'NONE',  ( -9.234979314279001983, -77.01021089112001050, -9.168119495123999485 ) ) ;
#42079 = CARTESIAN_POINT ( 'NONE',  ( 7.593872865574214259, -79.41257358862213778, 7.608910733373231317 ) ) ;
#42080 = EDGE_CURVE ( 'NONE', #31055, #38125, #51396, .T. ) ;
#42081 = CARTESIAN_POINT ( 'NONE',  ( -11.05000000000000071, -82.00000000000000000, 0.000000000000000000 ) ) ;
#42082 = FACE_OUTER_BOUND ( 'NONE', #6605, .T. ) ;
#42083 = EDGE_CURVE ( 'NONE', #28871, #52300, #2761, .T. ) ;
#42084 = CARTESIAN_POINT ( 'NONE',  ( -10.25580049915999936, -77.27540488493299620, -4.414041361589999823 ) ) ;
#42085 = CARTESIAN_POINT ( 'NONE',  ( 0.08339889454722999862, -81.72327760821899290, 1.503976585945999922 ) ) ;
#42086 = CARTESIAN_POINT ( 'NONE',  ( 2.013632425233999879, -78.29159514476064885, -9.512575055159999238 ) ) ;
#42087 = CARTESIAN_POINT ( 'NONE',  ( 8.857396897828001769, -77.74332746776399006, -3.187116989308000026 ) ) ;
#42089 = DIRECTION ( 'NONE',  ( 0.000000000000000000, 0.000000000000000000, 1.000000000000000000 ) ) ;
#42088 = CARTESIAN_POINT ( 'NONE',  ( -1.560211831905000013, -82.62253637535398809, 3.417178226333000168 ) ) ;
#42090 = CARTESIAN_POINT ( 'NONE',  ( 8.395992668097999712, -79.35954805011499502, 4.560928606276999808 ) ) ;
#42091 = CARTESIAN_POINT ( 'NONE',  ( -3.493489587975783461, -0.7565104147135170987, -0.4581487814226765654 ) ) ;
#42092 = CARTESIAN_POINT ( 'NONE',  ( 10.66047430956388098, -80.33875064089707507, -1.546821364917390085 ) ) ;
#42093 = DIRECTION ( 'NONE',  ( 0.000000000000000000, -1.000000000000000000, 0.000000000000000000 ) ) ;
#42094 = DIRECTION ( 'NONE',  ( 0.000000000000000000, 1.000000000000000000, 0.000000000000000000 ) ) ;
#42096 = EDGE_CURVE ( 'NONE', #50093, #37236, #17324, .T. ) ;
#42095 = VERTEX_POINT ( 'NONE', #48806 ) ;
#42097 = CARTESIAN_POINT ( 'NONE',  ( 10.52307592342000042, -79.49193466302899935, 5.828552047478999576 ) ) ;
#42098 = DIRECTION ( 'NONE',  ( 0.000000000000000000, 0.000000000000000000, -1.000000000000000000 ) ) ;
#42099 = DIRECTION ( 'NONE',  ( -0.5000000000000744960, -0.7071067811864422126, -0.5000000000000744960 ) ) ;
#42100 = VERTEX_POINT ( 'NONE', #26349 ) ;
#42101 = APPLICATION_CONTEXT ( 'automotive_design' ) ;
#42102 = CARTESIAN_POINT ( 'NONE',  ( 11.16572056546000091, -77.90213037933499152, 4.214520933710000250 ) ) ;
#42103 = ORIENTED_EDGE ( 'NONE', *, *, #21807, .T. ) ;
#42104 = ORIENTED_EDGE ( 'NONE', *, *, #3583, .T. ) ;
#42105 = ADVANCED_FACE ( 'NONE', ( #21066 ), #21640, .F. ) ;
#42107 = ORIENTED_EDGE ( 'NONE', *, *, #44295, .F. ) ;
#42106 = CONICAL_SURFACE ( 'NONE', #55293, 3.899999999992999733, 0.7853981633972997312 ) ;
#42108 = CONICAL_SURFACE ( 'NONE', #49653, 12.84999999995999964, 0.7853981633972997312 ) ;
#42109 = CARTESIAN_POINT ( 'NONE',  ( -0.9788390260998998116, -81.37919147407698972, 3.409317240057000209 ) ) ;
#42110 = DIRECTION ( 'NONE',  ( 0.000000000000000000, 1.000000000000000000, 0.000000000000000000 ) ) ;
#42111 = EDGE_CURVE ( 'NONE', #43554, #27720, #57080, .T. ) ;
#42112 = VERTEX_POINT ( 'NONE', #8351 ) ;
#42113 = CYLINDRICAL_SURFACE ( 'NONE', #32762, 12.50000000000000000 ) ;
#42114 = AXIS2_PLACEMENT_3D ( 'NONE', #13065, #22815, #26637 ) ;
#42115 = LINE ( 'NONE', #42697, #30610 ) ;
#42116 = VERTEX_POINT ( 'NONE', #7201 ) ;
#42117 = CARTESIAN_POINT ( 'NONE',  ( 0.000000000000000000, -75.00000000000000000, 0.000000000000000000 ) ) ;
#42118 = CARTESIAN_POINT ( 'NONE',  ( -1.505451346423154257, -79.24564413794375639, 0.08303611744945066375 ) ) ;
#42119 = AXIS2_PLACEMENT_3D ( 'NONE', #21752, #35912, #53344 ) ;
#42120 = CARTESIAN_POINT ( 'NONE',  ( 2.796280611080251166, -79.79999999999998295, -11.45656887133994672 ) ) ;
#42121 = CARTESIAN_POINT ( 'NONE',  ( -10.61761725430558378, -80.08783922550021828, 1.680617290028606270 ) ) ;
#42122 = CARTESIAN_POINT ( 'NONE',  ( 4.750170009413166916, -78.60686206216392691, -11.30680443602648211 ) ) ;
#42123 = CARTESIAN_POINT ( 'NONE',  ( 9.508122381440976767, -78.99355328149458444, -0.7695418330583383426 ) ) ;
#42124 = CARTESIAN_POINT ( 'NONE',  ( 1.546553306619000256, -76.33435708466599579, -11.07619323537999989 ) ) ;
#42125 = DIRECTION ( 'NONE',  ( -1.000000000000000000, 0.000000000000000000, 0.000000000000000000 ) ) ;
#42126 = CARTESIAN_POINT ( 'NONE',  ( 10.06614130400000029, -76.60994096989499269, 4.975593240213999735 ) ) ;
#42127 = CARTESIAN_POINT ( 'NONE',  ( -3.422957706972816094, -78.69494727339422013, -8.593410763649252715 ) ) ;
#42128 = CARTESIAN_POINT ( 'NONE',  ( 6.942576159420212889, -76.52437370351259460, 9.480114445733105910 ) ) ;
#42129 = CARTESIAN_POINT ( 'NONE',  ( -0.4764073897330970420, -23.51691643869884629, -10.98970030908002649 ) ) ;
#42130 = DIRECTION ( 'NONE',  ( 0.000000000000000000, 0.000000000000000000, -1.000000000000000000 ) ) ;
#42132 = ADVANCED_FACE ( 'NONE', ( #34049 ), #6217, .F. ) ;
#42131 = CARTESIAN_POINT ( 'NONE',  ( -5.563890944358950819, -80.18291473777019007, -9.489086410625162671 ) ) ;
#42133 = CARTESIAN_POINT ( 'NONE',  ( -3.013316066571108287, -3.070796228357301150, 1.215459137038311654 ) ) ;
#42134 = CARTESIAN_POINT ( 'NONE',  ( 3.746130956990000094, -79.16303455456849747, 0.2790430962004000204 ) ) ;
#42135 = CARTESIAN_POINT ( 'NONE',  ( -10.54622262059968918, -78.08456485334055230, 2.082890139455574552 ) ) ;
#42136 = CARTESIAN_POINT ( 'NONE',  ( 0.2018703831548298022, -82.96236683731123662, 1.233436793893810890 ) ) ;
#42137 = CARTESIAN_POINT ( 'NONE',  ( -3.407095545933000569, -78.77851879815550262, -1.429604595782733033E-14 ) ) ;
#42138 = CARTESIAN_POINT ( 'NONE',  ( 1.092232985442820992, -80.29166666666665719, 0.6295237254636267821 ) ) ;
#42139 = CARTESIAN_POINT ( 'NONE',  ( 7.374560639698954922, -79.22291666666669130, 9.596002108778179718 ) ) ;
#42140 = LINE ( 'NONE', #51008, #27196 ) ;
#42141 = CARTESIAN_POINT ( 'NONE',  ( 2.932093990090213875, -3.499999999999999556, 1.781698043337538451 ) ) ;
#42142 = CARTESIAN_POINT ( 'NONE',  ( -0.3926218265389190276, -77.60416666666667140, -1.460959015002473826 ) ) ;
#42143 = FACE_OUTER_BOUND ( 'NONE', #32499, .T. ) ;
#42144 = CARTESIAN_POINT ( 'NONE',  ( -9.646692012709999986, -78.55994805011499693, 1.218660606027000215 ) ) ;
#42145 = CARTESIAN_POINT ( 'NONE',  ( -7.730443418312603399, -24.12191635826273739, -10.25197760564498140 ) ) ;
#42146 = CONICAL_SURFACE ( 'NONE', #9141, 10.29999999990999981, 0.7853981633972997312 ) ;
#42147 = CARTESIAN_POINT ( 'NONE',  ( -6.224830695901311550, -77.52669311147933229, -8.871307822741991700 ) ) ;
#42148 = CARTESIAN_POINT ( 'NONE',  ( -11.43953470459854671, -78.22010116149509429, -3.071145924981994124 ) ) ;
#42149 = CARTESIAN_POINT ( 'NONE',  ( -7.508490145780001512, -78.91504759730605656, -8.005410190140000992 ) ) ;
#42150 = CARTESIAN_POINT ( 'NONE',  ( 10.06255860416000125, -76.46647654196999611, 6.919426796868999752 ) ) ;
#42151 = ORIENTED_EDGE ( 'NONE', *, *, #41982, .T. ) ;
#42152 = VECTOR ( 'NONE', #13064, 1000.000000000000000 ) ;
#42153 = CARTESIAN_POINT ( 'NONE',  ( 3.450648315675999722, -85.87746544543099958, 1.949103487304999938 ) ) ;
#42154 = CARTESIAN_POINT ( 'NONE',  ( -10.43174122427000050, -80.74346733149751287, 4.611552680554001249 ) ) ;
#42155 = AXIS2_PLACEMENT_3D ( 'NONE', #48365, #21762, #17054 ) ;
#42156 = CARTESIAN_POINT ( 'NONE',  ( 7.524111219894956903, -78.30076379627698202, -5.380381170981907601 ) ) ;
#42157 = CARTESIAN_POINT ( 'NONE',  ( 9.175589925015314563, -53.57304466838621693, 8.792768277016460132 ) ) ;
#42158 = DIRECTION ( 'NONE',  ( -1.000000000000000000, 0.000000000000000000, 0.000000000000000000 ) ) ;
#42159 = DIRECTION ( 'NONE',  ( 0.000000000000000000, 0.000000000000000000, -1.000000000000000000 ) ) ;
#42160 = CARTESIAN_POINT ( 'NONE',  ( -8.012466620630000591, -78.43986703093798951, -5.343555802860000981 ) ) ;
#42161 = VECTOR ( 'NONE', #40262, 1000.000000000000227 ) ;
#42162 = CARTESIAN_POINT ( 'NONE',  ( -0.4492251327744000156, -81.78555210223998984, 1.604198796042999753 ) ) ;
#42163 = CARTESIAN_POINT ( 'NONE',  ( 9.050966798898000931, -55.65000000893999754, -7.919595949288999570 ) ) ;
#42164 = CARTESIAN_POINT ( 'NONE',  ( 8.217893303462044940, -76.05520833333133623, 7.394497070576632858 ) ) ;
#42165 = VERTEX_POINT ( 'NONE', #35418 ) ;
#42166 = CARTESIAN_POINT ( 'NONE',  ( -10.12290050124000018, -23.24999999991999644, -7.648026767085999822 ) ) ;
#42167 = CARTESIAN_POINT ( 'NONE',  ( 11.02326530841000007, -80.95680626100980248, 1.187788371667000131 ) ) ;
#42168 = CARTESIAN_POINT ( 'NONE',  ( 2.264139176916503349, -78.96952922072273395, -2.758663917053780334 ) ) ;
#42169 = VERTEX_POINT ( 'NONE', #27448 ) ;
#42170 = EDGE_CURVE ( 'NONE', #1747, #13828, #3855, .T. ) ;
#42171 = CARTESIAN_POINT ( 'NONE',  ( 0.6284244718204999858, -78.34215887338820039, -1.176290284212999859 ) ) ;
#42172 = CARTESIAN_POINT ( 'NONE',  ( 12.82904091341000097, -60.12452529330000317, 2.062673488738000049 ) ) ;
#42173 = CARTESIAN_POINT ( 'NONE',  ( 0.007231935760147001867, -80.72610880796425192, -1.249626014905791171 ) ) ;
#42174 = ORIENTED_EDGE ( 'NONE', *, *, #8560, .F. ) ;
#42175 = CARTESIAN_POINT ( 'NONE',  ( 11.88669912479000068, -78.52591218578899657, 2.586293583890999948 ) ) ;
#42176 = CARTESIAN_POINT ( 'NONE',  ( 5.429444055910000344, -77.78519374448798374, -10.06097226053999982 ) ) ;
#42177 = CARTESIAN_POINT ( 'NONE',  ( -10.99608688423689173, -23.68532521788583622, -0.3139246511471364132 ) ) ;
#42178 = ORIENTED_EDGE ( 'NONE', *, *, #44622, .T. ) ;
#42179 = ORIENTED_EDGE ( 'NONE', *, *, #42567, .T. ) ;
#42180 = CARTESIAN_POINT ( 'NONE',  ( -0.9228900258640634346, -80.54165424860717337, 0.8427052285091912731 ) ) ;
#42181 = CARTESIAN_POINT ( 'NONE',  ( -8.268101562183998610, -77.17093998579798608, -4.764359567075000079 ) ) ;
#42182 = CARTESIAN_POINT ( 'NONE',  ( 9.630577183392999174, -79.09348223115100041, 1.628483183780000010 ) ) ;
#42183 = ADVANCED_FACE ( 'NONE', ( #39862 ), #12992, .T. ) ;
#42184 = ORIENTED_EDGE ( 'NONE', *, *, #25781, .F. ) ;
#42185 = CARTESIAN_POINT ( 'NONE',  ( 12.43356773662999970, -54.08739070985000552, 0.8411682846950000458 ) ) ;
#42186 = CARTESIAN_POINT ( 'NONE',  ( 17.49999986748943925, -13.07071424677999971, 0.002153571276233540773 ) ) ;
#42187 = ORIENTED_EDGE ( 'NONE', *, *, #25570, .T. ) ;
#42188 = CARTESIAN_POINT ( 'NONE',  ( -12.00000000000000000, -55.54999999966999980, 0.000000000000000000 ) ) ;
#42189 = CARTESIAN_POINT ( 'NONE',  ( -7.591316436381999821, -77.06111915034600202, -5.703451837412999659 ) ) ;
#42190 = AXIS2_PLACEMENT_3D ( 'NONE', #11640, #29615, #38196 ) ;
#42191 = CARTESIAN_POINT ( 'NONE',  ( -0.5056747962987626632, -80.19197092624497714, -1.143462194401485998 ) ) ;
#42192 = CARTESIAN_POINT ( 'NONE',  ( -1.931736162947161217, -18.23329604287648209, -12.72978979890375051 ) ) ;
#42193 = CARTESIAN_POINT ( 'NONE',  ( -3.040079553448159722, -79.14882913613843129, -9.237600482237251498 ) ) ;
#42194 = AXIS2_PLACEMENT_3D ( 'NONE', #42907, #51774, #57337 ) ;
#42195 = CARTESIAN_POINT ( 'NONE',  ( -1.463614972483658683, -78.37424901929817622, -0.4741960517313459356 ) ) ;
#42196 = CARTESIAN_POINT ( 'NONE',  ( 0.8825830062794586262, -80.62708333376913572, -3.954198616316053627 ) ) ;
#42197 = CARTESIAN_POINT ( 'NONE',  ( 10.69843650790000034, -76.27384350184999562, 6.089250768039999429 ) ) ;
#42198 = CARTESIAN_POINT ( 'NONE',  ( 9.393203674808285442, -77.70833333333332860, -5.413904038987152667 ) ) ;
#42199 = VECTOR ( 'NONE', #6931, 1000.000000000000000 ) ;
#42200 = EDGE_CURVE ( 'NONE', #14405, #19870, #8576, .T. ) ;
#42201 = CARTESIAN_POINT ( 'NONE',  ( 1.772203737798494716, -2.015750464275656739, -3.085565428039042324 ) ) ;
#42202 = CARTESIAN_POINT ( 'NONE',  ( 8.485538010685999666, -61.68067982404999583, -9.101501073510000595 ) ) ;
#42203 = VECTOR ( 'NONE', #22789, 1000.000000000000000 ) ;
#42204 = CARTESIAN_POINT ( 'NONE',  ( -9.042566447131001439, -79.07635346639000318, -8.284387575507999202 ) ) ;
#42205 = CARTESIAN_POINT ( 'NONE',  ( -4.885220488697999741, -76.47366117467699098, 11.26753068192000029 ) ) ;
#42206 =( BOUNDED_SURFACE ( )  B_SPLINE_SURFACE ( 3, 3, ( 
 ( #18689, #5972, #41995, #24277 ),
 ( #41117, #1563, #14822, #19555 ),
 ( #5393, #27523, #37553, #45565 ),
 ( #55570, #6262, #55276, #14242 ),
 ( #15119, #42295, #36391, #46742 ),
 ( #10412, #32821, #10713, #36973 ),
 ( #54417, #33117, #23109, #28691 ),
 ( #1278, #36682, #5678, #31949 ),
 ( #23689, #28104, #54986, #28397 ),
 ( #49994, #9540, #41702, #5110 ),
 ( #46154, #54698, #711, #19271 ),
 ( #18981, #50571, #50281, #14534 ),
 ( #37262, #32528, #32238, #9832 ),
 ( #50866, #27813, #45860, #23402 ),
 ( #41412, #995, #48184, #2723 ) ),
 .UNSPECIFIED., .F., .F., .F. ) 
 B_SPLINE_SURFACE_WITH_KNOTS ( ( 4, 1, 1, 1, 1, 1, 1, 1, 1, 1, 1, 1, 4 ),
 ( 4, 4 ),
 ( 0.009836358966825000175, 0.09153389967814999639, 0.1732269073519000224, 0.2549246240467999969, 0.3366128957582000258, 0.4183102327763000283, 0.5000049915180999616, 0.5816997512343000665, 0.6633971206824998967, 0.7450853986059999823, 0.8267830947368000061, 0.9084761241232000017, 0.9901736480482069558 ),
 ( 0.000000000000000000, 1.000000000000000000 ),
 .UNSPECIFIED. ) 
 GEOMETRIC_REPRESENTATION_ITEM ( )  RATIONAL_B_SPLINE_SURFACE ( (
 ( 1.000000000000000000, 0.3333333333333369786, 0.3333333333333369786, 1.000000000000000000),
 ( 1.000000000000000000, 0.3333333333333369786, 0.3333333333333369786, 1.000000000000000000),
 ( 1.000000000000000000, 0.3333333333333369786, 0.3333333333333369786, 1.000000000000000000),
 ( 1.000000000000000000, 0.3333333333333369786, 0.3333333333333369786, 1.000000000000000000),
 ( 1.000000000000000000, 0.3333333333333369786, 0.3333333333333369786, 1.000000000000000000),
 ( 1.000000000000000000, 0.3333333333333369786, 0.3333333333333369786, 1.000000000000000000),
 ( 1.000000000000000000, 0.3333333333333369786, 0.3333333333333369786, 1.000000000000000000),
 ( 1.000000000000000000, 0.3333333333333369786, 0.3333333333333369786, 1.000000000000000000),
 ( 1.000000000000000000, 0.3333333333333369786, 0.3333333333333369786, 1.000000000000000000),
 ( 1.000000000000000000, 0.3333333333333369786, 0.3333333333333369786, 1.000000000000000000),
 ( 1.000000000000000000, 0.3333333333333369786, 0.3333333333333369786, 1.000000000000000000),
 ( 1.000000000000000000, 0.3333333333333369786, 0.3333333333333369786, 1.000000000000000000),
 ( 1.000000000000000000, 0.3333333333333369786, 0.3333333333333369786, 1.000000000000000000),
 ( 1.000000000000000000, 0.3333333333333369786, 0.3333333333333369786, 1.000000000000000000),
 ( 1.000000000000000000, 0.3333333333333369786, 0.3333333333333369786, 1.000000000000000000) ) ) 
 REPRESENTATION_ITEM ( '' )  SURFACE ( )  );
#42207 = FACE_OUTER_BOUND ( 'NONE', #15293, .T. ) ;
#42208 = CARTESIAN_POINT ( 'NONE',  ( 2.412979349487003766, -2.792060389164095380, -2.177788168880055331 ) ) ;
#42209 = CARTESIAN_POINT ( 'NONE',  ( -9.233096103937967314, -77.61175265977985305, -9.061282067808580365 ) ) ;
#42210 = CARTESIAN_POINT ( 'NONE',  ( -8.286771986066998608, -78.69114955473354200, 7.559597915363999832 ) ) ;
#42211 = ORIENTED_EDGE ( 'NONE', *, *, #28484, .F. ) ;
#42213 = B_SPLINE_CURVE_WITH_KNOTS ( 'NONE', 3,
 ( #3602, #8029, #16612, #21318, #34882, #52910, #53786, #26595, #49062, #22182, #39612, #8610, #36055, #44631, #31314, #13320 ),
 .UNSPECIFIED., .F., .F.,
 ( 4, 2, 2, 2, 2, 2, 2, 4 ),
 ( 0.000000000000000000, 0.2500000000000023315, 0.3750000000000048295, 0.5000000000000073275, 0.6250000000000098810, 0.6875000000000082157, 0.7500000000000065503, 1.000000000000000000 ),
 .UNSPECIFIED. ) ;
#42212 = CARTESIAN_POINT ( 'NONE',  ( 1.242145130744999992, -82.73777244601899383, -0.5320213307544999770 ) ) ;
#42214 = CARTESIAN_POINT ( 'NONE',  ( 9.597472232836999240, -77.14168468004258727, -0.1661444564970999960 ) ) ;
#42215 = CARTESIAN_POINT ( 'NONE',  ( 7.792426477851446265, -24.29102098708791857, 10.18245125506949300 ) ) ;
#42216 = CARTESIAN_POINT ( 'NONE',  ( 0.000000000000000000, -3.749999999256000027, -8.749999999256001360 ) ) ;
#42217 = CARTESIAN_POINT ( 'NONE',  ( 2.696914660303999955, -3.191788721650999694, 2.553645155592000116 ) ) ;
#42218 = B_SPLINE_CURVE_WITH_KNOTS ( 'NONE', 3,
 ( #43799, #6904, #24912, #2485, #20488, #38485, #44657, #13050, #44951, #13643, #4799, #27212, #22207, #52935, #57935, #4211, #53218, #34904, #35780, #31638, #53809, #8635, #8342, #35478, #17794, #26621, #53509, #40518, #49681, #13345, #31342, #9226, #49384, #17198, #48509, #401, #40218, #22800, #8932, #45250, #58229, #12766, #4506, #17491, #31048, #22508, #12483, #26921, #3625, #44076, #49083, #35186, #36082, #111, #40809, #30483, #26051, #18089, #8056, #54101, #21630, #39635, #57643, #30762 ),
 .UNSPECIFIED., .F., .F.,
 ( 4, 2, 2, 1, 2, 2, 1, 1, 1, 2, 1, 1, 2, 2, 1, 2, 2, 2, 1, 1, 1, 2, 2, 2, 2, 2, 2, 2, 2, 2, 2, 2, 1, 2, 2, 1, 2, 4 ),
 ( 0.7213274189558753768, 0.7387444552711300849, 0.7474529734287574945, 0.7496301029681643469, 0.7499022441605901479, 0.7501743853530160600, 0.7507186677378677730, 0.7518072325075711992, 0.7561614915863849040, 0.7735785279016396121, 0.7822870460592670216, 0.7844641755986738740, 0.7855527403683773002, 0.7860970227532290133, 0.7866413051380807264, 0.7909955642168944312, 0.8084126005321492503, 0.8171211186897766598, 0.8192982482291834012, 0.8203868129988868274, 0.8209310953837385405, 0.8212032365761644526, 0.8214753777685903646, 0.8258296368474051796, 0.8606637094779239217, 0.8780807457931834037, 0.8867892639508130337, 0.8911435230296278487, 0.8933206525690353672, 0.8954977821084427747, 0.9303318547389628490, 0.9390403728965928121, 0.9433946319754078491, 0.9455717615148153676, 0.9466603262845191269, 0.9477488910542228862, 0.9651659273694819241, 1.000000000000000000 ),
 .UNSPECIFIED. ) ;
#42219 = CARTESIAN_POINT ( 'NONE',  ( 2.974124060854000273, -78.86371401997000419, 11.51680281503000103 ) ) ;
#42220 = CARTESIAN_POINT ( 'NONE',  ( 8.931146968900000260, -78.48816148727799202, -3.885139576175999920 ) ) ;
#42222 = CARTESIAN_POINT ( 'NONE',  ( -9.146956334765603103, -77.74765838888041003, -6.250533269645468515 ) ) ;
#42221 = CARTESIAN_POINT ( 'NONE',  ( -9.767653574770797320, -76.15254633665146855, 6.530473456064795457 ) ) ;
#42223 = B_SPLINE_CURVE_WITH_KNOTS ( 'NONE', 3,
 ( #55142, #37422, #46607, #32689 ),
 .UNSPECIFIED., .F., .F.,
 ( 4, 4 ),
 ( 0.000000000000000000, 1.000000000000000000 ),
 .UNSPECIFIED. ) ;
#42224 = CARTESIAN_POINT ( 'NONE',  ( 1.213634779058999857, -82.86625531570498993, 0.5941895605367999433 ) ) ;
#42225 = CARTESIAN_POINT ( 'NONE',  ( 1.368374140978463993, -85.94828564506399005, 3.153063748541422129 ) ) ;
#42226 = EDGE_LOOP ( 'NONE', ( #55886, #16541, #48749, #33588, #27235, #31321 ) ) ;
#42227 = CARTESIAN_POINT ( 'NONE',  ( 12.71759155191131185, -24.06493881574830951, 1.809604648260965343 ) ) ;
#42228 = CARTESIAN_POINT ( 'NONE',  ( -7.352179367232999141, -79.68555078125399405, 9.680938187455000232 ) ) ;
#42229 = CARTESIAN_POINT ( 'NONE',  ( -1.210774177386837902, -77.98557709862954823, 9.250434933897750511 ) ) ;
#42230 = CARTESIAN_POINT ( 'NONE',  ( 10.75000000000000000, -77.25000000000000000, 0.000000000000000000 ) ) ;
#42231 = CARTESIAN_POINT ( 'NONE',  ( -10.90760146693999921, -78.99931772544699982, -1.219937219691999974 ) ) ;
#42232 = CARTESIAN_POINT ( 'NONE',  ( -10.75000000000000000, -79.00000000000000000, 0.000000000000000000 ) ) ;
#42233 = CARTESIAN_POINT ( 'NONE',  ( 4.238048199687000306, -79.74073595533198500, -8.569131342697998477 ) ) ;
#42234 = CARTESIAN_POINT ( 'NONE',  ( 7.758650587948999977, -17.84922688128999724, -9.996717134846999642 ) ) ;
#42235 = CARTESIAN_POINT ( 'NONE',  ( 13.63885489310999510, -59.58578169018998949, -7.254376133916000668 ) ) ;
#42236 = ORIENTED_EDGE ( 'NONE', *, *, #46460, .F. ) ;
#42237 = CARTESIAN_POINT ( 'NONE',  ( 1.546579669427540882, -76.48592740986445904, -11.07638204203961863 ) ) ;
#42238 = DIRECTION ( 'NONE',  ( 0.000000000000000000, 1.000000000000000000, 0.000000000000000000 ) ) ;
#42239 = CARTESIAN_POINT ( 'NONE',  ( 3.400000000000108713, -78.67390000031814168, -4.163799117101134173E-16 ) ) ;
#42240 = CARTESIAN_POINT ( 'NONE',  ( -8.505218648663506187, -77.39023361062031370, 8.570118173896835501 ) ) ;
#42241 = ADVANCED_FACE ( 'NONE', ( #35723 ), #40897, .F. ) ;
#42242 = CARTESIAN_POINT ( 'NONE',  ( 0.4771002761174171769, -81.44403856892047600, 1.155230721378893044 ) ) ;
#42243 = AXIS2_PLACEMENT_3D ( 'NONE', #6806, #11248, #16249 ) ;
#42244 = EDGE_CURVE ( 'NONE', #19894, #42030, #40157, .T. ) ;
#42245 = DIRECTION ( 'NONE',  ( 0.000000000000000000, 1.000000000000000000, 0.000000000000000000 ) ) ;
#42246 = DIRECTION ( 'NONE',  ( 0.7071067811865475727, 0.000000000000000000, 0.7071067811865475727 ) ) ;
#42247 = CARTESIAN_POINT ( 'NONE',  ( 3.594201416108000036, -3.024676228556000268, 1.252117639952999850 ) ) ;
#42248 = VECTOR ( 'NONE', #53215, 1000.000000000000114 ) ;
#42249 = CARTESIAN_POINT ( 'NONE',  ( -1.405934784949000038, -79.13159159781999108, 0.2091203166687999881 ) ) ;
#42250 = FACE_OUTER_BOUND ( 'NONE', #7448, .T. ) ;
#42251 = CARTESIAN_POINT ( 'NONE',  ( -3.673276622528076629, -79.35225808950305293, 10.34286506330476740 ) ) ;
#42252 = DIRECTION ( 'NONE',  ( 0.000000000000000000, -1.000000000000000000, 0.000000000000000000 ) ) ;
#42253 = ORIENTED_EDGE ( 'NONE', *, *, #28555, .F. ) ;
#42254 = EDGE_CURVE ( 'NONE', #21333, #44757, #17735, .T. ) ;
#42255 = ORIENTED_EDGE ( 'NONE', *, *, #2552, .F. ) ;
#42256 = CARTESIAN_POINT ( 'NONE',  ( -9.144741847372999999, -78.41288998579800307, -4.101371784086000005 ) ) ;
#42257 = CARTESIAN_POINT ( 'NONE',  ( 9.008675998456572742, -78.80421538511130564, -5.865726045448368176 ) ) ;
#42258 = ORIENTED_EDGE ( 'NONE', *, *, #27697, .T. ) ;
#42259 = CARTESIAN_POINT ( 'NONE',  ( 8.798041828550999810, -17.06186490710999948, 8.790609563012999672 ) ) ;
#42260 = CARTESIAN_POINT ( 'NONE',  ( -9.040761882004836991, -79.37487198799524890, 2.917428640528126671 ) ) ;
#42261 = CARTESIAN_POINT ( 'NONE',  ( 10.64585027366999981, -79.12040545280000003, 5.670349170909000591 ) ) ;
#42262 = CARTESIAN_POINT ( 'NONE',  ( 9.992017125402000488, -60.96084086979999483, 7.762968460695000239 ) ) ;
#42263 = PLANE ( 'NONE',  #57056 ) ;
#42264 = CARTESIAN_POINT ( 'NONE',  ( 6.036049492268414696, -77.88288315575839249, 10.34824129380889168 ) ) ;
#42265 = CARTESIAN_POINT ( 'NONE',  ( 7.910349975595998728, -79.64660642326199991, 7.952639426948999279 ) ) ;
#42266 = ORIENTED_EDGE ( 'NONE', *, *, #52837, .T. ) ;
#42267 = DIRECTION ( 'NONE',  ( 0.000000000000000000, 1.000000000000000000, 0.000000000000000000 ) ) ;
#42268 = VERTEX_POINT ( 'NONE', #45192 ) ;
#42269 = CARTESIAN_POINT ( 'NONE',  ( 8.193194696117055642, -77.38854057934830166, 4.293485181109531368 ) ) ;
#42270 = CARTESIAN_POINT ( 'NONE',  ( -10.79754810892000094, -77.50716656116199488, -2.301543980133000211 ) ) ;
#42271 = CARTESIAN_POINT ( 'NONE',  ( -9.457632199924459471, -78.39508288952933412, -6.031152209911234685 ) ) ;
#42272 = CARTESIAN_POINT ( 'NONE',  ( -0.7952960770845000082, -77.90792523368020284, 1.405246626978000180 ) ) ;
#42273 = CARTESIAN_POINT ( 'NONE',  ( 0.000000000000000000, -9.638971321655001034, 0.000000000000000000 ) ) ;
#42274 = AXIS2_PLACEMENT_3D ( 'NONE', #37906, #11851, #38991 ) ;
#42275 = DIRECTION ( 'NONE',  ( 0.000000000000000000, 0.000000000000000000, 1.000000000000000000 ) ) ;
#42276 = CARTESIAN_POINT ( 'NONE',  ( -0.7004323366084000968, -78.41920298766999053, -1.469032877812000093 ) ) ;
#42277 = CARTESIAN_POINT ( 'NONE',  ( -1.049212147998610511, -79.14604918627101426, -0.6836784682508713074 ) ) ;
#42278 = CARTESIAN_POINT ( 'NONE',  ( -10.88870934378999955, -79.47949549020498239, 1.874540603341000145 ) ) ;
#42279 = CARTESIAN_POINT ( 'NONE',  ( -7.645391636765999976, -23.21530450358000053, -10.18949673576000059 ) ) ;
#42280 = CARTESIAN_POINT ( 'NONE',  ( 12.49168451100999988, -60.09848884406000025, -1.667916687331000070 ) ) ;
#42281 = CARTESIAN_POINT ( 'NONE',  ( -2.281180096131999679, -83.42707394314300018, -2.716758612191999767 ) ) ;
#42282 = ORIENTED_EDGE ( 'NONE', *, *, #10378, .F. ) ;
#42283 = CARTESIAN_POINT ( 'NONE',  ( 4.740509660090000743, -78.71728177378300018, 11.49416549648999819 ) ) ;
#42284 = DIRECTION ( 'NONE',  ( -0.7071067811865969777, -1.536189447283994854E-11, 0.7071067811864980568 ) ) ;
#42285 = CARTESIAN_POINT ( 'NONE',  ( 10.75000000000000000, -77.85000000000000853, 0.000000000000000000 ) ) ;
#42286 = B_SPLINE_CURVE_WITH_KNOTS ( 'NONE', 3,
 ( #56413, #25392, #48425, #42838 ),
 .UNSPECIFIED., .F., .F.,
 ( 4, 4 ),
 ( 0.000000000000000000, 1.000000000000000000 ),
 .UNSPECIFIED. ) ;
#42287 = CARTESIAN_POINT ( 'NONE',  ( -0.08519377839585000334, -78.44167163863899361, 11.97951611939999950 ) ) ;
#42288 = CARTESIAN_POINT ( 'NONE',  ( -7.956418361382000981, -17.47110680143000039, 9.787952249849000808 ) ) ;
#42289 = EDGE_CURVE ( 'NONE', #7824, #14640, #4851, .T. ) ;
#42290 = CARTESIAN_POINT ( 'NONE',  ( -0.7111482236519753863, -78.67248581485152670, 1.058674648179741773 ) ) ;
#42291 = AXIS2_PLACEMENT_3D ( 'NONE', #37836, #2993, #55855 ) ;
#42292 = CARTESIAN_POINT ( 'NONE',  ( 3.507528428923288200, -2.993384342491289818, -0.2940356736387945147 ) ) ;
#42293 = CARTESIAN_POINT ( 'NONE',  ( -7.401612602209000968, -79.24630584965400715, -6.305503003149000030 ) ) ;
#42294 = DIRECTION ( 'NONE',  ( 0.000000000000000000, -1.000000000000000000, 0.000000000000000000 ) ) ;
#42295 = CARTESIAN_POINT ( 'NONE',  ( 0.3917325915499037525, -85.88547955770000897, -8.744319679239929144 ) ) ;
#42296 = CARTESIAN_POINT ( 'NONE',  ( -5.656567264032000608, -78.04102034656098397, -9.471271359694998893 ) ) ;
#42297 = CARTESIAN_POINT ( 'NONE',  ( -1.925872869407999843, -76.76246555992319998, -12.12904120624999926 ) ) ;
#42298 = DIRECTION ( 'NONE',  ( 0.000000000000000000, -1.000000000000000000, 0.000000000000000000 ) ) ;
#42299 = ORIENTED_EDGE ( 'NONE', *, *, #4441, .F. ) ;
#42300 = CARTESIAN_POINT ( 'NONE',  ( -1.179157772963000061, -82.22698077501999592, 0.6230118014947999550 ) ) ;
#42301 = DIRECTION ( 'NONE',  ( 0.000000000000000000, -1.000000000000000000, 0.000000000000000000 ) ) ;
#42302 = CARTESIAN_POINT ( 'NONE',  ( -7.398464061241327272, -55.34839576621715906, 8.140250184786385290 ) ) ;
#42303 = CARTESIAN_POINT ( 'NONE',  ( 5.263131812197999970, -77.92997156672200276, -9.905430536777000583 ) ) ;
#42304 = CARTESIAN_POINT ( 'NONE',  ( 7.318097147681000614, -79.49262545241899147, -8.179820946710000484 ) ) ;
#42305 = CARTESIAN_POINT ( 'NONE',  ( 7.974014308125999762, -24.63100890329999970, -9.929675091742000248 ) ) ;
#42306 = CARTESIAN_POINT ( 'NONE',  ( 3.651490241511724300, -84.05729166430741373, 1.754833245226501859 ) ) ;
#42307 = CARTESIAN_POINT ( 'NONE',  ( -9.626240109848000159, -76.12883592657999543, -7.417705737357999318 ) ) ;
#42308 = CARTESIAN_POINT ( 'NONE',  ( -0.9465222407332000154, -81.15663953506998496, -0.8164530897714000757 ) ) ;
#42309 = ORIENTED_EDGE ( 'NONE', *, *, #57529, .T. ) ;
#42310 = CARTESIAN_POINT ( 'NONE',  ( -0.4987175214384371169, -80.00792896450899150, 1.146052696381754110 ) ) ;
#42311 = CARTESIAN_POINT ( 'NONE',  ( -1.310679582531386611, -79.54166666666667140, -0.7554284705563495406 ) ) ;
#42312 = CARTESIAN_POINT ( 'NONE',  ( 7.657744736598999680, -55.13080421771999795, -9.966195456739999514 ) ) ;
#42313 = CARTESIAN_POINT ( 'NONE',  ( -0.8287201338969000242, -77.39572957994299429, -11.23152649900999833 ) ) ;
#42314 = EDGE_CURVE ( 'NONE', #31856, #19957, #46568, .T. ) ;
#42315 = CARTESIAN_POINT ( 'NONE',  ( -1.387963714323000142, -79.72375898957000118, 0.9213108730841000904 ) ) ;
#42316 = CARTESIAN_POINT ( 'NONE',  ( 1.158746710145999836, -78.15648218165999594, -0.8458044512135999282 ) ) ;
#42317 = CARTESIAN_POINT ( 'NONE',  ( -12.00000000000000000, -78.29999999999999716, 0.000000000000000000 ) ) ;
#42318 = CARTESIAN_POINT ( 'NONE',  ( 1.105771037839567761, -81.55968126227546122, 1.028509483357399112 ) ) ;
#42319 = CARTESIAN_POINT ( 'NONE',  ( -1.464697089188547574, -83.32914288647991441, 0.3814761973796438888 ) ) ;
#42320 = CARTESIAN_POINT ( 'NONE',  ( -5.827782744364191636, -78.51269081667429361, 10.39236577010555607 ) ) ;
#42321 = CIRCLE ( 'NONE', #18755, 12.80000000000000071 ) ;
#42322 = CARTESIAN_POINT ( 'NONE',  ( 0.3279140402491176332, -80.95484126934748303, 1.218292940065619057 ) ) ;
#42323 = ORIENTED_EDGE ( 'NONE', *, *, #9988, .T. ) ;
#42324 = CARTESIAN_POINT ( 'NONE',  ( -0.03659624652677806456, -81.72330189448304338, -1.249620685942105958 ) ) ;
#42325 = B_SPLINE_CURVE_WITH_KNOTS ( 'NONE', 3,
 ( #46276, #5508, #55695, #15244, #11129, #6387 ),
 .UNSPECIFIED., .F., .F.,
 ( 4, 2, 4 ),
 ( 0.000000000000000000, 0.5000000000000001110, 1.000000000000000000 ),
 .UNSPECIFIED. ) ;
#42326 = CARTESIAN_POINT ( 'NONE',  ( 5.709935245961999861, -78.72334026635199677, 9.573465417320001336 ) ) ;
#42327 = CARTESIAN_POINT ( 'NONE',  ( -1.217465845835394411, -80.02083333333330017, -0.3271848554491003647 ) ) ;
#42328 = ORIENTED_EDGE ( 'NONE', *, *, #43127, .T. ) ;
#42329 = ADVANCED_FACE ( 'NONE', ( #41624 ), #1204, .T. ) ;
#42330 = EDGE_LOOP ( 'NONE', ( #21967, #42323 ) ) ;
#42331 = CARTESIAN_POINT ( 'NONE',  ( -0.6748602203104000496, -81.95902128140700427, 1.357759211597000082 ) ) ;
#42332 = EDGE_CURVE ( 'NONE', #51603, #7386, #5075, .T. ) ;
#42333 = ORIENTED_EDGE ( 'NONE', *, *, #33072, .T. ) ;
#42334 = VERTEX_POINT ( 'NONE', #28615 ) ;
#42335 = CARTESIAN_POINT ( 'NONE',  ( 0.005928781627485999947, -16.79886949736999924, 12.66336824419000173 ) ) ;
#42336 = LINE ( 'NONE', #1903, #18855 ) ;
#42337 = AXIS2_PLACEMENT_3D ( 'NONE', #23007, #24174, #23585 ) ;
#42338 = PRODUCT_CONTEXT ( 'NONE', #42101, 'mechanical' ) ;
#42339 = CARTESIAN_POINT ( 'NONE',  ( 1.310679582531387943, -78.20833333333334281, -0.7554284705563468760 ) ) ;
#42340 = CARTESIAN_POINT ( 'NONE',  ( 10.48543666025110710, -76.50833333332482766, -6.043427764450776785 ) ) ;
#42341 = CARTESIAN_POINT ( 'NONE',  ( 6.931362644077239565, -78.29243420434676182, -6.125879640451257657 ) ) ;
#42342 = CARTESIAN_POINT ( 'NONE',  ( 10.63562707217000103, -79.97404714773999501, 3.563914325689000240 ) ) ;
#42343 = ORIENTED_EDGE ( 'NONE', *, *, #34464, .T. ) ;
#42344 = VERTEX_POINT ( 'NONE', #38063 ) ;
#42345 = CARTESIAN_POINT ( 'NONE',  ( -9.012377310937894848, -77.58185562474179164, 2.097317376807573019 ) ) ;
#42346 = CARTESIAN_POINT ( 'NONE',  ( 7.128677745341877703, -77.70833333333332860, 6.432089047655187741 ) ) ;
#42347 = CARTESIAN_POINT ( 'NONE',  ( -0.9218200799623775810, -79.42708333333334281, 1.199500263597266247 ) ) ;
#42348 = CARTESIAN_POINT ( 'NONE',  ( -1.575772165365692645, -61.26154542772368927, -12.70597445621287847 ) ) ;
#42349 = CARTESIAN_POINT ( 'NONE',  ( -9.685922776715001348, -77.20466883505099531, 0.5943755449006998814 ) ) ;
#42350 = DIRECTION ( 'NONE',  ( 0.000000000000000000, 0.000000000000000000, -1.000000000000000000 ) ) ;
#42351 = CARTESIAN_POINT ( 'NONE',  ( -1.250000000000001332, -79.98958333333332860, 0.1636246173744632659 ) ) ;
#42352 = CARTESIAN_POINT ( 'NONE',  ( -2.653227710365042125, -77.40733822163998923, -11.74665041585867975 ) ) ;
#42353 = CARTESIAN_POINT ( 'NONE',  ( 1.554657762476000071, -80.98652648686000077, -0.6948770361563999520 ) ) ;
#42354 = AXIS2_PLACEMENT_3D ( 'NONE', #11666, #29641, #47694 ) ;
#42355 = CARTESIAN_POINT ( 'NONE',  ( -4.094075590313999591, -78.72741664101050674, -0.8028934812383000663 ) ) ;
#42356 = CARTESIAN_POINT ( 'NONE',  ( 1.437150570762024460, -79.52522577555218675, 0.4693744638702325722 ) ) ;
#42357 = CARTESIAN_POINT ( 'NONE',  ( 2.227885729735000098, -79.15013667140100040, -9.542051086884001165 ) ) ;
#42358 = CARTESIAN_POINT ( 'NONE',  ( 1.570796326794856590, -77.26458333333336270, 12.00000000000000711 ) ) ;
#42359 = CARTESIAN_POINT ( 'NONE',  ( 1.799475304559999822, -21.75171076523999858, -12.69616050742999924 ) ) ;
#42360 = EDGE_CURVE ( 'NONE', #50040, #54902, #51083, .T. ) ;
#42362 = CARTESIAN_POINT ( 'NONE',  ( 1.669849926071999890, -18.62771399582999976, -12.48404299553000030 ) ) ;
#42361 = CARTESIAN_POINT ( 'NONE',  ( 1.460959015002472494, -78.67083333333334849, 0.3926218265389232465 ) ) ;
#42363 = CIRCLE ( 'NONE', #10323, 10.50000000000000000 ) ;
#42364 = CARTESIAN_POINT ( 'NONE',  ( -14.00000000000000000, -46.09579702914000165, 0.000000000000000000 ) ) ;
#42365 = DIRECTION ( 'NONE',  ( 0.000000000000000000, 1.000000000000000000, 0.000000000000000000 ) ) ;
#42366 = CARTESIAN_POINT ( 'NONE',  ( -4.665811493887000339, -78.23240233375699404, 10.25008134894000023 ) ) ;
#42367 = CARTESIAN_POINT ( 'NONE',  ( 2.086062294176650678, -1.425354687551017463, -2.850033995333124182 ) ) ;
#42368 = EDGE_CURVE ( 'NONE', #42463, #27850, #27691, .T. ) ;
#42369 = ORIENTED_EDGE ( 'NONE', *, *, #13845, .F. ) ;
#42370 = CARTESIAN_POINT ( 'NONE',  ( 8.130811096204000776, -61.48523690322999613, 9.546858433459998849 ) ) ;
#42371 = CARTESIAN_POINT ( 'NONE',  ( -1.539691793600886482, -77.58363846744875048, 11.67469292510621948 ) ) ;
#42372 = CARTESIAN_POINT ( 'NONE',  ( 0.4847454816353202744, -78.44349313809972557, 1.152238203202561762 ) ) ;
#42373 = CARTESIAN_POINT ( 'NONE',  ( 8.558937808803998237, -79.68115074656799379, 4.441044281071000022 ) ) ;
#42374 = AXIS2_PLACEMENT_3D ( 'NONE', #39093, #12516, #25514 ) ;
#42375 = CARTESIAN_POINT ( 'NONE',  ( -12.54980553584999825, -53.75222688831999562, -0.05649961219500999887 ) ) ;
#42376 = CARTESIAN_POINT ( 'NONE',  ( -0.1055445576787907014, -79.47591176498374921, 10.74947584515206600 ) ) ;
#42377 = CARTESIAN_POINT ( 'NONE',  ( -2.389266123960000154, -79.48483998579800414, -9.554412305752000734 ) ) ;
#42378 = DIRECTION ( 'NONE',  ( -1.000000000000000000, 0.000000000000000000, 0.000000000000000000 ) ) ;
#42379 = CARTESIAN_POINT ( 'NONE',  ( -7.349905019660000427, -77.67524080624798444, 8.405004550887998249 ) ) ;
#42380 = B_SPLINE_CURVE_WITH_KNOTS ( 'NONE', 3,
 ( #15122, #5975, #6562, #51162, #1863, #37853, #15424, #33416, #51454, #11007, #28991, #53757, #39586, #17741, #30710, #40162, #35137, #39298 ),
 .UNSPECIFIED., .F., .F.,
 ( 4, 2, 2, 2, 2, 2, 2, 2, 4 ),
 ( 0.000000000000000000, 0.1250000000000000000, 0.2500000000000000000, 0.3750000000000000000, 0.5000000000000000000, 0.6250000000000000000, 0.7500000000000000000, 0.8750000000000000000, 1.000000000000000000 ),
 .UNSPECIFIED. ) ;
#42381 = CARTESIAN_POINT ( 'NONE',  ( -0.3849377561737999942, -82.01377306213599638, -1.557230663560999817 ) ) ;
#42382 = CARTESIAN_POINT ( 'NONE',  ( 6.669449228234999971, -78.33514514476064505, -7.075468016816000016 ) ) ;
#42383 = CARTESIAN_POINT ( 'NONE',  ( -5.511117113485999752, -78.59604234163299452, -7.631433854063000233 ) ) ;
#42385 = CARTESIAN_POINT ( 'NONE',  ( -3.165411199172029288, -2.979166666666666075, 0.8506806241676482250 ) ) ;
#42384 = CARTESIAN_POINT ( 'NONE',  ( 2.741005327708999850, -83.82504052802198657, 2.568707870063999810 ) ) ;
#42386 = CARTESIAN_POINT ( 'NONE',  ( 6.479078291783999966, -79.37445584965399803, -7.022474634662000170 ) ) ;
#42387 = CARTESIAN_POINT ( 'NONE',  ( -1.199500263597274241, -80.84791666666667709, 0.9218200799623669228 ) ) ;
#42388 = CARTESIAN_POINT ( 'NONE',  ( 6.016754219673178028, -80.27273110789552391, -8.908175812766630841 ) ) ;
#42389 = CARTESIAN_POINT ( 'NONE',  ( -7.559222841336621812, -77.16294525579797892, -7.643355431292909508 ) ) ;
#42390 = FACE_OUTER_BOUND ( 'NONE', #10445, .T. ) ;
#42391 = CARTESIAN_POINT ( 'NONE',  ( -12.50000000000000000, -23.24999999758999536, 1.750000000000000000 ) ) ;
#42392 = ORIENTED_EDGE ( 'NONE', *, *, #39224, .F. ) ;
#42393 = VERTEX_POINT ( 'NONE', #14744 ) ;
#42394 = CARTESIAN_POINT ( 'NONE',  ( 4.847151869481000297, -78.97589164704000098, 11.00961342987999991 ) ) ;
#42395 = DIRECTION ( 'NONE',  ( -0.7026410690473252618, -0.1122098755728027641, -0.7026410690473252618 ) ) ;
#42396 = DIRECTION ( 'NONE',  ( 0.000000000000000000, -1.000000000000000000, 0.000000000000000000 ) ) ;
#42397 = ORIENTED_EDGE ( 'NONE', *, *, #40270, .T. ) ;
#42398 = CARTESIAN_POINT ( 'NONE',  ( 10.14226539039000130, -78.41758737238698984, 6.290465419776000822 ) ) ;
#42399 = EDGE_CURVE ( 'NONE', #32925, #50534, #39341, .T. ) ;
#42400 = ORIENTED_EDGE ( 'NONE', *, *, #55187, .T. ) ;
#42401 = EDGE_LOOP ( 'NONE', ( #25019, #8687, #6964, #13437 ) ) ;
#42402 = AXIS2_PLACEMENT_3D ( 'NONE', #21646, #57953, #39653 ) ;
#42403 = VERTEX_POINT ( 'NONE', #54907 ) ;
#42404 = B_SPLINE_CURVE_WITH_KNOTS ( 'NONE', 3,
 ( #32026, #33188, #50067, #45643, #45345, #5755, #1644, #4896, #5181, #23472, #19633, #27600, #55648, #46231, #55062, #32605, #10198, #23763 ),
 .UNSPECIFIED., .F., .F.,
 ( 4, 2, 2, 2, 2, 2, 2, 2, 4 ),
 ( 0.000000000000000000, 0.06250000000000068001, 0.1250000000000013600, 0.2500000000000027200, 0.5000000000000014433, 0.7500000000000001110, 0.8124999999999988898, 0.8749999999999975575, 1.000000000000000000 ),
 .UNSPECIFIED. ) ;
#42405 = CARTESIAN_POINT ( 'NONE',  ( -3.026233407092999705, -80.05643680478300439, 1.850265178281999878 ) ) ;
#42406 = CARTESIAN_POINT ( 'NONE',  ( 6.204990652802643503, -79.21820937768764281, 7.193542684779512975 ) ) ;
#42407 = ORIENTED_EDGE ( 'NONE', *, *, #37066, .T. ) ;
#42408 = CARTESIAN_POINT ( 'NONE',  ( 0.7483892436387024061, -82.77648090350101029, -1.000966064142216450 ) ) ;
#42409 = VERTEX_POINT ( 'NONE', #32451 ) ;
#42410 = CARTESIAN_POINT ( 'NONE',  ( -3.060972652365999913, -2.035913946620000026, 0.7739355898497000119 ) ) ;
#42411 = ORIENTED_EDGE ( 'NONE', *, *, #57995, .T. ) ;
#42412 = CARTESIAN_POINT ( 'NONE',  ( 6.606377239730347739, -80.67708333333331439, -8.596418555780422466 ) ) ;
#42413 = CARTESIAN_POINT ( 'NONE',  ( -1.339962141614804425, -78.21213723365808335, 0.6906518060847610663 ) ) ;
#42414 = CIRCLE ( 'NONE', #2835, 4.299999999999999822 ) ;
#42415 = CARTESIAN_POINT ( 'NONE',  ( 0.000000000000000000, -75.10000000284179578, -7.200000000000000178 ) ) ;
#42416 = DIRECTION ( 'NONE',  ( 0.000000000000000000, 0.000000000000000000, 1.000000000000000000 ) ) ;
#42417 = VECTOR ( 'NONE', #38180, 1000.000000000000000 ) ;
#42418 = EDGE_CURVE ( 'NONE', #14353, #23790, #50496, .T. ) ;
#42419 = CARTESIAN_POINT ( 'NONE',  ( 5.091895231007000255, -78.58104366793577356, 8.260951054388000259 ) ) ;
#42420 = CARTESIAN_POINT ( 'NONE',  ( 5.177752511601999785, -76.73837828040700515, 9.912858493839999952 ) ) ;
#42421 = CARTESIAN_POINT ( 'NONE',  ( 1.459540817232405363, -76.46516187205870096, 10.67798020080688381 ) ) ;
#42422 = FACE_OUTER_BOUND ( 'NONE', #9319, .T. ) ;
#42423 = CARTESIAN_POINT ( 'NONE',  ( 1.092232985442823212, -81.20833333333332860, -0.6295237254636224522 ) ) ;
#42424 = CARTESIAN_POINT ( 'NONE',  ( -7.678690995233999672, -57.04351820043999766, -10.59551070214999946 ) ) ;
#42425 = CARTESIAN_POINT ( 'NONE',  ( -7.847716748518878127, -78.64456789939313808, -4.896326238464910219 ) ) ;
#42426 = CARTESIAN_POINT ( 'NONE',  ( 6.534747300401333447, -76.52789284558512861, 9.765094741288242730 ) ) ;
#42427 = CARTESIAN_POINT ( 'NONE',  ( -1.000649921775999873, -79.66441203194099785, 0.8816325131470000853 ) ) ;
#42428 = CARTESIAN_POINT ( 'NONE',  ( -5.608494644813585062, -80.18255198204721523, -9.462727630867055595 ) ) ;
#42429 = CARTESIAN_POINT ( 'NONE',  ( 12.00000000000000000, -60.04999999966999980, 0.000000000000000000 ) ) ;
#42430 = CARTESIAN_POINT ( 'NONE',  ( -2.051600333657000341, -80.24142549782600042, -2.945279881917999720 ) ) ;
#42431 = CARTESIAN_POINT ( 'NONE',  ( 1.490799555696999956, -79.37411536532098921, 12.10894905701999846 ) ) ;
#42432 = CARTESIAN_POINT ( 'NONE',  ( -8.590066394520892601, -78.04883425186237389, 6.463634606814313344 ) ) ;
#42433 = CARTESIAN_POINT ( 'NONE',  ( 0.8790514971010287004, -82.91354635334799639, 0.8881463262467683695 ) ) ;
#42434 = DIRECTION ( 'NONE',  ( 0.000000000000000000, 1.000000000000000000, 0.000000000000000000 ) ) ;
#42435 = CARTESIAN_POINT ( 'NONE',  ( -7.648802896946197194, -76.26817011481092834, -8.920997862297024739 ) ) ;
#42436 = CARTESIAN_POINT ( 'NONE',  ( 1.250000000000000000, -18.55321828668999729, 12.50000000000000000 ) ) ;
#42437 = EDGE_CURVE ( 'NONE', #27162, #29661, #5599, .T. ) ;
#42438 = CARTESIAN_POINT ( 'NONE',  ( -10.53559655518999882, -60.00569178284000316, -7.620036226177999694 ) ) ;
#42439 = CARTESIAN_POINT ( 'NONE',  ( 0.07833262907167658218, -3.500000000000000444, 3.294754266843233470 ) ) ;
#42440 = CARTESIAN_POINT ( 'NONE',  ( 1.221474390223999951, -81.35146937156800107, -0.5353283698298000326 ) ) ;
#42441 = VECTOR ( 'NONE', #54550, 1000.000000000000000 ) ;
#42442 = CARTESIAN_POINT ( 'NONE',  ( 1.371980222863132370, -79.21275704297983111, -0.7006253647128551920 ) ) ;
#42443 = CARTESIAN_POINT ( 'NONE',  ( 12.54901606605999831, -25.00731603500000233, 0.4733145588205000531 ) ) ;
#42444 = CARTESIAN_POINT ( 'NONE',  ( 8.601671466536686239, -78.14867843084759613, -6.555704085095740652 ) ) ;
#42445 = CARTESIAN_POINT ( 'NONE',  ( 11.74911438887889759, -78.44153470896613101, -0.7697094805160100695 ) ) ;
#42446 = CARTESIAN_POINT ( 'NONE',  ( 0.9090372547675998893, -78.71840111697744646, 10.93790052300000148 ) ) ;
#42447 = CARTESIAN_POINT ( 'NONE',  ( -11.41861126715999930, -76.22951562304000106, 3.886338190518000335 ) ) ;
#42448 = ORIENTED_EDGE ( 'NONE', *, *, #49350, .T. ) ;
#42449 = CARTESIAN_POINT ( 'NONE',  ( -3.929712059496000442, -85.03571544543099492, -0.5131704721504000144 ) ) ;
#42450 = CARTESIAN_POINT ( 'NONE',  ( -8.447960142255000804, -80.15114997703010147, 7.488267305661000961 ) ) ;
#42451 = DIRECTION ( 'NONE',  ( 0.000000000000000000, 1.000000000000000000, 0.000000000000000000 ) ) ;
#42452 = FACE_OUTER_BOUND ( 'NONE', #51120, .T. ) ;
#42453 = CARTESIAN_POINT ( 'NONE',  ( -9.524774638983998898, -77.35740375522699708, 5.924253427062000199 ) ) ;
#42454 = CARTESIAN_POINT ( 'NONE',  ( 12.70956139856000000, -55.39498835716000258, -1.933780970937999832 ) ) ;
#42455 = CARTESIAN_POINT ( 'NONE',  ( 1.492456682423999981, -77.46642875802798756, -9.624565956529000488 ) ) ;
#42456 = CARTESIAN_POINT ( 'NONE',  ( 1.484562552624000054, -82.10134817779000116, -0.7558657512595999828 ) ) ;
#42457 = CARTESIAN_POINT ( 'NONE',  ( 3.914500761937000028, -78.91452044229970397, 0.000000000000000000 ) ) ;
#42458 = CARTESIAN_POINT ( 'NONE',  ( 13.86363636363000218, -9.638971321655001034, 1.277887488545999904E-05 ) ) ;
#42459 = ORIENTED_EDGE ( 'NONE', *, *, #18529, .T. ) ;
#42460 = DIRECTION ( 'NONE',  ( 0.000000000000000000, 0.000000000000000000, -1.000000000000000000 ) ) ;
#42461 = VECTOR ( 'NONE', #44641, 1000.000000000000000 ) ;
#42462 = CARTESIAN_POINT ( 'NONE',  ( 2.220969153522253325, -78.96057212360685185, -3.162631883084828566 ) ) ;
#42463 = VERTEX_POINT ( 'NONE', #55201 ) ;
#42464 = CARTESIAN_POINT ( 'NONE',  ( -0.6568659331174000471, -78.05032173890430158, 1.160647793301999853 ) ) ;
#42465 = DIRECTION ( 'NONE',  ( 0.000000000000000000, -1.000000000000000000, 0.000000000000000000 ) ) ;
#42466 = CARTESIAN_POINT ( 'NONE',  ( -7.241278761924999863, -80.25027481282198494, -9.001616806789000336 ) ) ;
#42467 = ORIENTED_EDGE ( 'NONE', *, *, #42437, .T. ) ;
#42468 = CARTESIAN_POINT ( 'NONE',  ( -6.882647548562999873, -78.33600697782200939, -10.03053803679000033 ) ) ;
#42469 = CARTESIAN_POINT ( 'NONE',  ( 3.794578590805999685, -77.90474154703099430, 10.66739949363999962 ) ) ;
#42470 = CARTESIAN_POINT ( 'NONE',  ( 4.145634294517788199, -78.65634848184657812, -9.984937452013063819 ) ) ;
#42471 = ORIENTED_EDGE ( 'NONE', *, *, #20840, .F. ) ;
#42472 = ORIENTED_EDGE ( 'NONE', *, *, #19663, .T. ) ;
#42473 = CARTESIAN_POINT ( 'NONE',  ( -0.3529553161740807132, -80.49780249966943302, 1.199325851874515125 ) ) ;
#42474 = CARTESIAN_POINT ( 'NONE',  ( 2.813607249808706801, -77.74586376683228650, -10.46960172016192558 ) ) ;
#42475 = CARTESIAN_POINT ( 'NONE',  ( 9.630577183392999174, -79.27363800027249852, 1.628483183780000010 ) ) ;
#42476 = EDGE_LOOP ( 'NONE', ( #18804, #57662, #43778 ) ) ;
#42477 = CARTESIAN_POINT ( 'NONE',  ( 1.997394009589563924, -2.424135704803565439, 2.599556423877257938 ) ) ;
#42478 = CARTESIAN_POINT ( 'NONE',  ( 8.325251318307000048, -79.76743035202900955, -7.061554902978000037 ) ) ;
#42479 = AXIS2_PLACEMENT_3D ( 'NONE', #6060, #55662, #33202 ) ;
#42480 = ORIENTED_EDGE ( 'NONE', *, *, #25745, .T. ) ;
#42481 = CARTESIAN_POINT ( 'NONE',  ( -12.83838776459000108, -23.20596988487999823, -2.062170466181000528 ) ) ;
#42482 = CARTESIAN_POINT ( 'NONE',  ( -3.437217408589349432, -78.72609999968184979, -1.942147800595246165 ) ) ;
#42483 = EDGE_CURVE ( 'NONE', #49808, #1317, #32743, .T. ) ;
#42484 = CARTESIAN_POINT ( 'NONE',  ( 9.250000000000000000, -78.34999999999999432, 0.000000000000000000 ) ) ;
#42485 = CARTESIAN_POINT ( 'NONE',  ( 0.000000000000000000, -76.79999999999999716, 0.000000000000000000 ) ) ;
#42486 = CARTESIAN_POINT ( 'NONE',  ( 1.134100835125040119, -79.18344744587857065, -9.422324300646277351 ) ) ;
#42487 = CARTESIAN_POINT ( 'NONE',  ( 9.444950681165998674, -76.84924050810879237, -2.026199312500999827 ) ) ;
#42488 = CARTESIAN_POINT ( 'NONE',  ( 1.440361722493033625, -79.12381928720844826, 0.4511061928964619772 ) ) ;
#42489 = CARTESIAN_POINT ( 'NONE',  ( -10.99999999999999822, -79.61041666666666572, -1.439896632895323325 ) ) ;
#42490 = CARTESIAN_POINT ( 'NONE',  ( -6.282410744257000523, -75.90028781030999028, 10.58616248715999930 ) ) ;
#42491 = AXIS2_PLACEMENT_3D ( 'NONE', #5348, #663, #18650 ) ;
#42492 = CARTESIAN_POINT ( 'NONE',  ( 7.483407197968000801, -77.19999999999998863, -5.437013583705000208 ) ) ;
#42493 = CARTESIAN_POINT ( 'NONE',  ( 9.317978910689999950, -61.93238462986000314, -8.588869595475999930 ) ) ;
#42494 = CARTESIAN_POINT ( 'NONE',  ( -12.10179013622999911, -78.46094648960999507, -1.986401539992999954 ) ) ;
#42495 = CARTESIAN_POINT ( 'NONE',  ( -8.598496321198998871, -77.12938498755599426, -8.768570137950998600 ) ) ;
#42496 = CARTESIAN_POINT ( 'NONE',  ( -7.889735440110458242, -60.55042584425823549, -7.666647577132536640 ) ) ;
#42497 = EDGE_CURVE ( 'NONE', #43600, #25463, #49283, .T. ) ;
#42498 = CARTESIAN_POINT ( 'NONE',  ( 10.65229704191123616, -78.26108579923685227, -5.670296759119941576 ) ) ;
#42499 = DIRECTION ( 'NONE',  ( 0.000000000000000000, -1.000000000000000000, 0.000000000000000000 ) ) ;
#42500 = EDGE_LOOP ( 'NONE', ( #8910, #18862, #23014, #37375 ) ) ;
#42501 = CARTESIAN_POINT ( 'NONE',  ( -1.266615395500999997, -82.54829480068799796, -0.4708042714212999913 ) ) ;
#42502 = CARTESIAN_POINT ( 'NONE',  ( -8.355323416140999271, -77.28668387500499648, 4.941688539782999712 ) ) ;
#42503 = DIRECTION ( 'NONE',  ( 0.9999548435846228323, 0.000000000000000000, 0.009503199022040218977 ) ) ;
#42504 = DIRECTION ( 'NONE',  ( 0.000000000000000000, -1.000000000000000000, 0.000000000000000000 ) ) ;
#42505 = CARTESIAN_POINT ( 'NONE',  ( -1.465608348446000075, -2.200283069271000258, 3.582222755774000067 ) ) ;
#42506 = CARTESIAN_POINT ( 'NONE',  ( 1.730980777285999972, -77.14552404313198508, -11.76800180821999930 ) ) ;
#42507 = CARTESIAN_POINT ( 'NONE',  ( -5.370832524224000259, -77.69229427166699509, 8.124890996387998499 ) ) ;
#42508 = EDGE_CURVE ( 'NONE', #28917, #46546, #23868, .T. ) ;
#42510 = CARTESIAN_POINT ( 'NONE',  ( -4.043136777828878259, -77.79531677776081722, -10.31450538517582416 ) ) ;
#42509 = CARTESIAN_POINT ( 'NONE',  ( -2.856588293545408774, -76.09423490609401597, 11.40386817198159441 ) ) ;
#42511 = CARTESIAN_POINT ( 'NONE',  ( -5.128001663057999870, -78.94050342418300659, 9.637373342098999984 ) ) ;
#42512 = CARTESIAN_POINT ( 'NONE',  ( 1.026866341085000007E-14, -0.1000000000000002554, 0.000000000000000000 ) ) ;
#42513 = EDGE_LOOP ( 'NONE', ( #12380, #30590, #30743, #22623 ) ) ;
#42514 = DIRECTION ( 'NONE',  ( 0.000000000000000000, 1.000000000000000000, 0.000000000000000000 ) ) ;
#42515 = EDGE_CURVE ( 'NONE', #53612, #56919, #15922, .T. ) ;
#42516 = CYLINDRICAL_SURFACE ( 'NONE', #10692, 3.250000000000000000 ) ;
#42517 = CIRCLE ( 'NONE', #36854, 9.000000000000000000 ) ;
#42518 = CARTESIAN_POINT ( 'NONE',  ( 0.4254240051736068451, -2.364583333333333481, 3.250000000000001776 ) ) ;
#42519 = CARTESIAN_POINT ( 'NONE',  ( -9.213114944054998645, -61.80524898723000149, 8.533795138624000742 ) ) ;
#42520 = CARTESIAN_POINT ( 'NONE',  ( -10.47663719470709331, -80.07552825402615326, 3.352253582661057774 ) ) ;
#42521 = CARTESIAN_POINT ( 'NONE',  ( 7.655485751584000020, -79.77808361358998468, -5.725784120545999833 ) ) ;
#42522 = CARTESIAN_POINT ( 'NONE',  ( 1.695907231049564201, -3.266824736097686088, -2.897058440794695766 ) ) ;
#42523 = CARTESIAN_POINT ( 'NONE',  ( 5.684557159767975598, -79.17708333333330017, -7.396918292183157106 ) ) ;
#42524 = B_SPLINE_CURVE_WITH_KNOTS ( 'NONE', 3,
 ( #39640, #53224, #44662, #13648, #26344, #22213, #44362, #3915, #13055, #31054, #40224, #58235, #53814, #28092, #55556, #6248, #50854, #51146, #5960, #9817, #5665, #46431 ),
 .UNSPECIFIED., .F., .F.,
 ( 4, 2, 2, 2, 2, 2, 2, 2, 2, 2, 4 ),
 ( 0.3902582218033504580, 0.4664759440779315813, 0.5426936663525125937, 0.5808025274898032109, 0.6189113886270938281, 0.6951291109016750625, 0.7713468331762562968, 0.8475645554508375312, 0.8856734165881281484, 0.9237822777254187656, 1.000000000000000000 ),
 .UNSPECIFIED. ) ;
#42525 = VERTEX_POINT ( 'NONE', #12352 ) ;
#42526 = CARTESIAN_POINT ( 'NONE',  ( 10.12584611049472905, -76.13478022201745432, 4.748199717408892795 ) ) ;
#42527 = DIRECTION ( 'NONE',  ( 0.000000000000000000, -1.000000000000000000, 0.000000000000000000 ) ) ;
#42528 = CARTESIAN_POINT ( 'NONE',  ( -3.399395994687390399, -78.70000000000000284, -0.06408487577575257277 ) ) ;
#42529 = CARTESIAN_POINT ( 'NONE',  ( -11.56793956631425502, -77.42581400997612207, 4.165594241877493609 ) ) ;
#42530 = CARTESIAN_POINT ( 'NONE',  ( -0.007979420377872919676, -81.47602220864618516, 1.249669167965647532 ) ) ;
#42531 = CARTESIAN_POINT ( 'NONE',  ( 1.239259429943828650, -78.38146816523367022, -0.2975402487276854191 ) ) ;
#42532 = CARTESIAN_POINT ( 'NONE',  ( 10.14948852600999984, -59.55100835476999777, -7.674614791855999485 ) ) ;
#42533 = DIRECTION ( 'NONE',  ( 0.000000000000000000, -1.000000000000000000, 0.000000000000000000 ) ) ;
#42534 = ADVANCED_FACE ( 'NONE', ( #30049 ), #20922, .F. ) ;
#42535 = AXIS2_PLACEMENT_3D ( 'NONE', #50425, #49841, #36243 ) ;
#42536 = CARTESIAN_POINT ( 'NONE',  ( -1.293726968080000095, -79.06827490904998967, 0.1924304001467000147 ) ) ;
#42537 = CYLINDRICAL_SURFACE ( 'NONE', #18887, 9.000000000000000000 ) ;
#42538 = CARTESIAN_POINT ( 'NONE',  ( -0.1636246173744726473, -78.38541666666664298, 1.249999999999999112 ) ) ;
#42539 = CARTESIAN_POINT ( 'NONE',  ( 3.366547962069000199, -79.36254827890498120, -9.168809063548000182 ) ) ;
#42540 = ORIENTED_EDGE ( 'NONE', *, *, #25162, .T. ) ;
#42541 = VERTEX_POINT ( 'NONE', #11216 ) ;
#42542 = CARTESIAN_POINT ( 'NONE',  ( -9.500000000000000000, -77.89999999999999147, 0.000000000000000000 ) ) ;
#42543 = CARTESIAN_POINT ( 'NONE',  ( -1.085832016961150392, -78.71718408877019613, -10.71637321867290282 ) ) ;
#42544 = ORIENTED_EDGE ( 'NONE', *, *, #21338, .T. ) ;
#42545 = CARTESIAN_POINT ( 'NONE',  ( 7.658900723009000266, -18.79059707833999937, 10.01676258974000078 ) ) ;
#42546 = CARTESIAN_POINT ( 'NONE',  ( -9.037065544638657855, -79.37477492731599682, 2.928856757568816693 ) ) ;
#42547 = CARTESIAN_POINT ( 'NONE',  ( 11.96278553877000128, -79.09166473471999836, 1.542582301795999866 ) ) ;
#42548 = B_SPLINE_CURVE_WITH_KNOTS ( 'NONE', 3,
 ( #27136, #27433, #8854, #41026, #32147, #54610, #50187, #26844, #9732, #46059, #36001, #23309, #41316, #44873, #901, #18882, #32434, #36878 ),
 .UNSPECIFIED., .F., .F.,
 ( 4, 2, 2, 2, 2, 2, 2, 2, 4 ),
 ( 0.000000000000000000, 0.1250000000000000278, 0.2500000000000000555, 0.3750000000000001110, 0.5000000000000001110, 0.6250000000000001110, 0.7500000000000002220, 0.8750000000000001110, 1.000000000000000000 ),
 .UNSPECIFIED. ) ;
#42549 = CARTESIAN_POINT ( 'NONE',  ( 13.94827586207000003, -33.10361340872000113, 8.082385094115998871E-06 ) ) ;
#42550 = CARTESIAN_POINT ( 'NONE',  ( 0.000000000000000000, -23.15000000000000213, 11.79999999999999893 ) ) ;
#42551 = CARTESIAN_POINT ( 'NONE',  ( 1.199500263597268246, -79.80208333333334281, 0.9218200799623752495 ) ) ;
#42552 = CARTESIAN_POINT ( 'NONE',  ( -1.780884232981000181, -80.01399474955769620, -11.07459082487999957 ) ) ;
#42553 = ORIENTED_EDGE ( 'NONE', *, *, #41443, .F. ) ;
#42554 = CARTESIAN_POINT ( 'NONE',  ( 12.00000000000000000, -79.14999999999999147, 0.000000000000000000 ) ) ;
#42555 = AXIS2_PLACEMENT_3D ( 'NONE', #48844, #8389, #3958 ) ;
#42556 = ORIENTED_EDGE ( 'NONE', *, *, #50594, .T. ) ;
#42557 = CARTESIAN_POINT ( 'NONE',  ( 9.184859914837900874, -77.35958091549174753, 1.096818293188132065 ) ) ;
#42558 = CARTESIAN_POINT ( 'NONE',  ( 12.52582323437067124, -60.60939730725227292, -1.680974276192610972 ) ) ;
#42559 = CARTESIAN_POINT ( 'NONE',  ( 11.69999999991999928, -75.99999999992400035, 2.424609313239000216E-09 ) ) ;
#42560 = UNCERTAINTY_MEASURE_WITH_UNIT (LENGTH_MEASURE( 1.000000000000000082E-05 ), #602, 'distance_accuracy_value', 'NONE');
#42561 = CARTESIAN_POINT ( 'NONE',  ( 0.1747633057891999908, -77.85831261029910877, 1.605201443249000048 ) ) ;
#42562 = CARTESIAN_POINT ( 'NONE',  ( 11.82469666049999901, -76.02329627867000283, 4.496655510765000585 ) ) ;
#42563 = DIRECTION ( 'NONE',  ( -0.9859154929577472748, 0.1672442547470080754, 0.000000000000000000 ) ) ;
#42564 = CARTESIAN_POINT ( 'NONE',  ( 1.621809933883000099, -78.58624769700999479, 0.1356303529659999840 ) ) ;
#42565 = CARTESIAN_POINT ( 'NONE',  ( -7.705119999441000012, -20.24828923609000242, 10.24996238031000040 ) ) ;
#42566 = CARTESIAN_POINT ( 'NONE',  ( 4.665505440478000310, -78.83337134055398110, 10.01553556391000122 ) ) ;
#42567 = EDGE_CURVE ( 'NONE', #30430, #8440, #5567, .T. ) ;
#42568 = CARTESIAN_POINT ( 'NONE',  ( 7.710118476736999682, -57.05022860539000362, 10.18499221088999995 ) ) ;
#42569 = DIRECTION ( 'NONE',  ( 0.000000000000000000, 1.000000000000000000, 0.000000000000000000 ) ) ;
#42570 = FILL_AREA_STYLE ('',( #29547 ) ) ;
#42571 = CARTESIAN_POINT ( 'NONE',  ( -0.6683986366931999878, -84.38281177079799988, 3.483505843786999900 ) ) ;
#42572 = ORIENTED_EDGE ( 'NONE', *, *, #23059, .F. ) ;
#42573 = EDGE_CURVE ( 'NONE', #800, #42344, #31586, .T. ) ;
#42574 = CARTESIAN_POINT ( 'NONE',  ( -12.00000000000000000, -79.39999999999999147, 0.000000000000000000 ) ) ;
#42575 = VECTOR ( 'NONE', #56421, 1000.000000000000114 ) ;
#42576 = CARTESIAN_POINT ( 'NONE',  ( -0.9103895169571000201, -79.40443682768999167, -1.233764334031000054 ) ) ;
#42577 = CARTESIAN_POINT ( 'NONE',  ( -1.247385801080000078, -24.47722256257000240, -12.50301438876999960 ) ) ;
#42578 = CARTESIAN_POINT ( 'NONE',  ( 0.3864029911681999829, -77.26151168242199674, -11.74364478040999948 ) ) ;
#42579 = CARTESIAN_POINT ( 'NONE',  ( -8.666925696261760237, -53.80708316137260994, 9.019429295859271889 ) ) ;
#42580 = CARTESIAN_POINT ( 'NONE',  ( 0.8554194063300312179, -78.43396144911410772, -0.9449817633163264397 ) ) ;
#42581 = CARTESIAN_POINT ( 'NONE',  ( -2.105625082083603328, -2.323927937926350662, -2.820318438645454950 ) ) ;
#42582 = CARTESIAN_POINT ( 'NONE',  ( 9.571814930552291045, -80.88775658398785140, 4.892930331445250580 ) ) ;
#42583 = CARTESIAN_POINT ( 'NONE',  ( 4.996366032364999654, -78.47410532222798452, 8.105967104710000370 ) ) ;
#42584 = CARTESIAN_POINT ( 'NONE',  ( -10.69099419661866612, -76.59160594794379051, 1.136506249403649749 ) ) ;
#42585 = CARTESIAN_POINT ( 'NONE',  ( 3.906270390259000358, -78.68071061401199984, -10.19392449069000151 ) ) ;
#42586 = CYLINDRICAL_SURFACE ( 'NONE', #22417, 1.250000000000000000 ) ;
#42587 = CARTESIAN_POINT ( 'NONE',  ( 7.244718558131000741, -80.34293552609639733, 7.973405301998999661 ) ) ;
#42588 = CARTESIAN_POINT ( 'NONE',  ( 0.03026270826137486547, -82.02290750955010878, 1.273738630170636599 ) ) ;
#42589 = EDGE_LOOP ( 'NONE', ( #39313, #42107, #26451, #50210 ) ) ;
#42590 = CARTESIAN_POINT ( 'NONE',  ( 1.221474390223999951, -81.48279142430399702, -0.5353283698298000326 ) ) ;
#42591 = CARTESIAN_POINT ( 'NONE',  ( 0.000000000000000000, -60.04999999966999980, 12.50000000000000000 ) ) ;
#42592 = CARTESIAN_POINT ( 'NONE',  ( -0.4356486348705999601, -61.68064955776999625, -12.43591427125000060 ) ) ;
#42593 = EDGE_CURVE ( 'NONE', #10368, #10966, #12069, .T. ) ;
#42594 = CARTESIAN_POINT ( 'NONE',  ( -7.345153731672206199, -55.57158755757922108, 8.188331488387630586 ) ) ;
#42595 = CARTESIAN_POINT ( 'NONE',  ( 11.08595418830999968, -77.00393590465999694, -1.708721840212999998 ) ) ;
#42596 = CARTESIAN_POINT ( 'NONE',  ( -10.81649518602000093, -79.35628189776099362, 1.862108609190000097 ) ) ;
#42597 = CARTESIAN_POINT ( 'NONE',  ( 10.19022265128000093, -23.19634105642999700, -7.646946115745000050 ) ) ;
#42598 = CARTESIAN_POINT ( 'NONE',  ( 1.197295183284138975, -85.75312501589537817, 3.856364711603536222 ) ) ;
#42599 = CARTESIAN_POINT ( 'NONE',  ( -7.698110069955000689, -77.07989279640000291, -9.554382370588998086 ) ) ;
#42600 = CARTESIAN_POINT ( 'NONE',  ( 6.069819744066555778, -78.53115937559208248, 10.06047354936908178 ) ) ;
#42601 = DIRECTION ( 'NONE',  ( -0.7071067811865475727, 0.000000000000000000, -0.7071067811865475727 ) ) ;
#42602 = ORIENTED_EDGE ( 'NONE', *, *, #28766, .T. ) ;
#42603 = CARTESIAN_POINT ( 'NONE',  ( -1.157298774452520496, -80.06939412680100077, 0.4720562922803016592 ) ) ;
#42604 = CARTESIAN_POINT ( 'NONE',  ( -2.421167930323352646, -78.10416666666665719, -9.009247259181913492 ) ) ;
#42605 = CARTESIAN_POINT ( 'NONE',  ( 7.981651535783000462, -54.08135615453999634, -10.08154952393999970 ) ) ;
#42606 = CARTESIAN_POINT ( 'NONE',  ( 9.951586773259000651, -79.39035858408298907, -5.281558014135000256 ) ) ;
#42607 = CARTESIAN_POINT ( 'NONE',  ( -10.39929541389761702, -79.15104165712787676, -5.992801102062716545 ) ) ;
#42608 = FACE_BOUND ( 'NONE', #18735, .T. ) ;
#42609 = DIRECTION ( 'NONE',  ( 0.000000000000000000, -1.000000000000000000, 0.000000000000000000 ) ) ;
#42610 = CARTESIAN_POINT ( 'NONE',  ( -1.539734144441496699, -82.35743973534117401, -0.1659400480913056364 ) ) ;
#42611 = CARTESIAN_POINT ( 'NONE',  ( -1.151101085867609397, -79.63220894243453074, -0.4868159640311818803 ) ) ;
#42612 = CARTESIAN_POINT ( 'NONE',  ( -8.114915067887620737, -53.97115967817116200, 9.847905526091571105 ) ) ;
#42613 = ORIENTED_EDGE ( 'NONE', *, *, #21764, .T. ) ;
#42614 = CARTESIAN_POINT ( 'NONE',  ( 0.01697733933020722369, -81.72664603025980057, -1.249565628801712291 ) ) ;
#42615 = DIRECTION ( 'NONE',  ( 0.000000000000000000, 1.000000000000000000, 0.000000000000000000 ) ) ;
#42616 = EDGE_LOOP ( 'NONE', ( #7367, #23786, #12425, #36573 ) ) ;
#42617 = EDGE_LOOP ( 'NONE', ( #3902, #49880, #14929, #30180, #22405, #23850, #18141, #30816, #35989, #51052 ) ) ;
#42618 = CARTESIAN_POINT ( 'NONE',  ( -0.7401269933634999632, -81.46289504759600675, 1.323311824859999986 ) ) ;
#42619 = ORIENTED_EDGE ( 'NONE', *, *, #11855, .F. ) ;
#42620 = CARTESIAN_POINT ( 'NONE',  ( 9.499941120207004985, -79.99343229508609454, -0.7840560289833928831 ) ) ;
#42622 = EDGE_CURVE ( 'NONE', #39417, #26558, #56941, .T. ) ;
#42621 = VERTEX_POINT ( 'NONE', #24781 ) ;
#42623 = TOROIDAL_SURFACE ( 'NONE', #36915, 1.250000000000000000, 0.5000000000000000000 ) ;
#42624 = CARTESIAN_POINT ( 'NONE',  ( 1.890224871707000043, -18.25210751985000002, 12.68696160873999901 ) ) ;
#42625 = CARTESIAN_POINT ( 'NONE',  ( 0.5999999998848000171, -18.85000000520999919, -11.79999999988000070 ) ) ;
#42626 = DIRECTION ( 'NONE',  ( 1.000000000000000000, 0.000000000000000000, 0.000000000000000000 ) ) ;
#42627 = CARTESIAN_POINT ( 'NONE',  ( -13.63885489310999510, -59.58578169018998949, -7.254376133916000668 ) ) ;
#42628 = CARTESIAN_POINT ( 'NONE',  ( -3.063214743671000218, -79.29281332859899578, -9.307899183505000451 ) ) ;
#42629 = CARTESIAN_POINT ( 'NONE',  ( 7.910349975595998728, -79.51102931670899920, 7.952639426948999279 ) ) ;
#42630 = ORIENTED_EDGE ( 'NONE', *, *, #30277, .F. ) ;
#42631 = ORIENTED_EDGE ( 'NONE', *, *, #27677, .F. ) ;
#42632 = CARTESIAN_POINT ( 'NONE',  ( -9.150401306387172085, -77.58846111580191973, 1.353620980104426996 ) ) ;
#42633 = PLANE ( 'NONE',  #46135 ) ;
#42634 = CARTESIAN_POINT ( 'NONE',  ( 0.000000000000000000, -75.15999999999999659, 0.000000000000000000 ) ) ;
#42635 = CARTESIAN_POINT ( 'NONE',  ( -7.707166124622999881, -77.26151649330898863, -5.896629607976000109 ) ) ;
#42636 = CARTESIAN_POINT ( 'NONE',  ( 0.000000000000000000, 4.040000000000000036, 0.000000000000000000 ) ) ;
#42637 = CARTESIAN_POINT ( 'NONE',  ( 1.092232985442820992, -79.79166666666665719, 0.6295237254636267821 ) ) ;
#42638 = CARTESIAN_POINT ( 'NONE',  ( -9.404538367151719314, -77.35366911081999319, -7.521839627126677641 ) ) ;
#42639 = CARTESIAN_POINT ( 'NONE',  ( -0.7205381521189000438, -80.86020805664000477, -1.542932836074000003 ) ) ;
#42640 = FACE_BOUND ( 'NONE', #15865, .T. ) ;
#42641 = CARTESIAN_POINT ( 'NONE',  ( -9.734541936978917676, -76.65229327790524394, 6.579934271495913478 ) ) ;
#42642 = ADVANCED_FACE ( 'NONE', ( #34482, #51669 ), #38924, .F. ) ;
#42643 = CARTESIAN_POINT ( 'NONE',  ( 3.494359274950000316, -79.56916961237898533, 2.279475529283999879 ) ) ;
#42644 = CARTESIAN_POINT ( 'NONE',  ( -0.02850738685234475642, -79.62644246643365875, 1.511250209800697908 ) ) ;
#42645 = CARTESIAN_POINT ( 'NONE',  ( 9.557721383756000222, -78.17181332859900067, -2.621152531184999912 ) ) ;
#42646 = CARTESIAN_POINT ( 'NONE',  ( -9.484300247301399978, -80.30416666667800030, -5.483079476845273525 ) ) ;
#42647 = LINE ( 'NONE', #2781, #24017 ) ;
#42649 = CARTESIAN_POINT ( 'NONE',  ( 1.288488638074000159, -17.46435060632000003, -12.54709296483000003 ) ) ;
#42648 = CARTESIAN_POINT ( 'NONE',  ( -0.1963495408493673156, -78.78541666666669130, 1.499999999999999556 ) ) ;
#42650 = CARTESIAN_POINT ( 'NONE',  ( 12.00000000000000000, -78.14999999999999147, 0.000000000000000000 ) ) ;
#42651 = CARTESIAN_POINT ( 'NONE',  ( -8.839214553731000734, -80.04551656954198791, -6.848292123026999967 ) ) ;
#42652 = CARTESIAN_POINT ( 'NONE',  ( 3.938171349113054998, -79.27666666666658557, -8.369041066855391620 ) ) ;
#42653 = CARTESIAN_POINT ( 'NONE',  ( 3.110769248615221194, -0.9610483397592147758, -1.653932746071141935 ) ) ;
#42654 = ORIENTED_EDGE ( 'NONE', *, *, #26031, .T. ) ;
#42655 = DIRECTION ( 'NONE',  ( 0.7071067812094172789, -2.924114041541070768E-07, 0.7071067811636172484 ) ) ;
#42656 = CARTESIAN_POINT ( 'NONE',  ( 10.12290050124000018, -18.75000000007999645, -7.648026767085999822 ) ) ;
#42657 = CARTESIAN_POINT ( 'NONE',  ( -0.001748811790489142098, -78.47533359273272424, 1.249867168124328298 ) ) ;
#42658 = EDGE_CURVE ( 'NONE', #43048, #36029, #24613, .T. ) ;
#42659 = CARTESIAN_POINT ( 'NONE',  ( 9.474537194627000503, -79.71580382909299090, 1.059975283156000092 ) ) ;
#42660 = CARTESIAN_POINT ( 'NONE',  ( -3.274010471232999819, -77.34323873689000095, 12.59444704299999884 ) ) ;
#42661 = CARTESIAN_POINT ( 'NONE',  ( 1.807051837523000026, -61.10078415209999747, 12.77977401837999949 ) ) ;
#42662 = CARTESIAN_POINT ( 'NONE',  ( -0.2079424137668072214, -79.47668210426643043, 10.74817616777493079 ) ) ;
#42663 = CARTESIAN_POINT ( 'NONE',  ( -8.916572348234000245, -79.34443998579800450, 4.182142589683000011 ) ) ;
#42664 = CARTESIAN_POINT ( 'NONE',  ( -12.50000000000000000, -55.55000000209000177, -1.750000000000000000 ) ) ;
#42665 = VECTOR ( 'NONE', #34543, 1000.000000000000000 ) ;
#42666 = CARTESIAN_POINT ( 'NONE',  ( 9.146564807811000009, -77.57451461849198893, -6.016234306896000028 ) ) ;
#42667 = CARTESIAN_POINT ( 'NONE',  ( -4.528061651730656223, -76.29306646779448897, -10.84218088047703965 ) ) ;
#42668 = CARTESIAN_POINT ( 'NONE',  ( 0.6676470363431000754, -82.24889682832498750, 1.458559589245999932 ) ) ;
#42669 = CARTESIAN_POINT ( 'NONE',  ( -5.600962501325999376, -78.07384514476065362, 7.948110234177999445 ) ) ;
#42670 = CARTESIAN_POINT ( 'NONE',  ( -6.563619111649000359, -78.08441341731199259, -6.747599474233999750 ) ) ;
#42672 = CARTESIAN_POINT ( 'NONE',  ( 0.4254240051736068451, -2.864583333333333925, 3.250000000000001776 ) ) ;
#42671 = CARTESIAN_POINT ( 'NONE',  ( -3.776522694978999617, -85.86929758755698572, 0.4127208475760000272 ) ) ;
#42673 = CARTESIAN_POINT ( 'NONE',  ( -6.090475762158000350, -79.62015584965399739, 7.362120511650999788 ) ) ;
#42674 = CARTESIAN_POINT ( 'NONE',  ( -0.9995835529977249445, -82.55208333333330017, -0.7681833999686439318 ) ) ;
#42675 = CARTESIAN_POINT ( 'NONE',  ( 9.169614940969610828, -80.30620290186523391, -5.640497885845999981 ) ) ;
#42676 = DIRECTION ( 'NONE',  ( 1.000000000000000000, 0.000000000000000000, 0.000000000000000000 ) ) ;
#42677 = CARTESIAN_POINT ( 'NONE',  ( 2.486604901413133728, -77.25416666666667709, 9.252740428349007118 ) ) ;
#42678 = ADVANCED_BREP_SHAPE_REPRESENTATION ( '', ( #55564, #43526 ), #9600 ) ;
#42679 = ORIENTED_EDGE ( 'NONE', *, *, #4113, .F. ) ;
#42680 = VECTOR ( 'NONE', #56658, 1000.000000000000114 ) ;
#42681 = CARTESIAN_POINT ( 'NONE',  ( -0.9103933733443999587, -79.68507749579998745, -11.99492895764000089 ) ) ;
#42682 = DIRECTION ( 'NONE',  ( -0.7071067811865475727, 0.000000000000000000, 0.7071067811865475727 ) ) ;
#42683 = CARTESIAN_POINT ( 'NONE',  ( -10.14999999998000035, -87.10000000002298748, 2.878919856867000406E-10 ) ) ;
#42684 = ORIENTED_EDGE ( 'NONE', *, *, #22726, .F. ) ;
#42685 = CARTESIAN_POINT ( 'NONE',  ( -5.241653689492999924, -77.71222517136899910, -10.72196665943000049 ) ) ;
#42686 = VERTEX_POINT ( 'NONE', #47902 ) ;
#42688 = EDGE_CURVE ( 'NONE', #11684, #18435, #45748, .T. ) ;
#42687 = EDGE_LOOP ( 'NONE', ( #56754, #26231, #17395, #33743 ) ) ;
#42689 = CARTESIAN_POINT ( 'NONE',  ( 1.407171709420391936, -78.86458333333331439, 10.75000000000000178 ) ) ;
#42690 = ORIENTED_EDGE ( 'NONE', *, *, #42368, .T. ) ;
#42691 = ADVANCED_FACE ( 'NONE', ( #13589 ), #13296, .T. ) ;
#42692 = CARTESIAN_POINT ( 'NONE',  ( -2.658558477971000311, -81.85392767752199461, -2.348749639193000061 ) ) ;
#42693 = CARTESIAN_POINT ( 'NONE',  ( 5.930197972290384811, -79.22128088774034893, 7.423945719049496184 ) ) ;
#42694 = EDGE_LOOP ( 'NONE', ( #27312, #50515, #37296 ) ) ;
#42695 = CARTESIAN_POINT ( 'NONE',  ( 0.7046260488188935689, -82.77294570575585908, -1.032333493006673653 ) ) ;
#42696 = ORIENTED_EDGE ( 'NONE', *, *, #23897, .T. ) ;
#42697 = CARTESIAN_POINT ( 'NONE',  ( 7.919595949288999570, -55.64999999965999677, -8.768124086712999699 ) ) ;
#42698 = ORIENTED_EDGE ( 'NONE', *, *, #32191, .F. ) ;
#42699 = DIRECTION ( 'NONE',  ( 0.000000000000000000, 0.000000000000000000, 1.000000000000000000 ) ) ;
#42700 = CARTESIAN_POINT ( 'NONE',  ( 0.9175530224387180578, -78.92634932198247100, -1.226298970086918905 ) ) ;
#42701 = AXIS2_PLACEMENT_3D ( 'NONE', #5240, #50714, #46288 ) ;
#42702 = CARTESIAN_POINT ( 'NONE',  ( -2.902572068143752571, -79.79999999999998295, -11.46568512432220643 ) ) ;
#42703 = DIRECTION ( 'NONE',  ( 0.000000000000000000, -1.000000000000000000, 0.000000000000000000 ) ) ;
#42704 = CARTESIAN_POINT ( 'NONE',  ( -3.079437091258620196, -86.09999999999995168, 1.441203386403855591 ) ) ;
#42705 = CARTESIAN_POINT ( 'NONE',  ( -5.279550234765999939, -76.48755886051600328, -9.859017853534000508 ) ) ;
#42706 = CARTESIAN_POINT ( 'NONE',  ( -2.378576911058957855, -76.49343170455809116, 10.59748283465861363 ) ) ;
#42707 = CARTESIAN_POINT ( 'NONE',  ( 0.7445603198294054037, -81.18334426506562806, 1.317420973437698484 ) ) ;
#42708 = VECTOR ( 'NONE', #33595, 1000.000000000000000 ) ;
#42709 = DIRECTION ( 'NONE',  ( 1.000000000000000000, 0.000000000000000000, 0.000000000000000000 ) ) ;
#42710 = CARTESIAN_POINT ( 'NONE',  ( 9.815664359364999925, -76.03305630414600103, -5.453095817054999905 ) ) ;
#42711 = CARTESIAN_POINT ( 'NONE',  ( -2.417559983778709842, -78.70412069868730498, -8.933467346123652675 ) ) ;
#42712 = ADVANCED_FACE ( 'NONE', ( #40164 ), #44900, .F. ) ;
#42713 = CARTESIAN_POINT ( 'NONE',  ( 1.323534079420999987, -79.91831375464900589, -0.1638099207045999872 ) ) ;
#42714 = CARTESIAN_POINT ( 'NONE',  ( -7.958763980599000476, -17.52301961032999955, -9.723170659105999647 ) ) ;
#42715 = CARTESIAN_POINT ( 'NONE',  ( -9.500000000000007105, -77.28958333333333997, 1.243547092045919733 ) ) ;
#42716 = CARTESIAN_POINT ( 'NONE',  ( -1.357221183918999818, -78.68203455456848872, -3.502749927983000333 ) ) ;
#42717 = CARTESIAN_POINT ( 'NONE',  ( 12.19481035159000015, -79.75646030464399416, -0.3683939141165000208 ) ) ;
#42718 = VECTOR ( 'NONE', #26787, 999.9999999999998863 ) ;
#42719 = CARTESIAN_POINT ( 'NONE',  ( -9.939585253895419470, -78.06897173951264790, 4.094651989779796608 ) ) ;
#42720 = CARTESIAN_POINT ( 'NONE',  ( 0.8801428981091761194, -82.91344897987683282, 0.8870736079473547919 ) ) ;
#42721 = DIRECTION ( 'NONE',  ( 0.000000000000000000, -1.000000000000000000, 9.099419098363000178E-12 ) ) ;
#42722 = CARTESIAN_POINT ( 'NONE',  ( 12.50745077490000057, -17.00005551713000074, -2.011911479242000131E-09 ) ) ;
#42723 = VECTOR ( 'NONE', #37717, 1000.000000000000000 ) ;
#42724 = DIRECTION ( 'NONE',  ( -1.147010004338000229E-14, 0.000000000000000000, 1.000000000000000000 ) ) ;
#42725 = FACE_OUTER_BOUND ( 'NONE', #44481, .T. ) ;
#42726 = ADVANCED_FACE ( 'NONE', ( #53759 ), #8879, .T. ) ;
#42727 = CARTESIAN_POINT ( 'NONE',  ( 10.01332852690999964, -60.08056535122999975, 7.654537165486999584 ) ) ;
#42729 = EDGE_CURVE ( 'NONE', #20675, #26186, #4747, .T. ) ;
#42728 = CARTESIAN_POINT ( 'NONE',  ( -1.417334032777999964, -79.02654225787900089, -0.4910847579886000736 ) ) ;
#42730 = CARTESIAN_POINT ( 'NONE',  ( -8.266617305338565203, -24.97234527442468632, -9.697375114818715502 ) ) ;
#42731 = B_SPLINE_CURVE_WITH_KNOTS ( 'NONE', 3,
 ( #43236, #47970, #52669, #7507, #38508, #6926 ),
 .UNSPECIFIED., .F., .F.,
 ( 4, 2, 4 ),
 ( 0.000000000000000000, 0.5000000000000000000, 1.000000000000000000 ),
 .UNSPECIFIED. ) ;
#42732 = CARTESIAN_POINT ( 'NONE',  ( 10.83790964778171073, -77.70003328245064722, -0.06560966762940606545 ) ) ;
#42733 = SURFACE_STYLE_USAGE ( .BOTH. , #47179 ) ;
#42734 = CARTESIAN_POINT ( 'NONE',  ( -1.980611416588520024, -23.52597731804367953, -12.74335092663162250 ) ) ;
#42735 = CARTESIAN_POINT ( 'NONE',  ( 8.351130818052999061, -75.94147849534999750, -8.703251827980000854 ) ) ;
#42736 = EDGE_LOOP ( 'NONE', ( #9059, #8407, #22903, #11321 ) ) ;
#42737 = CARTESIAN_POINT ( 'NONE',  ( 3.840625598965000442, -84.31421544543098889, 0.9775355813133997929 ) ) ;
#42738 = CARTESIAN_POINT ( 'NONE',  ( 3.184161977317999881, -85.88547957940599531, -1.417680250971000033 ) ) ;
#42739 = CARTESIAN_POINT ( 'NONE',  ( 8.953311532445939136, -78.32993639350726767, -2.326867093362477323 ) ) ;
#42740 = DIRECTION ( 'NONE',  ( -1.000000000000000000, 0.000000000000000000, -3.332495962870000189E-11 ) ) ;
#42741 = CARTESIAN_POINT ( 'NONE',  ( 5.263131812197999970, -78.06554867327399450, -9.905430536777000583 ) ) ;
#42742 = CARTESIAN_POINT ( 'NONE',  ( 12.55485633992000061, -54.64594908747999824, -1.580761757393000178 ) ) ;
#42743 = CARTESIAN_POINT ( 'NONE',  ( -7.872620573787999732, -77.77909087844599867, 5.734242845189999827 ) ) ;
#42744 = VECTOR ( 'NONE', #3854, 1000.000000000000114 ) ;
#42745 = CARTESIAN_POINT ( 'NONE',  ( 3.471918836458000257, -82.34482020574199623, -1.985174022353000334 ) ) ;
#42746 = CARTESIAN_POINT ( 'NONE',  ( -1.392423410630999929E-14, -75.80000000000001137, 0.000000000000000000 ) ) ;
#42747 = CARTESIAN_POINT ( 'NONE',  ( 0.3742884389835000047, -79.19216343900099275, -1.469294133937999902 ) ) ;
#42748 = EDGE_LOOP ( 'NONE', ( #5466, #26388, #43418, #6592 ) ) ;
#42749 = ADVANCED_FACE ( 'NONE', ( #30998 ), #50146, .F. ) ;
#42750 = CARTESIAN_POINT ( 'NONE',  ( 0.000000000000000000, -75.67500000000001137, 0.000000000000000000 ) ) ;
#42751 = ORIENTED_EDGE ( 'NONE', *, *, #29293, .F. ) ;
#42752 = CARTESIAN_POINT ( 'NONE',  ( -1.327706488546999797, -79.14179945328800159, -0.1249263990498000187 ) ) ;
#42753 = CIRCLE ( 'NONE', #52191, 6.100000000000000533 ) ;
#42754 = CARTESIAN_POINT ( 'NONE',  ( 12.75761570869000039, -59.57819125629999490, 1.931043762602999925 ) ) ;
#42755 = CARTESIAN_POINT ( 'NONE',  ( 0.4031446930405725992, -80.75178943763351924, -1.187466692091743159 ) ) ;
#42756 = ORIENTED_EDGE ( 'NONE', *, *, #41284, .T. ) ;
#42757 = CARTESIAN_POINT ( 'NONE',  ( 11.38106369370999893, -78.03758450816098957, 4.295802577524999499 ) ) ;
#42758 = CARTESIAN_POINT ( 'NONE',  ( 9.248082609065999549, -77.75800271236998640, -6.531860890005000364 ) ) ;
#42759 = ORIENTED_EDGE ( 'NONE', *, *, #25360, .T. ) ;
#42760 = VERTEX_POINT ( 'NONE', #37193 ) ;
#42762 = ADVANCED_FACE ( 'NONE', ( #29489 ), #2082, .F. ) ;
#42761 = ORIENTED_EDGE ( 'NONE', *, *, #33179, .F. ) ;
#42763 = VECTOR ( 'NONE', #27669, 1000.000000000000000 ) ;
#42764 = CARTESIAN_POINT ( 'NONE',  ( -0.7013479997696390189, -80.52279179898042116, 1.035593156588225039 ) ) ;
#42765 = EDGE_CURVE ( 'NONE', #12597, #54609, #8387, .T. ) ;
#42766 = VECTOR ( 'NONE', #58407, 1000.000000000000000 ) ;
#42767 = CARTESIAN_POINT ( 'NONE',  ( -1.267348307942000041, -77.24373998579798695, -9.458036467157000970 ) ) ;
#42768 = CARTESIAN_POINT ( 'NONE',  ( -4.465297566879000257, -80.16279685233251939, 8.686876450551999085 ) ) ;
#42769 = ORIENTED_EDGE ( 'NONE', *, *, #4555, .F. ) ;
#42770 = CARTESIAN_POINT ( 'NONE',  ( 5.592013246121999792, -78.40561320193899064, 9.375753510130000024 ) ) ;
#42771 = VERTEX_POINT ( 'NONE', #46960 ) ;
#42772 = CARTESIAN_POINT ( 'NONE',  ( 1.407328957790502599, -80.73545652690489760, -10.68057248400399928 ) ) ;
#42773 = CARTESIAN_POINT ( 'NONE',  ( 7.092659876394000307, -77.81771915034599374, 6.312768414564000174 ) ) ;
#42774 = CARTESIAN_POINT ( 'NONE',  ( 9.841113773978118928, -17.16371975942079686, -8.121706172286355496 ) ) ;
#42775 = CARTESIAN_POINT ( 'NONE',  ( -1.460959015002474493, -81.37916666666664867, 0.3926218265389144757 ) ) ;
#42776 = CARTESIAN_POINT ( 'NONE',  ( -9.250000000000000000, -77.99999999999998579, 0.000000000000000000 ) ) ;
#42777 = CARTESIAN_POINT ( 'NONE',  ( -12.70455814334985511, -17.43992875973548706, -1.489882837223169387 ) ) ;
#42778 = FACE_OUTER_BOUND ( 'NONE', #29835, .T. ) ;
#42779 = CARTESIAN_POINT ( 'NONE',  ( 6.760013919724077169, -79.77708333333333712, -8.796335266379973206 ) ) ;
#42780 = CARTESIAN_POINT ( 'NONE',  ( -7.647735717248999698, -23.72294882383999948, 10.13404777202000062 ) ) ;
#42781 = CARTESIAN_POINT ( 'NONE',  ( -1.583750823903000038, -80.89244764574600310, 0.3147260902806000016 ) ) ;
#42782 = CARTESIAN_POINT ( 'NONE',  ( 2.421167930323313566, -77.85416666666664298, 9.009247259181924150 ) ) ;
#42783 = DIRECTION ( 'NONE',  ( 0.9999999924279685537, 0.000000000000000000, 0.0001230612157848962919 ) ) ;
#42784 = CARTESIAN_POINT ( 'NONE',  ( 3.086017585447000222, -79.09324228728000605, -11.86910201801999953 ) ) ;
#42785 = CARTESIAN_POINT ( 'NONE',  ( 1.298131932841000147, -76.50046698964798964, 12.21218573294999921 ) ) ;
#42786 = CARTESIAN_POINT ( 'NONE',  ( -8.300970689365467337, -78.85833333333332007, 4.784380313523513450 ) ) ;
#42787 = CARTESIAN_POINT ( 'NONE',  ( -9.188080731290124703, -77.99423656384304593, 7.746760052061067547 ) ) ;
#42788 = CARTESIAN_POINT ( 'NONE',  ( 6.043427764450807871, -77.96666666666668277, -10.48543666025108934 ) ) ;
#42789 = AXIS2_PLACEMENT_3D ( 'NONE', #31225, #3797, #4088 ) ;
#42790 = ORIENTED_EDGE ( 'NONE', *, *, #7357, .F. ) ;
#42791 = CARTESIAN_POINT ( 'NONE',  ( 1.465719397218613329, -79.98070088451875392, -0.3642262430507383630 ) ) ;
#42792 = CARTESIAN_POINT ( 'NONE',  ( 5.917523019358082337, -77.96666666666666856, -10.26699006316252394 ) ) ;
#42793 = CARTESIAN_POINT ( 'NONE',  ( 1.217465845835393967, -79.27083333333330017, 0.3271848554491025851 ) ) ;
#42794 = B_SPLINE_CURVE_WITH_KNOTS ( 'NONE', 3,
 ( #36597, #54897, #10623, #24189, #19767, #28604, #5018, #28021, #54619, #37764, #14157, #27729, #49907, #46651, #10327, #6178 ),
 .UNSPECIFIED., .F., .F.,
 ( 4, 2, 2, 2, 2, 2, 2, 4 ),
 ( 0.000000000000000000, 0.2499999999999970024, 0.3749999999999955036, 0.4999999999999940048, 0.6249999999999924505, 0.6874999999999932276, 0.7499999999999938938, 1.000000000000000000 ),
 .UNSPECIFIED. ) ;
#42795 = CARTESIAN_POINT ( 'NONE',  ( 10.00716890277181292, -78.69696047196750044, 6.699252482690747357 ) ) ;
#42796 = CARTESIAN_POINT ( 'NONE',  ( 0.5559119596479000780, -3.157909330902999745, 3.830311516254000015 ) ) ;
#42797 = VECTOR ( 'NONE', #18177, 1000.000000000000227 ) ;
#42798 = CARTESIAN_POINT ( 'NONE',  ( -12.14750708673999924, -77.93689196713800982, 0.6485384821269000177 ) ) ;
#42799 = CARTESIAN_POINT ( 'NONE',  ( -7.872620573787999732, -77.72071810079599175, 5.734242845189999827 ) ) ;
#42801 = DIRECTION ( 'NONE',  ( 1.000000000000000000, 0.000000000000000000, 0.000000000000000000 ) ) ;
#42800 = CARTESIAN_POINT ( 'NONE',  ( -1.136237469166809122, -76.08235068074559138, 11.70153850263246298 ) ) ;
#42802 = CARTESIAN_POINT ( 'NONE',  ( 5.708176239699000121, -78.69537633716700498, -9.305495801267001710 ) ) ;
#42803 = CARTESIAN_POINT ( 'NONE',  ( -10.16542146597221041, -79.57365022831298518, 3.500767233281877555 ) ) ;
#42804 = ORIENTED_EDGE ( 'NONE', *, *, #28150, .T. ) ;
#42805 = CARTESIAN_POINT ( 'NONE',  ( -6.024415200220997413, -76.46569630464409784, 10.73507988388000101 ) ) ;
#42806 = CARTESIAN_POINT ( 'NONE',  ( 1.155251330895799677, -79.11532408967735819, 9.449995398207709840 ) ) ;
#42807 = FACE_OUTER_BOUND ( 'NONE', #31812, .T. ) ;
#42808 = CARTESIAN_POINT ( 'NONE',  ( -7.961052042476000068, -61.33567434991999789, 9.783216378940000624 ) ) ;
#42809 = DIRECTION ( 'NONE',  ( -8.423171624505000574E-11, 1.000000000000000000, 1.870145497457000051E-10 ) ) ;
#42810 = CARTESIAN_POINT ( 'NONE',  ( 8.486433606932997975, -79.36725937275299714, 4.401307641916000435 ) ) ;
#42811 = CARTESIAN_POINT ( 'NONE',  ( -9.596002108778160178, -77.95208333333332007, -7.374560639698984232 ) ) ;
#42812 = CARTESIAN_POINT ( 'NONE',  ( 1.210822168571075386, -79.13541666666664298, -9.249999999999996447 ) ) ;
#42813 = ORIENTED_EDGE ( 'NONE', *, *, #43305, .F. ) ;
#42814 = CARTESIAN_POINT ( 'NONE',  ( 7.634645133843636522, -23.47584427336935775, -10.10912661252998923 ) ) ;
#42815 = CARTESIAN_POINT ( 'NONE',  ( -0.5111749199061261795, -78.92796920241946168, 11.82469092913801489 ) ) ;
#42816 = CARTESIAN_POINT ( 'NONE',  ( -13.94827586207000003, -45.69638659094999866, -8.082388077679998639E-06 ) ) ;
#42817 = ADVANCED_FACE ( 'NONE', ( #52520 ), #43638, .T. ) ;
#42818 = CARTESIAN_POINT ( 'NONE',  ( 0.4720932691372294321, -81.44439364009578242, 1.157282337904234737 ) ) ;
#42819 = EDGE_CURVE ( 'NONE', #5899, #55147, #22863, .T. ) ;
#42820 = TOROIDAL_SURFACE ( 'NONE', #47562, 1.250000000000000000, 0.5000000000000000000 ) ;
#42821 = CARTESIAN_POINT ( 'NONE',  ( 1.224222772991306885, -78.92211854823271722, 0.3526872050934898861 ) ) ;
#42822 = CARTESIAN_POINT ( 'NONE',  ( -8.919445846190019012, -77.00000000000001421, 2.652912942031755872 ) ) ;
#42823 = FACE_OUTER_BOUND ( 'NONE', #38323, .T. ) ;
#42824 = PRODUCT_DEFINITION_SHAPE ( 'NONE', 'NONE',  #58411 ) ;
#42825 = DIRECTION ( 'NONE',  ( -0.7071067811865475727, 0.000000000000000000, 0.7071067811865475727 ) ) ;
#42826 = CARTESIAN_POINT ( 'NONE',  ( -8.596685113910227827, -78.54795705239990866, 6.606654461210803575 ) ) ;
#42827 = ADVANCED_FACE ( 'NONE', ( #20362 ), #38647, .F. ) ;
#42828 = VECTOR ( 'NONE', #37358, 1000.000000000000000 ) ;
#42829 = CARTESIAN_POINT ( 'NONE',  ( -9.687172913667000174, -79.71974751974299522, -1.248753675804000096 ) ) ;
#42830 = VERTEX_POINT ( 'NONE', #43370 ) ;
#42831 = ORIENTED_EDGE ( 'NONE', *, *, #35921, .T. ) ;
#42832 = CARTESIAN_POINT ( 'NONE',  ( -10.77438703219000082, -76.28333592657999418, 6.510590034606999588 ) ) ;
#42833 = CARTESIAN_POINT ( 'NONE',  ( 0.7522352506039718945, -78.73061799086674739, -10.72516942589862765 ) ) ;
#42834 = B_SPLINE_CURVE_WITH_KNOTS ( 'NONE', 3,
 ( #22054, #8482, #39772, #9078, #57786, #54252, #17341, #45104, #22949, #35331, #26476, #4052, #40063, #58080, #35627, #53656, #27065, #13196 ),
 .UNSPECIFIED., .F., .F.,
 ( 4, 2, 2, 2, 2, 2, 2, 2, 4 ),
 ( 0.000000000000000000, 0.1250000000000000000, 0.2500000000000000000, 0.3750000000000000000, 0.5000000000000000000, 0.6250000000000000000, 0.7500000000000000000, 0.8750000000000000000, 1.000000000000000000 ),
 .UNSPECIFIED. ) ;
#42835 = ORIENTED_EDGE ( 'NONE', *, *, #42658, .F. ) ;
#42836 = VECTOR ( 'NONE', #32181, 999.9999999999998863 ) ;
#42837 = CARTESIAN_POINT ( 'NONE',  ( 10.13695543448000080, -18.29168900649999685, 7.646071007876000358 ) ) ;
#42838 = CARTESIAN_POINT ( 'NONE',  ( -0.6747260877994001316, -82.22962677363800310, -1.052256958371999840 ) ) ;
#42839 = ADVANCED_FACE ( 'NONE', ( #48109 ), #36085, .F. ) ;
#42840 = CARTESIAN_POINT ( 'NONE',  ( -10.38133291898000188, -78.11882557138000038, 7.485792156039000389 ) ) ;
#42841 = CARTESIAN_POINT ( 'NONE',  ( 2.787211053772591374, -79.74585132458871328, -10.40613102138284418 ) ) ;
#42842 = CARTESIAN_POINT ( 'NONE',  ( 9.722718241315000398, -55.35321828636000419, 7.954951288349001004 ) ) ;
#42843 = CARTESIAN_POINT ( 'NONE',  ( 6.879576957522999692, -79.15635224922900193, 8.859431780707000215 ) ) ;
#42844 = ADVANCED_FACE ( 'NONE', ( #2929 ), #56836, .T. ) ;
#42845 = ORIENTED_EDGE ( 'NONE', *, *, #42023, .T. ) ;
#42846 = CARTESIAN_POINT ( 'NONE',  ( -3.903942181442680681, -78.20186436195335489, 11.12926803347593996 ) ) ;
#42847 = EDGE_LOOP ( 'NONE', ( #23049, #9063, #21506, #38879 ) ) ;
#42848 = CARTESIAN_POINT ( 'NONE',  ( 4.204440787238356236, -77.26257104358636241, -8.239219949706841462 ) ) ;
#42849 = CARTESIAN_POINT ( 'NONE',  ( 4.799999999787999627, -74.99999999978798826, 2.226279959716000065E-09 ) ) ;
#42850 = DIRECTION ( 'NONE',  ( -0.7071067811865475727, 0.000000000000000000, 0.7071067811865475727 ) ) ;
#42851 = CARTESIAN_POINT ( 'NONE',  ( -2.185822373836047827, -77.95930140150034049, -11.00199025239787431 ) ) ;
#42852 = CARTESIAN_POINT ( 'NONE',  ( 0.6680689699263999692, -78.26673172604139950, -1.250497193771000104 ) ) ;
#42853 = DIRECTION ( 'NONE',  ( 0.000000000000000000, -1.000000000000000000, 0.000000000000000000 ) ) ;
#42854 = CARTESIAN_POINT ( 'NONE',  ( -10.42531124905999995, -18.73514851523999880, 7.624341765453999997 ) ) ;
#42855 = CARTESIAN_POINT ( 'NONE',  ( -0.8961266428360998848, -77.81024047417999157, 1.358359200922999888 ) ) ;
#42856 = CARTESIAN_POINT ( 'NONE',  ( -7.691893942754999713, -20.24546192895000019, 10.42272502865000128 ) ) ;
#42857 = CARTESIAN_POINT ( 'NONE',  ( -4.385047663734000345, -79.83700506441199707, 10.02292886995000032 ) ) ;
#42858 = CARTESIAN_POINT ( 'NONE',  ( 0.000000000000000000, -78.79999999980499581, 0.000000000000000000 ) ) ;
#42859 = CARTESIAN_POINT ( 'NONE',  ( -6.309004353333000026, -79.23106629041299698, -10.24224633278999796 ) ) ;
#42860 = CIRCLE ( 'NONE', #36225, 1.250000000000000000 ) ;
#42861 = SURFACE_STYLE_FILL_AREA ( #42570 ) ;
#42862 = CARTESIAN_POINT ( 'NONE',  ( 0.1743336006483000022, -85.82581675399998744, 3.542757096472000100 ) ) ;
#42863 = ORIENTED_EDGE ( 'NONE', *, *, #37206, .F. ) ;
#42864 = CARTESIAN_POINT ( 'NONE',  ( 0.8470819118255000779, -81.66359336816999814, 1.477252506412999988 ) ) ;
#42865 = CARTESIAN_POINT ( 'NONE',  ( -1.563706488702000019, -81.36237249610999811, -0.6734635195847999967 ) ) ;
#42866 = CARTESIAN_POINT ( 'NONE',  ( -2.814022724594611002, -79.20431978241809645, -10.47055871344663736 ) ) ;
#42867 = CARTESIAN_POINT ( 'NONE',  ( 7.851705946354000432, -77.24798175999399064, -9.048036745432998629 ) ) ;
#42868 = EDGE_CURVE ( 'NONE', #23950, #17469, #35089, .T. ) ;
#42869 = CARTESIAN_POINT ( 'NONE',  ( -7.622784390062999904, -18.21288991773999655, 10.47836615826999918 ) ) ;
#42870 = CARTESIAN_POINT ( 'NONE',  ( -1.172752930815400330, -77.78199484943172592, -0.4985573381714419883 ) ) ;
#42871 = CARTESIAN_POINT ( 'NONE',  ( 2.226387500030236222, -2.070620109172146783, 2.730464303426434647 ) ) ;
#42872 = CARTESIAN_POINT ( 'NONE',  ( 8.977835961907908668, -80.89677031670710505, 5.915845532768282844 ) ) ;
#42873 = CARTESIAN_POINT ( 'NONE',  ( 8.779834778627000347, -77.35854790367199030, 3.394951511978999914 ) ) ;
#42874 = CARTESIAN_POINT ( 'NONE',  ( 1.758095523371000057, -55.07708336086999878, -12.57362173513000059 ) ) ;
#42875 = CARTESIAN_POINT ( 'NONE',  ( -0.9355429176084000265, -78.34062011958100413, 10.99211052673000033 ) ) ;
#42876 = DIRECTION ( 'NONE',  ( 0.000000000000000000, 1.000000000000000000, 0.000000000000000000 ) ) ;
#42877 = CARTESIAN_POINT ( 'NONE',  ( -6.401221879440000428, -80.95148307551198741, 8.835606657229000405 ) ) ;
#42878 = CARTESIAN_POINT ( 'NONE',  ( -0.07592439753940152802, -81.52996157210986894, 1.272577748247039953 ) ) ;
#42879 = ORIENTED_EDGE ( 'NONE', *, *, #38692, .F. ) ;
#42880 = CARTESIAN_POINT ( 'NONE',  ( 10.98363359191198718, -18.81005173320433244, -0.5998275989260992702 ) ) ;
#42881 = DIRECTION ( 'NONE',  ( -0.5721800015184017596, -0.8201280667447015116, 0.000000000000000000 ) ) ;
#42882 = CIRCLE ( 'NONE', #57940, 9.549999999999998934 ) ;
#42883 = CARTESIAN_POINT ( 'NONE',  ( -0.5390150933989998894, -62.06260891619000120, -12.77520261008999825 ) ) ;
#42884 = LINE ( 'NONE', #10134, #1305 ) ;
#42885 = CARTESIAN_POINT ( 'NONE',  ( 6.329984427697000093, -78.09338962473199786, 9.260097609460000712 ) ) ;
#42886 = CARTESIAN_POINT ( 'NONE',  ( -3.673218652927999539, -79.27200483476298132, 10.34270183798999909 ) ) ;
#42887 = CARTESIAN_POINT ( 'NONE',  ( 10.45204383623999966, -59.56256649442000395, -7.651147548074000326 ) ) ;
#42888 = CARTESIAN_POINT ( 'NONE',  ( -0.08687330363763785812, -85.83020835005841320, 4.012123666634238361 ) ) ;
#42889 = DIRECTION ( 'NONE',  ( -0.7071067811813920301, 1.254536121801983732E-07, -0.7071067811916919021 ) ) ;
#42890 = CARTESIAN_POINT ( 'NONE',  ( 11.34432545814875759, -78.46928195054157129, 3.060665140078473456 ) ) ;
#42891 = DIRECTION ( 'NONE',  ( 0.7071067811865475727, 0.000000000000000000, -0.7071067811865475727 ) ) ;
#42892 = ORIENTED_EDGE ( 'NONE', *, *, #24691, .T. ) ;
#42893 = CARTESIAN_POINT ( 'NONE',  ( -0.7863337385806483670, -80.02967789379255237, 0.9744850512003893073 ) ) ;
#42894 = DIRECTION ( 'NONE',  ( 0.7071067811865969777, -0.7071067811864980568, -1.752031294627994831E-09 ) ) ;
#42895 = CARTESIAN_POINT ( 'NONE',  ( -4.391024480082000636, -78.77232678876399063, -10.37534762698999913 ) ) ;
#42896 = CARTESIAN_POINT ( 'NONE',  ( -1.564666716807709523, -79.19661455703162289, -11.94661365431226230 ) ) ;
#42897 = CARTESIAN_POINT ( 'NONE',  ( 5.896171905175000560, -77.96999999999999886, 7.127247495676000355 ) ) ;
#42898 = CARTESIAN_POINT ( 'NONE',  ( -10.18496935386000146, -58.55064714674999493, 7.710095619709000481 ) ) ;
#42899 = CARTESIAN_POINT ( 'NONE',  ( 0.5365775619572886734, -82.00317296149017920, -1.414790940926362151 ) ) ;
#42900 = CARTESIAN_POINT ( 'NONE',  ( 0.6717993463937350640, -79.77075207433689741, -1.054362998114927619 ) ) ;
#42901 = CARTESIAN_POINT ( 'NONE',  ( -1.093352572409234780, -81.05902749701662913, 0.6297817180695111094 ) ) ;
#42902 = B_SPLINE_CURVE_WITH_KNOTS ( 'NONE', 3,
 ( #13024, #17175, #3884, #39894, #30737, #8317, #12178, #4184, #53483, #49061 ),
 .UNSPECIFIED., .F., .F.,
 ( 4, 2, 2, 2, 4 ),
 ( 0.000000000000000000, 0.2500000000000000000, 0.5000000000000000000, 0.7500000000000000000, 1.000000000000000000 ),
 .UNSPECIFIED. ) ;
#42903 = ORIENTED_EDGE ( 'NONE', *, *, #49913, .T. ) ;
#42904 = FACE_OUTER_BOUND ( 'NONE', #15524, .T. ) ;
#42905 = EDGE_CURVE ( 'NONE', #20755, #10164, #44999, .T. ) ;
#42906 = AXIS2_PLACEMENT_3D ( 'NONE', #56439, #11283, #15110 ) ;
#42907 = CARTESIAN_POINT ( 'NONE',  ( 0.000000000000000000, -76.39999999999999147, 0.000000000000000000 ) ) ;
#42908 = ORIENTED_EDGE ( 'NONE', *, *, #20538, .T. ) ;
#42909 = ORIENTED_EDGE ( 'NONE', *, *, #14581, .T. ) ;
#42910 = CARTESIAN_POINT ( 'NONE',  ( -12.66235371494999917, -53.66260492101000068, -0.4957155363045000485 ) ) ;
#42911 = VECTOR ( 'NONE', #38714, 1000.000000000000000 ) ;
#42912 = ORIENTED_EDGE ( 'NONE', *, *, #40608, .T. ) ;
#42913 = VERTEX_POINT ( 'NONE', #46529 ) ;
#42914 = CARTESIAN_POINT ( 'NONE',  ( -0.8918451245034728636, -81.00000000000001421, -10.91351453700477947 ) ) ;
#42915 = CARTESIAN_POINT ( 'NONE',  ( -8.418448289622000758, -77.62832987473298374, -6.950186643912999784 ) ) ;
#42916 = PRODUCT_CONTEXT ( 'NONE', #11925, 'mechanical' ) ;
#42917 = CARTESIAN_POINT ( 'NONE',  ( 1.460959015002474048, -78.22916666666667140, -0.3926218265389178064 ) ) ;
#42918 = CARTESIAN_POINT ( 'NONE',  ( -7.662730551410999347, -78.63956332859899589, 6.107448752912000067 ) ) ;
#42919 = AXIS2_PLACEMENT_3D ( 'NONE', #43226, #19624, #51227 ) ;
#42920 = CARTESIAN_POINT ( 'NONE',  ( 0.03245390597466887156, -78.22536965980819446, -9.249895125673516461 ) ) ;
#42921 = LINE ( 'NONE', #47365, #4934 ) ;
#42922 = EDGE_CURVE ( 'NONE', #26124, #8841, #24061, .T. ) ;
#42923 = ORIENTED_EDGE ( 'NONE', *, *, #252, .T. ) ;
#42924 = ORIENTED_EDGE ( 'NONE', *, *, #46460, .T. ) ;
#42925 = CARTESIAN_POINT ( 'NONE',  ( -8.799679198670379066, -77.57509512262019769, 2.850925869413578173 ) ) ;
#42926 = DIRECTION ( 'NONE',  ( 0.000000000000000000, 1.000000000000000000, 0.000000000000000000 ) ) ;
#42927 = CARTESIAN_POINT ( 'NONE',  ( -12.65987830577000040, -61.73692962272999551, -0.9847759095506000149 ) ) ;
#42928 = CARTESIAN_POINT ( 'NONE',  ( 1.260641617779999946, -77.69478446506998637, 9.621927669549000584 ) ) ;
#42929 = CARTESIAN_POINT ( 'NONE',  ( 3.647699722740822548, -86.17851881763699851, -1.624060551956400866 ) ) ;
#42931 = CIRCLE ( 'NONE', #40894, 3.400000000000000799 ) ;
#42930 = DIRECTION ( 'NONE',  ( 0.6562721000563372931, 0.7545243075525430720, -7.866585117886450344E-10 ) ) ;
#42932 = CARTESIAN_POINT ( 'NONE',  ( 0.1636246173744642929, -79.86458333333331439, 1.250000000000000888 ) ) ;
#42933 = CARTESIAN_POINT ( 'NONE',  ( 10.48543666025108045, -76.69166666666666288, 6.043427764450817641 ) ) ;
#42934 = CARTESIAN_POINT ( 'NONE',  ( -0.5553526962645999321, -81.36548177752000299, -1.429183993495000138 ) ) ;
#42935 = CARTESIAN_POINT ( 'NONE',  ( -0.3271848554490991434, -81.10416666666665719, -1.217465845835395299 ) ) ;
#42936 = CARTESIAN_POINT ( 'NONE',  ( -9.830798712606000578, -54.70910918491000530, 7.765013391389000041 ) ) ;
#42937 = CARTESIAN_POINT ( 'NONE',  ( -3.098141882180000195, -79.04281332859899578, -9.414028956051998520 ) ) ;
#42938 = CARTESIAN_POINT ( 'NONE',  ( -3.140974612311405512, -77.29583333333333428, 11.68767212001977640 ) ) ;
#42939 = EDGE_CURVE ( 'NONE', #52539, #54974, #23471, .T. ) ;
#42940 = CARTESIAN_POINT ( 'NONE',  ( -7.646788101826000883, -18.62771363264999991, -10.00831428591000005 ) ) ;
#42942 = CARTESIAN_POINT ( 'NONE',  ( 1.807051837523000026, -17.69921584757000232, -12.77977401834999860 ) ) ;
#42941 = CARTESIAN_POINT ( 'NONE',  ( -1.500000000000000000, -78.89999999999999147, 0.000000000000000000 ) ) ;
#42943 = CARTESIAN_POINT ( 'NONE',  ( -3.251154051729839178, -1.100857096137070279, 2.995606203745920413E-05 ) ) ;
#42944 = CARTESIAN_POINT ( 'NONE',  ( 13.86363625866319715, -9.638971321655001034, 0.001706075946107427251 ) ) ;
#42945 = CARTESIAN_POINT ( 'NONE',  ( 3.383845406481000406, -2.564161638761000450, -1.742318191517000070 ) ) ;
#42946 = CARTESIAN_POINT ( 'NONE',  ( -0.8613851204907587711, -0.8555241698066097245, -3.423604145181888825 ) ) ;
#42947 = ORIENTED_EDGE ( 'NONE', *, *, #29731, .F. ) ;
#42948 = CARTESIAN_POINT ( 'NONE',  ( -8.768124086549999419, -59.94999999446000771, -7.919595949288999570 ) ) ;
#42949 = CARTESIAN_POINT ( 'NONE',  ( 0.000000000000000000, -76.30000000005068728, 0.000000000000000000 ) ) ;
#42950 = CARTESIAN_POINT ( 'NONE',  ( -1.667260628947000001, -55.59057987493000041, 12.49858003893000102 ) ) ;
#42951 = CONICAL_SURFACE ( 'NONE', #14611, 5.249999999862000166, 0.7853981633972997312 ) ;
#42952 = CARTESIAN_POINT ( 'NONE',  ( 0.4131922926977418253, -78.44830526474305543, 1.179719367296339527 ) ) ;
#42953 = B_SPLINE_CURVE_WITH_KNOTS ( 'NONE', 3,
 ( #11688, #43555, #29666, #12540, #20541, #3120, #57699, #44134, #21398, #38827 ),
 .UNSPECIFIED., .F., .F.,
 ( 4, 1, 1, 2, 2, 4 ),
 ( 0.000000000000000000, 0.2499999999999998890, 0.3749999999999998335, 0.4374999999999998890, 0.5000000000000000000, 1.000000000000000000 ),
 .UNSPECIFIED. ) ;
#42954 = AXIS2_PLACEMENT_3D ( 'NONE', #52149, #57435, #52433 ) ;
#42955 = CARTESIAN_POINT ( 'NONE',  ( 4.793796853326000473, -80.12492104470399568, -7.994680211816000970 ) ) ;
#42956 = CARTESIAN_POINT ( 'NONE',  ( -12.43570956081999945, -53.92016029949000000, 0.4384071701245000341 ) ) ;
#42957 = CARTESIAN_POINT ( 'NONE',  ( 12.00000000000000000, -23.25000000000000000, 0.000000000000000000 ) ) ;
#42958 = CARTESIAN_POINT ( 'NONE',  ( 1.382886570147999983, -61.43098219798999793, 12.65982054480000052 ) ) ;
#42959 = DIRECTION ( 'NONE',  ( -0.7071067811865475727, 0.000000000000000000, 0.7071067811865475727 ) ) ;
#42960 = CARTESIAN_POINT ( 'NONE',  ( 0.000000000000000000, -75.15999999999999659, 0.000000000000000000 ) ) ;
#42961 = CARTESIAN_POINT ( 'NONE',  ( -9.642170440073000393, -77.83155199647998757, 5.184908120652999663 ) ) ;
#42962 = CARTESIAN_POINT ( 'NONE',  ( -0.3136163193838756302, -76.32274192230099175, -11.74634812822112373 ) ) ;
#42963 = CARTESIAN_POINT ( 'NONE',  ( 1.623230447552999944, -77.84549303256399355, -11.02813327291000078 ) ) ;
#42964 = CARTESIAN_POINT ( 'NONE',  ( 9.722066209057999231, -78.90129514476063832, 0.1588365413100999990 ) ) ;
#42965 = CARTESIAN_POINT ( 'NONE',  ( -1.613878645371000120, -79.31052490905000241, 0.4035920743843999792 ) ) ;
#42966 = LINE ( 'NONE', #7810, #33907 ) ;
#42967 = CARTESIAN_POINT ( 'NONE',  ( 8.857115352654000517, -79.28934805011499520, -3.584237475251999872 ) ) ;
#42968 = FACE_OUTER_BOUND ( 'NONE', #44321, .T. ) ;
#42969 = CARTESIAN_POINT ( 'NONE',  ( 10.36861781779881220, -80.32830027787916549, -2.923430239069336078 ) ) ;
#42970 = CARTESIAN_POINT ( 'NONE',  ( -7.956214544937700417, -76.13333333331455322, 8.846276171663262744 ) ) ;
#42971 = DIRECTION ( 'NONE',  ( 0.000000000000000000, -1.000000000000000000, 0.000000000000000000 ) ) ;
#42972 = CARTESIAN_POINT ( 'NONE',  ( -10.65106809510000119, -79.02763761715399937, 5.591232889670999739 ) ) ;
#42973 = EDGE_CURVE ( 'NONE', #47711, #45259, #53033, .T. ) ;
#42974 = CARTESIAN_POINT ( 'NONE',  ( -0.9995835529977281642, -81.94791666666664298, 0.7681833999686391579 ) ) ;
#42975 = CARTESIAN_POINT ( 'NONE',  ( 13.89999999928999941, -5.999999999291000030, 8.437407073926000296E-09 ) ) ;
#42976 = VERTEX_POINT ( 'NONE', #39387 ) ;
#42977 = ADVANCED_FACE ( 'NONE', ( #52675 ), #52107, .T. ) ;
#42978 = CARTESIAN_POINT ( 'NONE',  ( 26.50000000000000000, -39.49523982883999906, 1.535553829149999833E-05 ) ) ;
#42979 = ORIENTED_EDGE ( 'NONE', *, *, #41429, .F. ) ;
#42980 = ORIENTED_EDGE ( 'NONE', *, *, #52535, .T. ) ;
#42981 = CARTESIAN_POINT ( 'NONE',  ( -3.250000000000000000, -1.500000000000000000, 0.000000000000000000 ) ) ;
#42982 = CARTESIAN_POINT ( 'NONE',  ( 7.220923959705269013, -77.47708333333335418, -9.396085398178609438 ) ) ;
#42983 = CARTESIAN_POINT ( 'NONE',  ( 3.496897448754000326, -80.96724209361498481, -0.5802409159389999571 ) ) ;
#42984 = CARTESIAN_POINT ( 'NONE',  ( 4.854244445426996180, -79.23213983034467844, 8.180124833994572242 ) ) ;
#42985 = VECTOR ( 'NONE', #590, 1000.000000000000000 ) ;
#42986 = ORIENTED_EDGE ( 'NONE', *, *, #1218, .T. ) ;
#42988 = EDGE_CURVE ( 'NONE', #46629, #4192, #43244, .T. ) ;
#42987 = CARTESIAN_POINT ( 'NONE',  ( 0.8412509418493856472, -82.78432527956375964, -0.9249430534936740056 ) ) ;
#42989 = ORIENTED_EDGE ( 'NONE', *, *, #2276, .T. ) ;
#42990 = CARTESIAN_POINT ( 'NONE',  ( -7.691893942748999180, -57.04546192861999998, 10.42272502865000128 ) ) ;
#42991 = VERTEX_POINT ( 'NONE', #44109 ) ;
#42992 = CARTESIAN_POINT ( 'NONE',  ( 5.292225205187681247, -79.72180290446119955, -7.854116158959713268 ) ) ;
#42993 = CARTESIAN_POINT ( 'NONE',  ( 1.440783608768007706, -78.47261458352124919, -0.5214944750746852709 ) ) ;
#42994 = CARTESIAN_POINT ( 'NONE',  ( 0.6398064034500148267, -79.79999999999999716, -11.76818875537070319 ) ) ;
#42995 = AXIS2_PLACEMENT_3D ( 'NONE', #28263, #38590, #24731 ) ;
#42996 = CARTESIAN_POINT ( 'NONE',  ( -10.35066237538938871, -80.07823043094967375, 2.909028927936140541 ) ) ;
#42997 = CARTESIAN_POINT ( 'NONE',  ( 1.250000000000000000, -76.29999999999999716, 0.000000000000000000 ) ) ;
#42998 = CARTESIAN_POINT ( 'NONE',  ( -3.280005808348441576, -86.39318692614396866, 1.535071293332731734 ) ) ;
#42999 = CARTESIAN_POINT ( 'NONE',  ( -9.939389728518001732, -76.86378799035300347, 5.126617716248000001 ) ) ;
#43000 = CARTESIAN_POINT ( 'NONE',  ( -8.707890922082185625, -79.81324511864698934, 4.310198284464144436 ) ) ;
#43001 = DIRECTION ( 'NONE',  ( -1.000000000000000000, 0.000000000000000000, 0.000000000000000000 ) ) ;
#43002 = CARTESIAN_POINT ( 'NONE',  ( 7.439409605643000134, -76.07570142656899748, -8.009466158711999739 ) ) ;
#43003 = CARTESIAN_POINT ( 'NONE',  ( -7.690083695982694145, -78.64705780292665338, -5.141504542771214936 ) ) ;
#43004 = CARTESIAN_POINT ( 'NONE',  ( -1.000649921775999873, -79.62063801436200094, 0.8816325131470000853 ) ) ;
#43005 = DIRECTION ( 'NONE',  ( 0.000000000000000000, -1.000000000000000000, 0.000000000000000000 ) ) ;
#43006 = DIRECTION ( 'NONE',  ( 0.000000000000000000, 0.000000000000000000, -1.000000000000000000 ) ) ;
#43007 = CARTESIAN_POINT ( 'NONE',  ( -3.666040373708999933, -81.44778455456800259, -0.8194572562286999151 ) ) ;
#43008 = CARTESIAN_POINT ( 'NONE',  ( 11.65955775483000068, -79.23508084193099421, -3.592192024490000080 ) ) ;
#43009 = CARTESIAN_POINT ( 'NONE',  ( -10.57218038258165116, -78.08557172664846746, 1.947236671181371337 ) ) ;
#43010 = CARTESIAN_POINT ( 'NONE',  ( -13.95956770449999951, -33.08075762116000362, -5.182382777876000184E-05 ) ) ;
#43011 = CARTESIAN_POINT ( 'NONE',  ( -12.99510751537000353, -63.10294702886003648, 6.911973076623003642 ) ) ;
#43012 = CARTESIAN_POINT ( 'NONE',  ( 1.862820775644999927, -85.68044503318799343, 3.018521682574000220 ) ) ;
#43013 = B_SPLINE_CURVE_WITH_KNOTS ( 'NONE', 3,
 ( #7398, #38111, #29532, #19829, #6820, #56990, #43417, #24252, #2698, #20122, #33387, #33677, #48155, #24830, #2122, #42846, #34535, #16552 ),
 .UNSPECIFIED., .F., .F.,
 ( 4, 2, 2, 2, 2, 2, 2, 2, 4 ),
 ( 0.000000000000000000, 0.1250000000000000000, 0.2500000000000000000, 0.3750000000000000000, 0.5000000000000000000, 0.6250000000000000000, 0.7500000000000000000, 0.8750000000000000000, 1.000000000000000000 ),
 .UNSPECIFIED. ) ;
#43014 = CARTESIAN_POINT ( 'NONE',  ( 1.249999999999999778, -80.26041666666665719, 0.1636246173744711763 ) ) ;
#43015 = CARTESIAN_POINT ( 'NONE',  ( 10.53101990620000095, -18.69360215052999763, 7.613962745610000304 ) ) ;
#43016 = CARTESIAN_POINT ( 'NONE',  ( -9.783241737811998462, -61.33564621498000946, -7.961026681588999843 ) ) ;
#43017 = CARTESIAN_POINT ( 'NONE',  ( -9.199999999968001774, -80.60000000003199716, 3.388760884947000060E-10 ) ) ;
#43018 = CARTESIAN_POINT ( 'NONE',  ( -1.234140985588999984, -81.10340625466299969, 0.5054425604136000283 ) ) ;
#43019 = CARTESIAN_POINT ( 'NONE',  ( 0.5951337072741889056, -79.15689260744959199, -1.420922764992056608 ) ) ;
#43020 = CARTESIAN_POINT ( 'NONE',  ( 5.715297388934000189, -78.39081763324999486, 11.69132169264999987 ) ) ;
#43021 = EDGE_CURVE ( 'NONE', #54392, #43629, #1228, .T. ) ;
#43022 = CARTESIAN_POINT ( 'NONE',  ( 6.123452257235864060, -77.62355967761020281, -8.862192408124634824 ) ) ;
#43023 = CARTESIAN_POINT ( 'NONE',  ( 3.747727186550270595, -78.25250684441732574, -10.42547443909607097 ) ) ;
#43024 = CARTESIAN_POINT ( 'NONE',  ( -9.331191635713286914, -77.45159008118203303, -0.1973268560526538207 ) ) ;
#43025 = CARTESIAN_POINT ( 'NONE',  ( 11.80084191424000117, -76.30738641031999236, -3.682937823519999654 ) ) ;
#43026 = ORIENTED_EDGE ( 'NONE', *, *, #32128, .F. ) ;
#43027 = CARTESIAN_POINT ( 'NONE',  ( 1.618170588614999961, -80.38646948174221052, -11.14857479085000058 ) ) ;
#43028 = DIRECTION ( 'NONE',  ( -1.000000000000000000, 0.000000000000000000, 0.000000000000000000 ) ) ;
#43029 = CARTESIAN_POINT ( 'NONE',  ( -1.001315002179000047, -24.68522411714000242, 12.50000000000000000 ) ) ;
#43030 = CARTESIAN_POINT ( 'NONE',  ( -10.43921282250999916, -78.53242462859000739, 7.393929757317000195 ) ) ;
#43031 = CARTESIAN_POINT ( 'NONE',  ( 12.72397198031000087, -55.57854962903999763, -1.930909771329999858 ) ) ;
#43032 = CARTESIAN_POINT ( 'NONE',  ( -5.310864497047000476, -77.81454279010098674, 8.034172531070000289 ) ) ;
#43033 = CARTESIAN_POINT ( 'NONE',  ( -1.596536837631000072, -81.91187053245998584, -0.4757406268331999533 ) ) ;
#43034 = CARTESIAN_POINT ( 'NONE',  ( 1.757484578084819615, -79.96227339042748383, 10.60516276134810987 ) ) ;
#43035 = CARTESIAN_POINT ( 'NONE',  ( 10.35453599130000057, -76.75783510652000530, -6.064947188958000446 ) ) ;
#43036 = VERTEX_POINT ( 'NONE', #21371 ) ;
#43037 = VECTOR ( 'NONE', #39011, 1000.000000000000227 ) ;
#43038 = CARTESIAN_POINT ( 'NONE',  ( 10.75336441781152175, -77.34819408117270712, -0.2553265604148902690 ) ) ;
#43039 = DIRECTION ( 'NONE',  ( -1.000000000000000000, 0.000000000000000000, 0.000000000000000000 ) ) ;
#43040 = ORIENTED_EDGE ( 'NONE', *, *, #10495, .T. ) ;
#43041 = VECTOR ( 'NONE', #58186, 1000.000000000000114 ) ;
#43042 = CARTESIAN_POINT ( 'NONE',  ( 7.267180141948999861, -79.12481710499199039, 8.322618964701998578 ) ) ;
#43043 = CARTESIAN_POINT ( 'NONE',  ( -1.249670801961172417, -80.60660109082429869, -0.09504704068232089353 ) ) ;
#43044 = AXIS2_PLACEMENT_3D ( 'NONE', #36393, #49701, #53529 ) ;
#43045 = ORIENTED_EDGE ( 'NONE', *, *, #9866, .F. ) ;
#43046 = EDGE_CURVE ( 'NONE', #51486, #44855, #27748, .T. ) ;
#43047 = CARTESIAN_POINT ( 'NONE',  ( -8.870296161681000768, -77.67513961849198267, -7.212480266026999765 ) ) ;
#43048 = VERTEX_POINT ( 'NONE', #29355 ) ;
#43049 = ORIENTED_EDGE ( 'NONE', *, *, #41212, .F. ) ;
#43050 = CARTESIAN_POINT ( 'NONE',  ( -0.2554408763343102851, -80.49153132872807248, 1.223531717389471307 ) ) ;
#43051 = B_SPLINE_CURVE_WITH_KNOTS ( 'NONE', 3,
 ( #18577, #874, #36852, #47204, #25024, #24740, #6147, #42755, #37436, #46910, #56616, #11179, #20602, #15591, #19735, #42173, #1450, #29155, #14999, #7021, #38601, #16175, #28276, #43043, #51625 ),
 .UNSPECIFIED., .F., .F.,
 ( 4, 2, 2, 2, 2, 1, 1, 1, 2, 2, 2, 2, 2, 4 ),
 ( 0.000000000000000000, 0.1249999999999988620, 0.2499999999999977240, 0.3749999999999965583, 0.4374999999999960587, 0.4687499999999961142, 0.4843749999999958367, 0.4921874999999953371, 0.4960937499999951150, 0.4999999999999948375, 0.6249999999999961142, 0.7499999999999973355, 0.8749999999999986677, 1.000000000000000000 ),
 .UNSPECIFIED. ) ;
#43052 = FACE_OUTER_BOUND ( 'NONE', #22483, .T. ) ;
#43053 = CARTESIAN_POINT ( 'NONE',  ( -8.448510849392999233, -79.46847394982049195, 4.901364000006999788 ) ) ;
#43054 = EDGE_LOOP ( 'NONE', ( #53444, #4090, #26148, #44467 ) ) ;
#43056 = EDGE_CURVE ( 'NONE', #2598, #39462, #56820, .T. ) ;
#43055 = FACE_OUTER_BOUND ( 'NONE', #9362, .T. ) ;
#43057 = CARTESIAN_POINT ( 'NONE',  ( 5.887377288745000214, -79.97133913145148654, 9.329533489291000237 ) ) ;
#43058 = EDGE_LOOP ( 'NONE', ( #32562, #19176, #8348, #58400 ) ) ;
#43059 = CARTESIAN_POINT ( 'NONE',  ( 0.4482635754052999855, -78.67790996937631576, -12.25553529036999834 ) ) ;
#43060 = EDGE_CURVE ( 'NONE', #54702, #53710, #46491, .T. ) ;
#43061 = CARTESIAN_POINT ( 'NONE',  ( 8.256620083228000340, -77.21874415034599792, -4.688888258373000717 ) ) ;
#43062 = CARTESIAN_POINT ( 'NONE',  ( 7.605690612596999856, -55.37434870709000023, 10.52682230156000109 ) ) ;
#43063 = CARTESIAN_POINT ( 'NONE',  ( 9.998734510692498745, -54.87263061026122557, 7.709128441167307777 ) ) ;
#43064 = CARTESIAN_POINT ( 'NONE',  ( -1.310679582531389276, -78.35833333333332007, 0.7554284705563443225 ) ) ;
#43065 = B_SPLINE_CURVE_WITH_KNOTS ( 'NONE', 3,
 ( #34497, #51962, #46965, #16227 ),
 .UNSPECIFIED., .F., .F.,
 ( 4, 4 ),
 ( 0.000000000000000000, 1.000000000000000000 ),
 .UNSPECIFIED. ) ;
#43066 = CARTESIAN_POINT ( 'NONE',  ( -3.962812355711000212, -78.54828561713269153, 3.526087981832999841E-09 ) ) ;
#43067 = CARTESIAN_POINT ( 'NONE',  ( 2.946656154917213222, -80.99641046095393904, -10.60865452211998772 ) ) ;
#43068 = CARTESIAN_POINT ( 'NONE',  ( 11.70594025892000012, -78.41704903027755336, 2.546964289010999583 ) ) ;
#43069 = CARTESIAN_POINT ( 'NONE',  ( -1.005435018732895314, -82.01458334923671600, -3.884934934212340263 ) ) ;
#43070 = CARTESIAN_POINT ( 'NONE',  ( -7.762981007049000404, -24.16089459216999913, 9.992000916352999695 ) ) ;
#43071 = VECTOR ( 'NONE', #30031, 1000.000000000000000 ) ;
#43072 = DIRECTION ( 'NONE',  ( 0.7071067811865969777, -0.7071067811864980568, -1.725239202167994796E-11 ) ) ;
#43073 = CARTESIAN_POINT ( 'NONE',  ( 5.131017344144000347, -78.15092668086899153, 8.166481637765999224 ) ) ;
#43074 = ADVANCED_FACE ( 'NONE', ( #2513 ), #30377, .T. ) ;
#43075 = CARTESIAN_POINT ( 'NONE',  ( 9.934814764497000183, -61.42368287795999748, -7.968971842771999547 ) ) ;
#43076 = CARTESIAN_POINT ( 'NONE',  ( 4.750030159171999777, -78.60465007998999454, -11.30647155123999958 ) ) ;
#43077 = DIRECTION ( 'NONE',  ( 0.000000000000000000, 0.000000000000000000, 1.000000000000000000 ) ) ;
#43078 = CARTESIAN_POINT ( 'NONE',  ( 0.000000000000000000, -81.79999999999998295, 0.000000000000000000 ) ) ;
#43079 = VECTOR ( 'NONE', #9193, 1000.000000000000000 ) ;
#43080 = CARTESIAN_POINT ( 'NONE',  ( 12.54238283046685076, -23.52853599825469644, -1.749799162367749794 ) ) ;
#43081 = CARTESIAN_POINT ( 'NONE',  ( -12.00000000000000178, -77.81041666666665435, -1.570796326794897890 ) ) ;
#43082 = AXIS2_PLACEMENT_3D ( 'NONE', #57656, #12215, #30496 ) ;
#43083 = ORIENTED_EDGE ( 'NONE', *, *, #32931, .F. ) ;
#43084 = CARTESIAN_POINT ( 'NONE',  ( -1.091831352987487014, -80.68921772068907217, 1.043502948795002494 ) ) ;
#43085 = DIRECTION ( 'NONE',  ( 0.7071067811865474617, 0.000000000000000000, -0.7071067811865474617 ) ) ;
#43086 = CARTESIAN_POINT ( 'NONE',  ( 1.667260628941999778, -23.20942012473999938, 12.49858003894999925 ) ) ;
#43087 = CARTESIAN_POINT ( 'NONE',  ( 11.87139580924463189, -78.66341727770496561, 2.023209039049198132 ) ) ;
#43088 = CARTESIAN_POINT ( 'NONE',  ( 2.583380683670000177, -3.278869571379000369, 2.446142499428999972 ) ) ;
#43089 = EDGE_CURVE ( 'NONE', #7256, #10595, #3111, .T. ) ;
#43090 = CARTESIAN_POINT ( 'NONE',  ( 0.3886576371541999864, -77.13648093799099570, -11.81216847760999933 ) ) ;
#43091 = CARTESIAN_POINT ( 'NONE',  ( 4.202230864774000096, -78.43131382901999871, -8.786407198941001084 ) ) ;
#43093 = CARTESIAN_POINT ( 'NONE',  ( -0.1746703279969999689, -78.35637572720449384, -1.307691051723000042 ) ) ;
#43092 = CARTESIAN_POINT ( 'NONE',  ( -8.079589622638239987, -76.13532046087181016, 8.532035202244687255 ) ) ;
#43094 = CARTESIAN_POINT ( 'NONE',  ( -0.3959877895327999497, -81.54006927205000466, 1.414086365320999850 ) ) ;
#43095 = CARTESIAN_POINT ( 'NONE',  ( -9.938393956912895177, -79.56898363239373850, 4.097518548705139096 ) ) ;
#43096 = VERTEX_POINT ( 'NONE', #25513 ) ;
#43097 = EDGE_CURVE ( 'NONE', #9068, #43122, #43530, .T. ) ;
#43098 = FACE_OUTER_BOUND ( 'NONE', #21279, .T. ) ;
#43099 = CARTESIAN_POINT ( 'NONE',  ( 1.316424014360000116, -79.32485377751800115, -11.96909690421999883 ) ) ;
#43100 = CARTESIAN_POINT ( 'NONE',  ( -9.498650009403984740, -79.25105001372490676, -0.1253404953979189163 ) ) ;
#43101 = FACE_OUTER_BOUND ( 'NONE', #28497, .T. ) ;
#43102 = CARTESIAN_POINT ( 'NONE',  ( -9.422842877325999567, -62.05952027250000214, 8.643944052328999206 ) ) ;
#43103 = CARTESIAN_POINT ( 'NONE',  ( -10.53088506292314008, -80.07679749114764434, 3.178975094537701107 ) ) ;
#43104 = CARTESIAN_POINT ( 'NONE',  ( -9.473445107265000331, -79.06847810668898546, 1.282537450098000020 ) ) ;
#43105 = CARTESIAN_POINT ( 'NONE',  ( 10.48543666025110355, -78.10833333333330586, -6.043427764450775008 ) ) ;
#43106 = CARTESIAN_POINT ( 'NONE',  ( -7.396918292183162436, -79.05208333333331439, -5.684557159767966716 ) ) ;
#43107 = VERTEX_POINT ( 'NONE', #9260 ) ;
#43108 = DIRECTION ( 'NONE',  ( -0.7071067811864980568, 0.7071067811865969777, -6.606096994262980545E-09 ) ) ;
#43109 = CARTESIAN_POINT ( 'NONE',  ( -9.500996395764293112, -79.10045220966165402, -7.058099219916003086 ) ) ;
#43110 = CARTESIAN_POINT ( 'NONE',  ( 0.5742445440065669926, -81.43721952292473532, 1.113553851155867358 ) ) ;
#43111 = B_SPLINE_CURVE_WITH_KNOTS ( 'NONE', 3,
 ( #18103, #9242, #36098, #27227, #45266, #4814, #46738, #32815, #15704, #1856, #6844, #33113, #50862, #33985, #23973, #52024, #47611, #2427, #24273, #11577, #14818, #10999, #28984, #37548 ),
 .UNSPECIFIED., .F., .F.,
 ( 4, 2, 2, 2, 2, 2, 2, 2, 2, 2, 2, 4 ),
 ( 0.000000000000000000, 0.06249999999999998612, 0.1249999999999999722, 0.2499999999999998890, 0.3749999999999998890, 0.4999999999999998890, 0.6249999999999998890, 0.7499999999999997780, 0.8124999999999997780, 0.8749999999999997780, 0.9374999999999998890, 1.000000000000000000 ),
 .UNSPECIFIED. ) ;
#43112 = ORIENTED_EDGE ( 'NONE', *, *, #45014, .F. ) ;
#43113 = CARTESIAN_POINT ( 'NONE',  ( -1.181111693982000110, -79.17654225787899236, -0.4092372983238000139 ) ) ;
#43114 = CARTESIAN_POINT ( 'NONE',  ( -0.2494208075201428676, -53.80711039216416225, -12.50614183109633260 ) ) ;
#43115 = CARTESIAN_POINT ( 'NONE',  ( 12.50483465198240474, -61.66452578640149085, 0.6958747608065251056 ) ) ;
#43116 = DIRECTION ( 'NONE',  ( 0.000000000000000000, 1.000000000000000000, 0.000000000000000000 ) ) ;
#43117 = AXIS2_PLACEMENT_3D ( 'NONE', #4362, #16287, #52299 ) ;
#43118 = CARTESIAN_POINT ( 'NONE',  ( 6.613044192456900561, -79.77364340449305757, 8.759878235630585763 ) ) ;
#43119 = CARTESIAN_POINT ( 'NONE',  ( 9.523132023602000729, -79.96870456638698954, 1.108936319727999997 ) ) ;
#43120 = EDGE_LOOP ( 'NONE', ( #52457, #6737, #18939, #16335 ) ) ;
#43121 = AXIS2_PLACEMENT_3D ( 'NONE', #34511, #42533, #24520 ) ;
#43122 = VERTEX_POINT ( 'NONE', #31669 ) ;
#43123 = CARTESIAN_POINT ( 'NONE',  ( 8.260736141417000411, -77.07624636657099870, 9.342201263974001080 ) ) ;
#43124 = CARTESIAN_POINT ( 'NONE',  ( -4.744750002824204671, -78.68878635233461694, -9.646253556620013825 ) ) ;
#43125 = CARTESIAN_POINT ( 'NONE',  ( 1.419425106214999843, -78.39754962090999868, 0.07512760555724000422 ) ) ;
#43126 = VECTOR ( 'NONE', #50601, 1000.000000000000000 ) ;
#43127 = EDGE_CURVE ( 'NONE', #48625, #23001, #18153, .T. ) ;
#43128 = ORIENTED_EDGE ( 'NONE', *, *, #18529, .F. ) ;
#43129 = B_SPLINE_CURVE_WITH_KNOTS ( 'NONE', 3,
 ( #51484, #29024, #50609, #47063 ),
 .UNSPECIFIED., .F., .F.,
 ( 4, 4 ),
 ( 0.000000000000000000, 1.000000000000000000 ),
 .UNSPECIFIED. ) ;
#43130 = CARTESIAN_POINT ( 'NONE',  ( 7.660431561281999535, -18.80820826823000047, 10.01749754194999831 ) ) ;
#43131 = DIRECTION ( 'NONE',  ( 0.000000000000000000, -1.000000000000000000, 0.000000000000000000 ) ) ;
#43132 = CARTESIAN_POINT ( 'NONE',  ( 1.689459950984219860, -54.50811746068924180, 12.71013585606941376 ) ) ;
#43133 = CARTESIAN_POINT ( 'NONE',  ( 7.167851722631999323, -78.34084413521999579, -10.60335505485999974 ) ) ;
#43134 = CARTESIAN_POINT ( 'NONE',  ( 3.463650534536347969, -79.75105914263811258, -10.20053198629427449 ) ) ;
#43135 = DIRECTION ( 'NONE',  ( -1.000000000000000000, 0.000000000000000000, 0.000000000000000000 ) ) ;
#43136 = CARTESIAN_POINT ( 'NONE',  ( 0.9218200799623694763, -79.82291666666667140, 1.199500263597272465 ) ) ;
#43137 = CARTESIAN_POINT ( 'NONE',  ( 10.54265532893000135, -78.61162538919300857, 3.830212845596999927 ) ) ;
#43138 = ORIENTED_EDGE ( 'NONE', *, *, #49890, .T. ) ;
#43139 = DIRECTION ( 'NONE',  ( -1.776356839400000238E-14, 1.000000000000000000, 0.000000000000000000 ) ) ;
#43140 = ORIENTED_EDGE ( 'NONE', *, *, #1079, .F. ) ;
#43141 = CARTESIAN_POINT ( 'NONE',  ( 6.980683240476435181, -77.29306357213712886, -6.070245327366276200 ) ) ;
#43142 = CARTESIAN_POINT ( 'NONE',  ( -1.141857967141000074, -79.78369273832200292, -0.6608524743567000259 ) ) ;
#43143 = CARTESIAN_POINT ( 'NONE',  ( 10.29127903888148587, -77.63246528547833236, 4.462195054874572797 ) ) ;
#43144 = CARTESIAN_POINT ( 'NONE',  ( -1.509488703453999880, -79.05477463579200048, -0.1420306293263000064 ) ) ;
#43145 = DIRECTION ( 'NONE',  ( 0.000000000000000000, -1.000000000000000000, 0.000000000000000000 ) ) ;
#43146 = EDGE_CURVE ( 'NONE', #49897, #19229, #31078, .T. ) ;
#43147 = FACE_OUTER_BOUND ( 'NONE', #379, .T. ) ;
#43148 = CARTESIAN_POINT ( 'NONE',  ( -1.573065832928000063, -78.86819029998999042, 0.4172852021023999991 ) ) ;
#43149 = CARTESIAN_POINT ( 'NONE',  ( -7.640030139758000161, -18.69283065396999888, 10.18491068059999805 ) ) ;
#43150 = CARTESIAN_POINT ( 'NONE',  ( 6.762881825298999949, -79.17047959254598766, -8.737352176957999816 ) ) ;
#43151 = EDGE_CURVE ( 'NONE', #17252, #57807, #18196, .T. ) ;
#43152 = FILL_AREA_STYLE ('',( #16568 ) ) ;
#43153 = CARTESIAN_POINT ( 'NONE',  ( 0.000000000000000000, 4.040000000000000036, 0.000000000000000000 ) ) ;
#43154 = CARTESIAN_POINT ( 'NONE',  ( -3.514851922797999961, -84.67451069913499850, -0.4591155470951999717 ) ) ;
#43155 = VERTEX_POINT ( 'NONE', #39953 ) ;
#43156 = CARTESIAN_POINT ( 'NONE',  ( 1.575652246471999973, -82.61098159482399694, 0.6458614041720999177 ) ) ;
#43157 = CARTESIAN_POINT ( 'NONE',  ( 0.2307066564514000107, -79.59422942033999959, -1.449970716867000187 ) ) ;
#43158 = CYLINDRICAL_SURFACE ( 'NONE', #16273, 10.75000000000000000 ) ;
#43159 = CARTESIAN_POINT ( 'NONE',  ( -11.74098051674999965, -78.48240034705800383, 2.380218674853999961 ) ) ;
#43160 = CARTESIAN_POINT ( 'NONE',  ( 8.899186938124000079, -76.04999999999999716, -6.465637775218000094 ) ) ;
#43161 = AXIS2_PLACEMENT_3D ( 'NONE', #49683, #9228, #27214 ) ;
#43162 = CARTESIAN_POINT ( 'NONE',  ( 0.3994397004326888379, -78.10002733708165579, 1.210016675113110507 ) ) ;
#43163 = CARTESIAN_POINT ( 'NONE',  ( 0.9301983931536133010, -2.396301603284799242, -3.396501321809576091 ) ) ;
#43164 = CARTESIAN_POINT ( 'NONE',  ( -9.646692012709999986, -78.68015584965399967, 1.218660606027000215 ) ) ;
#43165 = CARTESIAN_POINT ( 'NONE',  ( 5.315453493860999856, -78.81519127177598705, -7.900401732693999257 ) ) ;
#43166 = CARTESIAN_POINT ( 'NONE',  ( 0.3647771924839282587, -81.24853632404513348, -1.197947852285521142 ) ) ;
#43167 = CARTESIAN_POINT ( 'NONE',  ( -9.786314039287999478, -78.49005621299899360, 4.837708502169000724 ) ) ;
#43168 = CARTESIAN_POINT ( 'NONE',  ( -7.648026768024999811, -18.75000001589999954, 10.12290050218000026 ) ) ;
#43169 = CARTESIAN_POINT ( 'NONE',  ( 8.124492283498000234, -80.26625923301560306, 7.143800282656999734 ) ) ;
#43170 = CARTESIAN_POINT ( 'NONE',  ( 0.3166755616789259653, -81.00521267096443978, 1.233959662962462067 ) ) ;
#43171 = ORIENTED_EDGE ( 'NONE', *, *, #55762, .F. ) ;
#43172 = ADVANCED_FACE ( 'NONE', ( #4539 ), #57742, .F. ) ;
#43173 = CARTESIAN_POINT ( 'NONE',  ( -10.07627163191000008, -60.04999999725999515, -7.601397897754999633 ) ) ;
#43174 = CIRCLE ( 'NONE', #42194, 10.69999999999999929 ) ;
#43175 = CARTESIAN_POINT ( 'NONE',  ( -2.394033331947576837, -78.62148118236265759, -3.970517693957353877 ) ) ;
#43176 = CARTESIAN_POINT ( 'NONE',  ( 1.633411169670999863, -77.90273522372000059, -11.09730050697999992 ) ) ;
#43177 = CARTESIAN_POINT ( 'NONE',  ( -0.6514878906251000412, -79.74957485841899540, 10.95625855609000077 ) ) ;
#43178 = CARTESIAN_POINT ( 'NONE',  ( 10.42531125070999920, -60.06485145371000556, -7.624341767111000756 ) ) ;
#43179 = CARTESIAN_POINT ( 'NONE',  ( -2.639864145299684939, -84.90520834010136753, -3.072390398173608261 ) ) ;
#43180 = CARTESIAN_POINT ( 'NONE',  ( -1.031652589152999955, -76.69482700115399609, -12.10872576042000048 ) ) ;
#43181 = CARTESIAN_POINT ( 'NONE',  ( 7.247844507162001015, -60.04999999966999980, -9.722718241315000398 ) ) ;
#43182 = CARTESIAN_POINT ( 'NONE',  ( -9.175573575496970946, -62.02695822328879416, 8.792784719842536845 ) ) ;
#43183 = VERTEX_POINT ( 'NONE', #40843 ) ;
#43184 = CARTESIAN_POINT ( 'NONE',  ( -1.246072329358421271, -80.09278992987992751, 0.1233981338585028870 ) ) ;
#43185 = AXIS2_PLACEMENT_3D ( 'NONE', #28939, #54937, #37506 ) ;
#43186 = CARTESIAN_POINT ( 'NONE',  ( 0.01090852172292994249, -75.80000000000002558, -11.82854724701027038 ) ) ;
#43187 = ADVANCED_FACE ( 'NONE', ( #36117 ), #9447, .F. ) ;
#43188 = CARTESIAN_POINT ( 'NONE',  ( -9.332307860560000279, -78.63186501710099208, 6.311653060910999535 ) ) ;
#43189 = LINE ( 'NONE', #20742, #23623 ) ;
#43190 = CARTESIAN_POINT ( 'NONE',  ( 7.247844507162001015, -23.25000000000000000, -9.722718241315000398 ) ) ;
#43191 = CARTESIAN_POINT ( 'NONE',  ( -0.9820397338569999413, -80.80308451575899653, -0.7733679338621000099 ) ) ;
#43192 = CARTESIAN_POINT ( 'NONE',  ( -1.356806863440251254, -82.81292558743855636, 0.6692837476566168009 ) ) ;
#43193 = DIRECTION ( 'NONE',  ( -2.582621269620000094E-11, 0.000000000000000000, 1.000000000000000000 ) ) ;
#43194 = ORIENTED_EDGE ( 'NONE', *, *, #29959, .T. ) ;
#43195 = CARTESIAN_POINT ( 'NONE',  ( -11.75000000000000000, -76.04999999999999716, -3.652443742841000169E-09 ) ) ;
#43196 = CARTESIAN_POINT ( 'NONE',  ( -3.075537641221584018, -76.19583333333332575, 11.44417895085269876 ) ) ;
#43197 = ORIENTED_EDGE ( 'NONE', *, *, #38746, .T. ) ;
#43198 = ORIENTED_EDGE ( 'NONE', *, *, #36664, .F. ) ;
#43199 = CARTESIAN_POINT ( 'NONE',  ( -12.77656766269999977, -53.48801851230000182, -0.1555695072194999973 ) ) ;
#43200 = EDGE_LOOP ( 'NONE', ( #27703, #56199, #24030, #31539 ) ) ;
#43201 = ORIENTED_EDGE ( 'NONE', *, *, #26460, .F. ) ;
#43202 = CARTESIAN_POINT ( 'NONE',  ( -10.12544791843921921, -81.00000000000000000, -3.792049412059997238 ) ) ;
#43203 = CARTESIAN_POINT ( 'NONE',  ( -10.64055841416000092, -78.09134770576399376, -2.440058154124999934 ) ) ;
#43204 = FACE_OUTER_BOUND ( 'NONE', #1971, .T. ) ;
#43205 = CARTESIAN_POINT ( 'NONE',  ( 6.533310722863999942, -79.37991332859898819, -6.649273783659000792 ) ) ;
#43206 = CARTESIAN_POINT ( 'NONE',  ( 4.138892081263878531, -76.27265625027465035, -9.986824818711193430 ) ) ;
#43207 = ORIENTED_EDGE ( 'NONE', *, *, #43545, .F. ) ;
#43208 = ORIENTED_EDGE ( 'NONE', *, *, #25617, .T. ) ;
#43209 = CARTESIAN_POINT ( 'NONE',  ( -4.233603723169751198, -77.51295453581894890, 8.224218726036120586 ) ) ;
#43210 = CARTESIAN_POINT ( 'NONE',  ( 0.000000000000000000, -77.10000000000000853, 0.000000000000000000 ) ) ;
#43211 = CARTESIAN_POINT ( 'NONE',  ( 10.12290050124000018, -23.24999999991999644, 7.648026767085999822 ) ) ;
#43212 = CARTESIAN_POINT ( 'NONE',  ( -5.681372509047000641, -78.40538019329399333, -7.867192369580999767 ) ) ;
#43213 = CARTESIAN_POINT ( 'NONE',  ( 3.757989199629905297, -86.09999999999978115, 2.729540522067947173 ) ) ;
#43214 = VECTOR ( 'NONE', #33143, 1000.000000000000000 ) ;
#43215 = EDGE_CURVE ( 'NONE', #57279, #30548, #51164, .T. ) ;
#43216 = CARTESIAN_POINT ( 'NONE',  ( 8.266617305387050862, -61.77234527411995657, 9.697375114829227982 ) ) ;
#43217 = CARTESIAN_POINT ( 'NONE',  ( 0.6295237254636211199, -79.83333333333334281, 1.092232985442824322 ) ) ;
#43218 = CARTESIAN_POINT ( 'NONE',  ( -3.493617039247999934, -80.52908066372398821, -10.33892454317000187 ) ) ;
#43219 = CARTESIAN_POINT ( 'NONE',  ( -0.7646200840319000713, -80.29161764699000514, -1.389155443296000048 ) ) ;
#43220 = CARTESIAN_POINT ( 'NONE',  ( 1.980584515756000030, -60.06485150062000145, 12.76303204342999997 ) ) ;
#43221 = B_SPLINE_CURVE_WITH_KNOTS ( 'NONE', 3,
 ( #42542, #18940, #2109, #20109, #55830, #19230, #38100, #5355, #32199, #32488, #5638, #5932, #41661, #55237, #28653, #50825, #23937, #41955 ),
 .UNSPECIFIED., .F., .F.,
 ( 4, 2, 2, 2, 2, 2, 2, 2, 4 ),
 ( 0.000000000000000000, 0.1250000000000000000, 0.2500000000000000000, 0.3750000000000000000, 0.5000000000000000000, 0.6250000000000000000, 0.7500000000000000000, 0.8750000000000000000, 1.000000000000000000 ),
 .UNSPECIFIED. ) ;
#43222 = CARTESIAN_POINT ( 'NONE',  ( -0.4053727578492293815, -79.64668580460995884, 1.457040148635480703 ) ) ;
#43223 = CARTESIAN_POINT ( 'NONE',  ( 9.449971683680001178, -78.23558667140099487, -2.591602768458999950 ) ) ;
#43224 = CARTESIAN_POINT ( 'NONE',  ( 1.634596122093999959, -79.06557642282000131, 11.63574645295999943 ) ) ;
#43225 = CARTESIAN_POINT ( 'NONE',  ( 2.062597265787999845, -19.21538333566000034, -12.87024489160000051 ) ) ;
#43227 = CARTESIAN_POINT ( 'NONE',  ( 2.015551294784000191, -18.19652295155999866, -12.79857978895000059 ) ) ;
#43226 = CARTESIAN_POINT ( 'NONE',  ( 0.000000000000000000, 4.040000000000000036, 0.000000000000000000 ) ) ;
#43228 = CARTESIAN_POINT ( 'NONE',  ( 3.250000000000000000, -1.350000000000000089, 0.000000000000000000 ) ) ;
#43229 = PRESENTATION_STYLE_ASSIGNMENT (( #34918 ) ) ;
#43230 = CARTESIAN_POINT ( 'NONE',  ( -1.568660613942000071, -1.943195589986999927, -3.467930652269000102 ) ) ;
#43231 = CARTESIAN_POINT ( 'NONE',  ( 3.440865526187972367, -0.9821531737497413150, -0.7873258519433958824 ) ) ;
#43232 = ORIENTED_EDGE ( 'NONE', *, *, #2465, .F. ) ;
#43233 = CARTESIAN_POINT ( 'NONE',  ( 4.044903269867999640, -79.46000000000000796, -8.595856998426999240 ) ) ;
#43234 = EDGE_CURVE ( 'NONE', #49658, #54222, #33213, .T. ) ;
#43235 = CARTESIAN_POINT ( 'NONE',  ( 5.940599228801999379E-14, -5.950000000028910385, 0.000000000000000000 ) ) ;
#43236 = CARTESIAN_POINT ( 'NONE',  ( -12.56594317825999951, -60.05000001354000005, 1.750000000000000000 ) ) ;
#43237 = CARTESIAN_POINT ( 'NONE',  ( -9.283978793531677098, -77.14367230500779726, -1.155228012124903891 ) ) ;
#43238 = CARTESIAN_POINT ( 'NONE',  ( 1.354019794466000182, -1.887630151311999960, 3.211827542139999991 ) ) ;
#43239 = CARTESIAN_POINT ( 'NONE',  ( 0.5021253177900999454, -81.91975631494000254, -1.588436081161999969 ) ) ;
#43240 = CARTESIAN_POINT ( 'NONE',  ( 2.041361922787999994, -79.53503745527798685, -9.423965843603999915 ) ) ;
#43241 = CARTESIAN_POINT ( 'NONE',  ( 6.606680517516895890, -76.92308210898984555, 8.596804040872029873 ) ) ;
#43242 = CARTESIAN_POINT ( 'NONE',  ( 2.056966010086916707, -79.49179605286448691, -9.496002254240691443 ) ) ;
#43243 = CARTESIAN_POINT ( 'NONE',  ( -0.1963495408493605987, -80.11458333333334281, -1.500000000000000444 ) ) ;
#43244 = LINE ( 'NONE', #3377, #2153 ) ;
#43245 = CIRCLE ( 'NONE', #17778, 0.5000000000000004441 ) ;
#43246 = DIRECTION ( 'NONE',  ( 0.000000000000000000, -1.000000000000000000, 0.000000000000000000 ) ) ;
#43247 = EDGE_CURVE ( 'NONE', #41372, #57123, #10425, .T. ) ;
#43248 = DIRECTION ( 'NONE',  ( 0.000000000000000000, 0.000000000000000000, -1.000000000000000000 ) ) ;
#43249 = CARTESIAN_POINT ( 'NONE',  ( -10.42144728442999835, -77.34603694916899030, 3.353826678397000105 ) ) ;
#43250 = EDGE_CURVE ( 'NONE', #45676, #2820, #2164, .T. ) ;
#43251 = CARTESIAN_POINT ( 'NONE',  ( 7.991295277419832921, -76.38438841642825139, -8.615442090525050389 ) ) ;
#43252 = CARTESIAN_POINT ( 'NONE',  ( -6.868829560331000117, -77.06962105010399000, 8.632549730677999023 ) ) ;
#43253 = CARTESIAN_POINT ( 'NONE',  ( -0.3694735273699065181, -81.99927641614389984, 1.197870979555107684 ) ) ;
#43254 = CARTESIAN_POINT ( 'NONE',  ( 1.657805164101999962, -78.58666450191999786, 0.1386405982960000061 ) ) ;
#43255 = CARTESIAN_POINT ( 'NONE',  ( -8.324924863653999196, -77.22734602334399767, 4.923709561474999497 ) ) ;
#43256 = CARTESIAN_POINT ( 'NONE',  ( 12.76303204294999993, -23.26485150694999859, -1.980584515756000030 ) ) ;
#43257 = CARTESIAN_POINT ( 'NONE',  ( -0.001508081476238588370, -3.476049081606229052, 3.262047271239970847 ) ) ;
#43258 = CARTESIAN_POINT ( 'NONE',  ( 8.471468067312940775, -80.29723165198882384, -6.624523487606162497 ) ) ;
#43259 = CARTESIAN_POINT ( 'NONE',  ( 8.779306384098170213, -79.89934045272630669, 6.259721701839533914 ) ) ;
#43260 = CARTESIAN_POINT ( 'NONE',  ( 8.038883227244705054, -75.79999999999998295, 8.916086791020916280 ) ) ;
#43261 = AXIS2_PLACEMENT_3D ( 'NONE', #57357, #4207, #30480 ) ;
#43262 = CARTESIAN_POINT ( 'NONE',  ( 10.52307592342000042, -79.28856900320100465, 5.828552047478999576 ) ) ;
#43263 = LINE ( 'NONE', #30529, #29350 ) ;
#43264 = CARTESIAN_POINT ( 'NONE',  ( 9.492027143945000134, -79.11863103297000066, 6.060972302936999512 ) ) ;
#43265 = ORIENTED_EDGE ( 'NONE', *, *, #7728, .F. ) ;
#43266 = CARTESIAN_POINT ( 'NONE',  ( 7.678657038161719406, -60.59377623463995377, 10.03844138482045523 ) ) ;
#43267 = EDGE_CURVE ( 'NONE', #3300, #25746, #27827, .T. ) ;
#43268 = ORIENTED_EDGE ( 'NONE', *, *, #37608, .F. ) ;
#43269 = VERTEX_POINT ( 'NONE', #28117 ) ;
#43270 = CARTESIAN_POINT ( 'NONE',  ( -1.997276839918484148, -1.427083333333333259, 2.598917237794077018 ) ) ;
#43271 = EDGE_LOOP ( 'NONE', ( #14646, #42903, #18792, #24309 ) ) ;
#43272 = CARTESIAN_POINT ( 'NONE',  ( -0.05183153944128000151, -79.88498827328399443, 3.544331357887999800 ) ) ;
#43273 = CARTESIAN_POINT ( 'NONE',  ( 2.624138108766170152, -79.25253984762679238, 9.130854755080981988 ) ) ;
#43274 = B_SPLINE_SURFACE_WITH_KNOTS ( 'NONE', 3, 3, ( 
 ( #50619, #36725, #37600, #41747, #10757, #37017, #45902, #55916, #5433, #15467, #29035, #24324, #28145, #33457, #1039, #1906, #19024, #55031, #55322, #14577, #19900, #47074, #6602, #32571, #37306, #14866, #752, #32863, #10456, #46492, #6016, #24025, #42039, #1608, #48226 ),
 ( #25764, #16623, #12193, #11906, #16342, #7474, #20761, #21047, #38762, #29314, #11627, #30176, #34893, #52922, #21330, #56204, #7183, #47363, #48500, #6895, #2475, #2193, #57348, #24900, #57063, #25183, #39048, #3336, #12470, #34607, #16913, #7760, #16046, #29885, #30474 ),
 ( #43205, #24614, #43784, #42628, #3051, #20478, #33748, #34030, #20191, #2762, #38474, #51786, #39342, #56779, #38183, #15751, #11336, #52637, #42918, #56492, #52069, #29601, #47655, #34319, #52355, #47943, #25471, #43491, #100, #26909, #17780, #40505, #44065, #58217, #8621 ),
 ( #18075, #36069, #8043, #39909, #17480, #3613, #44939, #31036, #54090, #3896, #21618, #4784, #53207, #22786, #18365, #31626, #53495, #40794, #39623, #27199, #35175, #17186, #22195, #8330, #9212, #4496, #389, #57631, #21899, #40207, #36359, #30751, #13038, #4198, #12755 ) ),
 .UNSPECIFIED., .F., .F., .F.,
 ( 4, 4 ),
 ( 4, 1, 1, 1, 1, 1, 1, 1, 1, 1, 1, 1, 1, 1, 1, 1, 1, 1, 1, 1, 1, 1, 1, 1, 1, 1, 1, 1, 1, 1, 1, 1, 4 ),
 ( -0.1377334280162000046, 1.137733428016000081 ),
 ( -0.02000000000000000042, 0.01250000000000000069, 0.04499999999999999833, 0.07749999999999999944, 0.1100000000000000006, 0.1424999999999999878, 0.1749999999999999889, 0.2074999999999999900, 0.2399999999999999911, 0.2725000000000000200, 0.3049999999999999933, 0.3375000000000000222, 0.3699999999999999956, 0.4025000000000000244, 0.4349999999999999978, 0.4675000000000000266, 0.5000000000000000000, 0.5324999999999999734, 0.5649999999999999467, 0.5975000000000000311, 0.6300000000000000044, 0.6624999999999999778, 0.6949999999999999512, 0.7275000000000000355, 0.7600000000000000089, 0.7924999999999999822, 0.8249999999999999556, 0.8575000000000000400, 0.8900000000000000133, 0.9224999999999999867, 0.9549999999999999600, 0.9875000000000000444, 1.020000000000000018 ),
 .UNSPECIFIED. ) ;
#43275 = ORIENTED_EDGE ( 'NONE', *, *, #42729, .F. ) ;
#43276 = CARTESIAN_POINT ( 'NONE',  ( -0.7673595064252045628, -82.67326891823354629, -0.9989183397387743080 ) ) ;
#43277 = CARTESIAN_POINT ( 'NONE',  ( 1.026866341085000007E-14, -0.1000000000000002554, 0.000000000000000000 ) ) ;
#43278 = ORIENTED_EDGE ( 'NONE', *, *, #11514, .T. ) ;
#43279 = DIRECTION ( 'NONE',  ( 0.000000000000000000, -1.000000000000000000, 6.735201558252998979E-11 ) ) ;
#43280 = CARTESIAN_POINT ( 'NONE',  ( -1.455755625768786476, -79.22883914762999780, 0.3955483087397376751 ) ) ;
#43281 = CARTESIAN_POINT ( 'NONE',  ( -10.98465012826174281, -18.69514063119217795, 0.5809631169955963292 ) ) ;
#43282 = CARTESIAN_POINT ( 'NONE',  ( -6.933401639485825108, -80.03115928570328208, 8.214959689914797636 ) ) ;
#43283 = FACE_OUTER_BOUND ( 'NONE', #14571, .T. ) ;
#43284 = VECTOR ( 'NONE', #22657, 1000.000000000000114 ) ;
#43285 = CARTESIAN_POINT ( 'NONE',  ( -9.478938303170380664, -77.25897152220545649, -1.070660778503142785 ) ) ;
#43286 = CARTESIAN_POINT ( 'NONE',  ( -11.08400893143999966, -76.41231303454900115, -1.489506537590000068 ) ) ;
#43287 = B_SPLINE_CURVE_WITH_KNOTS ( 'NONE', 3,
 ( #48023, #39134, #20839, #56861, #57146, #52434, #24697, #55997, #7842, #52150, #48304, #43289, #52722, #47734, #11417, #15838, #51578, #2843 ),
 .UNSPECIFIED., .F., .F.,
 ( 4, 2, 2, 2, 2, 2, 2, 2, 4 ),
 ( 0.000000000000000000, 0.1250000000000000278, 0.2500000000000000000, 0.3750000000000001110, 0.5000000000000001110, 0.6250000000000001110, 0.7500000000000002220, 0.8750000000000001110, 1.000000000000000000 ),
 .UNSPECIFIED. ) ;
#43288 = CARTESIAN_POINT ( 'NONE',  ( -9.545928121132844169, -76.56127930255610181, 5.170097460472787176 ) ) ;
#43289 = CARTESIAN_POINT ( 'NONE',  ( 5.539808784079868431, -78.53333333333334565, 9.611650271896850839 ) ) ;
#43290 = CARTESIAN_POINT ( 'NONE',  ( -8.730066282802408040, -78.62683183961394207, -3.057454265489415679 ) ) ;
#43291 = CIRCLE ( 'NONE', #2753, 0.5000000000000006661 ) ;
#43292 = CARTESIAN_POINT ( 'NONE',  ( -10.80277078588560968, -80.11543121848195881, -2.112588677537822424 ) ) ;
#43293 = CARTESIAN_POINT ( 'NONE',  ( 2.156866207458188356, -2.917591387413716486, 2.431545018423679316 ) ) ;
#43294 = CARTESIAN_POINT ( 'NONE',  ( -1.296842085168999903, -78.79842549782625838, -3.346922059760999879 ) ) ;
#43295 = CARTESIAN_POINT ( 'NONE',  ( -10.71959597024094357, -78.09352535383699490, 0.8823199016135090389 ) ) ;
#43296 = AXIS2_PLACEMENT_3D ( 'NONE', #55037, #19322, #45618 ) ;
#43297 = DIRECTION ( 'NONE',  ( -1.000000000000000000, 0.000000000000000000, 0.000000000000000000 ) ) ;
#43298 = FILL_AREA_STYLE_COLOUR ( '', #11341 ) ;
#43299 = CARTESIAN_POINT ( 'NONE',  ( 0.2486648094367000239, -85.07919503318798604, -3.538322792724999832 ) ) ;
#43300 = CARTESIAN_POINT ( 'NONE',  ( 10.35845616727999996, -23.29778595484999926, 7.627487606609999915 ) ) ;
#43301 = CARTESIAN_POINT ( 'NONE',  ( -5.413904038987176648, -80.08333333333331439, -9.393203674808267678 ) ) ;
#43302 = ADVANCED_FACE ( 'NONE', ( #6574 ), #54932, .F. ) ;
#43303 = CYLINDRICAL_SURFACE ( 'NONE', #17571, 1.750000000000001332 ) ;
#43304 = CARTESIAN_POINT ( 'NONE',  ( 1.460959015002474048, -77.72916666666668561, -0.3926218265389178064 ) ) ;
#43305 = EDGE_CURVE ( 'NONE', #32917, #56978, #32650, .T. ) ;
#43306 = CARTESIAN_POINT ( 'NONE',  ( 0.3926218265389221362, -80.54583333333334849, -1.460959015002473160 ) ) ;
#43307 = CARTESIAN_POINT ( 'NONE',  ( -9.234979314279001983, -77.11421089111999549, -9.168119495123999485 ) ) ;
#43308 = CARTESIAN_POINT ( 'NONE',  ( 7.174506471390958318, -78.28110187774559847, -8.441707957340311097 ) ) ;
#43309 = CARTESIAN_POINT ( 'NONE',  ( 0.000000000000000000, -46.43897132165000130, 0.000000000000000000 ) ) ;
#43310 = CARTESIAN_POINT ( 'NONE',  ( -9.882566678146000427, -76.71850902869999800, -7.174148702167999936 ) ) ;
#43311 = ORIENTED_EDGE ( 'NONE', *, *, #32265, .T. ) ;
#43312 = CARTESIAN_POINT ( 'NONE',  ( -9.578166812159000898, -80.20588336572043886, 5.930253639819999201 ) ) ;
#43313 = CARTESIAN_POINT ( 'NONE',  ( -9.457088349255998949, -80.32379509945388918, -6.375823316407999819 ) ) ;
#43314 = EDGE_CURVE ( 'NONE', #56774, #24789, #19869, .T. ) ;
#43315 = FACE_OUTER_BOUND ( 'NONE', #25356, .T. ) ;
#43316 = CARTESIAN_POINT ( 'NONE',  ( 10.87611295313000070, -78.78733180935000746, -6.736118790891999275 ) ) ;
#43317 = CARTESIAN_POINT ( 'NONE',  ( -1.667916687244999974, -18.70150862776000267, -12.49168433580000048 ) ) ;
#43318 = CARTESIAN_POINT ( 'NONE',  ( -1.160011803644999784, -79.07221935430098370, -9.451177169703999681 ) ) ;
#43319 = CARTESIAN_POINT ( 'NONE',  ( 2.190920801479000257, -85.71183183321298316, 3.550554600649999948 ) ) ;
#43320 = CARTESIAN_POINT ( 'NONE',  ( -13.00000000000000000, -6.000000000000000000, 0.000000000000000000 ) ) ;
#43321 = CARTESIAN_POINT ( 'NONE',  ( 1.199999995321999968, -75.00000000467838390, 7.200000027511999079 ) ) ;
#43322 = ORIENTED_EDGE ( 'NONE', *, *, #13088, .F. ) ;
#43323 = CARTESIAN_POINT ( 'NONE',  ( 9.249483092228999226, -78.85084128437098627, 0.09778817195952001218 ) ) ;
#43324 = VECTOR ( 'NONE', #25548, 1000.000000000000114 ) ;
#43325 = CARTESIAN_POINT ( 'NONE',  ( 2.758540696617810983, -78.99078869009431969, -2.352279292788579390 ) ) ;
#43326 = EDGE_LOOP ( 'NONE', ( #10685, #6276, #57191, #43895 ) ) ;
#43327 = CARTESIAN_POINT ( 'NONE',  ( 10.52250585264000016, -78.59875340478899375, -2.994108701640999737 ) ) ;
#43328 = CARTESIAN_POINT ( 'NONE',  ( -8.190859204290999784, -55.64999999967000122, -7.342331066867000544 ) ) ;
#43329 = CARTESIAN_POINT ( 'NONE',  ( -7.155892224914999211, -79.94076805110799455, -8.639911640714998953 ) ) ;
#43330 = VERTEX_POINT ( 'NONE', #51466 ) ;
#43331 = ORIENTED_EDGE ( 'NONE', *, *, #51494, .T. ) ;
#43332 = ORIENTED_EDGE ( 'NONE', *, *, #49299, .F. ) ;
#43333 = AXIS2_PLACEMENT_3D ( 'NONE', #52991, #8114, #16692 ) ;
#43334 = CARTESIAN_POINT ( 'NONE',  ( -0.2640682808882320876, -80.49207712388174230, 1.221730848296998628 ) ) ;
#43335 = CARTESIAN_POINT ( 'NONE',  ( 7.216918803465672383, -78.02046273671660970, 9.394863879516428540 ) ) ;
#43336 = CARTESIAN_POINT ( 'NONE',  ( -7.545891804452000251, -80.07541666714000428, 6.201630566990999682 ) ) ;
#43337 = ORIENTED_EDGE ( 'NONE', *, *, #56544, .F. ) ;
#43338 = CARTESIAN_POINT ( 'NONE',  ( 0.4257466702800756231, -2.465754650056851904, 3.247861184464477802 ) ) ;
#43339 = VERTEX_POINT ( 'NONE', #41425 ) ;
#43340 = CARTESIAN_POINT ( 'NONE',  ( 11.03890801094999929, -78.76413212360631633, -5.342433469444999972 ) ) ;
#43341 = CARTESIAN_POINT ( 'NONE',  ( -3.699342691684420537, -79.00321104920828930, 0.06973985258851372881 ) ) ;
#43342 = ADVANCED_FACE ( 'NONE', ( #24292 ), #5985, .F. ) ;
#43343 = CARTESIAN_POINT ( 'NONE',  ( 7.760941378042000238, -54.56914109158999793, 10.15321372494000052 ) ) ;
#43344 = CARTESIAN_POINT ( 'NONE',  ( 10.03847181063950345, -55.00634590446509264, 7.678636148863391853 ) ) ;
#43345 = CARTESIAN_POINT ( 'NONE',  ( 1.980584515756000030, -60.06485150062000145, 12.76303204342999997 ) ) ;
#43346 = CARTESIAN_POINT ( 'NONE',  ( -7.402774007061660555, -79.10527913613843509, -6.306492414806010416 ) ) ;
#43347 = CARTESIAN_POINT ( 'NONE',  ( 3.399186938124000079, -81.00000000000000000, -10.46162167925000119 ) ) ;
#43348 = CARTESIAN_POINT ( 'NONE',  ( -0.4635254915624000271, -77.75000000000000000, 1.426584774443000025 ) ) ;
#43349 = CARTESIAN_POINT ( 'NONE',  ( -3.331633925631045656, -81.84114584730329511, -2.236105189373023272 ) ) ;
#43350 = CARTESIAN_POINT ( 'NONE',  ( -1.771468677314999907, -75.83449150267999528, 12.18184739844999953 ) ) ;
#43351 = CARTESIAN_POINT ( 'NONE',  ( -1.151390654609000030, -81.41057046129098751, 4.010092854424000208 ) ) ;
#43352 = CARTESIAN_POINT ( 'NONE',  ( -5.838193839761687265, -77.97291666666664867, -7.596835002782715840 ) ) ;
#43353 = DIRECTION ( 'NONE',  ( 9.217554798189211692E-07, 4.180954627647226425E-20, -0.9999999999995752287 ) ) ;
#43354 = CARTESIAN_POINT ( 'NONE',  ( -12.26143800982999998, -78.94953869689999237, -0.2371146996492999870 ) ) ;
#43355 = CARTESIAN_POINT ( 'NONE',  ( 12.50000000000000000, -54.11640971901999819, -1.003652782195000093 ) ) ;
#43356 = CARTESIAN_POINT ( 'NONE',  ( 0.000000000000000000, -76.00000000000000000, 0.000000000000000000 ) ) ;
#43357 = CYLINDRICAL_SURFACE ( 'NONE', #23894, 1.750000000000000000 ) ;
#43359 = EDGE_CURVE ( 'NONE', #25591, #17264, #5407, .T. ) ;
#43358 = CARTESIAN_POINT ( 'NONE',  ( 1.384776930952473339, -80.53739268436684995, 0.6934519277319081132 ) ) ;
#43360 = CARTESIAN_POINT ( 'NONE',  ( 12.61112459821999998, -60.01565178538000112, -1.798929298655999931 ) ) ;
#43361 = CARTESIAN_POINT ( 'NONE',  ( -10.75000000000000000, -77.10000000000000853, 0.000000000000000000 ) ) ;
#43362 = AXIS2_PLACEMENT_3D ( 'NONE', #46830, #51832, #20238 ) ;
#43363 = CARTESIAN_POINT ( 'NONE',  ( 7.223234266884169585, -78.72379502737751977, 9.635782272402776627 ) ) ;
#43364 = CARTESIAN_POINT ( 'NONE',  ( 2.095072722873000171, -3.738360633964000090, -2.362033056849000445 ) ) ;
#43365 = AXIS2_PLACEMENT_3D ( 'NONE', #9494, #27184, #26318 ) ;
#43366 = CARTESIAN_POINT ( 'NONE',  ( 2.263099670254000273, -77.80124539001899109, 11.95244370277000101 ) ) ;
#43367 = CARTESIAN_POINT ( 'NONE',  ( 9.164371241867000251, -77.49332746776399006, -3.297574176498999865 ) ) ;
#43368 = DIRECTION ( 'NONE',  ( 0.000000000000000000, 1.000000000000000000, 0.000000000000000000 ) ) ;
#43369 = CARTESIAN_POINT ( 'NONE',  ( 0.6721823118158000154, -81.41359336816999814, 1.172239651246999914 ) ) ;
#43370 = CARTESIAN_POINT ( 'NONE',  ( 7.685661446562000343, -77.00000000000000000, -5.583959896779000509 ) ) ;
#43371 = ORIENTED_EDGE ( 'NONE', *, *, #32547, .F. ) ;
#43372 = CARTESIAN_POINT ( 'NONE',  ( -10.55911395186000057, -22.78461666469000235, -7.642160924865000204 ) ) ;
#43373 = CARTESIAN_POINT ( 'NONE',  ( -9.584887312353000510, -79.20614542599899721, 7.476966992689000335 ) ) ;
#43374 = B_SPLINE_CURVE_WITH_KNOTS ( 'NONE', 3,
 ( #1889, #50309, #15448, #46471, #14851, #32845 ),
 .UNSPECIFIED., .F., .F.,
 ( 4, 1, 1, 4 ),
 ( 0.000000000000000000, 0.3333333333333000081, 0.6666666666667000474, 1.000000000000000000 ),
 .UNSPECIFIED. ) ;
#43375 = CARTESIAN_POINT ( 'NONE',  ( -8.848325884602834535, -79.28052203371991880, -3.567648052095428568 ) ) ;
#43376 = EDGE_CURVE ( 'NONE', #891, #21680, #41857, .T. ) ;
#43377 = CARTESIAN_POINT ( 'NONE',  ( -2.903215668995137388, -80.00000000000000000, -8.988737031711306003 ) ) ;
#43378 = CARTESIAN_POINT ( 'NONE',  ( -9.317978910689999950, -61.93238462986000314, 8.588869595475999930 ) ) ;
#43379 = DIRECTION ( 'NONE',  ( -0.6562721000562879992, 0.7545243075525860377, 7.877492217643861041E-10 ) ) ;
#43380 = CARTESIAN_POINT ( 'NONE',  ( 9.602680411058999610, -78.97214363870799048, 1.857383748591999950 ) ) ;
#43381 = CARTESIAN_POINT ( 'NONE',  ( -3.600000000000000089, -0.6500000000000000222, 0.000000000000000000 ) ) ;
#43382 = CARTESIAN_POINT ( 'NONE',  ( -5.684557159767956058, -79.07291666666664298, -7.396918292183169541 ) ) ;
#43383 = ORIENTED_EDGE ( 'NONE', *, *, #738, .T. ) ;
#43384 = CARTESIAN_POINT ( 'NONE',  ( 7.764010764699802891, -24.12280919934631029, -9.931043767183597382 ) ) ;
#43385 = CARTESIAN_POINT ( 'NONE',  ( 0.9255272111422516712, -78.91838681312817982, 11.79783862488386426 ) ) ;
#43386 = CARTESIAN_POINT ( 'NONE',  ( 5.941822435829999804, -79.64346001420200594, 7.720072325980000372 ) ) ;
#43387 = CARTESIAN_POINT ( 'NONE',  ( -10.01332852690999964, -60.08056535122999975, -7.654537165486999584 ) ) ;
#43388 = CARTESIAN_POINT ( 'NONE',  ( 1.472546342128999930, -80.54088589475999527, -0.7790162248558000213 ) ) ;
#43389 = VERTEX_POINT ( 'NONE', #11021 ) ;
#43390 = AXIS2_PLACEMENT_3D ( 'NONE', #40278, #17852, #35841 ) ;
#43391 = CARTESIAN_POINT ( 'NONE',  ( -12.50239399162999909, -54.11640749821000185, 1.003653728895000041 ) ) ;
#43392 = CARTESIAN_POINT ( 'NONE',  ( 0.3277380945383860378, -82.24648727505658030, -1.218584741938794069 ) ) ;
#43393 = CARTESIAN_POINT ( 'NONE',  ( 3.912590402935000267, -82.39999999999999147, -0.8316467632710000668 ) ) ;
#43394 = EDGE_CURVE ( 'NONE', #34855, #525, #16470, .T. ) ;
#43395 = CARTESIAN_POINT ( 'NONE',  ( -1.217465845835396188, -78.47916666666667140, 0.3271848554490955907 ) ) ;
#43396 = CARTESIAN_POINT ( 'NONE',  ( -9.699833017908000343, -79.20018498761599801, 1.146274062705999963 ) ) ;
#43397 = ORIENTED_EDGE ( 'NONE', *, *, #27017, .F. ) ;
#43398 = ORIENTED_EDGE ( 'NONE', *, *, #49858, .F. ) ;
#43399 = CARTESIAN_POINT ( 'NONE',  ( -2.034297237242999934, -76.21503136273899770, 12.04999153458000016 ) ) ;
#43400 = CARTESIAN_POINT ( 'NONE',  ( -4.627611545769539703, -78.68975661043700143, -9.702900749146444070 ) ) ;
#43401 = B_SPLINE_CURVE_WITH_KNOTS ( 'NONE', 3,
 ( #6614, #16924, #20772, #39354 ),
 .UNSPECIFIED., .F., .F.,
 ( 4, 4 ),
 ( 0.000000000000000000, 1.000000000000000000 ),
 .UNSPECIFIED. ) ;
#43402 = ORIENTED_EDGE ( 'NONE', *, *, #22210, .F. ) ;
#43403 = CARTESIAN_POINT ( 'NONE',  ( 8.652389292596000203, -16.73734871878000163, 9.414476472810001439 ) ) ;
#43404 = EDGE_CURVE ( 'NONE', #2471, #47498, #3213, .T. ) ;
#43405 = AXIS2_PLACEMENT_3D ( 'NONE', #9892, #13425, #27874 ) ;
#43406 = LINE ( 'NONE', #3539, #18798 ) ;
#43407 = CONICAL_SURFACE ( 'NONE', #29237, 10.04999999996000071, 0.7853981633972997312 ) ;
#43408 = DIRECTION ( 'NONE',  ( 0.000000000000000000, -1.000000000000000000, 1.567264836428999919E-13 ) ) ;
#43409 = CARTESIAN_POINT ( 'NONE',  ( 11.74505801343999956, -76.86614726144999565, 5.470698999298999610 ) ) ;
#43410 = EDGE_CURVE ( 'NONE', #5204, #52919, #38057, .T. ) ;
#43411 = CARTESIAN_POINT ( 'NONE',  ( 0.7035937412390291801, -79.73022787044054382, -10.74960056497591232 ) ) ;
#43412 = DIRECTION ( 'NONE',  ( 1.776356839400000238E-14, -1.000000000000000000, -1.361873576872999870E-13 ) ) ;
#43413 = CARTESIAN_POINT ( 'NONE',  ( -3.131568623105961624, -86.09999999999998010, 1.324114027861469589 ) ) ;
#43414 = CARTESIAN_POINT ( 'NONE',  ( 3.507155896972999898, -79.18358859223100410, 10.65448112794999957 ) ) ;
#43415 = CARTESIAN_POINT ( 'NONE',  ( 3.107115389279428985, -79.94787407444857763, 8.714688932331064564 ) ) ;
#43416 = VERTEX_POINT ( 'NONE', #30150 ) ;
#43417 = CARTESIAN_POINT ( 'NONE',  ( 9.064753713361380250, -78.10522340434667399, 7.545303945706750781 ) ) ;
#43418 = ORIENTED_EDGE ( 'NONE', *, *, #38010, .F. ) ;
#43419 = CARTESIAN_POINT ( 'NONE',  ( -11.25716098398999954, -78.62401457012799710, -0.4530573336216000002 ) ) ;
#43420 = CARTESIAN_POINT ( 'NONE',  ( 7.509078405248583721, -77.30045981524069987, -5.401436182427549859 ) ) ;
#43421 = CARTESIAN_POINT ( 'NONE',  ( -1.312870888196999930, -79.73408011494099412, 0.1301370089704000088 ) ) ;
#43422 = PLANE ( 'NONE',  #41811 ) ;
#43423 = CARTESIAN_POINT ( 'NONE',  ( 11.19968485648553091, -78.09548311650934238, -0.6234324976954068731 ) ) ;
#43424 = CARTESIAN_POINT ( 'NONE',  ( 1.066951212256000092, -78.36019790845671196, 1.077291633113999891 ) ) ;
#43425 = CYLINDRICAL_SURFACE ( 'NONE', #56862, 12.00000000000000000 ) ;
#43426 = CARTESIAN_POINT ( 'NONE',  ( 0.000000000000000000, -0.09999999858569999511, 0.000000000000000000 ) ) ;
#43427 = DIRECTION ( 'NONE',  ( -1.000000000000000000, 0.000000000000000000, 0.000000000000000000 ) ) ;
#43428 = CARTESIAN_POINT ( 'NONE',  ( 0.000000000000000000, -4.000000000000000000, 0.000000000000000000 ) ) ;
#43429 = CARTESIAN_POINT ( 'NONE',  ( -7.653559502277999194, -18.70150862776000267, 10.01234990228999955 ) ) ;
#43430 = B_SPLINE_SURFACE_WITH_KNOTS ( 'NONE', 3, 3, ( 
 ( #11004, #47319, #28988, #51451 ),
 ( #2148, #38136, #15708, #33703 ),
 ( #56447, #51742, #11291, #29271 ),
 ( #6848, #24858, #42874, #38429 ),
 ( #16002, #33989, #52028, #39585 ),
 ( #40465, #32385, #21580, #13293 ),
 ( #35424, #50429, #18032, #35728 ),
 ( #52882, #57882, #44025, #44897 ),
 ( #34850, #30709, #12435, #30428 ),
 ( #4450, #21860, #31286, #54051 ),
 ( #3862, #3576, #9979, #14385 ),
 ( #53756, #49330, #30996, #53454 ),
 ( #39869, #57, #48460, #17438 ),
 ( #48746, #43744, #12998, #17150 ),
 ( #17740, #3297, #49034, #8875 ),
 ( #8581, #26569, #8003, #21289 ),
 ( #35136, #26870, #57589, #53167 ) ),
 .UNSPECIFIED., .F., .F., .F.,
 ( 4, 1, 1, 1, 1, 1, 1, 1, 1, 1, 1, 1, 1, 1, 4 ),
 ( 4, 4 ),
 ( -0.01011408452864000045, 0.000000000000000000, 0.08333333333333001192, 0.1666666666667000196, 0.2500000000000000000, 0.3333333333333000081, 0.4166666666666999919, 0.5000000000000000000, 0.5833333333333000637, 0.6666666666667000474, 0.7500000000000000000, 0.8333333333333000637, 0.9166666666667000474, 1.000000000000000000, 1.010362559107000013 ),
 ( -0.3559705546267999954, 1.357612419580000118 ),
 .UNSPECIFIED. ) ;
#43431 = CARTESIAN_POINT ( 'NONE',  ( 3.197825632618000125, -79.84469609652998656, 10.57600109144000022 ) ) ;
#43432 = CARTESIAN_POINT ( 'NONE',  ( 0.000000000000000000, -74.99999999999998579, 0.000000000000000000 ) ) ;
#43433 = CARTESIAN_POINT ( 'NONE',  ( -3.250000000000000000, -1.500000000000000000, 0.000000000000000000 ) ) ;
#43434 = CARTESIAN_POINT ( 'NONE',  ( -3.380480680714999853, -86.19283349427999497, 0.3694390222027000292 ) ) ;
#43435 = CIRCLE ( 'NONE', #10447, 1.250000000000000000 ) ;
#43436 = ORIENTED_EDGE ( 'NONE', *, *, #14, .T. ) ;
#43438 = EDGE_CURVE ( 'NONE', #28634, #36787, #16017, .T. ) ;
#43437 = CARTESIAN_POINT ( 'NONE',  ( -0.5918520097389999846, -82.92677767037399406, -1.596724312065999962 ) ) ;
#43439 = CARTESIAN_POINT ( 'NONE',  ( 1.367321113498000118, -81.23636901320000447, 0.5356168500207999505 ) ) ;
#43440 = CARTESIAN_POINT ( 'NONE',  ( 0.000000000000000000, -78.79999999980499581, -5.599999999950999729 ) ) ;
#43441 = CARTESIAN_POINT ( 'NONE',  ( -0.7928179559538000021, -78.61804692417699414, -11.95355612866999984 ) ) ;
#43442 = CARTESIAN_POINT ( 'NONE',  ( -12.70556836329126504, -16.77227722666621901, 0.2641978056568241029 ) ) ;
#43443 = CARTESIAN_POINT ( 'NONE',  ( 0.9950501885573103111, -79.05412480003177222, 0.7968050507756183620 ) ) ;
#43444 = CARTESIAN_POINT ( 'NONE',  ( 0.2474615858699362181, -1.880639237606296144, -3.511584093533194117 ) ) ;
#43445 = CARTESIAN_POINT ( 'NONE',  ( 6.482950081930999531, -79.31685194988499177, -6.598019266050999754 ) ) ;
#43446 = CARTESIAN_POINT ( 'NONE',  ( 4.108390852610000366, -78.30356234745399036, -8.590197950816000017 ) ) ;
#43447 = CARTESIAN_POINT ( 'NONE',  ( 0.07980242249672332699, -81.22984433478460176, -1.250509936556952972 ) ) ;
#43448 = CARTESIAN_POINT ( 'NONE',  ( -10.30400671801000101, -77.99980203896599562, 3.605941145585999763 ) ) ;
#43449 = CARTESIAN_POINT ( 'NONE',  ( 11.53347032108356451, -75.96504513096159883, 2.244556689769372948 ) ) ;
#43450 = CARTESIAN_POINT ( 'NONE',  ( 1.078729748401755728, -81.35504527172810185, -0.6795942616195915775 ) ) ;
#43451 = VERTEX_POINT ( 'NONE', #39025 ) ;
#43452 = CARTESIAN_POINT ( 'NONE',  ( 10.98362417419999915, -18.84999999999999787, -0.5999999999999999778 ) ) ;
#43453 = DIRECTION ( 'NONE',  ( 1.000000000000000000, 0.000000000000000000, 0.000000000000000000 ) ) ;
#43454 = CARTESIAN_POINT ( 'NONE',  ( 4.819843862223000208, -79.98410264634560463, -11.11936209286999855 ) ) ;
#43455 = CARTESIAN_POINT ( 'NONE',  ( -0.03763201836869552869, -78.62148118236265759, -3.992727109996482060 ) ) ;
#43456 = EDGE_CURVE ( 'NONE', #14640, #22489, #52042, .T. ) ;
#43457 = B_SPLINE_CURVE_WITH_KNOTS ( 'NONE', 3,
 ( #23470, #1351, #29063, #47105, #6341, #50651, #55355, #6637, #1642, #19055, #24643, #10197, #19345, #37340, #46521, #6046, #19632, #34640, #21361, #47686, #2505 ),
 .UNSPECIFIED., .F., .F.,
 ( 4, 2, 2, 1, 1, 2, 2, 1, 1, 1, 2, 2, 4 ),
 ( 0.000000000000000000, 0.1250000000000000278, 0.2500000000000000555, 0.3750000000000001110, 0.4375000000000001110, 0.4687500000000001110, 0.5000000000000001110, 0.6250000000000002220, 0.6875000000000002220, 0.7187500000000002220, 0.7343750000000001110, 0.7500000000000000000, 1.000000000000000000 ),
 .UNSPECIFIED. ) ;
#43458 = CARTESIAN_POINT ( 'NONE',  ( 1.484562552624000054, -82.04213185391999730, -0.7558657512595999828 ) ) ;
#43459 = CARTESIAN_POINT ( 'NONE',  ( -4.647088938219000376, -78.24288720701400734, 10.20895072913000057 ) ) ;
#43460 = CARTESIAN_POINT ( 'NONE',  ( 3.915498778898000687, -79.21582012609798085, 10.25343288338999947 ) ) ;
#43461 = CARTESIAN_POINT ( 'NONE',  ( 10.53562597589000127, -23.20558297624999966, -7.620013358880999732 ) ) ;
#43462 = EDGE_CURVE ( 'NONE', #41593, #54974, #48892, .T. ) ;
#43463 = CARTESIAN_POINT ( 'NONE',  ( -3.654181822837000215, -86.09999999943198645, 1.626946589673999854 ) ) ;
#43464 = LINE ( 'NONE', #24291, #7245 ) ;
#43465 = CARTESIAN_POINT ( 'NONE',  ( -11.00000000000000533, -79.69292008887531154, 0.9786566581930159492 ) ) ;
#43466 = CARTESIAN_POINT ( 'NONE',  ( -10.10447584125107845, -61.25118490511745506, 7.864774383105175737 ) ) ;
#43467 = EDGE_LOOP ( 'NONE', ( #53263, #58209, #48862 ) ) ;
#43468 = AXIS2_PLACEMENT_3D ( 'NONE', #9325, #27316, #4898 ) ;
#43469 = CARTESIAN_POINT ( 'NONE',  ( 4.752670204043000446, -79.54881202183199207, 10.08299194199999960 ) ) ;
#43470 = CARTESIAN_POINT ( 'NONE',  ( -1.155224866089091806, -80.06903521657417855, 0.4771177278498179852 ) ) ;
#43471 = CARTESIAN_POINT ( 'NONE',  ( 10.13881649148000008, -76.50783510652000530, -5.938594122520999719 ) ) ;
#43472 = CARTESIAN_POINT ( 'NONE',  ( 4.757299607910999484, -78.51949559976999637, 10.21259197296000032 ) ) ;
#43473 = CYLINDRICAL_SURFACE ( 'NONE', #33978, 0.5000000000000004441 ) ;
#43474 = CARTESIAN_POINT ( 'NONE',  ( 3.075537641221509411, -77.65416666666668277, 11.44417895085272008 ) ) ;
#43475 = CARTESIAN_POINT ( 'NONE',  ( 0.000000000000000000, -75.67500000000001137, 0.000000000000000000 ) ) ;
#43476 = CARTESIAN_POINT ( 'NONE',  ( -1.373635873769706306, -82.88377894220877806, -0.6352465044905353242 ) ) ;
#43477 = CARTESIAN_POINT ( 'NONE',  ( -1.146293260019806359, -79.63300943463677584, -0.4980201403389062365 ) ) ;
#43478 = EDGE_CURVE ( 'NONE', #26583, #47291, #21304, .T. ) ;
#43479 = FACE_OUTER_BOUND ( 'NONE', #15746, .T. ) ;
#43480 = CARTESIAN_POINT ( 'NONE',  ( -12.50000000000000000, -39.30476017083000073, 0.000000000000000000 ) ) ;
#43481 = ORIENTED_EDGE ( 'NONE', *, *, #50662, .T. ) ;
#43482 = EDGE_LOOP ( 'NONE', ( #25539, #20111, #36717, #31469 ) ) ;
#43483 = CIRCLE ( 'NONE', #18022, 9.599999999999999645 ) ;
#43484 = CARTESIAN_POINT ( 'NONE',  ( 0.000000000000000000, 0.000000000000000000, 0.000000000000000000 ) ) ;
#43485 = ORIENTED_EDGE ( 'NONE', *, *, #49017, .F. ) ;
#43486 = ORIENTED_EDGE ( 'NONE', *, *, #50654, .T. ) ;
#43487 = CARTESIAN_POINT ( 'NONE',  ( -10.49277749691416162, -81.00000000000000000, -2.475435402500910431 ) ) ;
#43488 = CARTESIAN_POINT ( 'NONE',  ( 8.899710312955001257, -77.27425741570898765, -6.322224476856000308 ) ) ;
#43489 = ITEM_DEFINED_TRANSFORMATION ( 'NONE', 'NONE', #38585,  #43526 ) ;
#43490 = EDGE_CURVE ( 'NONE', #37470, #43629, #16403, .T. ) ;
#43491 = CARTESIAN_POINT ( 'NONE',  ( -7.589275504201999922, -78.24761332859900165, -6.198488971763000066 ) ) ;
#43492 = DIRECTION ( 'NONE',  ( 1.000000000000000000, 0.000000000000000000, 0.000000000000000000 ) ) ;
#43493 = EDGE_LOOP ( 'NONE', ( #19440, #47209, #47131, #53906, #9220 ) ) ;
#43494 = ORIENTED_EDGE ( 'NONE', *, *, #25360, .F. ) ;
#43495 = CARTESIAN_POINT ( 'NONE',  ( -7.272255731327333272, -77.54700831801773120, 5.716658912645681490 ) ) ;
#43496 = AXIS2_PLACEMENT_3D ( 'NONE', #42746, #11454, #33576 ) ;
#43497 = CARTESIAN_POINT ( 'NONE',  ( 5.341789944771999643, -77.64435487080298515, 9.661750877468000098 ) ) ;
#43498 = CARTESIAN_POINT ( 'NONE',  ( -12.54901606610000009, -61.80731603467000213, -0.4733145588201999598 ) ) ;
#43499 = AXIS2_PLACEMENT_3D ( 'NONE', #31532, #32411, #37145 ) ;
#43500 = CARTESIAN_POINT ( 'NONE',  ( -6.473047519705999342, -78.26326104764899583, 7.229824698717000508 ) ) ;
#43501 = CARTESIAN_POINT ( 'NONE',  ( 14.00000000000000000, -32.70420297070000260, 0.000000000000000000 ) ) ;
#43502 = DIRECTION ( 'NONE',  ( 0.000000000000000000, -1.000000000000000000, 0.000000000000000000 ) ) ;
#43503 = CARTESIAN_POINT ( 'NONE',  ( -10.53101998747000145, -18.69360374348000065, 7.613962827178999859 ) ) ;
#43504 = CARTESIAN_POINT ( 'NONE',  ( -1.870137171474999915, -79.92126121676598416, -11.09839649295000008 ) ) ;
#43505 = B_SPLINE_SURFACE_WITH_KNOTS ( 'NONE', 3, 3, ( 
 ( #39634, #11917, #8055, #34041 ),
 ( #11348, #16923, #52079, #26050 ),
 ( #3345, #11637, #29612, #16633 ),
 ( #47667, #39353, #30482, #16350 ),
 ( #34902, #52646, #34330, #57642 ),
 ( #7193, #17196, #29326, #30186 ),
 ( #47373, #21341, #52365, #57360 ),
 ( #29895, #6903, #12201, #7483 ) ),
 .UNSPECIFIED., .F., .F., .F.,
 ( 4, 1, 1, 1, 1, 4 ),
 ( 4, 4 ),
 ( -0.01200407347462999902, 0.000000000000000000, 0.3333333333333000081, 0.6666666666667000474, 1.000000000000000000, 1.011997855551999947 ),
 ( -0.3559705542741000150, 1.355970554273999928 ),
 .UNSPECIFIED. ) ;
#43506 = CARTESIAN_POINT ( 'NONE',  ( 0.9651418585498000580, -79.59702375444000211, 1.402967275931999769 ) ) ;
#43507 = CARTESIAN_POINT ( 'NONE',  ( 1.980584515752000119, -55.53514853344000102, 12.76303204600000107 ) ) ;
#43508 = ORIENTED_EDGE ( 'NONE', *, *, #4383, .F. ) ;
#43509 = CARTESIAN_POINT ( 'NONE',  ( -10.52074280999000067, -76.55859650580799780, 1.981313975351000289 ) ) ;
#43510 = CARTESIAN_POINT ( 'NONE',  ( -3.365558374102000094, -78.40978667140099390, 9.202792326454000360 ) ) ;
#43511 = CARTESIAN_POINT ( 'NONE',  ( 6.035966914210000311, -78.03466243671600466, 10.34809972146999968 ) ) ;
#43512 = CARTESIAN_POINT ( 'NONE',  ( -10.53495272788999948, -18.77289072628000355, -7.618387390369000478 ) ) ;
#43514 = CARTESIAN_POINT ( 'NONE',  ( -0.5154756746316999649, -16.86759400236999795, -12.66205448072999928 ) ) ;
#43513 = CARTESIAN_POINT ( 'NONE',  ( 7.678690995233999672, -57.04351820043999766, 10.59551070214999946 ) ) ;
#43515 = CARTESIAN_POINT ( 'NONE',  ( -9.500000000000000000, -78.79999999999999716, 0.000000000000000000 ) ) ;
#43516 = FILL_AREA_STYLE_COLOUR ( '', #31614 ) ;
#43517 = DIRECTION ( 'NONE',  ( 0.000000000000000000, 0.000000000000000000, 1.000000000000000000 ) ) ;
#43518 = CARTESIAN_POINT ( 'NONE',  ( 10.38236180178000012, -78.04174793274400201, -4.363545344708000151 ) ) ;
#43519 = CARTESIAN_POINT ( 'NONE',  ( -0.1115855426138554346, -3.500000000000000000, 3.288764228670495449 ) ) ;
#43520 = CARTESIAN_POINT ( 'NONE',  ( 3.018788407823380648, -1.457011938536811657, -1.814601626188562689 ) ) ;
#43521 = VERTEX_POINT ( 'NONE', #12164 ) ;
#43522 = CARTESIAN_POINT ( 'NONE',  ( 7.483407197968000801, -77.19999999999998863, -5.437013583705000208 ) ) ;
#43523 = LINE ( 'NONE', #47687, #17342 ) ;
#43524 = CARTESIAN_POINT ( 'NONE',  ( -12.64500484465999897, -19.22847221992000044, 1.799490225533999732 ) ) ;
#43525 = CARTESIAN_POINT ( 'NONE',  ( 2.602549234900000119, -3.533626866276999845, 2.777463315117000064 ) ) ;
#43526 = AXIS2_PLACEMENT_3D ( 'NONE', #45889, #10156, #14564 ) ;
#43527 = CARTESIAN_POINT ( 'NONE',  ( 9.316358549523000576, -79.28289437949098328, 1.425245117218999935 ) ) ;
#43528 = CARTESIAN_POINT ( 'NONE',  ( -12.49996905247000001, -55.60797343434000339, 1.666511841116000037 ) ) ;
#43529 = DIRECTION ( 'NONE',  ( 0.000000000000000000, 1.000000000000000000, 0.000000000000000000 ) ) ;
#43530 = LINE ( 'NONE', #16667, #17201 ) ;
#43531 = CYLINDRICAL_SURFACE ( 'NONE', #32940, 1.750000000000000000 ) ;
#43532 = CARTESIAN_POINT ( 'NONE',  ( -2.299999999999999822, -76.00000000000000000, 0.000000000000000000 ) ) ;
#43533 = CARTESIAN_POINT ( 'NONE',  ( 10.84676810008999936, -77.63163403582298372, 1.484029919422999999 ) ) ;
#43534 = CARTESIAN_POINT ( 'NONE',  ( 5.291843864070292724, -76.36141765332132536, -10.52905727750688847 ) ) ;
#43535 = CARTESIAN_POINT ( 'NONE',  ( -4.618124570880000057, -78.11785646258199733, 10.14532039989999923 ) ) ;
#43536 = CARTESIAN_POINT ( 'NONE',  ( 1.251911631106801481, -81.85749929900767086, 0.1121443075355554597 ) ) ;
#43537 = CARTESIAN_POINT ( 'NONE',  ( 7.648026768019999366, -23.24999998419999869, 10.12290050217000115 ) ) ;
#43538 = FACE_OUTER_BOUND ( 'NONE', #54730, .T. ) ;
#43539 = CARTESIAN_POINT ( 'NONE',  ( 5.684557159767968493, -78.32291666666665719, 7.396918292183160659 ) ) ;
#43540 = CARTESIAN_POINT ( 'NONE',  ( -0.4254240051736147277, -2.614583333333332149, -3.250000000000000888 ) ) ;
#43541 = CARTESIAN_POINT ( 'NONE',  ( -0.3522963194903876993, -80.22251540029562022, -10.74992595684041596 ) ) ;
#43542 = CARTESIAN_POINT ( 'NONE',  ( 1.250000000000000000, -23.25000000000000000, -12.50000000000000000 ) ) ;
#43543 = CARTESIAN_POINT ( 'NONE',  ( -7.861037107735485030, -17.53338873151346178, -10.10708465679509160 ) ) ;
#43544 = CONICAL_SURFACE ( 'NONE', #28438, 3.399999999997999733, 0.9827937232471395390 ) ;
#43545 = EDGE_CURVE ( 'NONE', #55842, #57192, #57037, .T. ) ;
#43546 = VERTEX_POINT ( 'NONE', #33721 ) ;
#43547 = CARTESIAN_POINT ( 'NONE',  ( 7.313768098873999257, -78.82039211992298533, 9.313141831727000053 ) ) ;
#43548 = CARTESIAN_POINT ( 'NONE',  ( -9.722718241315000398, -55.54999999966999980, 7.954951288349001004 ) ) ;
#43549 = CARTESIAN_POINT ( 'NONE',  ( 4.671862542492999815, -78.98244931796000401, -10.24732477002999964 ) ) ;
#43550 = CARTESIAN_POINT ( 'NONE',  ( -5.387453234146290626, -77.51668997339311318, 9.329326193316637372 ) ) ;
#43551 = ORIENTED_EDGE ( 'NONE', *, *, #30419, .F. ) ;
#43552 = LINE ( 'NONE', #11397, #45710 ) ;
#43553 = ORIENTED_EDGE ( 'NONE', *, *, #46771, .F. ) ;
#43554 = VERTEX_POINT ( 'NONE', #11306 ) ;
#43555 = CARTESIAN_POINT ( 'NONE',  ( 3.500000000000000444, -3.500000000000000444, -0.3803866565412687417 ) ) ;
#43556 = CARTESIAN_POINT ( 'NONE',  ( 0.000000000000000000, -86.09999999999999432, 0.000000000000000000 ) ) ;
#43557 = EDGE_CURVE ( 'NONE', #34809, #13233, #22847, .T. ) ;
#43558 = CARTESIAN_POINT ( 'NONE',  ( 2.110329786959999954, -79.28373615087838289, -2.848065553447999942 ) ) ;
#43559 = CARTESIAN_POINT ( 'NONE',  ( -5.911019111731017794, -79.32841036596610707, 7.438469953604046836 ) ) ;
#43560 = ORIENTED_EDGE ( 'NONE', *, *, #15032, .F. ) ;
#43561 = CARTESIAN_POINT ( 'NONE',  ( 0.4026330982763580701, -82.75123106872544554, -1.183384811856946550 ) ) ;
#43562 = CARTESIAN_POINT ( 'NONE',  ( -9.250000000000001776, -79.51041666666667140, -1.210822168571065616 ) ) ;
#43564 = ORIENTED_EDGE ( 'NONE', *, *, #8592, .T. ) ;
#43563 = B_SPLINE_CURVE_WITH_KNOTS ( 'NONE', 3,
 ( #55019, #50606, #10155, #5709, #19302, #16898 ),
 .UNSPECIFIED., .F., .F.,
 ( 4, 1, 1, 4 ),
 ( 0.000000000000000000, 0.3333333333333000081, 0.6666666666667000474, 0.9999998688569559091 ),
 .UNSPECIFIED. ) ;
#43565 = CARTESIAN_POINT ( 'NONE',  ( 0.4406872078701824513, -79.44681088524180268, 1.169590271965520678 ) ) ;
#43566 = DIRECTION ( 'NONE',  ( -1.000000000000000000, 0.000000000000000000, 0.000000000000000000 ) ) ;
#43567 = CARTESIAN_POINT ( 'NONE',  ( 8.395720671197342000, -79.79999999999999716, 8.420963863932922067 ) ) ;
#43568 = B_SPLINE_CURVE_WITH_KNOTS ( 'NONE', 3,
 ( #17734, #31279, #27151, #4740 ),
 .UNSPECIFIED., .F., .F.,
 ( 4, 4 ),
 ( 0.000000000000000000, 1.000000000000000000 ),
 .UNSPECIFIED. ) ;
#43569 = CARTESIAN_POINT ( 'NONE',  ( -10.22053362743914739, -80.07494894966288257, 3.332092116523411640 ) ) ;
#43570 = CARTESIAN_POINT ( 'NONE',  ( 10.50000000000000000, -73.00000000000001421, 0.000000000000000000 ) ) ;
#43571 = CARTESIAN_POINT ( 'NONE',  ( -9.161237776338555960, -77.27573413481378850, -3.065692136626856801 ) ) ;
#43573 = EDGE_CURVE ( 'NONE', #24318, #22028, #36850, .T. ) ;
#43572 = CARTESIAN_POINT ( 'NONE',  ( 8.332845033087998843, -75.95903132946799019, -7.273191856730000460 ) ) ;
#43574 = CARTESIAN_POINT ( 'NONE',  ( -11.87500000004000000, -79.12500000004000356, -1.061343742159000057E-08 ) ) ;
#43575 = CARTESIAN_POINT ( 'NONE',  ( -1.135826688880000157, -81.40663953506998496, -0.9797437077257000748 ) ) ;
#43576 = EDGE_CURVE ( 'NONE', #40202, #515, #22093, .T. ) ;
#43577 = CARTESIAN_POINT ( 'NONE',  ( 5.092348204433999825, -76.79555898269899217, 9.749351101430999478 ) ) ;
#43578 = CARTESIAN_POINT ( 'NONE',  ( -9.250001407686912813, -78.60108681346355297, -0.1266027648973193087 ) ) ;
#43579 = CARTESIAN_POINT ( 'NONE',  ( -1.642669681205999765, -77.61808667140098805, -9.377281606960000460 ) ) ;
#43580 = CONICAL_SURFACE ( 'NONE', #11519, 11.54999999996000071, 0.7853981633972997312 ) ;
#43581 = CARTESIAN_POINT ( 'NONE',  ( -10.89834548151206306, -80.11100334882785035, -1.491191014881230847 ) ) ;
#43582 = CARTESIAN_POINT ( 'NONE',  ( -2.342324693664710189, -3.039369196919617711, 2.252836536559642333 ) ) ;
#43583 = CARTESIAN_POINT ( 'NONE',  ( 3.534916081315999659, -79.41125264934790096, 0.2633100496122000589 ) ) ;
#43584 = CARTESIAN_POINT ( 'NONE',  ( -4.723605729682391008, -78.01121116410763534, 9.658205987086651234 ) ) ;
#43585 = CARTESIAN_POINT ( 'NONE',  ( 1.153890966263953377, -82.88144626544078619, 0.4805918701253220071 ) ) ;
#43586 = CARTESIAN_POINT ( 'NONE',  ( 2.586521478039999877, -84.18624735065199616, 2.423813200681999902 ) ) ;
#43587 = CARTESIAN_POINT ( 'NONE',  ( -0.6934022908089999548, -3.172245813181999718, 3.742362521638999961 ) ) ;
#43588 = CARTESIAN_POINT ( 'NONE',  ( 10.01235002622999914, -23.29848884437999956, 7.653559626096999580 ) ) ;
#43589 = CARTESIAN_POINT ( 'NONE',  ( -8.284635637516000628, -61.84861451525000575, -9.778492910201000754 ) ) ;
#43590 = VECTOR ( 'NONE', #23270, 1000.000000000000000 ) ;
#43591 = CARTESIAN_POINT ( 'NONE',  ( 2.445294723173425666, -79.15875305519165295, 11.79638544041784698 ) ) ;
#43592 = CARTESIAN_POINT ( 'NONE',  ( -0.4870599102559999838, -82.22795905130099925, -1.180149847382000017 ) ) ;
#43593 = CARTESIAN_POINT ( 'NONE',  ( 7.342331066867000544, -59.94999999967000548, -8.190859204290999784 ) ) ;
#43594 = CARTESIAN_POINT ( 'NONE',  ( 11.79660191402999914, -76.80202101964999883, 5.494707494196000575 ) ) ;
#43595 = EDGE_CURVE ( 'NONE', #26455, #56437, #47449, .T. ) ;
#43597 = DIRECTION ( 'NONE',  ( 0.000000000000000000, 1.000000000000000000, 0.000000000000000000 ) ) ;
#43596 = TOROIDAL_SURFACE ( 'NONE', #11576, 1.250000000000000000, 0.5000000000000000000 ) ;
#43598 = CARTESIAN_POINT ( 'NONE',  ( 1.749899258077701747, -23.38716848762994616, -12.55433901290728826 ) ) ;
#43599 = CARTESIAN_POINT ( 'NONE',  ( 3.798386035105999703, -75.73131215493000923, -11.76423408806999937 ) ) ;
#43600 = VERTEX_POINT ( 'NONE', #49935 ) ;
#43601 = AXIS2_PLACEMENT_3D ( 'NONE', #9553, #27245, #49116 ) ;
#43602 = CARTESIAN_POINT ( 'NONE',  ( 9.755626371838998168, -80.95832551581119674, -5.633583086437001342 ) ) ;
#43603 = CARTESIAN_POINT ( 'NONE',  ( 3.812565921075000031, -80.42871315746478444, -10.74951088042000080 ) ) ;
#43604 = B_SPLINE_CURVE_WITH_KNOTS ( 'NONE', 3,
 ( #20454, #56467, #16021, #52045, #25160, #43186, #40772, #366, #30728, #18346, #40481, #57607, #74, #22469, #35744, #12734, #40181, #52902, #22173, #53775, #44324, #13311, #48478, #18053, #49348, #48763 ),
 .UNSPECIFIED., .F., .F.,
 ( 4, 2, 2, 2, 2, 2, 1, 2, 2, 1, 2, 2, 2, 4 ),
 ( 0.000000000000000000, 0.06250000000000009714, 0.1250000000000001943, 0.2500000000000003331, 0.3750000000000004441, 0.5000000000000005551, 0.5625000000000005551, 0.5937500000000004441, 0.6250000000000004441, 0.6875000000000001110, 0.7187500000000000000, 0.7499999999999998890, 0.8750000000000000000, 1.000000000000000000 ),
 .UNSPECIFIED. ) ;
#43605 = CARTESIAN_POINT ( 'NONE',  ( -1.307405465782000009, -81.23633620685998835, 0.09225987258616000219 ) ) ;
#43606 = CARTESIAN_POINT ( 'NONE',  ( 12.59091967951000157, -78.92539409523000415, 1.087091891348999972 ) ) ;
#43607 = CARTESIAN_POINT ( 'NONE',  ( -1.931043762602999925, -19.22180874373999870, -12.75761570870000128 ) ) ;
#43608 = CARTESIAN_POINT ( 'NONE',  ( 9.508660861234000450, -78.70270957562398451, -0.5057122284909000287 ) ) ;
#43609 = CARTESIAN_POINT ( 'NONE',  ( -3.351688600863999667, -82.99100488540000242, 2.489135118475000130 ) ) ;
#43610 = DIRECTION ( 'NONE',  ( -1.000000000000000000, 0.000000000000000000, 0.000000000000000000 ) ) ;
#43611 = CARTESIAN_POINT ( 'NONE',  ( -1.419358333703000019, -79.04332556885799477, 0.07120080608633000407 ) ) ;
#43612 = EDGE_LOOP ( 'NONE', ( #1269, #51549, #54230, #27859, #50902 ) ) ;
#43613 = CARTESIAN_POINT ( 'NONE',  ( 9.178424375319440998, -78.86168501646835693, 1.303869873657260481 ) ) ;
#43614 = CARTESIAN_POINT ( 'NONE',  ( -3.407095545933000569, -78.77851879815550262, -1.429604595782732717E-14 ) ) ;
#43615 = EDGE_LOOP ( 'NONE', ( #48201, #53390, #43678, #10753 ) ) ;
#43616 = CARTESIAN_POINT ( 'NONE',  ( 8.291742182491999458, -78.17736808979898910, 7.136865503491999441 ) ) ;
#43617 = CARTESIAN_POINT ( 'NONE',  ( 12.49306764013999960, -55.51943464808999806, 1.667917367065999912 ) ) ;
#43618 = CARTESIAN_POINT ( 'NONE',  ( -11.27530493984999893, -79.72949423886399245, 1.941616567897000101 ) ) ;
#43619 = ORIENTED_EDGE ( 'NONE', *, *, #57353, .T. ) ;
#43620 = CARTESIAN_POINT ( 'NONE',  ( 3.268459929338999981, -78.83799553730899845, -11.59797143510999895 ) ) ;
#43621 = AXIS2_PLACEMENT_3D ( 'NONE', #55483, #32439, #19181 ) ;
#43622 = ORIENTED_EDGE ( 'NONE', *, *, #11339, .F. ) ;
#43623 = ORIENTED_EDGE ( 'NONE', *, *, #50786, .F. ) ;
#43624 = CARTESIAN_POINT ( 'NONE',  ( -0.4930276506569527539, -80.50736121252504063, 1.148608259268683041 ) ) ;
#43625 = EDGE_CURVE ( 'NONE', #1897, #55907, #43764, .T. ) ;
#43626 = VECTOR ( 'NONE', #53745, 1000.000000000000000 ) ;
#43627 = CARTESIAN_POINT ( 'NONE',  ( -11.75000000000000000, -78.20000000000000284, 1.702919296826999607E-14 ) ) ;
#43628 = CARTESIAN_POINT ( 'NONE',  ( 9.647254834573999460, -80.48752343491251793, -1.526580663425000095 ) ) ;
#43629 = VERTEX_POINT ( 'NONE', #30723 ) ;
#43630 = VERTEX_POINT ( 'NONE', #26582 ) ;
#43631 = CARTESIAN_POINT ( 'NONE',  ( -6.606539651197500973, -80.67294684482473599, -8.596716473525578550 ) ) ;
#43632 = CARTESIAN_POINT ( 'NONE',  ( -0.03211093172565316484, -78.77851879815550262, -3.406944224254369047 ) ) ;
#43633 = CIRCLE ( 'NONE', #17244, 1.250000000000000000 ) ;
#43634 = CARTESIAN_POINT ( 'NONE',  ( 10.13695543446000080, -55.09168900617999753, 7.646071007854999380 ) ) ;
#43635 = CARTESIAN_POINT ( 'NONE',  ( 9.713030931733710460, -54.27705886621562570, 7.970419577022584967 ) ) ;
#43636 = LINE ( 'NONE', #51645, #18546 ) ;
#43637 = CARTESIAN_POINT ( 'NONE',  ( -9.319010416584660561, -79.68098958332934956, 1.219003400097848910 ) ) ;
#43638 = CONICAL_SURFACE ( 'NONE', #19119, 4.899999999795999983, 0.7853981633972997312 ) ;
#43639 = B_SPLINE_CURVE_WITH_KNOTS ( 'NONE', 3,
 ( #1284, #51749, #42594, #38146, #37857, #42302, #33422, #46749, #6858, #19563, #50578, #55282, #56168, #2441, #20443, #47328, #23696, #33125 ),
 .UNSPECIFIED., .F., .F.,
 ( 4, 2, 2, 2, 2, 2, 2, 2, 4 ),
 ( 0.000000000000000000, 0.06250000000000620337, 0.1250000000000124067, 0.2500000000000148215, 0.5000000000000133227, 0.7500000000000117684, 0.8125000000000111022, 0.8750000000000104361, 1.000000000000000000 ),
 .UNSPECIFIED. ) ;
#43640 =( BOUNDED_SURFACE ( )  B_SPLINE_SURFACE ( 3, 3, ( 
 ( #58144, #3830, #26260, #8260 ),
 ( #35389, #30392, #17711, #17407 ),
 ( #39835, #8847, #26838, #34820 ),
 ( #57848, #12401, #53725, #53420 ),
 ( #30963, #48428, #32361, #3544 ),
 ( #27934, #41237, #49000, #45983 ),
 ( #5509, #8547, #40131, #7970 ) ),
 .UNSPECIFIED., .F., .F., .T. ) 
 B_SPLINE_SURFACE_WITH_KNOTS ( ( 4, 3, 4 ),
 ( 4, 4 ),
 ( 0.000000000000000000, 1.000000000000000000, 2.000000000000000000 ),
 ( 0.000000000000000000, 1.000000000000000000 ),
 .UNSPECIFIED. ) 
 GEOMETRIC_REPRESENTATION_ITEM ( )  RATIONAL_B_SPLINE_SURFACE ( (
 ( 1.196373642248999891, 1.184225762575999985, 1.184225762575999985, 1.196373642248999891),
 ( 0.9447739570234999773, 0.9351807998836999536, 0.9351807998836999536, 0.9447739570234999773),
 ( 0.9447739570234999773, 0.9351807998836999536, 0.9351807998836999536, 0.9447739570234999773),
 ( 1.196373642248999891, 1.184225762575999985, 1.184225762575999985, 1.196373642248999891),
 ( 0.9447739570234999773, 0.9351807998836999536, 0.9351807998836999536, 0.9447739570234999773),
 ( 0.9447739570234999773, 0.9351807998836999536, 0.9351807998836999536, 0.9447739570234999773),
 ( 1.196373642248999891, 1.184225762575999985, 1.184225762575999985, 1.196373642248999891) ) ) 
 REPRESENTATION_ITEM ( '' )  SURFACE ( )  );
#43641 = CARTESIAN_POINT ( 'NONE',  ( 0.6431793725385238636, -80.47942011144077412, -11.19244995239323082 ) ) ;
#43642 = ADVANCED_FACE ( 'NONE', ( #4465 ), #40888, .T. ) ;
#43643 = CARTESIAN_POINT ( 'NONE',  ( -10.61596739836999959, -78.68834218451513607, -5.551333230058001611 ) ) ;
#43644 = CARTESIAN_POINT ( 'NONE',  ( 9.073237612486709125, -78.83448602473089295, -1.799436367680483873 ) ) ;
#43645 = CARTESIAN_POINT ( 'NONE',  ( 9.754023262367999436, -76.14578791229999410, -7.509630405475999915 ) ) ;
#43646 = CARTESIAN_POINT ( 'NONE',  ( -4.005234755443000338, -81.65107046129099899, 1.168177984020000171 ) ) ;
#43647 = CARTESIAN_POINT ( 'NONE',  ( 1.478685717397393518, -77.04374999986741557, -9.318529382992288390 ) ) ;
#43648 = CARTESIAN_POINT ( 'NONE',  ( -12.77562786370999959, -16.73761952138000098, 0.5426593252874999385 ) ) ;
#43649 = DIRECTION ( 'NONE',  ( 0.000000000000000000, 1.000000000000000000, 0.000000000000000000 ) ) ;
#43650 = CARTESIAN_POINT ( 'NONE',  ( -4.885220488697999741, -76.40587262140100222, 11.26753068192000029 ) ) ;
#43651 = CARTESIAN_POINT ( 'NONE',  ( 0.000000000000000000, -76.29999999995945359, 0.000000000000000000 ) ) ;
#43652 = CARTESIAN_POINT ( 'NONE',  ( 7.601397897754999633, -55.55000000278000272, -10.07627163191000008 ) ) ;
#43653 = CARTESIAN_POINT ( 'NONE',  ( -1.570796326794885012, -77.91458333333332575, -12.00000000000000178 ) ) ;
#43654 = CARTESIAN_POINT ( 'NONE',  ( 0.01012999788566228306, -81.12444949148175510, 1.533525924451510258 ) ) ;
#43655 = CARTESIAN_POINT ( 'NONE',  ( 12.82202361519000000, -60.22627773000999696, -2.066043355638000012 ) ) ;
#43656 = FACE_OUTER_BOUND ( 'NONE', #53019, .T. ) ;
#43657 = CIRCLE ( 'NONE', #18219, 1.000000000000000000 ) ;
#43658 = CARTESIAN_POINT ( 'NONE',  ( 11.75000000000000000, -76.45000000000000284, 0.000000000000000000 ) ) ;
#43659 = EDGE_CURVE ( 'NONE', #45010, #56496, #24939, .T. ) ;
#43660 = CARTESIAN_POINT ( 'NONE',  ( 3.387743934813999935, -3.312748962127999963, 0.3042514350666000178 ) ) ;
#43661 = CARTESIAN_POINT ( 'NONE',  ( -6.882647548562999873, -78.01827991340999802, -10.03053803679000033 ) ) ;
#43662 = CARTESIAN_POINT ( 'NONE',  ( 0.000000000000000000, -18.84999999999999787, 11.79999999999999893 ) ) ;
#43664 = CARTESIAN_POINT ( 'NONE',  ( 0.9283799206808001081, -78.55482622072899801, 0.9373773696604000838 ) ) ;
#43663 = DIRECTION ( 'NONE',  ( 0.000000000000000000, 1.000000000000000000, 0.000000000000000000 ) ) ;
#43665 = CARTESIAN_POINT ( 'NONE',  ( -1.329983713389000011, -82.10850220804000799, 0.6225684403671000178 ) ) ;
#43666 = CARTESIAN_POINT ( 'NONE',  ( -8.963728694014600151, -79.55351885351645080, 5.934108186058405288 ) ) ;
#43667 = VERTEX_POINT ( 'NONE', #39599 ) ;
#43668 = CARTESIAN_POINT ( 'NONE',  ( -10.53101998747000145, -23.30639625649999758, -7.613962827179999948 ) ) ;
#43669 = CIRCLE ( 'NONE', #18224, 12.80000000000000071 ) ;
#43670 = CARTESIAN_POINT ( 'NONE',  ( -2.877117145850999869, -79.15287816430300438, 11.81089489835999906 ) ) ;
#43671 = CARTESIAN_POINT ( 'NONE',  ( -9.495705824214729418, -79.25230558782985213, -0.2751968363797689388 ) ) ;
#43672 = CARTESIAN_POINT ( 'NONE',  ( -6.603396513061970730, -79.99999999999998579, -6.628355741337830231 ) ) ;
#43673 = CARTESIAN_POINT ( 'NONE',  ( -2.828679940991994712, -76.24010416705776549, -10.52886932951727950 ) ) ;
#43674 = CARTESIAN_POINT ( 'NONE',  ( -3.387669551781999910, -1.642803219816000082, -0.5093631002026000054 ) ) ;
#43675 = CARTESIAN_POINT ( 'NONE',  ( 4.384927929828000615, -79.93236317768199228, -8.866115152190999993 ) ) ;
#43676 = DIRECTION ( 'NONE',  ( 0.000000000000000000, 1.000000000000000000, 0.000000000000000000 ) ) ;
#43677 = CARTESIAN_POINT ( 'NONE',  ( -11.00000000000000000, -78.59999999999999432, 0.000000000000000000 ) ) ;
#43678 = ORIENTED_EDGE ( 'NONE', *, *, #23990, .T. ) ;
#43679 = B_SPLINE_CURVE_WITH_KNOTS ( 'NONE', 3,
 ( #53659, #30040, #44505, #30330, #17061, #17642 ),
 .UNSPECIFIED., .F., .F.,
 ( 4, 2, 4 ),
 ( 0.000000000000000000, 0.5000000000000000000, 1.000000000000000000 ),
 .UNSPECIFIED. ) ;
#43680 = ADVANCED_FACE ( 'NONE', ( #13307 ), #13600, .T. ) ;
#43681 = VECTOR ( 'NONE', #30583, 1000.000000000000000 ) ;
#43682 = CARTESIAN_POINT ( 'NONE',  ( -12.70451796512396037, -53.62354927347614364, 0.5205401190852502191 ) ) ;
#43683 = PLANE ( 'NONE',  #10372 ) ;
#43684 = CARTESIAN_POINT ( 'NONE',  ( 2.815219788740999984, -79.60828667140098958, 9.212769588529999609 ) ) ;
#43685 = CARTESIAN_POINT ( 'NONE',  ( -9.549999999999998934, -79.99999999999998579, 0.000000000000000000 ) ) ;
#43686 = B_SPLINE_CURVE_WITH_KNOTS ( 'NONE', 3,
 ( #38810, #6648, #15800, #20236, #56828, #29361, #24944, #11672, #29648, #47699, #25233, #15209, #19645, #43253, #16383, #28486, #33201, #51249, #21378, #48835, #39393, #44695, #4250, #31086, #7523, #16958, #57108, #58271, #16674, #12238, #11955, #8673, #34655, #8377, #34940, #30802, #13089, #22247, #26375, #26662, #21949, #21666, #40258, #30229, #49123, #44394, #52972, #39961, #3946, #35521, #48272, #43837, #57400, #34367, #12803, #3666, #12522, #30519, #48549, #8096, #39672, #52401, #26092, #52683, #57974, #17530, #3385, #7809, #29933, #44117, #53550, #57678, #47986, #25520, #43536, #3100, #21095 ),
 .UNSPECIFIED., .F., .F.,
 ( 4, 2, 2, 1, 1, 2, 2, 2, 2, 2, 2, 2, 2, 2, 2, 2, 1, 1, 2, 2, 2, 2, 2, 2, 2, 2, 1, 2, 2, 2, 2, 2, 1, 1, 1, 2, 2, 2, 1, 1, 1, 2, 2, 4 ),
 ( 0.000000000000000000, 0.1249999999999903411, 0.1874999999999855671, 0.2187499999999831524, 0.2343749999999819034, 0.2421874999999813205, 0.2499999999999807376, 0.3749999999999688582, 0.4374999999999629186, 0.4687499999999600320, 0.4843749999999581446, 0.4999999999999562572, 0.5312499999999524825, 0.5468749999999509281, 0.5624999999999494849, 0.5937499999999463762, 0.6093749999999444888, 0.6171874999999434896, 0.6210937499999430456, 0.6249999999999424904, 0.6562499999999377165, 0.6718749999999353850, 0.6796874999999346079, 0.6874999999999338307, 0.7187499999999299449, 0.7343749999999280575, 0.7421874999999275024, 0.7460937499999268363, 0.7499999999999260591, 0.8124999999999485967, 0.8437499999999600320, 0.8593749999999655831, 0.8671874999999680256, 0.8710937499999695799, 0.8730468749999700240, 0.8740234374999701350, 0.8749999999999701350, 0.9062499999999734657, 0.9218749999999751310, 0.9296874999999763522, 0.9335937499999772404, 0.9355468749999780176, 0.9374999999999786837, 1.000000000000000000 ),
 .UNSPECIFIED. ) ;
#43687 = AXIS2_PLACEMENT_3D ( 'NONE', #5122, #43597, #23118 ) ;
#43688 = CARTESIAN_POINT ( 'NONE',  ( 3.699999999670000150, -78.39678895079168797, 0.000000000000000000 ) ) ;
#43689 = CARTESIAN_POINT ( 'NONE',  ( 0.9441861370063999725, -79.65665688321999482, 1.372505234203999835 ) ) ;
#43690 = VERTEX_POINT ( 'NONE', #22758 ) ;
#43691 = CARTESIAN_POINT ( 'NONE',  ( 9.179330843189999811, -77.22671943548499485, 6.243840602170999787 ) ) ;
#43692 = CARTESIAN_POINT ( 'NONE',  ( 10.14950121160999963, -56.04922972508000356, -7.674627477461999803 ) ) ;
#43693 = CARTESIAN_POINT ( 'NONE',  ( 2.062597265787999845, -56.01538333533000014, -12.87024489158000051 ) ) ;
#43694 = CARTESIAN_POINT ( 'NONE',  ( -12.80896991328000034, -57.04546192861999998, 1.930989179114000143 ) ) ;
#43695 = CARTESIAN_POINT ( 'NONE',  ( -0.9995835529977281642, -78.44791666666662877, 0.7681833999686391579 ) ) ;
#43696 = ADVANCED_FACE ( 'NONE', ( #70 ), #53181, .T. ) ;
#43697 = CARTESIAN_POINT ( 'NONE',  ( 8.985706068735000329, -79.42749359542099796, -3.828549499589000149 ) ) ;
#43698 = VERTEX_POINT ( 'NONE', #35740 ) ;
#43699 = EDGE_LOOP ( 'NONE', ( #5497, #40211 ) ) ;
#43700 = CARTESIAN_POINT ( 'NONE',  ( -4.960656284159999707, -76.66641898352099815, 11.44151978677999892 ) ) ;
#43701 = CARTESIAN_POINT ( 'NONE',  ( 5.478873870300920323, -78.76767635739062712, -9.249568154307317158 ) ) ;
#43702 = EDGE_CURVE ( 'NONE', #10013, #25387, #51270, .T. ) ;
#43703 = ORIENTED_EDGE ( 'NONE', *, *, #50035, .T. ) ;
#43704 = CARTESIAN_POINT ( 'NONE',  ( -11.00000000000000711, -77.68958333333333144, 1.439896632895276696 ) ) ;
#43705 = CARTESIAN_POINT ( 'NONE',  ( -12.00000000000000000, -79.79999999999999716, 6.639246269807000381E-13 ) ) ;
#43706 = CARTESIAN_POINT ( 'NONE',  ( -3.110005734825000090, -78.15040178014000105, 12.25287980954000133 ) ) ;
#43707 = DIRECTION ( 'NONE',  ( -0.7026410690473250398, -0.1122098755728047209, -0.7026410690473250398 ) ) ;
#43708 = CARTESIAN_POINT ( 'NONE',  ( -9.050966799188000067, -59.94999999969999749, 7.919595949288999570 ) ) ;
#43709 = CARTESIAN_POINT ( 'NONE',  ( -3.131568623105350113, -86.12609999968211127, 1.324114027861438503 ) ) ;
#43710 = AXIS2_PLACEMENT_3D ( 'NONE', #2737, #42891, #16886 ) ;
#43711 = FACE_OUTER_BOUND ( 'NONE', #21473, .T. ) ;
#43712 = CARTESIAN_POINT ( 'NONE',  ( 1.314364188573257319, -79.96416879256437937, 9.155857543867112369 ) ) ;
#43713 = ADVANCED_FACE ( 'NONE', ( #35439 ), #4171, .F. ) ;
#43714 = EDGE_LOOP ( 'NONE', ( #219, #41121, #16179, #4028, #33692 ) ) ;
#43715 = B_SPLINE_CURVE_WITH_KNOTS ( 'NONE', 3,
 ( #28412, #37867, #32836, #10730, #55888, #23125, #1879, #46459, #36698, #28709, #41717, #19288, #27829, #50883, #1293, #37278, #19572, #54715 ),
 .UNSPECIFIED., .F., .F.,
 ( 4, 2, 2, 2, 2, 2, 2, 2, 4 ),
 ( 0.000000000000000000, 0.1250000000000000833, 0.2500000000000001665, 0.3750000000000001665, 0.5000000000000002220, 0.6250000000000002220, 0.7500000000000001110, 0.8750000000000001110, 1.000000000000000000 ),
 .UNSPECIFIED. ) ;
#43716 = CARTESIAN_POINT ( 'NONE',  ( -1.250000000000000000, -82.25000000000000000, 8.279869130157999738E-11 ) ) ;
#43717 = VERTEX_POINT ( 'NONE', #13010 ) ;
#43718 = CARTESIAN_POINT ( 'NONE',  ( -2.226613147434000073, -78.51164515279698719, 11.04405396508999893 ) ) ;
#43719 = CARTESIAN_POINT ( 'NONE',  ( 6.769035029585133145, -77.29037018802434034, -6.304485289422735228 ) ) ;
#43720 = CARTESIAN_POINT ( 'NONE',  ( 0.2147767365671000017, -80.43441590662199303, -1.401402989476999927 ) ) ;
#43721 = CARTESIAN_POINT ( 'NONE',  ( 1.250000000000000222, -83.23958333333330017, -0.1636246173744659582 ) ) ;
#43722 = CARTESIAN_POINT ( 'NONE',  ( -1.265160441076000009, -79.08784971804600161, -0.7115061034973000353 ) ) ;
#43723 = AXIS2_PLACEMENT_3D ( 'NONE', #25205, #2780, #52087 ) ;
#43724 = DIRECTION ( 'NONE',  ( 0.000000000000000000, 0.000000000000000000, -1.000000000000000000 ) ) ;
#43725 = CARTESIAN_POINT ( 'NONE',  ( 12.50728313511535816, -53.80024825452284887, -0.1773837592813573005 ) ) ;
#43726 = CARTESIAN_POINT ( 'NONE',  ( 5.539808784079867543, -78.43333333333333712, 9.611650271896852615 ) ) ;
#43727 = DIRECTION ( 'NONE',  ( 0.000000000000000000, 1.000000000000000000, 0.000000000000000000 ) ) ;
#43728 = CARTESIAN_POINT ( 'NONE',  ( -1.120375320789137374, -79.13669362328037948, -0.5555032894416228606 ) ) ;
#43729 = CARTESIAN_POINT ( 'NONE',  ( -2.977158780993999887, -78.95343179000198575, 10.75305190397999944 ) ) ;
#43730 = CARTESIAN_POINT ( 'NONE',  ( 10.35845608625999859, -23.29778754190000001, -7.627487525415999947 ) ) ;
#43731 = CARTESIAN_POINT ( 'NONE',  ( -8.850953919802000414, -79.70920438397355667, -8.146641040006999290 ) ) ;
#43732 = CARTESIAN_POINT ( 'NONE',  ( -1.507575758304999791, -78.96791748997289062, -3.890205925644000029 ) ) ;
#43733 = CARTESIAN_POINT ( 'NONE',  ( 10.74999999999999645, -77.76041666666667140, 1.407171709420451666 ) ) ;
#43734 = ORIENTED_EDGE ( 'NONE', *, *, #11308, .T. ) ;
#43735 = CARTESIAN_POINT ( 'NONE',  ( 0.7233469165846999616, -82.98993688548499392, -1.541617362406000113 ) ) ;
#43736 = CARTESIAN_POINT ( 'NONE',  ( -0.3011984493834000132, -79.78354959200999019, 1.556817658704999996 ) ) ;
#43737 = DIRECTION ( 'NONE',  ( 0.000000000000000000, -1.000000000000000000, 0.000000000000000000 ) ) ;
#43738 = CARTESIAN_POINT ( 'NONE',  ( 5.537129384246000541, -78.83508144756699210, 10.62336504503000079 ) ) ;
#43739 = CARTESIAN_POINT ( 'NONE',  ( 11.00000000000000000, -76.04999999999999716, -1.235097113410999977E-09 ) ) ;
#43740 = CARTESIAN_POINT ( 'NONE',  ( 1.531359430757999851, -82.42897292706200574, -0.6558942768039000004 ) ) ;
#43741 = CARTESIAN_POINT ( 'NONE',  ( -8.070845824547967950, -76.33295874851062024, 8.970534776983710046 ) ) ;
#43742 = CARTESIAN_POINT ( 'NONE',  ( 5.279327442448000340, -79.24223138344899553, -7.780650776298999816 ) ) ;
#43743 = CARTESIAN_POINT ( 'NONE',  ( 9.480930971721999612, -78.90046275916299123, 0.8843128721991000418 ) ) ;
#43744 = CARTESIAN_POINT ( 'NONE',  ( -1.890224871708999999, -55.05210751953000425, -12.68696160870999989 ) ) ;
#43745 = CARTESIAN_POINT ( 'NONE',  ( -7.710095619854000937, -20.24935285776999905, 10.18496935401000059 ) ) ;
#43746 = CARTESIAN_POINT ( 'NONE',  ( 9.815103194665955044, -75.99628344196712249, 6.459577566555076977 ) ) ;
#43747 = CARTESIAN_POINT ( 'NONE',  ( -1.222766595631025854, -81.67307490878640408, -0.3613108255141002645 ) ) ;
#43748 = ORIENTED_EDGE ( 'NONE', *, *, #33558, .F. ) ;
#43749 = CARTESIAN_POINT ( 'NONE',  ( 10.98961866300693657, -18.48267221962651163, -0.4810437121500372171 ) ) ;
#43750 = CARTESIAN_POINT ( 'NONE',  ( -10.19670478072613307, -77.15724104849601872, 5.890804208869317549 ) ) ;
#43751 = CARTESIAN_POINT ( 'NONE',  ( -10.21995024406999875, -79.77991147651499659, 6.792424309783999803 ) ) ;
#43752 = DIRECTION ( 'NONE',  ( 0.000000000000000000, 1.000000000000000000, 0.000000000000000000 ) ) ;
#43753 = CARTESIAN_POINT ( 'NONE',  ( -9.091539081997000338, -78.82252716544098803, 6.148815634104000338 ) ) ;
#43754 = CARTESIAN_POINT ( 'NONE',  ( 1.417398248412324424, -80.36536458333203825, 10.83463541661525831 ) ) ;
#43755 = B_SPLINE_CURVE_WITH_KNOTS ( 'NONE', 3,
 ( #51644, #43635, #6752, #43063, #43344, #7042, #56349, #3197 ),
 .UNSPECIFIED., .F., .F.,
 ( 4, 2, 2, 4 ),
 ( 0.000000000000000000, 0.5000000000000000000, 0.7500000000000000000, 1.000000000000000000 ),
 .UNSPECIFIED. ) ;
#43756 = CARTESIAN_POINT ( 'NONE',  ( 11.59326225177000147, -76.21977822758400123, 4.362717408256999718 ) ) ;
#43757 = CARTESIAN_POINT ( 'NONE',  ( 7.954951288349001004, -55.35321828636000419, -9.722718241315000398 ) ) ;
#43758 = CARTESIAN_POINT ( 'NONE',  ( -10.36745710150462507, -60.56601929499609582, 7.635228183650350609 ) ) ;
#43759 = ORIENTED_EDGE ( 'NONE', *, *, #17867, .F. ) ;
#43760 = ADVANCED_FACE ( 'NONE', ( #45208 ), #45768, .F. ) ;
#43761 = CARTESIAN_POINT ( 'NONE',  ( 10.05750832943000006, -79.49433933582800194, 4.806363154649000435 ) ) ;
#43762 = CARTESIAN_POINT ( 'NONE',  ( 1.197732772806416435, -79.87413707337499602, 0.3747399189747252501 ) ) ;
#43763 = CARTESIAN_POINT ( 'NONE',  ( 5.539808784079868431, -78.03333333333331723, 9.611650271896850839 ) ) ;
#43764 = CIRCLE ( 'NONE', #55979, 14.00000000000000000 ) ;
#43765 = CARTESIAN_POINT ( 'NONE',  ( -8.774483958462999666, -78.19007837989597931, 6.892026619272999532 ) ) ;
#43766 = DIRECTION ( 'NONE',  ( 0.000000000000000000, 0.000000000000000000, -1.000000000000000000 ) ) ;
#43767 = DIRECTION ( 'NONE',  ( 0.000000000000000000, 1.000000000000000000, 0.000000000000000000 ) ) ;
#43768 = LINE ( 'NONE', #38454, #44416 ) ;
#43769 = CARTESIAN_POINT ( 'NONE',  ( 0.09712307587844953849, -82.47890262923529292, -1.544439509817217893 ) ) ;
#43770 = CARTESIAN_POINT ( 'NONE',  ( -0.4052009782446514552, -79.69920052394734000, -1.182528148650172195 ) ) ;
#43771 = CARTESIAN_POINT ( 'NONE',  ( -9.250000000000000000, -79.99999999999998579, 2.662757480928999879E-14 ) ) ;
#43772 = CARTESIAN_POINT ( 'NONE',  ( 1.799475304559999822, -20.24828923609000242, 12.69616050747999836 ) ) ;
#43773 = DIRECTION ( 'NONE',  ( 1.000000000000000000, 0.000000000000000000, 0.000000000000000000 ) ) ;
#43774 = EDGE_LOOP ( 'NONE', ( #24253, #31768, #30535, #4040 ) ) ;
#43775 = ORIENTED_EDGE ( 'NONE', *, *, #47982, .F. ) ;
#43776 = CARTESIAN_POINT ( 'NONE',  ( -12.43641395959999940, -53.88198970716000247, 0.03481089025435999545 ) ) ;
#43777 = EDGE_CURVE ( 'NONE', #1033, #42976, #21113, .T. ) ;
#43778 = ORIENTED_EDGE ( 'NONE', *, *, #20521, .T. ) ;
#43779 = DIRECTION ( 'NONE',  ( 0.000000000000000000, -1.000000000000000000, 0.000000000000000000 ) ) ;
#43780 = ORIENTED_EDGE ( 'NONE', *, *, #31115, .T. ) ;
#43781 = CARTESIAN_POINT ( 'NONE',  ( 1.500000000000000000, -81.76041666666726826, 0.1963495408493652339 ) ) ;
#43782 = CARTESIAN_POINT ( 'NONE',  ( -3.419437234775999812, -78.17305673476900552, -10.36738907398999920 ) ) ;
#43783 = SHAPE_DEFINITION_REPRESENTATION ( #33367, #46016 ) ;
#43784 = CARTESIAN_POINT ( 'NONE',  ( 2.227885729735000098, -79.33636332859900619, -9.542051086884001165 ) ) ;
#43785 = CARTESIAN_POINT ( 'NONE',  ( 0.01737526028195334263, -78.22524228320165207, -9.249935897884874691 ) ) ;
#43786 = CARTESIAN_POINT ( 'NONE',  ( 4.653115705712000505, -78.85735708466600613, -10.20620521156999949 ) ) ;
#43787 = VECTOR ( 'NONE', #49296, 1000.000000000000114 ) ;
#43788 = ADVANCED_FACE ( 'NONE', ( #3234 ), #34299, .F. ) ;
#43789 = EDGE_LOOP ( 'NONE', ( #26426, #36946, #56666, #12096, #38059, #58047 ) ) ;
#43790 = ORIENTED_EDGE ( 'NONE', *, *, #55553, .T. ) ;
#43791 = CARTESIAN_POINT ( 'NONE',  ( -4.204260939637024741, -77.51267571432379100, 8.239242333927206730 ) ) ;
#43792 = CARTESIAN_POINT ( 'NONE',  ( -5.876696946710000091, -77.38987720147999028, -9.346046374399000101 ) ) ;
#43793 = ADVANCED_FACE ( 'NONE', ( #34500 ), #51965, .F. ) ;
#43794 = DIRECTION ( 'NONE',  ( 0.000000000000000000, 0.000000000000000000, -1.000000000000000000 ) ) ;
#43795 = CIRCLE ( 'NONE', #18343, 12.50000000000000000 ) ;
#43796 = CARTESIAN_POINT ( 'NONE',  ( -12.43647262256999930, -61.71807034702999317, 0.03492325570154000691 ) ) ;
#43797 = CARTESIAN_POINT ( 'NONE',  ( 5.927986824875999261, -78.00744658548798327, -7.683077610609999830 ) ) ;
#43798 = CARTESIAN_POINT ( 'NONE',  ( -2.764837346328719025, -86.09999999999978115, 3.732097096069707742 ) ) ;
#43799 = CARTESIAN_POINT ( 'NONE',  ( -9.500094076791862463, -79.39994338716823563, -4.328536937075411965E-07 ) ) ;
#43800 = CARTESIAN_POINT ( 'NONE',  ( -8.838834764832000701, -18.75000000000000000, 8.838834764832000701 ) ) ;
#43801 = B_SPLINE_CURVE_WITH_KNOTS ( 'NONE', 3,
 ( #57386, #34926, #21080, #3933, #48534, #53534 ),
 .UNSPECIFIED., .F., .F.,
 ( 4, 1, 1, 4 ),
 ( 0.000000000000000000, 0.3333333333333000081, 0.6666666666667000474, 1.000000000000000000 ),
 .UNSPECIFIED. ) ;
#43802 = CARTESIAN_POINT ( 'NONE',  ( 3.942135768300999654, -79.96302238210400049, -10.54187931140000067 ) ) ;
#43803 = CARTESIAN_POINT ( 'NONE',  ( 12.66232176275999954, -16.86513311418999805, -0.5079086068997000769 ) ) ;
#43804 = AXIS2_PLACEMENT_3D ( 'NONE', #15290, #10882, #42460 ) ;
#43805 = CARTESIAN_POINT ( 'NONE',  ( -1.250000000000000000, -80.99999999999998579, 0.000000000000000000 ) ) ;
#43806 = ORIENTED_EDGE ( 'NONE', *, *, #55117, .T. ) ;
#43807 = CARTESIAN_POINT ( 'NONE',  ( -7.622784390041999814, -55.01288991740999990, 10.47836615824999917 ) ) ;
#43808 = DIRECTION ( 'NONE',  ( 0.000000000000000000, -1.000000000000000000, 0.000000000000000000 ) ) ;
#43809 = CARTESIAN_POINT ( 'NONE',  ( -9.038965287783000235, -16.66737759107000372, -9.029769469460999787 ) ) ;
#43811 = LINE ( 'NONE', #3357, #42152 ) ;
#43810 = CARTESIAN_POINT ( 'NONE',  ( 7.705119999413000187, -58.55171076491000548, 10.24996238027999951 ) ) ;
#43812 = ADVANCED_FACE ( 'NONE', ( #7365 ), #47834, .T. ) ;
#43813 = CARTESIAN_POINT ( 'NONE',  ( 0.8492415665292510907, -1.247390030182168541, -3.167727707052294228 ) ) ;
#43814 = CARTESIAN_POINT ( 'NONE',  ( -9.567284400036999870, -80.01536253608898619, 5.522558287099000651 ) ) ;
#43815 = CARTESIAN_POINT ( 'NONE',  ( 12.76303204294000082, -18.73514849292999784, 1.980584515756000030 ) ) ;
#43816 = CARTESIAN_POINT ( 'NONE',  ( -2.194598275924000141, -77.93280256073698808, -11.04616236372000060 ) ) ;
#43817 = CARTESIAN_POINT ( 'NONE',  ( 0.5420726531984851881, -3.499999999999999556, 3.280180941426340979 ) ) ;
#43818 = CARTESIAN_POINT ( 'NONE',  ( -8.796335266380014062, -80.14791666668804737, 6.760013919724027431 ) ) ;
#43819 = ORIENTED_EDGE ( 'NONE', *, *, #19051, .T. ) ;
#43820 = CARTESIAN_POINT ( 'NONE',  ( -4.000000000000000000, -5.000000000000000000, -0.5999999999999999778 ) ) ;
#43821 = CARTESIAN_POINT ( 'NONE',  ( -1.374053708643000007E-14, -74.80000000000001137, 0.000000000000000000 ) ) ;
#43822 = CARTESIAN_POINT ( 'NONE',  ( -26.49999981590656262, -39.30476017083000073, -0.003123612069538085796 ) ) ;
#43823 = CARTESIAN_POINT ( 'NONE',  ( -2.331653612116000307, -3.201240180630999799, -2.802716395477999889 ) ) ;
#43824 = CARTESIAN_POINT ( 'NONE',  ( 4.739049146600000206, -80.18879678548698564, -7.903376716697000148 ) ) ;
#43825 = CARTESIAN_POINT ( 'NONE',  ( -12.65987793659000005, -53.86302453462000273, 0.9847129294438998759 ) ) ;
#43826 = CARTESIAN_POINT ( 'NONE',  ( 4.401050137192186185, -77.19999999999998863, 9.873231036884021705 ) ) ;
#43827 = CARTESIAN_POINT ( 'NONE',  ( -1.636740604697537016, -2.018159380161653083, 2.842028451810316270 ) ) ;
#43828 = CARTESIAN_POINT ( 'NONE',  ( 7.541360678298886455, -79.09749999999999659, -5.846326858574182772 ) ) ;
#43829 = EDGE_CURVE ( 'NONE', #45130, #20752, #33644, .T. ) ;
#43830 = CARTESIAN_POINT ( 'NONE',  ( -3.242402341787999909, -86.35846544543099412, 2.278681733043999902 ) ) ;
#43831 = DIRECTION ( 'NONE',  ( 0.000000000000000000, 0.000000000000000000, 1.000000000000000000 ) ) ;
#43832 = EDGE_CURVE ( 'NONE', #16988, #22076, #34740, .T. ) ;
#43833 = CARTESIAN_POINT ( 'NONE',  ( -11.98222815316549905, -76.96326881833607558, -1.546144727786179951 ) ) ;
#43834 = AXIS2_PLACEMENT_3D ( 'NONE', #10253, #31789, #49832 ) ;
#43835 = CARTESIAN_POINT ( 'NONE',  ( 10.48850619502800718, -76.41229039468936435, -5.300019550382959466 ) ) ;
#43836 = CARTESIAN_POINT ( 'NONE',  ( 7.384237969039999072, -76.82449396308798839, -8.196021229627000082 ) ) ;
#43837 = CARTESIAN_POINT ( 'NONE',  ( 0.8828684872424523711, -81.91318357668050965, 0.8843653071331574189 ) ) ;
#43838 = AXIS2_PLACEMENT_3D ( 'NONE', #7108, #2692, #2116 ) ;
#43839 = CARTESIAN_POINT ( 'NONE',  ( 2.632967082928999947, -77.06260562980078532, 9.306700570505000769 ) ) ;
#43840 = CARTESIAN_POINT ( 'NONE',  ( -8.630067035710000667, -79.54514415034600461, -4.100810385846999750 ) ) ;
#43841 = CARTESIAN_POINT ( 'NONE',  ( 3.250000000000000000, -3.350000000000000089, 0.000000000000000000 ) ) ;
#43842 = CARTESIAN_POINT ( 'NONE',  ( -4.109332157379601114, -80.19416283618738817, -9.933321846854338943 ) ) ;
#43843 = FACE_OUTER_BOUND ( 'NONE', #47182, .T. ) ;
#43844 = CARTESIAN_POINT ( 'NONE',  ( 1.099834709382747855, -79.71709307677275547, 11.16297328563665126 ) ) ;
#43845 = CARTESIAN_POINT ( 'NONE',  ( -6.309004353333000026, -79.07938358726799777, -10.24224633278999796 ) ) ;
#43846 = AXIS2_PLACEMENT_3D ( 'NONE', #45297, #36129, #26669 ) ;
#43847 = CARTESIAN_POINT ( 'NONE',  ( -1.217465845835396188, -81.97916666666667140, 0.3271848554490955907 ) ) ;
#43848 = CARTESIAN_POINT ( 'NONE',  ( -2.721343196572999723, -79.71783057900900360, 10.92832355692000057 ) ) ;
#43849 = B_SPLINE_CURVE_WITH_KNOTS ( 'NONE', 3,
 ( #40823, #35791, #18685, #36677, #50565, #27808, #23396, #415, #13947, #5673, #58243, #31944, #17805, #5104, #26933, #49988, #44964, #45855 ),
 .UNSPECIFIED., .F., .F.,
 ( 4, 2, 2, 2, 2, 2, 2, 2, 4 ),
 ( 0.000000000000000000, 0.1250000000000001665, 0.2500000000000002776, 0.3750000000000002776, 0.5000000000000002220, 0.6250000000000001110, 0.7500000000000001110, 0.8750000000000000000, 1.000000000000000000 ),
 .UNSPECIFIED. ) ;
#43850 = CARTESIAN_POINT ( 'NONE',  ( 6.606255055572026080, -77.42296540801065419, 8.596106853357831312 ) ) ;
#43851 = ORIENTED_EDGE ( 'NONE', *, *, #35602, .T. ) ;
#43852 = CARTESIAN_POINT ( 'NONE',  ( -1.003693376014196836, -24.96223992107934109, 12.70247752664746521 ) ) ;
#43853 = VERTEX_POINT ( 'NONE', #43381 ) ;
#43854 = ORIENTED_EDGE ( 'NONE', *, *, #40836, .F. ) ;
#43855 = CARTESIAN_POINT ( 'NONE',  ( 1.636761686205415067, -1.333333333333332815, 2.839805762151342616 ) ) ;
#43856 = CARTESIAN_POINT ( 'NONE',  ( -12.50000000000000000, -18.75000000310999937, 1.750000000000000000 ) ) ;
#43857 = CARTESIAN_POINT ( 'NONE',  ( -1.778283081280999989, -80.13706584928699783, 3.117924708102000064 ) ) ;
#43858 = CARTESIAN_POINT ( 'NONE',  ( -3.479070826201084543, -79.30455014728846663, 8.840435339296620398 ) ) ;
#43859 = ORIENTED_EDGE ( 'NONE', *, *, #24901, .T. ) ;
#43860 = CARTESIAN_POINT ( 'NONE',  ( -7.826265407172001254, -78.57604920034999907, -9.564588425367000823 ) ) ;
#43861 = ORIENTED_EDGE ( 'NONE', *, *, #23941, .T. ) ;
#43862 = CARTESIAN_POINT ( 'NONE',  ( -4.658475568430814562, -79.58333333333330017, -8.082524092276884176 ) ) ;
#43863 = ORIENTED_EDGE ( 'NONE', *, *, #57812, .F. ) ;
#43864 = CARTESIAN_POINT ( 'NONE',  ( -1.376157783432642834, -77.78360998065747367, -0.6179252952255732678 ) ) ;
#43865 = FACE_OUTER_BOUND ( 'NONE', #16902, .T. ) ;
#43866 = CARTESIAN_POINT ( 'NONE',  ( -4.017030179565191261, -80.00544080255656354, 9.987515399741488054 ) ) ;
#43867 = CARTESIAN_POINT ( 'NONE',  ( 12.00000000000000000, -23.15000000002000036, 0.7999999999999001243 ) ) ;
#43868 = CARTESIAN_POINT ( 'NONE',  ( 3.184161977317942149, -86.31452042059399332, -1.417680250971129707 ) ) ;
#43869 = CARTESIAN_POINT ( 'NONE',  ( 2.076475668830000121, -76.26182138261400212, 10.98918251355999942 ) ) ;
#43870 = CARTESIAN_POINT ( 'NONE',  ( 7.909383950897899140, -79.01041666666978358, 8.790170633244827059 ) ) ;
#43871 = CARTESIAN_POINT ( 'NONE',  ( -3.040431873813000063, -78.13870099961999927, 12.26916943822000050 ) ) ;
#43872 = VECTOR ( 'NONE', #5475, 1000.000000000000114 ) ;
#43873 = CARTESIAN_POINT ( 'NONE',  ( -7.647058570136000100, -76.32652084646099411, 8.064869325795999799 ) ) ;
#43874 = CARTESIAN_POINT ( 'NONE',  ( -8.743226456218904374, -78.62649317345338318, -3.019661628328330405 ) ) ;
#43875 = CARTESIAN_POINT ( 'NONE',  ( 0.9179173133781000082, -81.45982051858098316, 4.026902219962999574 ) ) ;
#43876 = AXIS2_PLACEMENT_3D ( 'NONE', #5078, #23370, #964 ) ;
#43877 = DIRECTION ( 'NONE',  ( 0.000000000000000000, -1.000000000000000000, 0.000000000000000000 ) ) ;
#43878 = CARTESIAN_POINT ( 'NONE',  ( -1.247739402645562823, -3.007575997018046454, 3.000140550506007919 ) ) ;
#43879 = CARTESIAN_POINT ( 'NONE',  ( -3.402924446111000201, -81.57575264934799009, 0.9925064726425999462 ) ) ;
#43880 = VECTOR ( 'NONE', #41552, 1000.000000000000000 ) ;
#43881 = EDGE_CURVE ( 'NONE', #22868, #17863, #19303, .T. ) ;
#43882 = CARTESIAN_POINT ( 'NONE',  ( 0.04193593611180446157, -25.01009741336668313, -12.50649570005624334 ) ) ;
#43883 = CARTESIAN_POINT ( 'NONE',  ( 2.951758530439000161, -82.31344503318798900, -1.687752529438000026 ) ) ;
#43884 = CARTESIAN_POINT ( 'NONE',  ( 3.190249742999000215, -1.986765174611999862, -2.075671974272999876 ) ) ;
#43885 = CARTESIAN_POINT ( 'NONE',  ( -0.5176806821990824758, -80.34214269217306992, -1.165494644203259655 ) ) ;
#43886 = CARTESIAN_POINT ( 'NONE',  ( -7.647093862774999806, -60.16895637605999525, -10.00844027277999970 ) ) ;
#43887 = EDGE_CURVE ( 'NONE', #22028, #6729, #30068, .T. ) ;
#43888 = DIRECTION ( 'NONE',  ( 1.000000000000000000, 0.000000000000000000, 0.000000000000000000 ) ) ;
#43889 = CARTESIAN_POINT ( 'NONE',  ( -0.9657971644277000278, -82.19488396904600336, -0.9195906491977999808 ) ) ;
#43890 = CARTESIAN_POINT ( 'NONE',  ( -12.77306291386999959, -16.94129324301999873, -1.041150512314999999 ) ) ;
#43891 = CARTESIAN_POINT ( 'NONE',  ( 11.85869973992999959, -77.83577122363000456, 5.358216250391999225 ) ) ;
#43892 = CARTESIAN_POINT ( 'NONE',  ( 0.000000000000000000, -6.049999999381999949, -13.94999999937999924 ) ) ;
#43893 = DIRECTION ( 'NONE',  ( 0.7071067811865975328, 0.7071067811864976127, -1.047750255310995327E-09 ) ) ;
#43894 = CARTESIAN_POINT ( 'NONE',  ( -11.70293741273999899, -76.05535392359000468, 3.983108938927999443 ) ) ;
#43895 = ORIENTED_EDGE ( 'NONE', *, *, #36248, .T. ) ;
#43896 = EDGE_CURVE ( 'NONE', #31619, #25098, #33330, .T. ) ;
#43897 = PLANE ( 'NONE',  #52342 ) ;
#43898 = DIRECTION ( 'NONE',  ( 0.000000000000000000, 1.000000000000000000, 0.000000000000000000 ) ) ;
#43899 = CARTESIAN_POINT ( 'NONE',  ( 12.66232158689999920, -61.93482640547999551, 0.5080765942054999984 ) ) ;
#43900 = CARTESIAN_POINT ( 'NONE',  ( 7.655542440091000600, -19.22180874373999870, -10.38645071870000081 ) ) ;
#43901 = CARTESIAN_POINT ( 'NONE',  ( -5.120069445942999842, -77.47345684055298420, -8.157089945504001349 ) ) ;
#43902 = CARTESIAN_POINT ( 'NONE',  ( 4.172307193540000014, -85.46506550819998438, 0.04387830479587000176 ) ) ;
#43903 = CARTESIAN_POINT ( 'NONE',  ( -12.60356226360999798, -22.75077028889999653, 1.750000000000000000 ) ) ;
#43904 = CARTESIAN_POINT ( 'NONE',  ( -1.260178996155999931, -80.14056234758800201, -0.6496216418182000352 ) ) ;
#43905 = ORIENTED_EDGE ( 'NONE', *, *, #6014, .F. ) ;
#43906 = CARTESIAN_POINT ( 'NONE',  ( -10.75000000000000000, -80.00000000000000000, 0.000000000000000000 ) ) ;
#43907 = CARTESIAN_POINT ( 'NONE',  ( -3.699999999670031237, -79.00321104920828930, 7.399999999340018064 ) ) ;
#43908 = ORIENTED_EDGE ( 'NONE', *, *, #29229, .T. ) ;
#43909 = CARTESIAN_POINT ( 'NONE',  ( 8.185910223524000884, -78.06499867246799340, -6.914387615432000977 ) ) ;
#43910 = ADVANCED_FACE ( 'NONE', ( #21225 ), #39230, .T. ) ;
#43911 = CARTESIAN_POINT ( 'NONE',  ( -10.42531125070999920, -60.06485145371000556, 7.624341767111000756 ) ) ;
#43912 = CONICAL_SURFACE ( 'NONE', #53334, 5.199999999809000073, 0.7853981633972997312 ) ;
#43913 = CARTESIAN_POINT ( 'NONE',  ( -1.629734310963000032, -80.48366320050999434, -10.59064910002000026 ) ) ;
#43914 = ORIENTED_EDGE ( 'NONE', *, *, #45725, .T. ) ;
#43915 = EDGE_LOOP ( 'NONE', ( #21455, #54811, #42042, #45834 ) ) ;
#43916 = ORIENTED_EDGE ( 'NONE', *, *, #50253, .T. ) ;
#43917 = FACE_OUTER_BOUND ( 'NONE', #36439, .T. ) ;
#43918 = DIRECTION ( 'NONE',  ( 0.000000000000000000, 0.000000000000000000, -1.000000000000000000 ) ) ;
#43919 = LINE ( 'NONE', #8466, #55342 ) ;
#43920 = EDGE_LOOP ( 'NONE', ( #3735, #6162, #34449, #45892 ) ) ;
#43921 = CYLINDRICAL_SURFACE ( 'NONE', #36523, 11.00000000000000000 ) ;
#43922 = ORIENTED_EDGE ( 'NONE', *, *, #50253, .F. ) ;
#43923 = CARTESIAN_POINT ( 'NONE',  ( 1.179993905018462241, -79.43096596752555172, 0.4803374300081332260 ) ) ;
#43924 = CARTESIAN_POINT ( 'NONE',  ( -3.893811372584298880, -78.96264283715740362, -2.200139326159465281 ) ) ;
#43925 = CARTESIAN_POINT ( 'NONE',  ( 8.292781013277000568, -53.74469293044000295, 9.770415148702999986 ) ) ;
#43926 = CARTESIAN_POINT ( 'NONE',  ( 0.9218200799623692543, -78.22291666666664867, 1.199500263597272687 ) ) ;
#43927 = CARTESIAN_POINT ( 'NONE',  ( -7.473530895688906384, -79.65494791666267815, 5.742368501771844436 ) ) ;
#43928 = CARTESIAN_POINT ( 'NONE',  ( 11.04260898239051514, -80.61365854145890353, 1.935304240822113275 ) ) ;
#43929 = CARTESIAN_POINT ( 'NONE',  ( 4.899854808515000215, -78.30853176858254017, -10.93194800986000459 ) ) ;
#43930 = CARTESIAN_POINT ( 'NONE',  ( 9.041762528755288741, -78.83306936774171447, -1.957752293751276351 ) ) ;
#43931 = CARTESIAN_POINT ( 'NONE',  ( 11.50190934395000042, -76.67499180864999175, -3.421415122956000143 ) ) ;
#43932 = CARTESIAN_POINT ( 'NONE',  ( 3.979601129954999816, -82.48655496681199395, 0.4014263888467000108 ) ) ;
#43933 = CARTESIAN_POINT ( 'NONE',  ( -5.436604004633999843, -77.33488667140099437, -8.108850267457999195 ) ) ;
#43934 = DIRECTION ( 'NONE',  ( -0.9999999999998321343, 0.000000000000000000, -5.794540613806191565E-07 ) ) ;
#43935 = CARTESIAN_POINT ( 'NONE',  ( 12.85140862681000051, -20.24439829998999940, -1.980464483675000054 ) ) ;
#43936 = CARTESIAN_POINT ( 'NONE',  ( 11.13784153760999907, -76.28292440648600348, 5.174080857020999957 ) ) ;
#43937 = CARTESIAN_POINT ( 'NONE',  ( -3.250000000000000000, -2.500000000000000000, 0.000000000000000000 ) ) ;
#43938 = CARTESIAN_POINT ( 'NONE',  ( 2.697037849775999696, -1.612630151311999827, 3.117841812466000118 ) ) ;
#43939 = CARTESIAN_POINT ( 'NONE',  ( 1.570796326794909881, -77.93541666666664014, -11.99999999999999822 ) ) ;
#43940 = B_SPLINE_CURVE_WITH_KNOTS ( 'NONE', 3,
 ( #44205, #54236, #40356, #27053, #53346, #26187, #17927, #53947, #57773, #30607, #13772, #26464, #13482, #22043, #45090, #4642 ),
 .UNSPECIFIED., .F., .F.,
 ( 4, 2, 2, 2, 2, 2, 2, 4 ),
 ( 0.2857224320369311510, 0.3750071280323146738, 0.4642918240276981967, 0.5535765200230817751, 0.6428612160184652424, 0.8214306080092326212, 0.9107153040046163106, 1.000000000000000000 ),
 .UNSPECIFIED. ) ;
#43941 = CARTESIAN_POINT ( 'NONE',  ( -0.8698823052784736554, -80.17301259719361894, 1.277977011521524986 ) ) ;
#43942 = FACE_OUTER_BOUND ( 'NONE', #7599, .T. ) ;
#43943 = CARTESIAN_POINT ( 'NONE',  ( 0.3098463080081999554, -79.21130845337700066, 1.484230999220000013 ) ) ;
#43944 = CARTESIAN_POINT ( 'NONE',  ( -0.3926218265389190276, -78.60416666666667140, -1.460959015002473826 ) ) ;
#43945 = CARTESIAN_POINT ( 'NONE',  ( 1.640804023310000082, -3.633545964575999765, -2.958959333410000170 ) ) ;
#43946 = AXIS2_PLACEMENT_3D ( 'NONE', #49249, #43529, #52674 ) ;
#43947 = CARTESIAN_POINT ( 'NONE',  ( 12.16237383090999913, -77.69272812832399211, 0.2432969017631999853 ) ) ;
#43948 = CARTESIAN_POINT ( 'NONE',  ( 7.624341764926000131, -23.26485149464000202, -10.42531124853000080 ) ) ;
#43950 = CARTESIAN_POINT ( 'NONE',  ( 0.6216730717741000278, -78.40598835058560212, -1.163652956044999964 ) ) ;
#43949 = CARTESIAN_POINT ( 'NONE',  ( -10.49999999996000000, -76.19999999995870610, -1.566656233679999990E-09 ) ) ;
#43951 = CARTESIAN_POINT ( 'NONE',  ( -1.486328135279999962, -82.23497811192000029, -0.5524720742449998889 ) ) ;
#43952 = CARTESIAN_POINT ( 'NONE',  ( -7.803105408193176551, -79.53977973565120863, 7.394832696508047754 ) ) ;
#43953 = AXIS2_PLACEMENT_3D ( 'NONE', #51402, #33365, #19220 ) ;
#43954 = EDGE_LOOP ( 'NONE', ( #40113, #19088, #54500, #29135 ) ) ;
#43955 = CIRCLE ( 'NONE', #27922, 9.199999999999999289 ) ;
#43956 = EDGE_CURVE ( 'NONE', #11972, #32127, #50990, .T. ) ;
#43957 = CARTESIAN_POINT ( 'NONE',  ( -4.882675258918448336, -78.80818948587457839, 11.01334000465016061 ) ) ;
#43958 = CARTESIAN_POINT ( 'NONE',  ( -1.773463207542000042, -79.73653206836100082, -11.79367842281000023 ) ) ;
#43959 = CARTESIAN_POINT ( 'NONE',  ( 7.495001602003393160, -79.05287805411308000, 5.870005187018274562 ) ) ;
#43960 = CARTESIAN_POINT ( 'NONE',  ( -8.414570695956999913, -59.94999999967000548, -8.414570695956999913 ) ) ;
#43961 = CARTESIAN_POINT ( 'NONE',  ( -1.439896632895359962, -78.98541666666666572, 10.99999999999999645 ) ) ;
#43962 = CARTESIAN_POINT ( 'NONE',  ( -2.838799636221999823, -1.159209358523000111, 2.621254923317000163 ) ) ;
#43963 = CARTESIAN_POINT ( 'NONE',  ( 9.780341196751001220, -79.45766319606099160, 0.08914745397413999239 ) ) ;
#43964 = CARTESIAN_POINT ( 'NONE',  ( 12.66319951811000166, -25.18148258132000095, -0.1455783832297000147 ) ) ;
#43965 = DIRECTION ( 'NONE',  ( -1.000000000000000000, 0.000000000000000000, 0.000000000000000000 ) ) ;
#43966 = ORIENTED_EDGE ( 'NONE', *, *, #17405, .T. ) ;
#43967 = CARTESIAN_POINT ( 'NONE',  ( 0.000000000000000000, -7.000000000000000000, 0.000000000000000000 ) ) ;
#43968 = CARTESIAN_POINT ( 'NONE',  ( 7.958776492191999452, -24.47699850276000078, -9.723157982392999443 ) ) ;
#43969 = CYLINDRICAL_SURFACE ( 'NONE', #48811, 1.000000000000000000 ) ;
#43970 = CARTESIAN_POINT ( 'NONE',  ( -10.18491080495000034, -60.10716680829000325, -7.640030264173999441 ) ) ;
#43971 = CARTESIAN_POINT ( 'NONE',  ( 2.575800521921999930, -83.75017953870899134, -2.439222067143000494 ) ) ;
#43972 = ADVANCED_FACE ( 'NONE', ( #58113 ), #2255, .F. ) ;
#43973 = VERTEX_POINT ( 'NONE', #49570 ) ;
#43974 = CARTESIAN_POINT ( 'NONE',  ( 4.000000000000000000, -5.000000000000000000, 0.5999999999999999778 ) ) ;
#43975 = CARTESIAN_POINT ( 'NONE',  ( 8.060180465568407726, -61.42064870639847385, -9.621709427723352803 ) ) ;
#43976 = DIRECTION ( 'NONE',  ( 0.000000000000000000, -1.000000000000000000, 0.000000000000000000 ) ) ;
#43977 = CARTESIAN_POINT ( 'NONE',  ( -7.624341766629000539, -55.53514853726999689, 10.42531125022999916 ) ) ;
#43978 = CARTESIAN_POINT ( 'NONE',  ( 9.647254834573999460, -80.06766197889000125, -1.526580663425000095 ) ) ;
#43979 = ORIENTED_EDGE ( 'NONE', *, *, #10515, .T. ) ;
#43980 = VERTEX_POINT ( 'NONE', #9117 ) ;
#43981 = CARTESIAN_POINT ( 'NONE',  ( 11.41682566273999910, -76.61119783301998609, 5.303682846453999566 ) ) ;
#43982 = CYLINDRICAL_SURFACE ( 'NONE', #426, 11.00000000000000000 ) ;
#43983 = VERTEX_POINT ( 'NONE', #57817 ) ;
#43984 = ADVANCED_FACE ( 'NONE', ( #295 ), #41029, .F. ) ;
#43985 = CARTESIAN_POINT ( 'NONE',  ( -9.061228178001998756, -77.71430584965399646, -2.837532765875999896 ) ) ;
#43986 = CIRCLE ( 'NONE', #9096, 5.100000000000000533 ) ;
#43987 = CARTESIAN_POINT ( 'NONE',  ( 10.71369944335147117, -77.47083333333331723, 2.879226727952105769 ) ) ;
#43988 = CARTESIAN_POINT ( 'NONE',  ( 11.75000000000000178, -76.03958333333331154, -1.538071403319980268 ) ) ;
#43989 = CARTESIAN_POINT ( 'NONE',  ( 5.488127745643000210, -77.50827452080000057, 11.56242237764000080 ) ) ;
#43990 = PRODUCT_DEFINITION_CONTEXT ( 'detailed design', #34138, 'design' ) ;
#43991 = CIRCLE ( 'NONE', #18554, 9.700000000000001066 ) ;
#43992 = CARTESIAN_POINT ( 'NONE',  ( 5.151324428776999476, -77.58703011150687701, 9.964033682248000900 ) ) ;
#43993 = CARTESIAN_POINT ( 'NONE',  ( -8.485281374238999419, -23.25000000000000000, -8.485281374238999419 ) ) ;
#43994 = CARTESIAN_POINT ( 'NONE',  ( -3.480234241935507900, -86.39318692756698681, 1.471539517285501475 ) ) ;
#43995 = CARTESIAN_POINT ( 'NONE',  ( -1.639962962630000076, -78.78835931447599705, 11.09633417262999977 ) ) ;
#43996 = B_SPLINE_CURVE_WITH_KNOTS ( 'NONE', 3,
 ( #52860, #12126, #7406, #38117, #57285, #48441, #20699, #25411 ),
 .UNSPECIFIED., .F., .F.,
 ( 4, 2, 2, 4 ),
 ( 0.000000000000000000, 0.5000000000000049960, 0.7500000000000024425, 1.000000000000000000 ),
 .UNSPECIFIED. ) ;
#43997 = CARTESIAN_POINT ( 'NONE',  ( 1.445445956927814191, -79.96300696816564368, 9.136058195600192278 ) ) ;
#43998 = CIRCLE ( 'NONE', #15728, 14.00000000000000355 ) ;
#43999 = CARTESIAN_POINT ( 'NONE',  ( 7.861037107701863036, -17.53338873154977406, 10.10708465682759183 ) ) ;
#44000 = ORIENTED_EDGE ( 'NONE', *, *, #33798, .T. ) ;
#44001 = CARTESIAN_POINT ( 'NONE',  ( 6.344372811184452843, -77.28524184710113332, -6.736967749196288047 ) ) ;
#44002 = CARTESIAN_POINT ( 'NONE',  ( 1.187026915874999755, -80.52788208903798761, 0.5757885860275999690 ) ) ;
#44003 = CARTESIAN_POINT ( 'NONE',  ( 0.000000000000000000, -6.049999999381999949, 0.000000000000000000 ) ) ;
#44004 = VECTOR ( 'NONE', #23877, 1000.000000000000000 ) ;
#44005 = CARTESIAN_POINT ( 'NONE',  ( -12.60354432327999952, -22.75100837100999840, -1.750000000001000089 ) ) ;
#44006 = CARTESIAN_POINT ( 'NONE',  ( 3.504452398293381510, -3.107075414968905491, 0.3467038912678755969 ) ) ;
#44007 = CARTESIAN_POINT ( 'NONE',  ( 12.82904091339000097, -23.32452529362999982, 2.062673488738000049 ) ) ;
#44008 = LINE ( 'NONE', #21562, #40407 ) ;
#44009 = CARTESIAN_POINT ( 'NONE',  ( -1.181111693982000110, -79.17654225787899236, -0.4092372983238000139 ) ) ;
#44010 = CARTESIAN_POINT ( 'NONE',  ( 10.48730647577000141, -78.27921528601798684, -3.808884262352000061 ) ) ;
#44011 = CARTESIAN_POINT ( 'NONE',  ( 10.42274798266999980, -20.24634220924000161, -7.691916945430000041 ) ) ;
#44012 = CARTESIAN_POINT ( 'NONE',  ( -10.65106809510000119, -79.11153176702256928, 5.591232889670999739 ) ) ;
#44013 = CARTESIAN_POINT ( 'NONE',  ( 2.571160684530000129, -82.22094444544498515, -3.286247495836000176 ) ) ;
#44014 = ORIENTED_EDGE ( 'NONE', *, *, #25296, .F. ) ;
#44015 = CARTESIAN_POINT ( 'NONE',  ( -0.7976765672644999805, -81.91623022861000436, -1.504502914139000058 ) ) ;
#44016 = CARTESIAN_POINT ( 'NONE',  ( -0.6213570041975999825, -81.04689136786998915, -1.330550119908999962 ) ) ;
#44017 = CARTESIAN_POINT ( 'NONE',  ( -0.7494329999370912265, -77.79166666666556296, 1.289876867660085802 ) ) ;
#44018 = CARTESIAN_POINT ( 'NONE',  ( 3.925078296951999501, -78.34675376993899931, 11.31856107452000160 ) ) ;
#44019 = CARTESIAN_POINT ( 'NONE',  ( 3.148593469528859767, -77.00000000000000000, 8.707564246707935496 ) ) ;
#44020 = CARTESIAN_POINT ( 'NONE',  ( -0.5790013745696001024, -82.80792821772298851, -1.562055304842999925 ) ) ;
#44021 = CARTESIAN_POINT ( 'NONE',  ( 11.16572056546000091, -77.85531157257399570, 4.214520933710000250 ) ) ;
#44022 = CARTESIAN_POINT ( 'NONE',  ( -8.997179024602999675, -79.03899805011499780, 3.687079342327000298 ) ) ;
#44023 = CARTESIAN_POINT ( 'NONE',  ( 7.830665294675000609, -78.90749084168798788, -5.606588350762000239 ) ) ;
#44024 = ADVANCED_BREP_SHAPE_REPRESENTATION ( '', ( #57583, #43526 ), #13324 ) ;
#44025 = CARTESIAN_POINT ( 'NONE',  ( 0.4701041210481999855, -53.79203065542999695, -12.54901038410999980 ) ) ;
#44026 = CARTESIAN_POINT ( 'NONE',  ( 9.368450651685826358, -76.00132557254696053, 7.092182908105610473 ) ) ;
#44027 = CARTESIAN_POINT ( 'NONE',  ( -3.684198380124839023, -86.07389998728979208, 1.557781209248620957 ) ) ;
#44028 = ORIENTED_EDGE ( 'NONE', *, *, #29153, .F. ) ;
#44029 = DIRECTION ( 'NONE',  ( -0.7071067811864976127, -0.7071067811865975328, -8.872361892382962277E-10 ) ) ;
#44030 = ADVANCED_FACE ( 'NONE', ( #40100 ), #27679, .F. ) ;
#44031 = CARTESIAN_POINT ( 'NONE',  ( 8.620724302459001009, -79.51357516803899728, -8.733127930375998105 ) ) ;
#44032 = DIRECTION ( 'NONE',  ( 0.000000000000000000, 1.000000000000000000, 0.000000000000000000 ) ) ;
#44033 = EDGE_CURVE ( 'NONE', #38753, #56422, #26507, .T. ) ;
#44034 = CARTESIAN_POINT ( 'NONE',  ( 1.541440768196999933, -82.61056478991099539, 0.6318380856084999664 ) ) ;
#44035 = CARTESIAN_POINT ( 'NONE',  ( 8.867070753125000593, -78.62999890211698073, -6.468312982590000537 ) ) ;
#44036 = CARTESIAN_POINT ( 'NONE',  ( 10.60938144191372068, -80.30677083333185351, 2.852067028529588377 ) ) ;
#44037 = CARTESIAN_POINT ( 'NONE',  ( -12.24519951262000106, -76.51390172182600224, -0.7763026236661999535 ) ) ;
#44038 = CYLINDRICAL_SURFACE ( 'NONE', #19063, 0.5000000000000006661 ) ;
#44039 = CARTESIAN_POINT ( 'NONE',  ( -9.848022987154569918, -61.62869493570523360, 8.114799025198225380 ) ) ;
#44040 = ORIENTED_EDGE ( 'NONE', *, *, #21807, .F. ) ;
#44041 = CARTESIAN_POINT ( 'NONE',  ( -10.88242774903000054, -79.15424884139699202, -1.809558141819000099 ) ) ;
#44042 = CARTESIAN_POINT ( 'NONE',  ( 0.8345252027113252424, -79.91718069607952657, 0.9304729155346801450 ) ) ;
#44043 = CARTESIAN_POINT ( 'NONE',  ( -10.71369944335147117, -77.62083333333335133, -2.879226727952084453 ) ) ;
#44044 = VECTOR ( 'NONE', #32524, 1000.000000000000000 ) ;
#44045 = EDGE_CURVE ( 'NONE', #25757, #3967, #13629, .T. ) ;
#44046 = AXIS2_PLACEMENT_3D ( 'NONE', #55038, #46206, #50331 ) ;
#44047 = CARTESIAN_POINT ( 'NONE',  ( 10.92153517268999963, -78.97666430121098813, -2.282908042080999955 ) ) ;
#44048 = DIRECTION ( 'NONE',  ( 1.000000000000000000, 0.000000000000000000, 0.000000000000000000 ) ) ;
#44049 = DIRECTION ( 'NONE',  ( 0.000000000000000000, 1.000000000000000000, 0.000000000000000000 ) ) ;
#44050 = AXIS2_PLACEMENT_3D ( 'NONE', #11653, #51811, #11367 ) ;
#44051 = CARTESIAN_POINT ( 'NONE',  ( -1.011175526638764532, -81.41610230767864209, -1.124394554489388964 ) ) ;
#44052 = CARTESIAN_POINT ( 'NONE',  ( -5.830174433585000315, -78.24095814969300022, 10.80762903023000021 ) ) ;
#44053 = ORIENTED_EDGE ( 'NONE', *, *, #27026, .T. ) ;
#44054 = CARTESIAN_POINT ( 'NONE',  ( -6.606377239730371720, -79.42708333333332860, 8.596418555780411808 ) ) ;
#44055 = CARTESIAN_POINT ( 'NONE',  ( 0.000000000000000000, -76.89999999999999147, 0.000000000000000000 ) ) ;
#44056 = CARTESIAN_POINT ( 'NONE',  ( 0.8000000000000000444, -23.15000000000000213, -12.00000000000000000 ) ) ;
#44057 = ORIENTED_EDGE ( 'NONE', *, *, #19838, .T. ) ;
#44058 = ORIENTED_EDGE ( 'NONE', *, *, #4982, .T. ) ;
#44059 = CARTESIAN_POINT ( 'NONE',  ( 10.54844216519820321, -78.83464910448034857, -2.071644353491631119 ) ) ;
#44060 = ORIENTED_EDGE ( 'NONE', *, *, #15617, .T. ) ;
#44061 = CARTESIAN_POINT ( 'NONE',  ( -2.654829587612529629, -79.64748934874999975, 9.152484904945515254 ) ) ;
#44062 = ORIENTED_EDGE ( 'NONE', *, *, #36242, .F. ) ;
#44063 = CARTESIAN_POINT ( 'NONE',  ( -4.037131867638475313, -81.00000000000001421, -10.13568147781903406 ) ) ;
#44064 = CARTESIAN_POINT ( 'NONE',  ( -6.797161730763000342, -77.00189398569099808, 8.542479639784000156 ) ) ;
#44065 = CARTESIAN_POINT ( 'NONE',  ( 4.530904210857999992, -78.02986332859900642, 8.688217354640999091 ) ) ;
#44066 = CARTESIAN_POINT ( 'NONE',  ( -6.537588131481950171, -78.16270971461653971, -6.543733269810712905 ) ) ;
#44067 = CARTESIAN_POINT ( 'NONE',  ( 10.89876807034000095, -79.42932028770400166, -2.652350870517000025 ) ) ;
#44068 = VERTEX_POINT ( 'NONE', #4976 ) ;
#44069 = ORIENTED_EDGE ( 'NONE', *, *, #21619, .F. ) ;
#44070 = CARTESIAN_POINT ( 'NONE',  ( -6.946610297121736721, -77.54270072396643343, 6.109334087155939841 ) ) ;
#44071 = CARTESIAN_POINT ( 'NONE',  ( -1.776188306762000124, -77.48198983581598043, -10.89629776253999971 ) ) ;
#44072 = CARTESIAN_POINT ( 'NONE',  ( -1.500000000000000000, -78.00000000000000000, 0.000000000000000000 ) ) ;
#44073 = CIRCLE ( 'NONE', #38424, 1.750000000000001332 ) ;
#44074 = EDGE_CURVE ( 'NONE', #4486, #36041, #38466, .T. ) ;
#44075 = CARTESIAN_POINT ( 'NONE',  ( -4.814859605045999302, -78.74646614284199586, 8.425427962446999430 ) ) ;
#44076 = CARTESIAN_POINT ( 'NONE',  ( -6.387953794381322936, -79.46628966331279287, -7.041750404545100039 ) ) ;
#44077 = CARTESIAN_POINT ( 'NONE',  ( 1.136899222205000060, -79.02463074706000157, 1.164526648744999893 ) ) ;
#44078 = CARTESIAN_POINT ( 'NONE',  ( -11.11771682179999843, -80.35741463048398714, 1.751409206030000165 ) ) ;
#44079 = DIRECTION ( 'NONE',  ( 0.000000000000000000, 1.000000000000000000, 0.000000000000000000 ) ) ;
#44080 = DIRECTION ( 'NONE',  ( 1.000000000000000000, 0.000000000000000000, 0.000000000000000000 ) ) ;
#44081 = AXIS2_PLACEMENT_3D ( 'NONE', #41587, #32126, #28280 ) ;
#44082 = CARTESIAN_POINT ( 'NONE',  ( -11.00000000000000000, -79.69999999999998863, 0.000000000000000000 ) ) ;
#44083 = ORIENTED_EDGE ( 'NONE', *, *, #5058, .T. ) ;
#44084 = CARTESIAN_POINT ( 'NONE',  ( -5.605966151088000338, -78.98998022871599289, 10.70477826589000081 ) ) ;
#44085 = AXIS2_PLACEMENT_3D ( 'NONE', #34118, #52161, #21136 ) ;
#44086 = CARTESIAN_POINT ( 'NONE',  ( -7.761025538834000592, -54.71850014388999739, 9.835174270505000038 ) ) ;
#44087 = CARTESIAN_POINT ( 'NONE',  ( 2.956870837876000468, -79.05653331767798875, 11.44999256673999888 ) ) ;
#44088 = CARTESIAN_POINT ( 'NONE',  ( -10.13695543448000080, -18.29168900649999685, -7.646071007876000358 ) ) ;
#44090 = LINE ( 'NONE', #34916, #4418 ) ;
#44089 = CYLINDRICAL_SURFACE ( 'NONE', #6156, 14.00000000000000000 ) ;
#44091 = AXIS2_PLACEMENT_3D ( 'NONE', #20018, #37420, #51609 ) ;
#44092 = CARTESIAN_POINT ( 'NONE',  ( 7.395758551695209349, -79.40217280339305717, 5.683424056470474994 ) ) ;
#44093 = CARTESIAN_POINT ( 'NONE',  ( -11.99999999994999911, -76.29999999994899440, 3.078392110872999642E-09 ) ) ;
#44094 = CARTESIAN_POINT ( 'NONE',  ( -0.5900578684300998855, -82.25488867623700173, -1.108170840844000082 ) ) ;
#44095 = CARTESIAN_POINT ( 'NONE',  ( 3.911191660715999774, -77.17018495668600053, 10.56108632439999973 ) ) ;
#44096 = CARTESIAN_POINT ( 'NONE',  ( 12.50409240825462120, -24.52129362382453692, 1.233800929768811283 ) ) ;
#44097 = CARTESIAN_POINT ( 'NONE',  ( -5.396048678459999692, -80.23819584820419948, 9.878076380210000451 ) ) ;
#44098 = ORIENTED_EDGE ( 'NONE', *, *, #34477, .T. ) ;
#44099 = DIRECTION ( 'NONE',  ( 0.000000000000000000, -1.000000000000000000, 0.000000000000000000 ) ) ;
#44100 = CARTESIAN_POINT ( 'NONE',  ( 0.9212224518320000222, -53.98045898127999465, 12.54670315977999984 ) ) ;
#44101 = CARTESIAN_POINT ( 'NONE',  ( -12.87022657274000004, -19.21514526754999963, 2.062597299672999540 ) ) ;
#44102 = CARTESIAN_POINT ( 'NONE',  ( -3.251796736646000330, -2.675056440563999605, 1.977781782242000075 ) ) ;
#44103 = EDGE_CURVE ( 'NONE', #57621, #15231, #24878, .T. ) ;
#44104 = CARTESIAN_POINT ( 'NONE',  ( -4.952462208631658314, -77.86317697277696936, 9.641482076232696485 ) ) ;
#44105 = CARTESIAN_POINT ( 'NONE',  ( -1.444794657067000054, -79.63356627858598813, -9.313366329545999633 ) ) ;
#44106 = CARTESIAN_POINT ( 'NONE',  ( -12.72558083408000051, -55.59866855809999464, 1.930284430576000076 ) ) ;
#44107 = DIRECTION ( 'NONE',  ( -1.224058225713999994E-08, -0.9999999999999998890, 4.602708956829999399E-10 ) ) ;
#44108 = CARTESIAN_POINT ( 'NONE',  ( -2.019183793707000074, -60.58720277209999949, 12.79944116707999946 ) ) ;
#44109 = CARTESIAN_POINT ( 'NONE',  ( 1.250000000000000000, -79.75000000000000000, 0.000000000000000000 ) ) ;
#44110 = CARTESIAN_POINT ( 'NONE',  ( 2.283504659536000236, -82.67419503318798490, 3.492219933351000005 ) ) ;
#44111 = CARTESIAN_POINT ( 'NONE',  ( 2.426647618366999603E-14, -5.949999999936550488, 0.000000000000000000 ) ) ;
#44112 = CARTESIAN_POINT ( 'NONE',  ( -10.12213620585348828, -76.99884921769482560, -6.582638106783194942 ) ) ;
#44113 = B_SPLINE_SURFACE_WITH_KNOTS ( 'NONE', 3, 3, ( 
 ( #38788, #14894, #24926, #24640, #38210, #51231, #42069, #10783, #28762, #46811, #24354, #42366, #35203, #21356, #26356, #52664, #52381, #53528, #43518, #13068, #8654, #21929, #43816, #31066, #34345, #17508, #25500, #7501, #12501, #57086, #57954, #53235, #49104, #11935, #47965, #48528, #56807, #21647, #3361, #52951, #3079, #35498, #34636, #39373, #39938, #12783, #21073, #26640, #48815, #44375, #44095, #8073, #39654, #30499, #30781, #26069, #39079, #57379, #3927, #44675, #4228, #22226, #3644, #8358, #16364, #57659, #16652 ),
 ( #29914, #12217, #30206, #16939, #48251, #7788, #17215, #25788, #34920, #49405, #27232, #8954, #9833, #35798, #22819, #14535, #996, #18690, #36103, #36392, #27814, #49700, #28105, #40830, #18109, #26938, #45861, #422, #54120, #50572, #32239, #18982, #45271, #132, #5394, #23403, #9247, #32529, #22527, #5111, #40537, #13954, #41413, #36974, #54987, #10127, #36683, #13661, #50282, #4820, #46155, #18400, #17812, #4527, #31656, #53828, #40237, #31950, #54418, #49995, #23110, #5680, #58252, #712, #41118, #13363, #31361 ),
 ( #44971, #9541, #27524, #45566, #54699, #14243, #10714, #32822, #51743, #19272, #6263, #56448, #42875, #2149, #19556, #19856, #11292, #33118, #11582, #24278, #1564, #50867, #29272, #42296, #37554, #33990, #15709, #2433, #28692, #41996, #47320, #6849, #51160, #16003, #5973, #47030, #23977, #55871, #24859, #20435, #38430, #52029, #20150, #55571, #33704, #46743, #29561, #1861, #1279, #46445, #15120, #37263, #23690, #15422, #37851, #33414, #6560, #51452, #11005, #47616, #41703, #38138, #56160, #55277, #14823, #28989, #10413 ),
 ( #24568, #28399, #42585, #52313, #4675, #18255, #31505, #53370, #40685, #43167, #27085, #34278, #16300, #22070, #7430, #9095, #4371, #22673, #2724, #56741, #58095, #7140, #31206, #12920, #4067, #11869, #45124, #43448, #30917, #49550, #44817, #29846, #277, #58392, #53973, #53671, #17657, #49246, #40079, #22373, #35643, #47899, #48953, #13512, #36249, #54269, #13802, #13210, #40384, #8795, #39786, #35946, #31805, #26788, #17954, #25142, #20720, #38719, #25433, #8496, #3009, #21782, #57800, #17360, #35346, #26493, #44516 ) ),
 .UNSPECIFIED., .F., .F., .F.,
 ( 4, 4 ),
 ( 4, 1, 1, 1, 1, 1, 1, 1, 1, 1, 1, 1, 1, 1, 1, 1, 1, 1, 1, 1, 1, 1, 1, 1, 1, 1, 1, 1, 1, 1, 1, 1, 1, 1, 1, 1, 1, 1, 1, 1, 1, 1, 1, 1, 1, 1, 1, 1, 1, 1, 1, 1, 1, 1, 1, 1, 1, 1, 1, 1, 1, 1, 1, 1, 4 ),
 ( -0.1772706441294000235, 1.177270644128999955 ),
 ( -0.02000000000000000042, -0.003749999999999999861, 0.01250000000000000069, 0.02875000000000000125, 0.04499999999999999833, 0.06124999999999999889, 0.07749999999999999944, 0.09375000000000000000, 0.1100000000000000006, 0.1262500000000000011, 0.1424999999999999878, 0.1587500000000000022, 0.1749999999999999889, 0.1912500000000000033, 0.2074999999999999900, 0.2237500000000000044, 0.2399999999999999911, 0.2562499999999999778, 0.2725000000000000200, 0.2887500000000000067, 0.3049999999999999933, 0.3212499999999999800, 0.3375000000000000222, 0.3537500000000000089, 0.3699999999999999956, 0.3862499999999999822, 0.4025000000000000244, 0.4187500000000000111, 0.4349999999999999978, 0.4512499999999999845, 0.4675000000000000266, 0.4837500000000000133, 0.5000000000000000000, 0.5162499999999999867, 0.5324999999999999734, 0.5487499999999999600, 0.5649999999999999467, 0.5812500000000000444, 0.5975000000000000311, 0.6137500000000000178, 0.6300000000000000044, 0.6462499999999999911, 0.6624999999999999778, 0.6787499999999999645, 0.6949999999999999512, 0.7112500000000000488, 0.7275000000000000355, 0.7437500000000000222, 0.7600000000000000089, 0.7762499999999999956, 0.7924999999999999822, 0.8087499999999999689, 0.8249999999999999556, 0.8412500000000000533, 0.8575000000000000400, 0.8737500000000000266, 0.8900000000000000133, 0.9062500000000000000, 0.9224999999999999867, 0.9387499999999999734, 0.9549999999999999600, 0.9712499999999999467, 0.9875000000000000444, 1.003749999999999920, 1.020000000000000018 ),
 .UNSPECIFIED. ) ;
#44114 = B_SPLINE_CURVE_WITH_KNOTS ( 'NONE', 3,
 ( #53857, #54724, #46180, #24004, #41144, #36997, #41439, #19297, #32264, #19882, #5705, #55305, #19005, #55896, #1304, #1024, #45886, #42022 ),
 .UNSPECIFIED., .F., .F.,
 ( 4, 2, 2, 2, 2, 2, 2, 2, 4 ),
 ( 0.000000000000000000, 0.1250000000000000833, 0.2500000000000001665, 0.3750000000000002220, 0.5000000000000002220, 0.6250000000000002220, 0.7500000000000001110, 0.8750000000000001110, 1.000000000000000000 ),
 .UNSPECIFIED. ) ;
#44115 = ADVANCED_FACE ( 'NONE', ( #12462, #30463 ), #52346, .F. ) ;
#44116 = CARTESIAN_POINT ( 'NONE',  ( -3.224264963920000504, -76.81051199849498801, -10.67046002915000003 ) ) ;
#44117 = CARTESIAN_POINT ( 'NONE',  ( 1.217406450052350930, -81.86832592185405133, 0.2837533658167560313 ) ) ;
#44118 = CARTESIAN_POINT ( 'NONE',  ( 1.750000000001000089, -55.54999998977000075, -12.56594317853999954 ) ) ;
#44119 = CARTESIAN_POINT ( 'NONE',  ( -0.1834469635243000107, -79.61327907013999550, -1.236465612773999911 ) ) ;
#44120 = CARTESIAN_POINT ( 'NONE',  ( -0.3926218265389255779, -78.89583333333335702, 1.460959015002472494 ) ) ;
#44121 = CARTESIAN_POINT ( 'NONE',  ( 3.250000000000000444, -2.739583333333333481, -0.4254240051736113415 ) ) ;
#44122 = CARTESIAN_POINT ( 'NONE',  ( -5.916486123000844088, -80.17868767483665238, -8.975394947010663316 ) ) ;
#44123 = CARTESIAN_POINT ( 'NONE',  ( 5.413904038987179312, -77.16666666666664298, -9.393203674808262349 ) ) ;
#44124 = CARTESIAN_POINT ( 'NONE',  ( -8.532671860997186997, -16.87201063391398748, -9.433519686788320868 ) ) ;
#44125 = CARTESIAN_POINT ( 'NONE',  ( -11.60111135005000094, -79.01961632557299708, -3.181408645392000523 ) ) ;
#44126 = CARTESIAN_POINT ( 'NONE',  ( -4.784380313523580064, -78.71666666666669698, 8.300970689365431809 ) ) ;
#44127 = CARTESIAN_POINT ( 'NONE',  ( -1.788059198778999770, -79.93572132302399780, -11.11920900327000084 ) ) ;
#44128 = CARTESIAN_POINT ( 'NONE',  ( 9.599999999999999645, -90.39999999999999147, 0.000000000000000000 ) ) ;
#44129 = ORIENTED_EDGE ( 'NONE', *, *, #31581, .T. ) ;
#44130 = CARTESIAN_POINT ( 'NONE',  ( 12.50485632864967123, -17.13407884568546891, 0.6924337387642888197 ) ) ;
#44131 = EDGE_LOOP ( 'NONE', ( #9207, #25321 ) ) ;
#44132 =( NAMED_UNIT ( * ) SI_UNIT ( $, .STERADIAN. ) SOLID_ANGLE_UNIT ( ) );
#44133 = ORIENTED_EDGE ( 'NONE', *, *, #15164, .F. ) ;
#44134 = CARTESIAN_POINT ( 'NONE',  ( 2.380924776420011657, -3.499999999999999556, -2.674844963567099221 ) ) ;
#44135 = AXIS2_PLACEMENT_3D ( 'NONE', #8213, #30183, #24335 ) ;
#44136 = CARTESIAN_POINT ( 'NONE',  ( -0.4035306080773887194, -79.04687499584814248, -3.408455983050635130 ) ) ;
#44137 = CARTESIAN_POINT ( 'NONE',  ( -9.543280303650000462, -79.11375811998600227, -5.301053389303000074 ) ) ;
#44138 = CARTESIAN_POINT ( 'NONE',  ( 3.440333001647999822, -82.42136181958099428, -0.2267620307923000067 ) ) ;
#44139 = CARTESIAN_POINT ( 'NONE',  ( 0.9576858015051188389, -79.26683165706418777, 9.453865573464822702 ) ) ;
#44140 = ORIENTED_EDGE ( 'NONE', *, *, #5283, .F. ) ;
#44141 = CARTESIAN_POINT ( 'NONE',  ( 9.554844271749594498, -78.06000170479207156, -5.239760174894856348 ) ) ;
#44142 = CARTESIAN_POINT ( 'NONE',  ( -1.791405018985999797, -78.89219709918999968, 12.22794537915999946 ) ) ;
#44143 = VERTEX_POINT ( 'NONE', #48220 ) ;
#44144 = ORIENTED_EDGE ( 'NONE', *, *, #50116, .T. ) ;
#44145 = DIRECTION ( 'NONE',  ( -0.7071067811865475727, 0.000000000000000000, 0.7071067811865475727 ) ) ;
#44146 = FACE_BOUND ( 'NONE', #26332, .T. ) ;
#44147 = B_SPLINE_CURVE_WITH_KNOTS ( 'NONE', 3,
 ( #27696, #8825, #5558, #44841, #31529, #9417, #40409, #17981, #4983, #53997, #54585, #13538, #13832, #49576, #9123, #45147, #27406, #4698 ),
 .UNSPECIFIED., .F., .F.,
 ( 4, 2, 2, 2, 2, 2, 2, 2, 4 ),
 ( 0.000000000000000000, 0.1250000000000000000, 0.2500000000000000000, 0.3750000000000000000, 0.5000000000000000000, 0.6250000000000000000, 0.7500000000000000000, 0.8750000000000000000, 1.000000000000000000 ),
 .UNSPECIFIED. ) ;
#44148 = CARTESIAN_POINT ( 'NONE',  ( 9.567264450310133839, -79.79999999999999716, 6.968530294715381324 ) ) ;
#44149 = ADVANCED_FACE ( 'NONE', ( #38174 ), #27344, .F. ) ;
#44150 = CARTESIAN_POINT ( 'NONE',  ( -8.446513303087588298, -80.04704965811107797, 6.650504277378666451 ) ) ;
#44151 = FACE_OUTER_BOUND ( 'NONE', #57763, .T. ) ;
#44152 = CARTESIAN_POINT ( 'NONE',  ( -3.597908783441192249, -86.39318692756698681, -2.511058746283273191 ) ) ;
#44153 = CARTESIAN_POINT ( 'NONE',  ( 1.604468093511001614, -85.90488784433034652, 3.083698236688781513 ) ) ;
#44154 = CARTESIAN_POINT ( 'NONE',  ( 5.623102978484999959, -77.34535537052001075, 11.84678905512000036 ) ) ;
#44155 = ADVANCED_FACE ( 'NONE', ( #21324 ), #39332, .T. ) ;
#44156 = CARTESIAN_POINT ( 'NONE',  ( 8.913248419499998576, -76.43655867677999538, -7.987006294937000206 ) ) ;
#44157 = CARTESIAN_POINT ( 'NONE',  ( 1.800245306220000119, -76.88836798910099901, 10.73450256003999925 ) ) ;
#44158 = CARTESIAN_POINT ( 'NONE',  ( -7.624341764926000131, -23.26485149464000202, 10.42531124853000080 ) ) ;
#44159 = CARTESIAN_POINT ( 'NONE',  ( -1.390935043183000097, -82.18132306546799271, -3.888936835908999967 ) ) ;
#44160 = CARTESIAN_POINT ( 'NONE',  ( -10.35845616725999996, -55.50221404479999876, 7.627487606591000002 ) ) ;
#44161 = CARTESIAN_POINT ( 'NONE',  ( -1.906216885303581243, -3.025969998097067570, 2.639459242746020617 ) ) ;
#44162 = CARTESIAN_POINT ( 'NONE',  ( -3.180430419197999736, -80.32205496681199008, -1.570485499300999788 ) ) ;
#44163 = VECTOR ( 'NONE', #34466, 1000.000000000000000 ) ;
#44164 = DIRECTION ( 'NONE',  ( 0.000000000000000000, 1.000000000000000000, 0.000000000000000000 ) ) ;
#44165 = CARTESIAN_POINT ( 'NONE',  ( -0.6860765926954999205, -83.58499735065198877, -3.477680648429000154 ) ) ;
#44166 = CARTESIAN_POINT ( 'NONE',  ( -3.054513261463999818, -2.833537059304999772, -2.270689576097000284 ) ) ;
#44167 = CARTESIAN_POINT ( 'NONE',  ( 10.75000000000000000, -77.19999999999998863, -6.141891925717000695E-13 ) ) ;
#44168 = ORIENTED_EDGE ( 'NONE', *, *, #8375, .T. ) ;
#44169 = CARTESIAN_POINT ( 'NONE',  ( -9.029867227927999451, -62.13262194258000193, -9.038867509651000276 ) ) ;
#44170 = DIRECTION ( 'NONE',  ( 0.000000000000000000, 1.000000000000000000, 0.000000000000000000 ) ) ;
#44171 = CARTESIAN_POINT ( 'NONE',  ( 0.8471236057751000414, -81.04211641967700075, 1.030027924806000028 ) ) ;
#44172 = CARTESIAN_POINT ( 'NONE',  ( -12.77656766273999978, -16.68801851262999847, -0.1555695072196000006 ) ) ;
#44173 = CARTESIAN_POINT ( 'NONE',  ( 5.579996517577999526, -77.39173409593000486, 11.75597208960999929 ) ) ;
#44174 = CARTESIAN_POINT ( 'NONE',  ( 5.539808784079907511, -79.86666666666667425, -9.611650271896827746 ) ) ;
#44175 = AXIS2_PLACEMENT_3D ( 'NONE', #49318, #13578, #49618 ) ;
#44176 = CARTESIAN_POINT ( 'NONE',  ( -10.41144098944999463, -60.32546312031783486, -7.610433527982627844 ) ) ;
#44177 = CARTESIAN_POINT ( 'NONE',  ( 6.099198899075000568, -76.41540033321001602, 10.75284491171999868 ) ) ;
#44178 = EDGE_LOOP ( 'NONE', ( #46189, #16975, #9723, #2930, #29788 ) ) ;
#44179 = CARTESIAN_POINT ( 'NONE',  ( -11.26045488450000143, -80.74764171378579647, 0.3336940576009999604 ) ) ;
#44180 = CARTESIAN_POINT ( 'NONE',  ( -1.500000000000000000, -80.40000000000000568, 0.000000000000000000 ) ) ;
#44181 = EDGE_CURVE ( 'NONE', #31248, #55607, #39944, .T. ) ;
#44182 = CARTESIAN_POINT ( 'NONE',  ( 12.70956478401000034, -60.20497526583999814, 1.933781249744999986 ) ) ;
#44183 = CARTESIAN_POINT ( 'NONE',  ( -1.667936697358999965, -22.76462890193000277, -12.53241208773999915 ) ) ;
#44184 = CARTESIAN_POINT ( 'NONE',  ( -7.784718833714999064, -77.84296661922998339, 5.670217160303000270 ) ) ;
#44185 = EDGE_CURVE ( 'NONE', #4989, #44143, #53200, .T. ) ;
#44186 = CARTESIAN_POINT ( 'NONE',  ( 1.289148685043999931, -84.26882685001099560, 3.967952992048999761 ) ) ;
#44187 = DIRECTION ( 'NONE',  ( -1.000000000000000000, 0.000000000000000000, 0.000000000000000000 ) ) ;
#44188 = CARTESIAN_POINT ( 'NONE',  ( -1.063776463958000074, -79.54521086701498689, 0.9372507776557998938 ) ) ;
#44189 = EDGE_LOOP ( 'NONE', ( #54957, #21552, #18357, #49580, #17314, #35460 ) ) ;
#44190 = B_SPLINE_CURVE_WITH_KNOTS ( 'NONE', 3,
 ( #52620, #47923, #7162, #3317, #16025, #12172, #7456, #43474, #29581, #30158, #21311, #2456, #47638, #25166, #20460, #30448, #20743, #3595 ),
 .UNSPECIFIED., .F., .F.,
 ( 4, 2, 2, 2, 2, 2, 2, 2, 4 ),
 ( 0.000000000000000000, 0.1250000000000000833, 0.2500000000000001665, 0.3750000000000001110, 0.5000000000000001110, 0.6250000000000001110, 0.7500000000000000000, 0.8750000000000000000, 1.000000000000000000 ),
 .UNSPECIFIED. ) ;
#44191 = CARTESIAN_POINT ( 'NONE',  ( -8.035810179446766455, -79.05885488453131416, 4.621717112953465545 ) ) ;
#44192 = CARTESIAN_POINT ( 'NONE',  ( -3.999999999999745093, -78.71311462308116802, -0.4401583980473047220 ) ) ;
#44193 = ORIENTED_EDGE ( 'NONE', *, *, #58205, .F. ) ;
#44194 = ORIENTED_EDGE ( 'NONE', *, *, #33929, .F. ) ;
#44195 = CARTESIAN_POINT ( 'NONE',  ( 6.696351723200000272, -79.04823107411199601, -8.651398149159000184 ) ) ;
#44196 = CARTESIAN_POINT ( 'NONE',  ( -7.434020715871331397, -55.28308356097138443, -8.107762507645487560 ) ) ;
#44197 = CARTESIAN_POINT ( 'NONE',  ( -1.864102395052000150, -79.98252921644699143, -11.06258289461000111 ) ) ;
#44198 = ORIENTED_EDGE ( 'NONE', *, *, #14702, .F. ) ;
#44199 = ORIENTED_EDGE ( 'NONE', *, *, #49457, .F. ) ;
#44200 = ORIENTED_EDGE ( 'NONE', *, *, #18771, .T. ) ;
#44201 = ADVANCED_FACE ( 'NONE', ( #12748 ), #37126, .F. ) ;
#44202 = CARTESIAN_POINT ( 'NONE',  ( -3.785083400059697567, -78.09945095226758838, 11.15180688584555213 ) ) ;
#44203 = CARTESIAN_POINT ( 'NONE',  ( 9.767191983224998708, -80.00043356103655867, 0.05162932631433000269 ) ) ;
#44204 = ORIENTED_EDGE ( 'NONE', *, *, #51138, .T. ) ;
#44205 = CARTESIAN_POINT ( 'NONE',  ( -1.499934128473817241, -81.90004407876089942, 2.109063419893342596E-06 ) ) ;
#44206 = EDGE_LOOP ( 'NONE', ( #715, #11570, #8241, #35554 ) ) ;
#44207 = CARTESIAN_POINT ( 'NONE',  ( -12.10179013622999911, -78.56294709707631796, -1.986401539992999954 ) ) ;
#44208 = CARTESIAN_POINT ( 'NONE',  ( -2.309341173333539388, -78.96264283715740362, -3.830055274395752551 ) ) ;
#44209 = CARTESIAN_POINT ( 'NONE',  ( 7.624757993407000001, -54.99647951274999969, 10.47516388917000008 ) ) ;
#44210 = CIRCLE ( 'NONE', #43296, 12.00000000000000178 ) ;
#44211 = CARTESIAN_POINT ( 'NONE',  ( 0.5999999999999999778, -23.15000000000000213, -11.79999999999999893 ) ) ;
#44212 = FACE_OUTER_BOUND ( 'NONE', #20892, .T. ) ;
#44213 = EDGE_CURVE ( 'NONE', #35193, #23446, #4122, .T. ) ;
#44214 = DIRECTION ( 'NONE',  ( 0.000000000000000000, -1.000000000000000000, 0.000000000000000000 ) ) ;
#44215 = CARTESIAN_POINT ( 'NONE',  ( 7.718346056121999865, -57.05111654290000445, -10.07719973194999952 ) ) ;
#44216 = CARTESIAN_POINT ( 'NONE',  ( 7.919595949288999570, -59.94999999967000548, 8.768124086712999699 ) ) ;
#44217 = CARTESIAN_POINT ( 'NONE',  ( 0.000000000000000000, -76.39999999999999147, 0.000000000000000000 ) ) ;
#44218 = CARTESIAN_POINT ( 'NONE',  ( -3.561950367126999861, -80.01250264934799361, 2.177638482891999683 ) ) ;
#44219 = CARTESIAN_POINT ( 'NONE',  ( 3.110024790766000358, -77.40768667140099524, -9.254072701159000047 ) ) ;
#44220 = CARTESIAN_POINT ( 'NONE',  ( 0.3271848554490964789, -83.35416666666665719, 1.217465845835395521 ) ) ;
#44221 = DIRECTION ( 'NONE',  ( 0.000000000000000000, 1.000000000000000000, 0.000000000000000000 ) ) ;
#44222 = CARTESIAN_POINT ( 'NONE',  ( 3.090997446795999970, -77.14356191088999992, -11.88544462247999967 ) ) ;
#44223 = CARTESIAN_POINT ( 'NONE',  ( -0.9234216768726070113, -80.80927045197968539, -0.8478083823816136011 ) ) ;
#44224 = CARTESIAN_POINT ( 'NONE',  ( -10.34999999999999964, -82.00000000000000000, 0.000000000000000000 ) ) ;
#44225 = CARTESIAN_POINT ( 'NONE',  ( 6.722974506806673745, -79.33790088530881235, -6.669842186947492202 ) ) ;
#44226 = CARTESIAN_POINT ( 'NONE',  ( -1.239625787815246127, -79.89786197137119927, -0.8640456112635624963 ) ) ;
#44227 = CARTESIAN_POINT ( 'NONE',  ( 1.118108678836999825, -79.16169582999499710, 1.024097206608999944 ) ) ;
#44228 = DIRECTION ( 'NONE',  ( 1.000000000000000000, 0.000000000000000000, 0.000000000000000000 ) ) ;
#44229 = CARTESIAN_POINT ( 'NONE',  ( -11.79389253715000052, -77.42143497408700625, 2.981045019388999684 ) ) ;
#44230 = DIRECTION ( 'NONE',  ( 0.000000000000000000, 1.000000000000000000, 0.000000000000000000 ) ) ;
#44231 = CIRCLE ( 'NONE', #22582, 9.750000000000000000 ) ;
#44233 = CARTESIAN_POINT ( 'NONE',  ( -7.709154088328800114, -18.07253195914548627, 9.998702477107983100 ) ) ;
#44232 = DIRECTION ( 'NONE',  ( 0.000000000000000000, 1.000000000000000000, 0.000000000000000000 ) ) ;
#44234 = CARTESIAN_POINT ( 'NONE',  ( -0.5103843434498001042, -82.74009435914298649, -1.376937268564000005 ) ) ;
#44235 = CARTESIAN_POINT ( 'NONE',  ( -7.653399028025074102, -79.53820228785095026, 7.548941424443766479 ) ) ;
#44236 = ORIENTED_EDGE ( 'NONE', *, *, #51772, .T. ) ;
#44237 = FACE_OUTER_BOUND ( 'NONE', #32868, .T. ) ;
#44238 = CARTESIAN_POINT ( 'NONE',  ( -10.02838903155999972, -79.64445734768898433, 6.665108128633999485 ) ) ;
#44239 = CARTESIAN_POINT ( 'NONE',  ( 9.550506292781999917, -80.36542270824050149, 5.569596721165000375 ) ) ;
#44240 = CARTESIAN_POINT ( 'NONE',  ( 1.121668155292469438, -80.00000000000000000, -9.414507127281368071 ) ) ;
#44241 = CARTESIAN_POINT ( 'NONE',  ( 11.00000000000000000, -78.84999999999999432, 0.000000000000000000 ) ) ;
#44242 = CONICAL_SURFACE ( 'NONE', #23516, 2.399999999383999771, 0.7853981633972997312 ) ;
#44243 = CARTESIAN_POINT ( 'NONE',  ( 1.752416575730000092, -1.467211001040999996, 3.260037978519999768 ) ) ;
#44244 = CARTESIAN_POINT ( 'NONE',  ( -9.133499927808999885, -79.16970150572998932, -3.177109475039999964 ) ) ;
#44245 = CARTESIAN_POINT ( 'NONE',  ( 12.66235429707000115, -25.13741783422999987, -0.4955846680316000619 ) ) ;
#44246 = CARTESIAN_POINT ( 'NONE',  ( 6.365665562422999635, -79.13050366622999832, 10.17242851768000023 ) ) ;
#44247 = ORIENTED_EDGE ( 'NONE', *, *, #2689, .T. ) ;
#44248 = FACE_OUTER_BOUND ( 'NONE', #11162, .T. ) ;
#44249 = AXIS2_PLACEMENT_3D ( 'NONE', #5441, #50042, #49460 ) ;
#44250 = FACE_OUTER_BOUND ( 'NONE', #46624, .T. ) ;
#44251 = LINE ( 'NONE', #39236, #35598 ) ;
#44252 = CARTESIAN_POINT ( 'NONE',  ( 0.7554284705563509839, -78.56666666666666288, -1.310679582531386167 ) ) ;
#44253 = CARTESIAN_POINT ( 'NONE',  ( -3.309179897806000525, -83.26917953870899680, -1.278233535900999973 ) ) ;
#44254 = ORIENTED_EDGE ( 'NONE', *, *, #27902, .F. ) ;
#44255 = CARTESIAN_POINT ( 'NONE',  ( -12.54435570279974854, -55.27582218184407736, 1.733918077762378829 ) ) ;
#44256 = DIRECTION ( 'NONE',  ( 0.000000000000000000, -1.000000000000000000, 0.000000000000000000 ) ) ;
#44257 = CARTESIAN_POINT ( 'NONE',  ( 1.250000000000000000, -80.84999999999999432, 0.000000000000000000 ) ) ;
#44258 = ORIENTED_EDGE ( 'NONE', *, *, #27261, .T. ) ;
#44259 = ADVANCED_FACE ( 'NONE', ( #13917 ), #8912, .F. ) ;
#44260 = CARTESIAN_POINT ( 'NONE',  ( 1.232226823490451428, -54.27709088663625181, 12.50408896745931386 ) ) ;
#44261 = CARTESIAN_POINT ( 'NONE',  ( -8.227509542961000122, -53.97460508840000415, -9.516261809240999625 ) ) ;
#44262 = CARTESIAN_POINT ( 'NONE',  ( -8.396223008680999911, -79.81252310367197822, -4.990405176070999538 ) ) ;
#44263 = ORIENTED_EDGE ( 'NONE', *, *, #41370, .F. ) ;
#44264 = ORIENTED_EDGE ( 'NONE', *, *, #17332, .F. ) ;
#44265 = CARTESIAN_POINT ( 'NONE',  ( -3.685303599376999806, -77.02275771435500928, 11.66643009639000006 ) ) ;
#44266 = CARTESIAN_POINT ( 'NONE',  ( -10.43384097447730419, -78.61940185271862447, -2.589511503229956713 ) ) ;
#44267 = VERTEX_POINT ( 'NONE', #44637 ) ;
#44268 = CARTESIAN_POINT ( 'NONE',  ( 9.136202122873999798, -77.46210584965400869, 2.585973524422000125 ) ) ;
#44269 = CYLINDRICAL_SURFACE ( 'NONE', #6522, 1.500000000000000000 ) ;
#44270 = CARTESIAN_POINT ( 'NONE',  ( 0.008809971122743728150, -80.22610841291549377, -1.249644143390686413 ) ) ;
#44271 = CARTESIAN_POINT ( 'NONE',  ( -9.247037010692000791, -77.64321223492000001, -9.074963555248000802 ) ) ;
#44272 = CARTESIAN_POINT ( 'NONE',  ( 8.282307197233999219, -77.94110257053002044, -7.564489280984999731 ) ) ;
#44273 = EDGE_CURVE ( 'NONE', #18472, #41331, #37835, .T. ) ;
#44274 = CARTESIAN_POINT ( 'NONE',  ( -2.662296488501999292, -86.36264283715698298, 3.593683008806643375 ) ) ;
#44275 = CARTESIAN_POINT ( 'NONE',  ( -0.2721098858049000313, -79.27861348850899503, 11.21356619464000026 ) ) ;
#44276 = CARTESIAN_POINT ( 'NONE',  ( 2.590478588064626386, -79.95266178902241450, 8.887573261231658250 ) ) ;
#44277 = CARTESIAN_POINT ( 'NONE',  ( 8.423937229337077781, -80.14385089984534716, -7.240779987882011604 ) ) ;
#44278 = ORIENTED_EDGE ( 'NONE', *, *, #50436, .F. ) ;
#44279 = CARTESIAN_POINT ( 'NONE',  ( 11.23392183412000023, -78.87684575912199136, 0.8531908288953000685 ) ) ;
#44280 = CARTESIAN_POINT ( 'NONE',  ( 7.331368884251999951, -75.84156555408999623, 9.888700222343000945 ) ) ;
#44281 = CARTESIAN_POINT ( 'NONE',  ( -0.5412065714428999641, -79.83330536170299752, -1.203187872875000064 ) ) ;
#44282 = VECTOR ( 'NONE', #26889, 1000.000000000000114 ) ;
#44283 = CARTESIAN_POINT ( 'NONE',  ( -10.64937091039521988, -76.82864424258517033, 2.917955610043998504 ) ) ;
#44284 = CARTESIAN_POINT ( 'NONE',  ( -1.197912192620000038, -78.12365292024510666, 0.5527856627588000338 ) ) ;
#44285 = CARTESIAN_POINT ( 'NONE',  ( 3.012546900933178673, -3.055919557904988260, -1.823338109451127620 ) ) ;
#44286 = VECTOR ( 'NONE', #55460, 1000.000000000000114 ) ;
#44287 = CARTESIAN_POINT ( 'NONE',  ( 12.92181194099999963, -20.24351820077000141, 2.062502994258999856 ) ) ;
#44288 = EDGE_CURVE ( 'NONE', #47573, #31099, #26902, .T. ) ;
#44289 = CARTESIAN_POINT ( 'NONE',  ( -12.49168451098999988, -18.70151115557999688, -1.667916687331000070 ) ) ;
#44290 = CARTESIAN_POINT ( 'NONE',  ( 8.199999995296000321, -81.00000000470399186, 2.775962726994000217E-08 ) ) ;
#44291 = CARTESIAN_POINT ( 'NONE',  ( -9.937637090044999510, -79.95706551386098226, 4.829168387547000840 ) ) ;
#44292 = CARTESIAN_POINT ( 'NONE',  ( 10.35845616727999996, -18.70221404512000163, -7.627487606607999737 ) ) ;
#44293 = CARTESIAN_POINT ( 'NONE',  ( 10.13881649148000008, -76.90783510652001098, -5.938594122520999719 ) ) ;
#44294 = CARTESIAN_POINT ( 'NONE',  ( -2.384769505383999899, -80.41092258374798973, -3.423365290318999943 ) ) ;
#44295 = EDGE_CURVE ( 'NONE', #45569, #40274, #56024, .T. ) ;
#44296 = ORIENTED_EDGE ( 'NONE', *, *, #25470, .T. ) ;
#44297 = CARTESIAN_POINT ( 'NONE',  ( -0.6878774159238000285, -82.04286360614999296, -1.297410027194999982 ) ) ;
#44298 = CARTESIAN_POINT ( 'NONE',  ( 0.5308835263170998964, -81.36284491707999678, 1.242631599581000001 ) ) ;
#44299 = CARTESIAN_POINT ( 'NONE',  ( 0.000000000000000000, -60.04999999966999980, -12.00000000000000000 ) ) ;
#44300 = CARTESIAN_POINT ( 'NONE',  ( -8.557169117579000783, -77.56000362265000092, -8.383968101560000719 ) ) ;
#44301 = CARTESIAN_POINT ( 'NONE',  ( -12.76303204517000012, -18.73514852243999940, 1.980584515753000208 ) ) ;
#44302 = CARTESIAN_POINT ( 'NONE',  ( 0.06739636946983651455, -78.87920693182361731, -1.272432065101433807 ) ) ;
#44303 = CARTESIAN_POINT ( 'NONE',  ( 10.65351345285000129, -78.28938061935399162, -5.379419444189999844 ) ) ;
#44304 = CARTESIAN_POINT ( 'NONE',  ( -8.871933854994999535, -78.72370584965399587, -3.979018739998999354 ) ) ;
#44305 = CARTESIAN_POINT ( 'NONE',  ( -8.517419447173999458, -77.10976152403689809, 3.788002893487000033 ) ) ;
#44306 = CARTESIAN_POINT ( 'NONE',  ( -12.70556836343000029, -53.57227722738999631, 1.774192865971000122E-09 ) ) ;
#44307 = CARTESIAN_POINT ( 'NONE',  ( 9.182347698127177438, -76.00326530161947858, 7.331077060909383825 ) ) ;
#44308 = CARTESIAN_POINT ( 'NONE',  ( -3.649946715412256015, -85.94828561723799965, 1.543298655875836367 ) ) ;
#44309 = ORIENTED_EDGE ( 'NONE', *, *, #23579, .T. ) ;
#44310 = CARTESIAN_POINT ( 'NONE',  ( -8.852883971327290880, -77.14144752210202682, 7.763934591146516517 ) ) ;
#44311 = CARTESIAN_POINT ( 'NONE',  ( 5.385928292795701289, -78.86210492683198936, -10.60790267139944021 ) ) ;
#44312 = CARTESIAN_POINT ( 'NONE',  ( -0.03769889196560113204, -78.69999999999998863, -3.999822345247804556 ) ) ;
#44313 = CIRCLE ( 'NONE', #12290, 11.00000000000000000 ) ;
#44314 = CARTESIAN_POINT ( 'NONE',  ( -8.649885944100999424, -77.88881474799100602, -7.141259254888000285 ) ) ;
#44315 = CARTESIAN_POINT ( 'NONE',  ( 6.083963560182000130, -78.60190654778497787, -9.135064530700001129 ) ) ;
#44316 = CARTESIAN_POINT ( 'NONE',  ( 8.694733073939660883, -80.32630208333191035, 6.682997992873382920 ) ) ;
#44317 = EDGE_CURVE ( 'NONE', #20614, #54465, #31028, .T. ) ;
#44318 = CARTESIAN_POINT ( 'NONE',  ( 11.91558074863000094, -76.77803088996098779, 2.926857068649999949 ) ) ;
#44319 = CARTESIAN_POINT ( 'NONE',  ( 0.3141224841222575170, -78.56945284321614054, 11.74397421471209313 ) ) ;
#44320 = CARTESIAN_POINT ( 'NONE',  ( 9.249483092228999226, -79.25084128437099196, 0.09778817195952001218 ) ) ;
#44321 = EDGE_LOOP ( 'NONE', ( #57369, #35091, #50693, #57634 ) ) ;
#44322 = CARTESIAN_POINT ( 'NONE',  ( -3.953505135776000046, -79.04530346938999230, 10.29910343295999908 ) ) ;
#44323 = CARTESIAN_POINT ( 'NONE',  ( 0.5265852960253567527, -79.94056130876022337, 1.134781841323134088 ) ) ;
#44324 = CARTESIAN_POINT ( 'NONE',  ( 10.53393757967567090, -75.80000000000001137, -5.616035657633564604 ) ) ;
#44325 = CARTESIAN_POINT ( 'NONE',  ( -10.51276546006999979, -78.28204647501199531, 3.399949415165999689 ) ) ;
#44326 = CARTESIAN_POINT ( 'NONE',  ( -11.79999999988000070, -23.14999999478999726, 0.5999999998848000171 ) ) ;
#44327 = CARTESIAN_POINT ( 'NONE',  ( -10.07627163191000008, -55.55000000278000272, -7.601397897754999633 ) ) ;
#44328 = CARTESIAN_POINT ( 'NONE',  ( -6.947761447124999989, -78.40373404223500131, -10.12543283296999874 ) ) ;
#44329 = VECTOR ( 'NONE', #26977, 1000.000000000000000 ) ;
#44330 = CIRCLE ( 'NONE', #26410, 13.94827586206999825 ) ;
#44331 = LINE ( 'NONE', #44630, #17955 ) ;
#44332 = CARTESIAN_POINT ( 'NONE',  ( 4.054145691792253814, -79.54511357774050850, 10.29526509435834036 ) ) ;
#44333 = DIRECTION ( 'NONE',  ( 0.000000000000000000, -0.1122098755727947705, 0.9936845293270585300 ) ) ;
#44334 = ORIENTED_EDGE ( 'NONE', *, *, #14364, .F. ) ;
#44335 = ORIENTED_EDGE ( 'NONE', *, *, #57513, .F. ) ;
#44336 = DIRECTION ( 'NONE',  ( 0.000000000000000000, -1.000000000000000000, -1.820765760384999999E-13 ) ) ;
#44337 = CARTESIAN_POINT ( 'NONE',  ( 7.275511224484000117, -77.93533998579799515, 6.174641004814999334 ) ) ;
#44338 = ORIENTED_EDGE ( 'NONE', *, *, #32753, .F. ) ;
#44339 = CARTESIAN_POINT ( 'NONE',  ( 9.889431646000000242, -78.85235367036999321, 7.252463523969000292 ) ) ;
#44340 = VERTEX_POINT ( 'NONE', #26600 ) ;
#44341 = CARTESIAN_POINT ( 'NONE',  ( 7.657745562908000458, -23.66920625126000033, 9.966193613329998868 ) ) ;
#44342 = CARTESIAN_POINT ( 'NONE',  ( -3.157677208335999630, -76.67505786966898995, -10.45009290908999944 ) ) ;
#44343 = CARTESIAN_POINT ( 'NONE',  ( 1.500000000000000000, -79.65000000000000568, 0.000000000000000000 ) ) ;
#44344 = CARTESIAN_POINT ( 'NONE',  ( -9.249888792690324379, -78.10286309832869733, -0.3112582798825216379 ) ) ;
#44345 = CARTESIAN_POINT ( 'NONE',  ( -6.206245474241999460, -79.68776324199299665, 9.343480492029000217 ) ) ;
#44346 = VERTEX_POINT ( 'NONE', #40198 ) ;
#44347 = AXIS2_PLACEMENT_3D ( 'NONE', #27397, #50443, #40991 ) ;
#44349 = ORIENTED_EDGE ( 'NONE', *, *, #57533, .T. ) ;
#44348 = EDGE_CURVE ( 'NONE', #3688, #10604, #51974, .T. ) ;
#44350 = CARTESIAN_POINT ( 'NONE',  ( -1.170847499494476862, -77.48521246895937509, 9.179786802956089176 ) ) ;
#44351 = CARTESIAN_POINT ( 'NONE',  ( 9.391860901740999523, -77.10358982349210066, 5.803232400709999794 ) ) ;
#44352 = B_SPLINE_CURVE_WITH_KNOTS ( 'NONE', 3,
 ( #2622, #56636, #11764, #29741, #47793, #7325, #1367, #32912, #1660, #2242, #1958, #19074, #19951, #42387, #55666, #19363, #15215, #37939 ),
 .UNSPECIFIED., .F., .F.,
 ( 4, 2, 2, 2, 2, 2, 2, 2, 4 ),
 ( 0.000000000000000000, 0.1249999999999999722, 0.2499999999999999445, 0.3749999999999998890, 0.4999999999999998890, 0.6249999999999998890, 0.7499999999999997780, 0.8749999999999998890, 1.000000000000000000 ),
 .UNSPECIFIED. ) ;
#44353 = LINE ( 'NONE', #30760, #24338 ) ;
#44354 = CARTESIAN_POINT ( 'NONE',  ( -3.536681740116999872, -78.29514014419099510, 9.036735673663999435 ) ) ;
#44355 = CARTESIAN_POINT ( 'NONE',  ( 12.11913442928999984, -76.19745797811999921, 4.608623306100999351 ) ) ;
#44356 = CARTESIAN_POINT ( 'NONE',  ( 3.174095336822680746, -2.230252669283250277, -0.8063667267729033306 ) ) ;
#44357 = CARTESIAN_POINT ( 'NONE',  ( 7.610717068315568490, -55.27984996805254525, -10.41172376761247875 ) ) ;
#44358 = CARTESIAN_POINT ( 'NONE',  ( -1.635010352784000087, -80.42239520082898707, -10.62493487727000030 ) ) ;
#44359 = CARTESIAN_POINT ( 'NONE',  ( 0.000000000000000000, -0.2000000000000000111, 0.000000000000000000 ) ) ;
#44360 = CARTESIAN_POINT ( 'NONE',  ( 0.3271848554491016414, -78.14583333333330017, -1.217465845835393967 ) ) ;
#44361 = EDGE_CURVE ( 'NONE', #14201, #2137, #49452, .T. ) ;
#44362 = CARTESIAN_POINT ( 'NONE',  ( -5.795199452793384332, -79.22747400600979972, 7.554545710430467409 ) ) ;
#44363 = ORIENTED_EDGE ( 'NONE', *, *, #4584, .T. ) ;
#44364 = CARTESIAN_POINT ( 'NONE',  ( 7.469016288970999895, -78.89729054645600570, 9.172865387330000786 ) ) ;
#44365 = VECTOR ( 'NONE', #9184, 1000.000000000000000 ) ;
#44366 = CARTESIAN_POINT ( 'NONE',  ( -8.870405106233999248, -53.73036971739000478, 8.878274241729000593 ) ) ;
#44367 = CARTESIAN_POINT ( 'NONE',  ( -11.74098051674999965, -78.68576600688699330, 2.380218674853999961 ) ) ;
#44368 = CARTESIAN_POINT ( 'NONE',  ( -12.70619440583237214, -61.26151788281449484, 1.571771935835015510 ) ) ;
#44369 = AXIS2_PLACEMENT_3D ( 'NONE', #54242, #23231, #13777 ) ;
#44371 = CARTESIAN_POINT ( 'NONE',  ( -1.666727925315000025, -18.80825518223999993, -12.50018462903999961 ) ) ;
#44370 = CARTESIAN_POINT ( 'NONE',  ( -9.249777342727782070, -78.58959268168034384, 1.210717463251290482 ) ) ;
#44372 = CARTESIAN_POINT ( 'NONE',  ( 0.000000000000000000, 4.040000000000000036, 0.000000000000000000 ) ) ;
#44373 = CARTESIAN_POINT ( 'NONE',  ( 5.550018459581000485, -80.45535737381698027, 9.959756219182001047 ) ) ;
#44374 = FACE_BOUND ( 'NONE', #57753, .T. ) ;
#44375 = CARTESIAN_POINT ( 'NONE',  ( 0.1398360057836000037, -77.19742129968800270, 11.26119045437999944 ) ) ;
#44376 = CARTESIAN_POINT ( 'NONE',  ( 6.043427764450761686, -78.13333333333331154, 10.48543666025110888 ) ) ;
#44377 = CARTESIAN_POINT ( 'NONE',  ( -10.34222918238999966, -80.85569262628774823, -4.442072403260000080 ) ) ;
#44378 = ORIENTED_EDGE ( 'NONE', *, *, #18570, .F. ) ;
#44379 = DIRECTION ( 'NONE',  ( 0.7071067811864980568, -1.536189447283994854E-11, 0.7071067811865969777 ) ) ;
#44380 = CARTESIAN_POINT ( 'NONE',  ( -1.576170184336000091, -54.63913032751000287, 12.55466896101999907 ) ) ;
#44381 = CARTESIAN_POINT ( 'NONE',  ( -12.82904109062999964, -23.32452273707999879, 2.062673488410000200 ) ) ;
#44382 = CARTESIAN_POINT ( 'NONE',  ( 3.221176052379999710, -2.342669754918000002, -1.707589208867000163 ) ) ;
#44383 = CARTESIAN_POINT ( 'NONE',  ( 9.423985469995999509, -79.21901863870799332, 1.441710213756000059 ) ) ;
#44384 = CARTESIAN_POINT ( 'NONE',  ( -3.250000000000001332, -1.510416666666666741, -0.4254240051736181139 ) ) ;
#44385 = CARTESIAN_POINT ( 'NONE',  ( 3.321932689531000182, -77.19999999999998863, 10.22385755016999909 ) ) ;
#44386 = EDGE_CURVE ( 'NONE', #38967, #45976, #51350, .T. ) ;
#44387 = CARTESIAN_POINT ( 'NONE',  ( -1.930009203933999995, -60.00099032284000344, 12.72537718780000127 ) ) ;
#44388 = CARTESIAN_POINT ( 'NONE',  ( 12.43646312222999839, -17.07951485557000026, 0.1257251053153000120 ) ) ;
#44389 = CARTESIAN_POINT ( 'NONE',  ( 1.269300699276999955, -83.70524735065198740, -3.977244714148000071 ) ) ;
#44390 = CARTESIAN_POINT ( 'NONE',  ( 0.000000000000000000, -75.15999999999999659, 0.000000000000000000 ) ) ;
#44391 = CARTESIAN_POINT ( 'NONE',  ( 11.86339925601972922, -77.19009386423427088, -1.944120246756255943 ) ) ;
#44392 = AXIS2_PLACEMENT_3D ( 'NONE', #47133, #42682, #42395 ) ;
#44393 = CARTESIAN_POINT ( 'NONE',  ( 2.866472250631999952, -78.13111084099200809, 10.89115702734000024 ) ) ;
#44394 = CARTESIAN_POINT ( 'NONE',  ( 0.8296278938361448807, -81.91774775679489551, 0.9347690852748764545 ) ) ;
#44395 = CARTESIAN_POINT ( 'NONE',  ( -1.391773598262999956, -79.42952316759999576, -0.6803270823529999900 ) ) ;
#44396 = CARTESIAN_POINT ( 'NONE',  ( 7.559982449049000408, -77.08685820500399188, -6.032732969207000195 ) ) ;
#44397 = FACE_OUTER_BOUND ( 'NONE', #8252, .T. ) ;
#44398 = FACE_OUTER_BOUND ( 'NONE', #23935, .T. ) ;
#44399 = CARTESIAN_POINT ( 'NONE',  ( -5.965906064879229476, -80.17825941931280909, -8.942563257856061654 ) ) ;
#44400 = ADVANCED_FACE ( 'NONE', ( #17699 ), #43982, .T. ) ;
#44401 = CARTESIAN_POINT ( 'NONE',  ( -12.54435915805012414, -23.52412882219291035, -1.733925320388666202 ) ) ;
#44402 = CARTESIAN_POINT ( 'NONE',  ( 8.728206860394864819, -75.80000000000001137, 8.278571939072135066 ) ) ;
#44403 = B_SPLINE_CURVE_WITH_KNOTS ( 'NONE', 3,
 ( #53089, #12642, #30635, #31507, #4962, #41557 ),
 .UNSPECIFIED., .F., .F.,
 ( 4, 1, 1, 4 ),
 ( 0.000000000000000000, 0.3333333333333000081, 0.6666666666667000474, 1.000000000000000000 ),
 .UNSPECIFIED. ) ;
#44404 = ORIENTED_EDGE ( 'NONE', *, *, #32547, .T. ) ;
#44405 = CARTESIAN_POINT ( 'NONE',  ( 1.199037830717708752, -81.82746532552805263, -0.3535722597945603063 ) ) ;
#44406 = CARTESIAN_POINT ( 'NONE',  ( 0.000000000000000000, -75.15999999999999659, 0.000000000000000000 ) ) ;
#44407 = CARTESIAN_POINT ( 'NONE',  ( 10.42771306556999988, -80.11239375944418839, -3.939212573787000515 ) ) ;
#44408 = DIRECTION ( 'NONE',  ( 0.7272727272724163194, -0.6863485850246158204, 6.703676216208155796E-07 ) ) ;
#44409 = ORIENTED_EDGE ( 'NONE', *, *, #10969, .F. ) ;
#44410 = ORIENTED_EDGE ( 'NONE', *, *, #40953, .F. ) ;
#44411 = CARTESIAN_POINT ( 'NONE',  ( -0.9950304368180999948, -80.56410876238999208, -1.271568498479000109 ) ) ;
#44412 = VECTOR ( 'NONE', #46415, 1000.000000000000000 ) ;
#44413 = VERTEX_POINT ( 'NONE', #3535 ) ;
#44414 = DIRECTION ( 'NONE',  ( 1.000000000000000000, 0.000000000000000000, 0.000000000000000000 ) ) ;
#44415 = ORIENTED_EDGE ( 'NONE', *, *, #35758, .F. ) ;
#44416 = VECTOR ( 'NONE', #52051, 1000.000000000000000 ) ;
#44417 = CARTESIAN_POINT ( 'NONE',  ( -1.374053708643000007E-14, -74.80000000000001137, 0.000000000000000000 ) ) ;
#44418 = CARTESIAN_POINT ( 'NONE',  ( 7.698699457163000304, -79.38612155000399184, 7.739857405570000459 ) ) ;
#44420 = ADVANCED_FACE ( 'NONE', ( #44858 ), #53407, .T. ) ;
#44419 = CARTESIAN_POINT ( 'NONE',  ( 0.4802748259353999960, -25.00526907281999911, -12.54896097834000024 ) ) ;
#44421 = CARTESIAN_POINT ( 'NONE',  ( -1.861077379058000192, -80.25345679254499487, 3.263090789613000364 ) ) ;
#44422 = CARTESIAN_POINT ( 'NONE',  ( -6.391975584201730065, -79.33365083746186031, 7.030076347870032549 ) ) ;
#44423 = ORIENTED_EDGE ( 'NONE', *, *, #57675, .F. ) ;
#44424 = CARTESIAN_POINT ( 'NONE',  ( -12.50000000000000000, -23.25000000000000000, 0.000000000000000000 ) ) ;
#44425 = CARTESIAN_POINT ( 'NONE',  ( 12.25699876382000042, -79.26582643418001339, 1.580520632500000078 ) ) ;
#44426 = ORIENTED_EDGE ( 'NONE', *, *, #55841, .F. ) ;
#44428 = ORIENTED_EDGE ( 'NONE', *, *, #56141, .T. ) ;
#44427 = ADVANCED_FACE ( 'NONE', ( #52838 ), #8249, .F. ) ;
#44429 = CARTESIAN_POINT ( 'NONE',  ( -0.1461529444412975054, -77.86763493222619559, -1.524614525945181320 ) ) ;
#44430 = CARTESIAN_POINT ( 'NONE',  ( 0.3292142484335000563, -79.41051030923300402, -1.292352404326999826 ) ) ;
#44431 = CARTESIAN_POINT ( 'NONE',  ( 1.260641617779999946, -77.57417861372799450, 9.621927669549000584 ) ) ;
#44432 = CARTESIAN_POINT ( 'NONE',  ( -3.523111701668359963, -86.40321104920798234, -2.458856237079841467 ) ) ;
#44433 = FACE_BOUND ( 'NONE', #51715, .T. ) ;
#44434 = CARTESIAN_POINT ( 'NONE',  ( 5.554685856605999561, -76.84581360187000598, 11.87889705760999881 ) ) ;
#44435 = CARTESIAN_POINT ( 'NONE',  ( 12.17287523535000027, -77.47264530806999971, -3.409737174454000375 ) ) ;
#44436 = CARTESIAN_POINT ( 'NONE',  ( -1.616093070969999879, -76.91344993108998551, 10.76376729404999999 ) ) ;
#44437 = ADVANCED_FACE ( 'NONE', ( #31246 ), #31545, .F. ) ;
#44438 = CARTESIAN_POINT ( 'NONE',  ( -8.731575513440832381, -78.62679321767426188, -3.053146778519897797 ) ) ;
#44439 = B_SPLINE_CURVE_WITH_KNOTS ( 'NONE', 3,
 ( #48573, #39414, #40582, #12823, #12541, #45314, #8997, #26981, #179, #31104, #35845, #18152, #53874, #26396, #53276, #54162, #8115, #4271 ),
 .UNSPECIFIED., .F., .F.,
 ( 4, 2, 2, 2, 2, 2, 2, 2, 4 ),
 ( 0.000000000000000000, 0.1250000000000000833, 0.2500000000000001665, 0.3750000000000001665, 0.5000000000000002220, 0.6250000000000002220, 0.7500000000000001110, 0.8750000000000001110, 1.000000000000000000 ),
 .UNSPECIFIED. ) ;
#44440 = CIRCLE ( 'NONE', #39713, 2.299999999999999822 ) ;
#44441 = CARTESIAN_POINT ( 'NONE',  ( -10.55911395186000057, -56.01538333533000014, 7.642160924870000649 ) ) ;
#44442 = CARTESIAN_POINT ( 'NONE',  ( 1.721677682318950575, -2.931119376536615917, 2.765314047765481398 ) ) ;
#44443 = CARTESIAN_POINT ( 'NONE',  ( -3.502948155309999922, -81.56417549782598542, -0.7830018197964999649 ) ) ;
#44444 = DIRECTION ( 'NONE',  ( 0.000000000000000000, -1.000000000000000000, 0.000000000000000000 ) ) ;
#44445 = CARTESIAN_POINT ( 'NONE',  ( -11.03620408507000050, -80.34997377947260588, -2.260839449595000161 ) ) ;
#44446 = CARTESIAN_POINT ( 'NONE',  ( 3.702420020526000055, -2.516613097741000171, 0.8821385418971999792 ) ) ;
#44447 = CARTESIAN_POINT ( 'NONE',  ( 1.180314793947099261, -79.53115984866582266, 0.4804541877614367240 ) ) ;
#44448 = ORIENTED_EDGE ( 'NONE', *, *, #46354, .F. ) ;
#44449 = CARTESIAN_POINT ( 'NONE',  ( 9.249483092228999226, -78.85084128437098627, 0.09778817195952001218 ) ) ;
#44450 = CARTESIAN_POINT ( 'NONE',  ( 2.879226727952094222, -79.34583333333331723, -10.71369944335146940 ) ) ;
#44451 = CARTESIAN_POINT ( 'NONE',  ( 1.304222966381000104, -81.44485601252800677, 0.2785293583740000023 ) ) ;
#44452 = AXIS2_PLACEMENT_3D ( 'NONE', #20842, #38846, #52436 ) ;
#44453 = CARTESIAN_POINT ( 'NONE',  ( -12.55458938220999876, -17.83720883386000011, -1.575070636625000242 ) ) ;
#44454 = CARTESIAN_POINT ( 'NONE',  ( 11.85869973992999959, -77.76643789029000686, 5.358216250391999225 ) ) ;
#44455 = VECTOR ( 'NONE', #47134, 1000.000000000000000 ) ;
#44456 = CARTESIAN_POINT ( 'NONE',  ( -10.36597333715949176, -60.57522428981332752, -7.635925938723863382 ) ) ;
#44457 = CARTESIAN_POINT ( 'NONE',  ( 9.998734510784624163, -18.07263061081724942, 7.709128441133644927 ) ) ;
#44458 = ORIENTED_EDGE ( 'NONE', *, *, #30472, .T. ) ;
#44459 = CARTESIAN_POINT ( 'NONE',  ( -10.10912542004608561, -55.32413588744719135, 7.634643956462955572 ) ) ;
#44460 = CARTESIAN_POINT ( 'NONE',  ( 8.251806177857083924, -53.99944067038419604, -9.431051272625094128 ) ) ;
#44461 = CARTESIAN_POINT ( 'NONE',  ( 0.1719131973598000129, -81.37741046657400545, -1.299333209432999903 ) ) ;
#44462 = CARTESIAN_POINT ( 'NONE',  ( -2.062670899148999926, -23.30639625649999758, -12.83044039274999903 ) ) ;
#44463 = CARTESIAN_POINT ( 'NONE',  ( -7.921993249237998747, -78.50374277172099369, -5.283218639336999978 ) ) ;
#44464 = CARTESIAN_POINT ( 'NONE',  ( 3.029714949896999965, -83.78155969446399354, -2.868954476365999984 ) ) ;
#44465 = CARTESIAN_POINT ( 'NONE',  ( -1.667936688463999895, -56.03513569577999931, -12.53239398060000021 ) ) ;
#44466 = CARTESIAN_POINT ( 'NONE',  ( -0.5179932711920000044, -79.19792250334801054, -1.319781611125000031 ) ) ;
#44467 = ORIENTED_EDGE ( 'NONE', *, *, #51070, .F. ) ;
#44468 = EDGE_CURVE ( 'NONE', #56551, #38752, #57597, .T. ) ;
#44469 = CARTESIAN_POINT ( 'NONE',  ( 8.166441406547827242, -77.29381170557186920, -6.992710802927438962 ) ) ;
#44470 = CARTESIAN_POINT ( 'NONE',  ( -8.604107503949739666, -79.06923224600832611, 3.550580747324208364 ) ) ;
#44471 = CARTESIAN_POINT ( 'NONE',  ( 1.630469595029759189, -78.93919352839404269, -3.527628001382114409 ) ) ;
#44472 = VERTEX_POINT ( 'NONE', #21537 ) ;
#44473 = EDGE_CURVE ( 'NONE', #57766, #53695, #31498, .T. ) ;
#44474 = ORIENTED_EDGE ( 'NONE', *, *, #41654, .T. ) ;
#44475 = CARTESIAN_POINT ( 'NONE',  ( -10.40934573790000073, -78.34592221579498528, 3.366502286031999969 ) ) ;
#44476 = CARTESIAN_POINT ( 'NONE',  ( 12.60552522433000000, -55.51082434643999619, 1.799501877760999902 ) ) ;
#44477 = CARTESIAN_POINT ( 'NONE',  ( -9.616088855336998975, -79.70165346197198630, 5.532765289540999554 ) ) ;
#44478 = VERTEX_POINT ( 'NONE', #9721 ) ;
#44479 = MECHANICAL_DESIGN_GEOMETRIC_PRESENTATION_REPRESENTATION (  '', ( #57667 ), #1147 ) ;
#44480 = CARTESIAN_POINT ( 'NONE',  ( -10.32936100969000037, -78.64809032934199706, 6.204842689816000068 ) ) ;
#44481 = EDGE_LOOP ( 'NONE', ( #30640, #38542, #55316, #7464 ) ) ;
#44482 = EDGE_LOOP ( 'NONE', ( #49059, #31468, #11123, #4204, #2948, #29950, #47213, #33860, #36065, #3962, #12612, #5715 ) ) ;
#44483 = CARTESIAN_POINT ( 'NONE',  ( 11.38757821100306522, -76.62325149914207145, -3.866458184269738307 ) ) ;
#44484 = LINE ( 'NONE', #53945, #11033 ) ;
#44485 = VERTEX_POINT ( 'NONE', #50764 ) ;
#44486 = CARTESIAN_POINT ( 'NONE',  ( 1.406250000003000045, -82.09374999999700151, -9.314605757769000352E-11 ) ) ;
#44488 = EDGE_CURVE ( 'NONE', #37542, #27414, #45754, .T. ) ;
#44487 = ORIENTED_EDGE ( 'NONE', *, *, #35209, .F. ) ;
#44489 = CARTESIAN_POINT ( 'NONE',  ( 1.219314106501412365, -79.87620745940748179, -0.3721447959605043154 ) ) ;
#44490 = CIRCLE ( 'NONE', #33192, 10.50000000000000000 ) ;
#44491 = CARTESIAN_POINT ( 'NONE',  ( -2.060841138106245474, -78.85171435493610659, -3.417916573713450479 ) ) ;
#44492 = CARTESIAN_POINT ( 'NONE',  ( 0.000000000000000000, -80.99999999999998579, 7.000000000000000000 ) ) ;
#44493 = CARTESIAN_POINT ( 'NONE',  ( -10.67244467921999984, -76.67714362518299254, 2.904229794498999873 ) ) ;
#44494 = CARTESIAN_POINT ( 'NONE',  ( -9.312500000004000356, -79.68749999999599254, 6.570867420027000168E-10 ) ) ;
#44495 = B_SPLINE_CURVE_WITH_KNOTS ( 'NONE', 3,
 ( #31419, #40296, #35857, #36157, #13714, #42348, #1619, #5733, #33168, #15174, #46794, #41462, #55039, #50628, #37900, #24034, #32873, #5161, #6319, #51213, #23741, #37609, #24336, #10178, #5445, #10765, #28743, #14588, #27864, #55924 ),
 .UNSPECIFIED., .F., .F.,
 ( 4, 2, 2, 2, 2, 2, 2, 2, 2, 2, 2, 2, 2, 2, 4 ),
 ( 0.000000000000000000, 0.1250000000000041633, 0.1875000000000046907, 0.2500000000000052180, 0.3125000000000057176, 0.3750000000000062728, 0.5000000000000072164, 0.5625000000000077716, 0.6250000000000082157, 0.6875000000000087708, 0.7500000000000093259, 0.8125000000000098810, 0.8437500000000087708, 0.8750000000000075495, 1.000000000000000000 ),
 .UNSPECIFIED. ) ;
#44496 = CARTESIAN_POINT ( 'NONE',  ( 8.190859204290999784, -55.64999999967000122, -7.342331066867000544 ) ) ;
#44497 = CARTESIAN_POINT ( 'NONE',  ( -8.885616033064000163, -78.09149724519254221, 8.035041515002001589 ) ) ;
#44498 = EDGE_CURVE ( 'NONE', #55676, #21570, #23094, .T. ) ;
#44499 = CARTESIAN_POINT ( 'NONE',  ( 12.00000000000000000, -18.75000000000000000, -1.250000000000000000 ) ) ;
#44500 = DIRECTION ( 'NONE',  ( -1.000000000000000000, 0.000000000000000000, 0.000000000000000000 ) ) ;
#44501 = EDGE_CURVE ( 'NONE', #41372, #50093, #17352, .T. ) ;
#44502 = CARTESIAN_POINT ( 'NONE',  ( 1.961272738943000027, -79.65175264934788402, 3.685513403684000266 ) ) ;
#44503 = CARTESIAN_POINT ( 'NONE',  ( 0.7189379956714000430, -77.68986001420199727, 9.846538930731000505 ) ) ;
#44504 = AXIS2_PLACEMENT_3D ( 'NONE', #23562, #9413, #27403 ) ;
#44505 = CARTESIAN_POINT ( 'NONE',  ( -12.52582323433392197, -23.80939730775229890, 1.680974276152719771 ) ) ;
#44506 = CARTESIAN_POINT ( 'NONE',  ( -8.796335266380006956, -78.04791666666666572, 6.760013919724027431 ) ) ;
#44507 = CARTESIAN_POINT ( 'NONE',  ( -1.798368564625000054, -23.19636757045999786, 12.61278090841000044 ) ) ;
#44508 = DIRECTION ( 'NONE',  ( 0.000000000000000000, 0.8191944460894394764, 0.5735158755398287456 ) ) ;
#44509 = CARTESIAN_POINT ( 'NONE',  ( -1.557495164653000197, -85.95233266374599168, 3.187306976996000074 ) ) ;
#44510 = CARTESIAN_POINT ( 'NONE',  ( -0.4165118319448999351, -1.439790208251000125, 3.598914716717999784 ) ) ;
#44511 = CARTESIAN_POINT ( 'NONE',  ( -9.983732787439539180, -78.13092931071430769, -4.071056266153238568 ) ) ;
#44512 = CARTESIAN_POINT ( 'NONE',  ( 0.2546825748345945550, -80.21164111392475604, 1.525549965237892769 ) ) ;
#44513 = CARTESIAN_POINT ( 'NONE',  ( 12.43640309388999832, -61.71747517570000241, 0.05224034426410999882 ) ) ;
#44514 = CARTESIAN_POINT ( 'NONE',  ( 1.190716386653000169, -79.21706751772300947, 1.090600000265000036 ) ) ;
#44515 = CARTESIAN_POINT ( 'NONE',  ( 0.000000000000000000, -15.69705297114000331, -12.53545825868000207 ) ) ;
#44516 = CARTESIAN_POINT ( 'NONE',  ( -7.639223145873000220, -76.96482100489700429, 7.500260266847000423 ) ) ;
#44517 = CARTESIAN_POINT ( 'NONE',  ( -5.830174433585000315, -77.78777695645399604, 10.80762903023000021 ) ) ;
#44518 = CARTESIAN_POINT ( 'NONE',  ( 0.000000000000000000, -26.93717104351999936, 0.000000000000000000 ) ) ;
#44519 = EDGE_CURVE ( 'NONE', #3012, #23500, #5116, .T. ) ;
#44521 = CARTESIAN_POINT ( 'NONE',  ( -0.7468003766476000171, -78.26866860913609969, 1.319557257415000073 ) ) ;
#44520 = DIRECTION ( 'NONE',  ( -0.7071067811865474617, -0.7071067811865474617, 1.305612310955086883E-09 ) ) ;
#44522 = CARTESIAN_POINT ( 'NONE',  ( -0.5667803598935999831, -82.17197637046999148, 1.605794812195000087 ) ) ;
#44523 = ORIENTED_EDGE ( 'NONE', *, *, #21169, .T. ) ;
#44524 = CARTESIAN_POINT ( 'NONE',  ( -1.250000000000000000, -83.09999999999999432, 0.000000000000000000 ) ) ;
#44525 = CARTESIAN_POINT ( 'NONE',  ( 10.30142167872999970, -80.92276737670430009, 4.324873734307999484 ) ) ;
#44526 = CARTESIAN_POINT ( 'NONE',  ( -10.07627163191000008, -23.24999999688999708, 7.601397897754999633 ) ) ;
#44527 = CARTESIAN_POINT ( 'NONE',  ( 3.083885533095168885, -85.56041667406407214, 1.532545329980541604 ) ) ;
#44528 = CARTESIAN_POINT ( 'NONE',  ( -10.35410175341000105, -60.20399325318000194, 7.619715687221999545 ) ) ;
#44529 = LINE ( 'NONE', #14401, #7608 ) ;
#44530 = CIRCLE ( 'NONE', #28517, 2.899999999999999911 ) ;
#44531 = CARTESIAN_POINT ( 'NONE',  ( 3.586056226710999884, -1.401363919000000013, 0.9161727453457999548 ) ) ;
#44532 = CARTESIAN_POINT ( 'NONE',  ( 8.963249880471998665, -78.87092023966599186, -2.560381131858999737 ) ) ;
#44533 = CARTESIAN_POINT ( 'NONE',  ( 12.82202361517000000, -23.42627773034000427, -2.066043355638000012 ) ) ;
#44534 = LINE ( 'NONE', #40101, #1012 ) ;
#44535 = EDGE_LOOP ( 'NONE', ( #13919, #8515, #505, #53714 ) ) ;
#44536 = EDGE_CURVE ( 'NONE', #30361, #23662, #18300, .T. ) ;
#44537 = CARTESIAN_POINT ( 'NONE',  ( 0.000000000000000000, -77.01875000000549676, 0.000000000000000000 ) ) ;
#44538 = DIRECTION ( 'NONE',  ( -1.000000000000000000, 0.000000000000000000, 0.000000000000000000 ) ) ;
#44539 = DIRECTION ( 'NONE',  ( -1.000000000000000000, 0.000000000000000000, 0.000000000000000000 ) ) ;
#44540 = EDGE_CURVE ( 'NONE', #53636, #8280, #25828, .T. ) ;
#44541 = CARTESIAN_POINT ( 'NONE',  ( -1.460959015002473826, -78.42083333333336270, -0.3926218265389207485 ) ) ;
#44542 = CARTESIAN_POINT ( 'NONE',  ( -1.557331793415999810, -85.91467953870898100, 3.187385650886000121 ) ) ;
#44543 = AXIS2_PLACEMENT_3D ( 'NONE', #43960, #3793, #3510 ) ;
#44544 = ORIENTED_EDGE ( 'NONE', *, *, #14587, .F. ) ;
#44545 = CARTESIAN_POINT ( 'NONE',  ( -10.78523893070000028, -77.41014297881199013, 2.631402515253999930 ) ) ;
#44546 = DIRECTION ( 'NONE',  ( 0.000000000000000000, -1.000000000000000000, 0.000000000000000000 ) ) ;
#44547 = CARTESIAN_POINT ( 'NONE',  ( 1.997276839918477265, -1.177083333333333481, -2.598917237794082791 ) ) ;
#44548 = VERTEX_POINT ( 'NONE', #10309 ) ;
#44549 = ORIENTED_EDGE ( 'NONE', *, *, #41879, .T. ) ;
#44550 = AXIS2_PLACEMENT_3D ( 'NONE', #4694, #22987, #33284 ) ;
#44551 = CARTESIAN_POINT ( 'NONE',  ( -12.60552511008000032, -55.51082276539999327, 1.799501877793999949 ) ) ;
#44552 = CARTESIAN_POINT ( 'NONE',  ( -7.961057357800999768, -54.26431744618999886, -9.783210913615000948 ) ) ;
#44553 = SHAPE_REPRESENTATION_RELATIONSHIP ( 'NONE' , 'NONE' ,  #7879, #11003 ) ;
#44554 = CARTESIAN_POINT ( 'NONE',  ( -5.809791519574999619, -79.19554259676998242, 7.851562197947999699 ) ) ;
#44555 = VERTEX_POINT ( 'NONE', #46046 ) ;
#44556 = ORIENTED_EDGE ( 'NONE', *, *, #25410, .T. ) ;
#44557 = CARTESIAN_POINT ( 'NONE',  ( 11.56754288844999934, -76.89980949943999633, 3.984846766858999967 ) ) ;
#44558 = DIRECTION ( 'NONE',  ( 0.000000000000000000, 1.000000000000000000, 0.000000000000000000 ) ) ;
#44559 = CARTESIAN_POINT ( 'NONE',  ( -0.7298471776477999384, -78.68147770778000449, 1.477907092941999956 ) ) ;
#44560 = ORIENTED_EDGE ( 'NONE', *, *, #55472, .T. ) ;
#44561 = CARTESIAN_POINT ( 'NONE',  ( 10.18949731070999931, -18.78470987703000006, 7.645392562261999814 ) ) ;
#44562 = CARTESIAN_POINT ( 'NONE',  ( -1.505183525871029993, -79.25404663310062858, -0.07739674404991536694 ) ) ;
#44563 = CARTESIAN_POINT ( 'NONE',  ( -0.2325945923070667498, -80.21064443203673022, -1.228314969166735215 ) ) ;
#44564 = CARTESIAN_POINT ( 'NONE',  ( 5.759449073023001020, -78.33319635864999952, 11.78163922240000083 ) ) ;
#44565 = CARTESIAN_POINT ( 'NONE',  ( 7.199825537761999961, -77.06953959447203317, 8.601198917431998936 ) ) ;
#44566 = DIRECTION ( 'NONE',  ( 0.7071067811865475727, 0.000000000000000000, 0.7071067811865475727 ) ) ;
#44567 = CARTESIAN_POINT ( 'NONE',  ( 3.677662896325522457, -86.31452044230000809, 2.671197113342799856 ) ) ;
#44568 = CARTESIAN_POINT ( 'NONE',  ( -11.06493808903000087, -79.41479520351799692, -1.839906431680000010 ) ) ;
#44569 = CARTESIAN_POINT ( 'NONE',  ( -0.7613100899427974744, -79.98164650648521956, 9.218583111519835782 ) ) ;
#44570 = CARTESIAN_POINT ( 'NONE',  ( -0.9967936402423711595, -82.25000000000000000, -0.7825337139414764165 ) ) ;
#44571 = ORIENTED_EDGE ( 'NONE', *, *, #33060, .F. ) ;
#44572 = CARTESIAN_POINT ( 'NONE',  ( 0.9331110433225999756, -78.98921517645298707, 11.22756599386000076 ) ) ;
#44573 = CARTESIAN_POINT ( 'NONE',  ( 2.900604236686527670, -77.25055390848557124, -8.783348422349369855 ) ) ;
#44574 = CARTESIAN_POINT ( 'NONE',  ( -1.356492273396000092, -79.45368156769499990, -0.8757286844311999996 ) ) ;
#44575 = CIRCLE ( 'NONE', #41765, 9.000000000000000000 ) ;
#44576 = ADVANCED_FACE ( 'NONE', ( #5571 ), #9431, .F. ) ;
#44577 = CARTESIAN_POINT ( 'NONE',  ( -1.169594621339999918, -78.61977915405600470, 0.6104211924069999906 ) ) ;
#44578 = CARTESIAN_POINT ( 'NONE',  ( -3.580942884975041984, -2.851296129650088496, -0.07958713964337410518 ) ) ;
#44579 = CARTESIAN_POINT ( 'NONE',  ( -7.730439324435801396, -17.87809618957197699, 10.25198230928420173 ) ) ;
#44580 = CARTESIAN_POINT ( 'NONE',  ( -4.000000000000000000, -75.00000000000001421, -0.5999999999999999778 ) ) ;
#44581 = DIRECTION ( 'NONE',  ( 0.000000000000000000, -1.000000000000000000, 0.000000000000000000 ) ) ;
#44582 = CARTESIAN_POINT ( 'NONE',  ( -0.5280093414736000135, -79.17817062466399136, -11.14507989169999824 ) ) ;
#44583 = CARTESIAN_POINT ( 'NONE',  ( -8.175152901933000038, -76.92503998579799429, -5.289553387389999806 ) ) ;
#44584 = B_SPLINE_CURVE_WITH_KNOTS ( 'NONE', 3,
 ( #49573, #22692, #14122, #36560, #22394, #40997, #45437, #54292, #589, #36847 ),
 .UNSPECIFIED., .F., .F.,
 ( 4, 2, 2, 2, 4 ),
 ( 0.000000000000000000, 0.2499999999999998890, 0.4999999999999998890, 0.7499999999999998890, 1.000000000000000000 ),
 .UNSPECIFIED. ) ;
#44585 = DIRECTION ( 'NONE',  ( 1.000000000000000000, 0.000000000000000000, 0.000000000000000000 ) ) ;
#44586 = DIRECTION ( 'NONE',  ( 0.7071067811865975328, 0.7071067811864976127, 5.769403951028974600E-09 ) ) ;
#44587 = CARTESIAN_POINT ( 'NONE',  ( 8.962106380668664940, -80.05087147346051779, 6.668020604379202965 ) ) ;
#44588 = AXIS2_PLACEMENT_3D ( 'NONE', #5878, #55482, #15331 ) ;
#44589 = B_SPLINE_SURFACE_WITH_KNOTS ( 'NONE', 3, 3, ( 
 ( #25512, #7222, #56819, #16375 ),
 ( #39091, #2512, #10270, #29354 ),
 ( #1140, #37121, #57099, #50730 ),
 ( #47401, #28251, #5828, #23835 ),
 ( #42661, #38222, #56243, #24936 ),
 ( #15793, #42958, #33781, #20516 ),
 ( #38513, #17522, #12513, #16950 ),
 ( #53246, #17227, #48827, #7800 ),
 ( #4239, #35217, #13080, #21370 ),
 ( #18121, #48540, #35811, #12795 ),
 ( #8666, #49115, #22540, #17824 ),
 ( #143, #57967, #26950, #36116 ),
 ( #40550, #53841, #39665, #35512 ),
 ( #44108, #44983, #22238, #8369 ),
 ( #31077, #3657, #13376, #57671 ),
 ( #54133, #26652, #53540, #30795 ),
 ( #26368, #44387, #44688, #13672 ) ),
 .UNSPECIFIED., .F., .F., .F.,
 ( 4, 1, 1, 1, 1, 1, 1, 1, 1, 1, 1, 1, 1, 1, 4 ),
 ( 4, 4 ),
 ( -0.01011408452875999994, 0.000000000000000000, 0.08333333333333001192, 0.1666666666667000196, 0.2500000000000000000, 0.3333333333333000081, 0.4166666666666999919, 0.5000000000000000000, 0.5833333333333000637, 0.6666666666667000474, 0.7500000000000000000, 0.8333333333333000637, 0.9166666666667000474, 1.000000000000000000, 1.010362559108000102 ),
 ( -0.3559705546268999710, 1.357612419623000166 ),
 .UNSPECIFIED. ) ;
#44590 = ORIENTED_EDGE ( 'NONE', *, *, #8876, .F. ) ;
#44591 = CARTESIAN_POINT ( 'NONE',  ( -1.519651782304000109, -81.91638770227000066, -0.4528301974880000191 ) ) ;
#44592 = CARTESIAN_POINT ( 'NONE',  ( -1.273831304311999979, -81.04704884152999966, -0.4509157470602000450 ) ) ;
#44593 = CYLINDRICAL_SURFACE ( 'NONE', #3131, 1.750000000000000000 ) ;
#44594 = CARTESIAN_POINT ( 'NONE',  ( -3.545645331619000196, -77.39722773010799983, 11.44309676683000099 ) ) ;
#44595 = CARTESIAN_POINT ( 'NONE',  ( 9.029734473257063243, -77.00000000000000000, -2.837209596131928802 ) ) ;
#44596 = CONICAL_SURFACE ( 'NONE', #41784, 1.099999997148999986, 0.7853981633972997312 ) ;
#44597 = CARTESIAN_POINT ( 'NONE',  ( 0.8120539164135156529, -79.07002642441428009, 0.9822165099403028510 ) ) ;
#44598 = CARTESIAN_POINT ( 'NONE',  ( 11.90740810048999876, -78.83196692782999548, 0.8057021066547999100 ) ) ;
#44599 = CARTESIAN_POINT ( 'NONE',  ( 9.377128579935000374, -78.29864805011499129, -2.571625947824999869 ) ) ;
#44600 = CARTESIAN_POINT ( 'NONE',  ( -4.778484498315999751, -78.62325255039799288, 8.361775879827998637 ) ) ;
#44602 = EDGE_CURVE ( 'NONE', #57807, #43416, #29618, .T. ) ;
#44601 = CARTESIAN_POINT ( 'NONE',  ( -12.50000000000000000, -18.75000000240999753, -1.750000000000000000 ) ) ;
#44603 = CARTESIAN_POINT ( 'NONE',  ( 11.00423669942431104, -75.97794915958310469, 4.119231451974944669 ) ) ;
#44604 = CARTESIAN_POINT ( 'NONE',  ( 4.614362421890519705, -86.10000000000000853, 0.5296543453898030496 ) ) ;
#44605 = ORIENTED_EDGE ( 'NONE', *, *, #30923, .T. ) ;
#44606 = AXIS2_PLACEMENT_3D ( 'NONE', #19358, #32908, #9042 ) ;
#44607 = CARTESIAN_POINT ( 'NONE',  ( 3.165057598945393291, -2.330483944310657307, -0.8521617472482003741 ) ) ;
#44608 = EDGE_CURVE ( 'NONE', #31908, #11806, #14427, .T. ) ;
#44609 = CARTESIAN_POINT ( 'NONE',  ( -2.265513919728744163, -78.40681307243319509, -3.757367528743593699 ) ) ;
#44610 = CARTESIAN_POINT ( 'NONE',  ( 0.8286895765316001361, -81.60396023938999122, 1.445177540541999983 ) ) ;
#44611 = CARTESIAN_POINT ( 'NONE',  ( 8.282307197233999219, -78.02499646299999370, -7.564489280985000619 ) ) ;
#44612 = CARTESIAN_POINT ( 'NONE',  ( -9.505686244346000180, -79.38849246909899193, 5.486888517706000279 ) ) ;
#44613 = CARTESIAN_POINT ( 'NONE',  ( -10.48321433724633245, -80.43697916666563685, 2.816410591909088268 ) ) ;
#44614 = CARTESIAN_POINT ( 'NONE',  ( 9.264606868682999874, -76.81576362826599791, 8.044539538861000594 ) ) ;
#44615 = CARTESIAN_POINT ( 'NONE',  ( 4.598774055804255134, -78.54242297502504755, 10.81608457866212802 ) ) ;
#44616 = CARTESIAN_POINT ( 'NONE',  ( 9.332634751654579119, -79.20070731308940992, 0.09866879888904338258 ) ) ;
#44617 = ORIENTED_EDGE ( 'NONE', *, *, #3751, .F. ) ;
#44618 = CARTESIAN_POINT ( 'NONE',  ( 2.392795665116000059, -80.06630253886619641, 10.66634390655999987 ) ) ;
#44619 = CARTESIAN_POINT ( 'NONE',  ( 0.8492318889338164034, -79.91594626102744314, 0.9170975991313886633 ) ) ;
#44620 = CARTESIAN_POINT ( 'NONE',  ( -10.99999999999999822, -77.61041666666666572, -1.439896632895323325 ) ) ;
#44621 = CARTESIAN_POINT ( 'NONE',  ( 3.962812355711000212, -78.54828561723799396, -4.853045467043058701E-16 ) ) ;
#44622 = EDGE_CURVE ( 'NONE', #32925, #12786, #5287, .T. ) ;
#44623 = CARTESIAN_POINT ( 'NONE',  ( -7.632977269198000236, -78.80811017521499195, -8.138136006783000198 ) ) ;
#44624 = DIRECTION ( 'NONE',  ( -1.000000000000000000, 0.000000000000000000, 0.000000000000000000 ) ) ;
#44625 = CIRCLE ( 'NONE', #54995, 13.79999999999999893 ) ;
#44626 = CARTESIAN_POINT ( 'NONE',  ( -10.98676125741665643, -23.41445108201299874, 0.5397229578417699347 ) ) ;
#44627 = B_SPLINE_SURFACE_WITH_KNOTS ( 'NONE', 3, 3, ( 
 ( #32900, #28180, #41195, #54201, #27604, #13737, #40618, #18190, #49780, #45938, #5758, #1072, #499, #18477, #36468, #50073, #5186, #23190, #784, #50360, #14613, #18764, #23474, #41485, #27891, #19059, #36757, #23765, #32607, #10201, #54776, #14317, #37047, #15790, #33493 ),
 ( #37924, #52392, #51531, #25220, #11087, #28771, #47397, #34355, #55949, #15201, #6051, #33778, #20793, #19636, #42373, #46820, #2797, #38797, #6345, #43240, #46527, #56816, #34065, #29637, #1942, #51818, #42077, #29066, #16373, #7219, #24059, #24933, #19936, #55652, #15499 ),
 ( #42955, #11373, #1647, #11946, #16084, #6640, #29351, #37634, #52102, #24649, #33191, #6929, #11661, #47109, #51238, #42659, #2226, #2509, #10790, #20227, #24360, #38219, #56241, #20513, #38510, #56525, #47690, #39089, #25509, #17821, #25797, #26648, #44383, #48537, #17518 ),
 ( #43824, #57096, #39383, #35807, #8083, #7796, #26080, #58260, #44685, #13077, #53838, #21937, #8662, #34928, #48262, #57964, #35508, #57388, #12225, #29923, #44105, #53537, #3654, #49113, #4237, #22235, #7510, #21367, #3936, #34644, #30215, #35213, #43527, #3372, #3087 ) ),
 .UNSPECIFIED., .F., .F., .F.,
 ( 4, 4 ),
 ( 4, 1, 1, 1, 1, 1, 1, 1, 1, 1, 1, 1, 1, 1, 1, 1, 1, 1, 1, 1, 1, 1, 1, 1, 1, 1, 1, 1, 1, 1, 1, 1, 4 ),
 ( -0.1387574078320000237, 1.138757407831999968 ),
 ( 0.4756668553019000045, 0.4923735486379000048, 0.5090802419739000051, 0.5257869353097999188, 0.5424936286457999746, 0.5592003219817999193, 0.5759070153176999440, 0.5926137086536999998, 0.6093204019896999446, 0.6260270953255999693, 0.6427337886616000251, 0.6594404819975999699, 0.6761471753334999946, 0.6928538686695000504, 0.7095605620054999951, 0.7262672553414000198, 0.7429739486774000756, 0.7596806420133999094, 0.7763873353493999652, 0.7930940286852999899, 0.8098007220212999346, 0.8265074153572999904, 0.8432141086932000151, 0.8599208020291999599, 0.8766274953652000157, 0.8933341887010999294, 0.9100408820370999852, 0.9267475753731000410, 0.9434542687089999546, 0.9601609620450000104, 0.9768676553809999552, 0.9935743487168999799, 1.010281042052999956 ),
 .UNSPECIFIED. ) ;
#44628 = CARTESIAN_POINT ( 'NONE',  ( -1.394284273676999808, -77.94253568003099986, -12.20048157021999913 ) ) ;
#44629 = ADVANCED_FACE ( 'NONE', ( #23580 ), #25094, .F. ) ;
#44630 = CARTESIAN_POINT ( 'NONE',  ( -1.500000000000000000, -75.67500000000001137, 0.000000000000000000 ) ) ;
#44631 = CARTESIAN_POINT ( 'NONE',  ( -12.72966770609339804, -60.56881200329789294, -1.931346186347923766 ) ) ;
#44632 = AXIS2_PLACEMENT_3D ( 'NONE', #40368, #49532, #19399 ) ;
#44633 = EDGE_CURVE ( 'NONE', #38125, #40983, #14765, .T. ) ;
#44634 = FACE_OUTER_BOUND ( 'NONE', #40336, .T. ) ;
#44635 = EDGE_LOOP ( 'NONE', ( #27842, #1098, #36394, #28368, #53049, #48327, #52176 ) ) ;
#44636 = EDGE_LOOP ( 'NONE', ( #21534, #35765, #35585, #7963 ) ) ;
#44637 = CARTESIAN_POINT ( 'NONE',  ( 4.000000000000000000, -77.29999999999999716, 0.000000000000000000 ) ) ;
#44638 = ORIENTED_EDGE ( 'NONE', *, *, #16691, .F. ) ;
#44639 = CARTESIAN_POINT ( 'NONE',  ( -0.4256071464968388396, -79.62857731458335309, 9.520305438052526270 ) ) ;
#44640 = ORIENTED_EDGE ( 'NONE', *, *, #16504, .F. ) ;
#44641 = DIRECTION ( 'NONE',  ( 0.7071067812863980340, -6.386274622742979319E-09, -0.7071067810866970005 ) ) ;
#44642 = AXIS2_PLACEMENT_3D ( 'NONE', #28626, #23622, #28041 ) ;
#44643 = CARTESIAN_POINT ( 'NONE',  ( 10.58169901997000117, -77.91394768316000352, 3.119195446298999919 ) ) ;
#44644 = CARTESIAN_POINT ( 'NONE',  ( -1.218569463821508547, -82.57982710409879701, 0.3278157668757434862 ) ) ;
#44645 = CARTESIAN_POINT ( 'NONE',  ( -5.372582819375519847, -78.17569175854035279, -7.531333529607578292 ) ) ;
#44646 = CARTESIAN_POINT ( 'NONE',  ( -10.75729140709000120, -78.72117536965599527, -3.177859684493999914 ) ) ;
#44647 = CARTESIAN_POINT ( 'NONE',  ( 1.086236247072508654, -79.39183646607358469, 0.6189023910738301604 ) ) ;
#44648 = ORIENTED_EDGE ( 'NONE', *, *, #27677, .T. ) ;
#44649 = ORIENTED_EDGE ( 'NONE', *, *, #23773, .T. ) ;
#44650 = CARTESIAN_POINT ( 'NONE',  ( -1.624220529728441997, -77.48908808038281393, 9.106525592228415178 ) ) ;
#44651 = CARTESIAN_POINT ( 'NONE',  ( -10.84202097104999929, -77.35475100115499458, 2.082001701158999740 ) ) ;
#44652 = FACE_OUTER_BOUND ( 'NONE', #57929, .T. ) ;
#44653 = EDGE_CURVE ( 'NONE', #18080, #6792, #47570, .T. ) ;
#44654 = CARTESIAN_POINT ( 'NONE',  ( 7.624341766647000362, -18.73514853758999976, -10.42531125024999916 ) ) ;
#44655 = CARTESIAN_POINT ( 'NONE',  ( -9.157500079073999544, -78.86361672676999035, 3.211059275314999795 ) ) ;
#44656 = CARTESIAN_POINT ( 'NONE',  ( 5.890705889994000799, -75.57722202328000094, 10.05943228418000146 ) ) ;
#44657 = CARTESIAN_POINT ( 'NONE',  ( -9.392562919573798297, -79.41163292977475407, -1.424155904483036084 ) ) ;
#44658 = FACE_OUTER_BOUND ( 'NONE', #12438, .T. ) ;
#44659 = DIRECTION ( 'NONE',  ( -1.000000000000000000, 0.000000000000000000, 0.000000000000000000 ) ) ;
#44660 = PLANE ( 'NONE',  #50493 ) ;
#44661 = CARTESIAN_POINT ( 'NONE',  ( -10.53494356938999843, -23.22715052988000295, -7.618393677165000710 ) ) ;
#44662 = CARTESIAN_POINT ( 'NONE',  ( -9.253333465380869427, -79.27966831068214049, 2.487796638288232831 ) ) ;
#44663 = VERTEX_POINT ( 'NONE', #38011 ) ;
#44664 = CARTESIAN_POINT ( 'NONE',  ( -8.484929685468999949, -79.30817849819099763, 9.088234785002999416 ) ) ;
#44665 = DIRECTION ( 'NONE',  ( 0.000000000000000000, 1.000000000000000000, 0.000000000000000000 ) ) ;
#44666 = CARTESIAN_POINT ( 'NONE',  ( -3.610176697326359374, -78.00228815355546885, 10.14026356443288712 ) ) ;
#44667 = CARTESIAN_POINT ( 'NONE',  ( 7.851705946354000432, -77.38355886654599658, -9.048036745432998629 ) ) ;
#44668 = CARTESIAN_POINT ( 'NONE',  ( -8.292781013307999771, -16.94469293076999961, -9.770415148734000965 ) ) ;
#44670 = CARTESIAN_POINT ( 'NONE',  ( -1.930638663166000191, -18.77877936711000117, -12.72375916873000001 ) ) ;
#44669 = CARTESIAN_POINT ( 'NONE',  ( -1.532229595825244761, -60.92298962908660087, -12.51228690890456541 ) ) ;
#44671 = CARTESIAN_POINT ( 'NONE',  ( 0.04193593712240011040, -53.78990258635192134, 12.50649570002414279 ) ) ;
#44672 = CARTESIAN_POINT ( 'NONE',  ( 6.169139874394665490, -80.92666250314678678, 8.803678268947257024 ) ) ;
#44673 = CARTESIAN_POINT ( 'NONE',  ( 10.21381326472999795, -56.02870851050000311, -7.668949790007999923 ) ) ;
#44674 = DIRECTION ( 'NONE',  ( 0.7071067811865475727, 0.000000000000000000, -0.7071067811865475727 ) ) ;
#44675 = CARTESIAN_POINT ( 'NONE',  ( -3.257558841711999609, -76.92505786966898995, -10.78064358917000121 ) ) ;
#44676 = CARTESIAN_POINT ( 'NONE',  ( -12.76303204513999923, -55.53514852210999919, 1.980584515753000208 ) ) ;
#44677 = CARTESIAN_POINT ( 'NONE',  ( 8.294030550005999203, -80.13080510418970448, 7.292873907683000034 ) ) ;
#44678 = ORIENTED_EDGE ( 'NONE', *, *, #26975, .T. ) ;
#44679 = DIRECTION ( 'NONE',  ( -1.000000000000000000, 0.000000000000000000, 0.000000000000000000 ) ) ;
#44680 = AXIS2_PLACEMENT_3D ( 'NONE', #92, #57914, #36060 ) ;
#44681 = CARTESIAN_POINT ( 'NONE',  ( 1.582498447120999963, -54.64913877488999816, 12.55493832969000145 ) ) ;
#44682 = CARTESIAN_POINT ( 'NONE',  ( -12.49168451098999988, -23.29848884437999956, 1.667916687331000070 ) ) ;
#44683 = B_SPLINE_CURVE_WITH_KNOTS ( 'NONE', 3,
 ( #15179, #6616, #29048, #33172 ),
 .UNSPECIFIED., .F., .F.,
 ( 4, 4 ),
 ( 0.000000000000000000, 0.2500000082780876598 ),
 .UNSPECIFIED. ) ;
#44684 = CARTESIAN_POINT ( 'NONE',  ( -0.07105210834495999384, -3.682034174984999630, 3.964982828070999332 ) ) ;
#44685 = CARTESIAN_POINT ( 'NONE',  ( -8.446673021817000304, -79.98423817768198774, 4.180901655042999820 ) ) ;
#44686 = CARTESIAN_POINT ( 'NONE',  ( 2.839805762151339952, -1.708333333333332815, -1.636761686205418176 ) ) ;
#44687 = CARTESIAN_POINT ( 'NONE',  ( 7.164578282910722962, -77.28124999999998579, -8.391376934739398052 ) ) ;
#44688 = CARTESIAN_POINT ( 'NONE',  ( -1.798368564622000010, -59.99636757014000210, 12.61278090843000044 ) ) ;
#44689 = CARTESIAN_POINT ( 'NONE',  ( 3.677265727246999738, -85.38874735065199673, -1.976693371404000255 ) ) ;
#44690 = DIRECTION ( 'NONE',  ( 0.000000000000000000, 1.000000000000000000, 0.000000000000000000 ) ) ;
#44691 = EDGE_CURVE ( 'NONE', #4024, #47903, #8236, .T. ) ;
#44692 = CARTESIAN_POINT ( 'NONE',  ( -10.34725804423785256, -76.90989821929815662, 6.236182828636385622 ) ) ;
#44693 = CARTESIAN_POINT ( 'NONE',  ( -3.600020634850999546, -78.65560489188999327, 11.08749048210999888 ) ) ;
#44694 = CARTESIAN_POINT ( 'NONE',  ( 9.087383623426001478, -77.40971154453498571, -6.455544860934000262 ) ) ;
#44695 = CARTESIAN_POINT ( 'NONE',  ( 0.03753981069206074189, -81.97327235835214765, 1.249602265122939704 ) ) ;
#44696 = CARTESIAN_POINT ( 'NONE',  ( 0.1360381241691999976, -78.76134433024999737, 1.543111746742000134 ) ) ;
#44697 = CARTESIAN_POINT ( 'NONE',  ( 1.980584515756000030, -60.06485150062000145, 12.76303204342999997 ) ) ;
#44698 = CARTESIAN_POINT ( 'NONE',  ( -1.250000000000000000, -55.35321828636000419, -12.50000000000000000 ) ) ;
#44699 = CARTESIAN_POINT ( 'NONE',  ( -12.66235429711000116, -61.93741783389999966, 0.4955846680318000130 ) ) ;
#44700 = CARTESIAN_POINT ( 'NONE',  ( 0.3418130752321197896, -80.22786251027696380, -10.74510901840848121 ) ) ;
#44701 = CARTESIAN_POINT ( 'NONE',  ( -10.47020627418439354, -77.02083333333335702, -2.813789756862263847 ) ) ;
#44702 = CARTESIAN_POINT ( 'NONE',  ( -8.286887192105083955, -78.79105741471079227, 7.559703011935064332 ) ) ;
#44703 = ORIENTED_EDGE ( 'NONE', *, *, #53175, .T. ) ;
#44704 = CARTESIAN_POINT ( 'NONE',  ( 0.8896540882221496416, -81.78862763931634561, -0.8776062606573753477 ) ) ;
#44705 = CARTESIAN_POINT ( 'NONE',  ( 0.3664097495389522785, -61.77190017435451352, 12.50575740046243922 ) ) ;
#44706 = ADVANCED_FACE ( 'NONE', ( #14990 ), #51034, .F. ) ;
#44707 = CARTESIAN_POINT ( 'NONE',  ( 2.325232682335999890, -78.46495880092599862, -11.01938817673000059 ) ) ;
#44708 = VECTOR ( 'NONE', #21415, 1000.000000000000000 ) ;
#44709 = CARTESIAN_POINT ( 'NONE',  ( 7.555116226634262411, -55.11315380192718294, 7.995796640817951939 ) ) ;
#44710 = VERTEX_POINT ( 'NONE', #6431 ) ;
#44711 = EDGE_LOOP ( 'NONE', ( #28204, #43790, #37300, #11082, #29878, #15682 ) ) ;
#44712 = CARTESIAN_POINT ( 'NONE',  ( 1.025649293883999835, -80.81217187929600243, 1.247099486493999931 ) ) ;
#44713 = ORIENTED_EDGE ( 'NONE', *, *, #31074, .T. ) ;
#44714 = CARTESIAN_POINT ( 'NONE',  ( 12.50000000000000000, -60.04999999966999980, 0.000000000000000000 ) ) ;
#44715 = VERTEX_POINT ( 'NONE', #5551 ) ;
#44716 = LINE ( 'NONE', #32279, #45194 ) ;
#44717 = DIRECTION ( 'NONE',  ( -1.000000000000000000, 0.000000000000000000, 0.000000000000000000 ) ) ;
#44718 = CARTESIAN_POINT ( 'NONE',  ( 9.953654131039998632, -79.42661227141499580, 4.756732473150000473 ) ) ;
#44719 = CARTESIAN_POINT ( 'NONE',  ( 0.9887300587124998597, -24.93410057768999977, -12.65963207090000076 ) ) ;
#44720 = CIRCLE ( 'NONE', #23011, 13.94827586206999825 ) ;
#44721 = CARTESIAN_POINT ( 'NONE',  ( 1.861913176741999854, -80.01295594358298047, 3.498466738908999840 ) ) ;
#44722 = CARTESIAN_POINT ( 'NONE',  ( -3.386084928587058229, -79.30373914007272163, 8.876438725661222051 ) ) ;
#44723 = ORIENTED_EDGE ( 'NONE', *, *, #7321, .F. ) ;
#44724 = CARTESIAN_POINT ( 'NONE',  ( 10.94195044575999987, -77.58938080696006523, -1.468969119710000104 ) ) ;
#44725 = CARTESIAN_POINT ( 'NONE',  ( 8.402029934263000044, -78.60393122293001511, -8.859658380982999404 ) ) ;
#44726 = ORIENTED_EDGE ( 'NONE', *, *, #41744, .F. ) ;
#44727 = ORIENTED_EDGE ( 'NONE', *, *, #44884, .F. ) ;
#44728 = FACE_OUTER_BOUND ( 'NONE', #23939, .T. ) ;
#44729 = VECTOR ( 'NONE', #27277, 1000.000000000000000 ) ;
#44730 = ADVANCED_FACE ( 'NONE', ( #46613 ), #23561, .F. ) ;
#44731 = CARTESIAN_POINT ( 'NONE',  ( 0.5765222740522000233, -80.06131301898899721, 1.202579817323000233 ) ) ;
#44732 = CARTESIAN_POINT ( 'NONE',  ( 9.703485699160999900, -77.46048329721199366, 0.1143444355825999903 ) ) ;
#44733 = CARTESIAN_POINT ( 'NONE',  ( -3.773359617072352457, -86.25171438276197478, -2.633509696780396592 ) ) ;
#44734 = CARTESIAN_POINT ( 'NONE',  ( 3.047513760736739741, -85.83947020242759152, 1.827440418503480490 ) ) ;
#44735 = CARTESIAN_POINT ( 'NONE',  ( -2.472194872447494696, -79.05729166668488972, 11.61165635167936472 ) ) ;
#44736 = CARTESIAN_POINT ( 'NONE',  ( -0.4406873220133000202, -81.17553171121998901, -1.134095991600000186 ) ) ;
#44737 = B_SPLINE_CURVE_WITH_KNOTS ( 'NONE', 3,
 ( #56097, #51680, #51383, #55805, #46964, #1794, #29207, #10940, #28330, #42518, #47254, #33921, #51961, #2370, #37198, #46675, #5904, #29495 ),
 .UNSPECIFIED., .F., .F.,
 ( 4, 2, 2, 2, 2, 2, 2, 2, 4 ),
 ( 0.000000000000000000, 0.1250000000000001665, 0.2500000000000002776, 0.3750000000000002776, 0.5000000000000002220, 0.6250000000000001110, 0.7500000000000001110, 0.8750000000000000000, 1.000000000000000000 ),
 .UNSPECIFIED. ) ;
#44738 = CARTESIAN_POINT ( 'NONE',  ( -9.910042757802999702, -76.49457567883000308, -4.772096900591000335 ) ) ;
#44739 = CARTESIAN_POINT ( 'NONE',  ( -1.989514602459929504, -76.94999999999998863, -9.342458649981287166 ) ) ;
#44740 = CARTESIAN_POINT ( 'NONE',  ( -3.770453462111999610, -78.81431117999389357, 1.207889202028999964 ) ) ;
#44741 = CARTESIAN_POINT ( 'NONE',  ( 0.000000000000000000, -75.15999999999999659, 0.000000000000000000 ) ) ;
#44742 = CARTESIAN_POINT ( 'NONE',  ( -1.842154520908950044, -76.81205411479356826, -11.67446096355657126 ) ) ;
#44743 = CARTESIAN_POINT ( 'NONE',  ( -2.501232889508999691, -81.45550264934799145, 2.511732025391000267 ) ) ;
#44744 = DIRECTION ( 'NONE',  ( 0.000000000000000000, 0.000000000000000000, -1.000000000000000000 ) ) ;
#44745 = CARTESIAN_POINT ( 'NONE',  ( 5.365883907697000410, -80.16938766345090528, 9.905345355165000143 ) ) ;
#44746 = CARTESIAN_POINT ( 'NONE',  ( -0.3113020967593000399, -2.629516015700000153, 3.793306396812999637 ) ) ;
#44747 = CARTESIAN_POINT ( 'NONE',  ( -0.7342790699846932778, -79.67427446810803815, 1.041378959097729817 ) ) ;
#44748 = ORIENTED_EDGE ( 'NONE', *, *, #37486, .F. ) ;
#44749 = CARTESIAN_POINT ( 'NONE',  ( -10.75000000000000000, -80.01041666666668561, -1.407171709420427019 ) ) ;
#44750 = CARTESIAN_POINT ( 'NONE',  ( -10.71369944335148183, -79.17916666666667425, 2.879226727952048481 ) ) ;
#44751 = TOROIDAL_SURFACE ( 'NONE', #20272, 1.250000000000000000, 0.5000000000000000000 ) ;
#44752 = CARTESIAN_POINT ( 'NONE',  ( 0.7341740840635999632, -80.84950453195499165, -1.113348630318000021 ) ) ;
#44753 = CARTESIAN_POINT ( 'NONE',  ( -4.418379168946118263, -78.98666666666667879, -8.447563838020446525 ) ) ;
#44754 = CARTESIAN_POINT ( 'NONE',  ( 7.287838312904000304, -78.15497037702999705, -10.78085041437000058 ) ) ;
#44755 = CARTESIAN_POINT ( 'NONE',  ( 9.613649280381000750, -79.26138667140099869, 0.5442168635241999564 ) ) ;
#44756 = CARTESIAN_POINT ( 'NONE',  ( -10.12561891750000065, -76.54434732925000162, -7.350590001713999122 ) ) ;
#44757 = VERTEX_POINT ( 'NONE', #42166 ) ;
#44758 = EDGE_CURVE ( 'NONE', #3325, #42463, #28697, .T. ) ;
#44759 = AXIS2_PLACEMENT_3D ( 'NONE', #7535, #3117, #21108 ) ;
#44760 = CARTESIAN_POINT ( 'NONE',  ( 8.414570695956999913, -59.94999999967000548, 8.414570695956999913 ) ) ;
#44761 = CARTESIAN_POINT ( 'NONE',  ( 4.490468926300999364, -77.02113108638108940, 10.16576052825000076 ) ) ;
#44762 = ADVANCED_FACE ( 'NONE', ( #55745 ), #10813, .T. ) ;
#44763 = CARTESIAN_POINT ( 'NONE',  ( -0.9429895430810999457, -80.92385680317599395, -1.174528710654999974 ) ) ;
#44764 = CARTESIAN_POINT ( 'NONE',  ( 12.00000000000000711, -79.13958333333332007, -1.570796326794872355 ) ) ;
#44765 = CARTESIAN_POINT ( 'NONE',  ( 1.236990682704000033, -77.82157087262599759, 9.441410396910001168 ) ) ;
#44767 = CARTESIAN_POINT ( 'NONE',  ( -3.161392481395000065, -1.887292672027000018, -1.501864700490999960 ) ) ;
#44766 = CARTESIAN_POINT ( 'NONE',  ( 0.2051906278595000133, -85.75676443653598824, 4.169824694008999799 ) ) ;
#44768 = CARTESIAN_POINT ( 'NONE',  ( -1.667917367010000040, -55.51943307300000185, -12.49306752631999906 ) ) ;
#44769 = CARTESIAN_POINT ( 'NONE',  ( -0.6885369103866999518, -80.13480328324099844, -1.350873448928000098 ) ) ;
#44770 = ORIENTED_EDGE ( 'NONE', *, *, #43127, .F. ) ;
#44771 = CARTESIAN_POINT ( 'NONE',  ( -1.301360059616015308, -77.21547344162672744, -10.68678654117428195 ) ) ;
#44772 = DIRECTION ( 'NONE',  ( 1.000000000000000000, 0.000000000000000000, 0.000000000000000000 ) ) ;
#44773 = CARTESIAN_POINT ( 'NONE',  ( 3.548349909811000291, -78.96264282632948550, -4.345475359304840494E-16 ) ) ;
#44774 = ORIENTED_EDGE ( 'NONE', *, *, #13626, .T. ) ;
#44775 = ORIENTED_EDGE ( 'NONE', *, *, #17197, .F. ) ;
#44776 = CARTESIAN_POINT ( 'NONE',  ( 0.000000000000000000, -76.75499999999999545, 0.000000000000000000 ) ) ;
#44777 = EDGE_CURVE ( 'NONE', #20674, #57578, #48339, .T. ) ;
#44778 = DIRECTION ( 'NONE',  ( 0.9998748951565024079, 0.000000000000000000, 0.01581752306063006000 ) ) ;
#44779 = ORIENTED_EDGE ( 'NONE', *, *, #3191, .T. ) ;
#44780 = CARTESIAN_POINT ( 'NONE',  ( 10.53043183326000154, -77.48152976611999065, 5.857113494126000575 ) ) ;
#44781 = VERTEX_POINT ( 'NONE', #3173 ) ;
#44782 = VERTEX_POINT ( 'NONE', #21456 ) ;
#44783 = CARTESIAN_POINT ( 'NONE',  ( -2.288966405475738597, -2.663704043780092956, -2.306431892470109712 ) ) ;
#44784 = CARTESIAN_POINT ( 'NONE',  ( 11.79999999999999893, -23.15000000000000213, 0.000000000000000000 ) ) ;
#44785 = CYLINDRICAL_SURFACE ( 'NONE', #17620, 0.5000000000000004441 ) ;
#44786 = AXIS2_PLACEMENT_3D ( 'NONE', #37930, #15206, #27896 ) ;
#44787 = ORIENTED_EDGE ( 'NONE', *, *, #30881, .T. ) ;
#44788 = DIRECTION ( 'NONE',  ( -0.7071067811865475727, 0.000000000000000000, -0.7071067811865475727 ) ) ;
#44789 = ORIENTED_EDGE ( 'NONE', *, *, #35835, .T. ) ;
#44790 = CARTESIAN_POINT ( 'NONE',  ( 0.4801485855953882553, -80.30554746943639088, -1.179926170174790512 ) ) ;
#44791 = VECTOR ( 'NONE', #16293, 1000.000000000000000 ) ;
#44792 = CARTESIAN_POINT ( 'NONE',  ( -11.67929340176440078, -79.80000000000001137, -2.658825183345205456 ) ) ;
#44793 = LINE ( 'NONE', #17931, #49098 ) ;
#44794 = CARTESIAN_POINT ( 'NONE',  ( -7.626500777234999973, -23.31584731985000047, -10.35747145892000098 ) ) ;
#44795 = CARTESIAN_POINT ( 'NONE',  ( 5.891554620702148526, -77.36431389369244016, -10.19904068193172719 ) ) ;
#44796 = CARTESIAN_POINT ( 'NONE',  ( -12.50000000000000000, -18.75000000000000000, 0.000000000000000000 ) ) ;
#44797 = CARTESIAN_POINT ( 'NONE',  ( 7.678667886061999681, -57.04263462147999775, -10.59548767699999949 ) ) ;
#44798 = CARTESIAN_POINT ( 'NONE',  ( -2.858407197967999913, -79.99999999999998579, 8.797272775729998884 ) ) ;
#44799 = CARTESIAN_POINT ( 'NONE',  ( -9.108250977391000092, -24.87811334491999915, 8.478720681740998799 ) ) ;
#44800 = LINE ( 'NONE', #4352, #43284 ) ;
#44801 = CARTESIAN_POINT ( 'NONE',  ( -10.15788409568143713, -76.92166188270672933, 3.765279467776149858 ) ) ;
#44802 = CARTESIAN_POINT ( 'NONE',  ( 7.396646590749633710, -77.79807357050631822, -5.684287846210173356 ) ) ;
#44803 = CARTESIAN_POINT ( 'NONE',  ( 2.777255051931000196, -81.09475264934799554, 3.117122737064000226 ) ) ;
#44804 = ADVANCED_FACE ( 'NONE', ( #7592 ), #53187, .F. ) ;
#44805 = CARTESIAN_POINT ( 'NONE',  ( -9.511284522137000152, -77.79906001420199857, 2.647011044820000158 ) ) ;
#44806 = CARTESIAN_POINT ( 'NONE',  ( -12.54981748964999966, -16.95163512371999914, -0.03767836620435000006 ) ) ;
#44807 = DIRECTION ( 'NONE',  ( -0.7272727272724163194, -0.6863485850246158204, -6.703676215667153735E-07 ) ) ;
#44808 = CARTESIAN_POINT ( 'NONE',  ( -1.930009203935999951, -23.20099032317000365, 12.72537718777000038 ) ) ;
#44809 = CARTESIAN_POINT ( 'NONE',  ( -7.919595949288999570, -55.64999999964999233, 9.050966799188000067 ) ) ;
#44810 = CARTESIAN_POINT ( 'NONE',  ( -3.302484149747999975, -84.62957809581099866, 1.295437536289999914 ) ) ;
#44811 = CARTESIAN_POINT ( 'NONE',  ( -3.236421654187000119, -2.018566864578999809, 1.624998546076000139 ) ) ;
#44812 = CARTESIAN_POINT ( 'NONE',  ( -10.27011860311526092, -78.12477168548677753, -3.283755321494949087 ) ) ;
#44813 = CARTESIAN_POINT ( 'NONE',  ( -0.6609564419650209022, -79.93834960266842415, -1.360574577815365949 ) ) ;
#44814 = CARTESIAN_POINT ( 'NONE',  ( 12.66736977985000046, -61.03307288738999858, -1.690635117038999935 ) ) ;
#44815 = CARTESIAN_POINT ( 'NONE',  ( -0.2137776359178999996, -78.52249079038800517, -1.600472757759999753 ) ) ;
#44816 = CARTESIAN_POINT ( 'NONE',  ( 7.601397897754999633, -18.75000000000000000, 9.369164850722000892 ) ) ;
#44817 = CARTESIAN_POINT ( 'NONE',  ( -2.247674004742000076, -77.91809300996099807, 10.68285203299000052 ) ) ;
#44818 = CARTESIAN_POINT ( 'NONE',  ( 3.330893700617000075, -78.52026847289599232, -11.81951464247000061 ) ) ;
#44819 = DIRECTION ( 'NONE',  ( 0.000000000000000000, 0.000000000000000000, -1.000000000000000000 ) ) ;
#44820 = CARTESIAN_POINT ( 'NONE',  ( -2.813789756862251856, -79.10416666666665719, -10.47020627418439709 ) ) ;
#44822 = CARTESIAN_POINT ( 'NONE',  ( -1.472799192485999997, -77.87176762208750347, -0.3599880333205999761 ) ) ;
#44821 = DIRECTION ( 'NONE',  ( 0.000000000000000000, 1.000000000000000000, 2.031724556816999953E-13 ) ) ;
#44823 = CARTESIAN_POINT ( 'NONE',  ( -0.4591954515747000420, -81.66670264959000747, 1.639803156192000122 ) ) ;
#44824 = ORIENTED_EDGE ( 'NONE', *, *, #27994, .T. ) ;
#44825 = CARTESIAN_POINT ( 'NONE',  ( 1.160825211897999809, -84.55471544543098616, 3.572652644192999993 ) ) ;
#44826 = CARTESIAN_POINT ( 'NONE',  ( -12.56594317989000054, -23.24999999414999863, -1.750000000001000089 ) ) ;
#44827 = TOROIDAL_SURFACE ( 'NONE', #1486, 17.50000000000000000, 5.000000000000000000 ) ;
#44828 = CARTESIAN_POINT ( 'NONE',  ( 3.734633266582000122, -80.29325902863899955, -10.52978014402000007 ) ) ;
#44829 = ADVANCED_FACE ( 'NONE', ( #34147 ), #26171, .T. ) ;
#44830 = CARTESIAN_POINT ( 'NONE',  ( 0.000000000000000000, -75.15999999999999659, 0.000000000000000000 ) ) ;
#44831 = CARTESIAN_POINT ( 'NONE',  ( 0.5288065283753385915, -84.28854167802401776, 3.403152181769989681 ) ) ;
#44832 = CARTESIAN_POINT ( 'NONE',  ( -10.36292431360000066, -60.00096201600999990, 7.633479737330000070 ) ) ;
#44833 = DIRECTION ( 'NONE',  ( 0.000000000000000000, 1.000000000000000000, 0.000000000000000000 ) ) ;
#44834 = DIRECTION ( 'NONE',  ( -0.7071067811864980568, 0.7071067811865969777, 4.151099656137985125E-09 ) ) ;
#44835 = CARTESIAN_POINT ( 'NONE',  ( 0.000000000000000000, -80.59999999999999432, -9.199999999999974420 ) ) ;
#44836 = CARTESIAN_POINT ( 'NONE',  ( -10.42531124903999995, -55.53514851492000304, 7.624341765436000173 ) ) ;
#44837 = CARTESIAN_POINT ( 'NONE',  ( -1.667916687244999974, -60.09849137196000157, 12.49168433582000226 ) ) ;
#44838 = EDGE_LOOP ( 'NONE', ( #53747, #27778, #22088, #34604 ) ) ;
#44839 = CARTESIAN_POINT ( 'NONE',  ( -12.70299804974076530, -53.77411689953881790, 0.8844418155833001505 ) ) ;
#44840 = DIRECTION ( 'NONE',  ( 0.000000000000000000, -1.000000000000000000, 0.000000000000000000 ) ) ;
#44841 = CARTESIAN_POINT ( 'NONE',  ( -1.310679582531386389, -81.44166666666667709, -0.7554284705563492075 ) ) ;
#44842 = CARTESIAN_POINT ( 'NONE',  ( 2.952109282631000031, -82.30717953870899350, -1.687953082055999809 ) ) ;
#44843 = CARTESIAN_POINT ( 'NONE',  ( -12.49168451095999899, -55.50151115525000023, -1.667916687331000070 ) ) ;
#44844 = EDGE_CURVE ( 'NONE', #57837, #1524, #3736, .T. ) ;
#44845 = ORIENTED_EDGE ( 'NONE', *, *, #31831, .T. ) ;
#44846 = CARTESIAN_POINT ( 'NONE',  ( -6.031270819540000439, -77.00661118349269429, -8.856729339061999440 ) ) ;
#44847 = CARTESIAN_POINT ( 'NONE',  ( -1.537993320270047315, -77.81278135628818404, -11.67747152160435142 ) ) ;
#44848 = CARTESIAN_POINT ( 'NONE',  ( -2.062670899361999766, -23.30639784948999704, 12.83044027760000105 ) ) ;
#44849 = EDGE_CURVE ( 'NONE', #45077, #9760, #44720, .T. ) ;
#44850 = VERTEX_POINT ( 'NONE', #39463 ) ;
#44851 = ORIENTED_EDGE ( 'NONE', *, *, #4905, .T. ) ;
#44852 = CARTESIAN_POINT ( 'NONE',  ( -7.620037552694999938, -55.59433113521999559, -10.53559761426999764 ) ) ;
#44853 = SURFACE_STYLE_FILL_AREA ( #13248 ) ;
#44854 = CARTESIAN_POINT ( 'NONE',  ( -2.116314338179000387, -79.87746842018698601, -9.535298106756000536 ) ) ;
#44855 = VERTEX_POINT ( 'NONE', #15876 ) ;
#44856 = ORIENTED_EDGE ( 'NONE', *, *, #19298, .F. ) ;
#44857 = CARTESIAN_POINT ( 'NONE',  ( 7.117776695569999923, -76.44899937808600043, 9.951095779506998085 ) ) ;
#44858 = FACE_OUTER_BOUND ( 'NONE', #15755, .T. ) ;
#44859 = CARTESIAN_POINT ( 'NONE',  ( -1.301250031112000105, -78.25114003055999490, -0.8139582694945000085 ) ) ;
#44860 = VERTEX_POINT ( 'NONE', #2599 ) ;
#44861 = CARTESIAN_POINT ( 'NONE',  ( 0.000000000000000000, -63.73717104351998586, 0.000000000000000000 ) ) ;
#44862 = EDGE_CURVE ( 'NONE', #37723, #8940, #11457, .T. ) ;
#44863 = CARTESIAN_POINT ( 'NONE',  ( 1.203234187881469852, -80.32853980534089544, -0.3383792636773915730 ) ) ;
#44864 = CARTESIAN_POINT ( 'NONE',  ( 12.64769468388000107, -77.22310353941999495, -3.464320626314000062 ) ) ;
#44865 = CARTESIAN_POINT ( 'NONE',  ( -11.21668965365999959, -77.75044816951745474, -0.06311738993059996805 ) ) ;
#44866 = CARTESIAN_POINT ( 'NONE',  ( -6.354078923955547964, -78.36956649114314644, 10.19482050615332369 ) ) ;
#44867 = CARTESIAN_POINT ( 'NONE',  ( 3.200957065930781997, -86.17851879815599148, 2.324951338795794520 ) ) ;
#44868 = CARTESIAN_POINT ( 'NONE',  ( 10.05828973332000054, -79.11519543049799097, -4.964767691657000270 ) ) ;
#44869 = CONICAL_SURFACE ( 'NONE', #39205, 2.699999999213000379, 0.7853981633972997312 ) ;
#44870 = CARTESIAN_POINT ( 'NONE',  ( 5.368767637727030362, -79.92621298444481681, 7.532222042164998577 ) ) ;
#44871 = CARTESIAN_POINT ( 'NONE',  ( 7.624341764923000753, -18.73514850530999709, 10.42531124853000080 ) ) ;
#44872 = ORIENTED_EDGE ( 'NONE', *, *, #2197, .F. ) ;
#44873 = CARTESIAN_POINT ( 'NONE',  ( -7.596835002782738933, -77.74791666666666856, 5.838193839761661508 ) ) ;
#44874 = B_SPLINE_CURVE_WITH_KNOTS ( 'NONE', 3,
 ( #39218, #21787, #21210, #44233, #53374, #3223, #57231, #2927 ),
 .UNSPECIFIED., .F., .F.,
 ( 4, 2, 2, 4 ),
 ( 0.000000000000000000, 0.4999999999999995559, 0.7499999999999997780, 1.000000000000000000 ),
 .UNSPECIFIED. ) ;
#44875 = CARTESIAN_POINT ( 'NONE',  ( 7.568503529865000523, -76.37430647614999657, 9.708412483427999007 ) ) ;
#44876 = CARTESIAN_POINT ( 'NONE',  ( 0.3219823053856999961, -80.04903304826798660, -1.582258297802999980 ) ) ;
#44877 = VECTOR ( 'NONE', #11937, 1000.000000000000000 ) ;
#44879 = EDGE_CURVE ( 'NONE', #14636, #7888, #25186, .T. ) ;
#44878 = CARTESIAN_POINT ( 'NONE',  ( -0.1746703279969999689, -78.27249079038830359, -1.307691051723000042 ) ) ;
#44880 = CARTESIAN_POINT ( 'NONE',  ( 3.432017302438363338, -3.081497486436961530, -0.7773794206622555159 ) ) ;
#44881 = CARTESIAN_POINT ( 'NONE',  ( 12.50745077485999879, -53.80005551680000053, -2.012158279073999839E-09 ) ) ;
#44882 = CARTESIAN_POINT ( 'NONE',  ( 5.459501886381000091, -76.36334185139999420, -11.00074850082999767 ) ) ;
#44883 = CARTESIAN_POINT ( 'NONE',  ( 0.000000000000000000, -76.29999999999999716, 0.000000000000000000 ) ) ;
#44884 = EDGE_CURVE ( 'NONE', #47498, #37882, #33510, .T. ) ;
#44885 = CARTESIAN_POINT ( 'NONE',  ( -7.445902463126000015, -77.49776332859899242, -6.104824477164000562 ) ) ;
#44886 = CARTESIAN_POINT ( 'NONE',  ( -10.11788549770072621, -77.09584413801610481, -6.579903885935526553 ) ) ;
#44887 = DIRECTION ( 'NONE',  ( 0.000000000000000000, -1.000000000000000000, 0.000000000000000000 ) ) ;
#44888 = DIRECTION ( 'NONE',  ( -0.7071067811865474617, 0.000000000000000000, -0.7071067811865474617 ) ) ;
#44889 = ORIENTED_EDGE ( 'NONE', *, *, #30211, .T. ) ;
#44890 = CARTESIAN_POINT ( 'NONE',  ( 0.3767945000176999848, -81.53743241160998423, -1.540381938526000027 ) ) ;
#44891 = CARTESIAN_POINT ( 'NONE',  ( 0.3870708775265000456, -80.66809355086999744, -1.294661097694999929 ) ) ;
#44892 = CARTESIAN_POINT ( 'NONE',  ( 7.674627477118999508, -59.55077028051999832, -10.14950121126999960 ) ) ;
#44893 = CARTESIAN_POINT ( 'NONE',  ( 11.97742283006000186, -77.74990883061599334, 0.2395971301470000148 ) ) ;
#44894 = CARTESIAN_POINT ( 'NONE',  ( 7.551616412536306555, -76.99999999999998579, 5.485893062531241426 ) ) ;
#44895 = CARTESIAN_POINT ( 'NONE',  ( -6.752419751440000617, -78.15373404223500131, -9.840748444448999876 ) ) ;
#44896 = CARTESIAN_POINT ( 'NONE',  ( -8.918806285220000518, -77.97724415034599588, 3.872830773119999570 ) ) ;
#44897 = CARTESIAN_POINT ( 'NONE',  ( 0.4356486348728999536, -53.91935044157000334, -12.43591427117000059 ) ) ;
#44898 = CARTESIAN_POINT ( 'NONE',  ( 5.240463812692992107, -76.03770333581218210, 10.52392510242733259 ) ) ;
#44899 = CARTESIAN_POINT ( 'NONE',  ( -1.448527388915000103, -78.57317658674999450, -10.72114852740000046 ) ) ;
#44900 = PLANE ( 'NONE',  #12487 ) ;
#44901 = EDGE_LOOP ( 'NONE', ( #7241, #33074, #46331, #46684 ) ) ;
#44902 = CARTESIAN_POINT ( 'NONE',  ( 9.250000000000000000, -78.74999999999998579, 0.000000000000000000 ) ) ;
#44903 = CARTESIAN_POINT ( 'NONE',  ( 7.331368884251999951, -75.87423312637412209, 9.888700222343000945 ) ) ;
#44904 = CARTESIAN_POINT ( 'NONE',  ( -3.406490272659984164, -78.62148120184446043, 0.06421901112149774882 ) ) ;
#44905 = CARTESIAN_POINT ( 'NONE',  ( -3.673218652927999539, -79.33230776043399146, 10.34270183798999909 ) ) ;
#44906 = CARTESIAN_POINT ( 'NONE',  ( 9.611650271896824194, -79.30833333333332291, -5.539808784079918169 ) ) ;
#44907 = CARTESIAN_POINT ( 'NONE',  ( -11.31898586865000134, -75.98564338555699749, 3.399843791672999771 ) ) ;
#44908 = CARTESIAN_POINT ( 'NONE',  ( 9.722718241315000398, -60.24678171298000251, -7.954951288349001004 ) ) ;
#44909 = CARTESIAN_POINT ( 'NONE',  ( 3.126548645920367520, -76.85163636138472043, 10.36074945036640393 ) ) ;
#44910 = ORIENTED_EDGE ( 'NONE', *, *, #35376, .T. ) ;
#44911 = CARTESIAN_POINT ( 'NONE',  ( 10.86346900787000003, -78.97684881879399654, 2.497927478100999910 ) ) ;
#44912 = CARTESIAN_POINT ( 'NONE',  ( 8.824074283052752321, -77.22496508380866942, -2.868679438668469750 ) ) ;
#44913 = CARTESIAN_POINT ( 'NONE',  ( 11.00000000000000000, -77.84999999999999432, 0.000000000000000000 ) ) ;
#44914 = CARTESIAN_POINT ( 'NONE',  ( 8.302863715705628422, -76.38741280764111252, -8.314095789455475227 ) ) ;
#44915 = ADVANCED_FACE ( 'NONE', ( #51547 ), #6655, .F. ) ;
#44916 = CARTESIAN_POINT ( 'NONE',  ( -10.74684349920000059, -79.72579375008199065, 2.363312785431999963 ) ) ;
#44917 = CARTESIAN_POINT ( 'NONE',  ( 1.500000000000000000, -78.25000000000000000, 0.000000000000000000 ) ) ;
#44918 = CARTESIAN_POINT ( 'NONE',  ( 11.00000000000000533, -23.75000000000000355, -0.1604995627819790494 ) ) ;
#44919 = EDGE_CURVE ( 'NONE', #44548, #2890, #55668, .T. ) ;
#44920 = CARTESIAN_POINT ( 'NONE',  ( 9.199999999999999289, -80.59999999999999432, 0.000000000000000000 ) ) ;
#44921 = FACE_OUTER_BOUND ( 'NONE', #25956, .T. ) ;
#44922 = AXIS2_PLACEMENT_3D ( 'NONE', #2290, #56301, #52169 ) ;
#44923 = CARTESIAN_POINT ( 'NONE',  ( 0.000000000000000000, -75.20000000000000284, 0.000000000000000000 ) ) ;
#44924 = AXIS2_PLACEMENT_3D ( 'NONE', #25729, #39022, #3307 ) ;
#44925 = CARTESIAN_POINT ( 'NONE',  ( 0.000000000000000000, -32.36102867817999851, 0.000000000000000000 ) ) ;
#44926 = DIRECTION ( 'NONE',  ( 0.7071067811865475727, 0.000000000000000000, 0.7071067811865475727 ) ) ;
#44927 = ORIENTED_EDGE ( 'NONE', *, *, #32322, .F. ) ;
#44928 = AXIS2_PLACEMENT_3D ( 'NONE', #40609, #40311, #45046 ) ;
#44929 = ORIENTED_EDGE ( 'NONE', *, *, #33347, .T. ) ;
#44930 = CARTESIAN_POINT ( 'NONE',  ( 0.000000000000000000, -74.64999999999999147, 0.000000000000000000 ) ) ;
#44931 = CARTESIAN_POINT ( 'NONE',  ( 7.965859911057998843, -77.42573998579798911, 5.254112810574000036 ) ) ;
#44932 = VERTEX_POINT ( 'NONE', #36775 ) ;
#44933 = CARTESIAN_POINT ( 'NONE',  ( -1.185608318420265928, -79.63492132814884883, 9.455258074239862864 ) ) ;
#44934 = ORIENTED_EDGE ( 'NONE', *, *, #34117, .F. ) ;
#44935 = CARTESIAN_POINT ( 'NONE',  ( 9.389195554418000356, -24.71043214204999927, 8.194863653270999748 ) ) ;
#44936 = CARTESIAN_POINT ( 'NONE',  ( -7.675142533464999417, -78.07736574117099337, 7.924261572595001191 ) ) ;
#44937 = EDGE_CURVE ( 'NONE', #42095, #53581, #9837, .T. ) ;
#44938 = CARTESIAN_POINT ( 'NONE',  ( 8.190859204290999784, -55.64999999967000122, -7.342331066867000544 ) ) ;
#44939 = CARTESIAN_POINT ( 'NONE',  ( -8.963686800021001488, -79.09838998579799352, 3.673354096997999640 ) ) ;
#44940 = EDGE_CURVE ( 'NONE', #30569, #35193, #32333, .T. ) ;
#44941 = CARTESIAN_POINT ( 'NONE',  ( -3.659791739852715331, -78.19279094063269042, -8.496079794231707893 ) ) ;
#44942 = CARTESIAN_POINT ( 'NONE',  ( 2.407803015296000382, -80.12354473002160660, 10.73324203768999929 ) ) ;
#44943 = CARTESIAN_POINT ( 'NONE',  ( 8.857589609082554105, -79.26910282387936491, -3.584429394132419677 ) ) ;
#44944 = ORIENTED_EDGE ( 'NONE', *, *, #3038, .T. ) ;
#44945 = VERTEX_POINT ( 'NONE', #19077 ) ;
#44946 = CARTESIAN_POINT ( 'NONE',  ( 1.369538937357239083, -77.46319207057830170, 9.148125136416654257 ) ) ;
#44947 = CARTESIAN_POINT ( 'NONE',  ( 10.77519778174000109, -77.23148241939499314, -1.228540277667999892 ) ) ;
#44948 =( LENGTH_UNIT ( ) NAMED_UNIT ( * ) SI_UNIT ( .MILLI., .METRE. ) );
#44949 = CARTESIAN_POINT ( 'NONE',  ( -9.669247687117000112, -77.89720653638498504, -0.8224101967608999919 ) ) ;
#44950 = CARTESIAN_POINT ( 'NONE',  ( 11.93795915497000060, -75.96753699673999449, -4.186706965401000069 ) ) ;
#44951 = CARTESIAN_POINT ( 'NONE',  ( -9.382670943801374008, -79.41215256169735426, -1.487056722518299345 ) ) ;
#44952 = DIRECTION ( 'NONE',  ( 0.000000000000000000, -1.000000000000000000, 0.000000000000000000 ) ) ;
#44953 = CARTESIAN_POINT ( 'NONE',  ( 2.562649862274036572, -79.44753403950033999, -9.184391689306689699 ) ) ;
#44954 = EDGE_CURVE ( 'NONE', #31323, #51555, #46247, .T. ) ;
#44955 = CARTESIAN_POINT ( 'NONE',  ( 12.54987159816999842, -16.94886760191999997, -0.1385534523823999942 ) ) ;
#44956 = CARTESIAN_POINT ( 'NONE',  ( 12.00000000000000000, -55.54999999966999980, 1.750000000000000000 ) ) ;
#44957 = CARTESIAN_POINT ( 'NONE',  ( 9.250000000000000000, -78.74999999999998579, 0.000000000000000000 ) ) ;
#44958 = CARTESIAN_POINT ( 'NONE',  ( -3.073513311004000048, -85.74904717229100015, 2.159747950585999998 ) ) ;
#44959 = EDGE_LOOP ( 'NONE', ( #18668, #29664, #26682, #13518, #1962, #16553, #18655, #51563, #32024, #57483, #17123 ) ) ;
#44960 = CARTESIAN_POINT ( 'NONE',  ( -5.166309513786999652, -79.78321311977300923, 11.02043503902999966 ) ) ;
#44961 = CARTESIAN_POINT ( 'NONE',  ( 8.910932162214999508, -76.00998311897500059, 6.639958018061999034 ) ) ;
#44962 = CARTESIAN_POINT ( 'NONE',  ( -7.208993631127555979, -78.03351433546752958, 7.975374487723845718 ) ) ;
#44963 = CARTESIAN_POINT ( 'NONE',  ( 7.919842512016999514, -77.51920544366500110, 8.988445846368000147 ) ) ;
#44964 = CARTESIAN_POINT ( 'NONE',  ( 3.250000000000000444, -3.260416666666665630, 0.4254240051736248862 ) ) ;
#44965 = CIRCLE ( 'NONE', #14774, 1.749999999999998446 ) ;
#44967 = CARTESIAN_POINT ( 'NONE',  ( 12.50000000000000000, -23.25000000000000000, 0.000000000000000000 ) ) ;
#44966 = CARTESIAN_POINT ( 'NONE',  ( 10.26699006316253637, -78.50833333333332575, -5.917523019358050362 ) ) ;
#44968 = CARTESIAN_POINT ( 'NONE',  ( 3.112536659742000111, -86.17851879815599148, -1.385790604991000041 ) ) ;
#44969 = CARTESIAN_POINT ( 'NONE',  ( 10.59548767697000038, -58.55736537918999574, -7.678667886039000301 ) ) ;
#44970 = CARTESIAN_POINT ( 'NONE',  ( -9.500000000000000000, -78.29999999999999716, 0.000000000000000000 ) ) ;
#44971 = CARTESIAN_POINT ( 'NONE',  ( 7.037082147462999870, -78.64021989260099588, -8.217099986793998667 ) ) ;
#44972 = CARTESIAN_POINT ( 'NONE',  ( -0.8506806241676722058, -1.895833333333333037, 3.165411199172021739 ) ) ;
#44973 = CARTESIAN_POINT ( 'NONE',  ( -3.110348726875999947, -80.42612965022969718, -10.81755274276999934 ) ) ;
#44974 = VECTOR ( 'NONE', #50782, 1000.000000000000000 ) ;
#44975 = CARTESIAN_POINT ( 'NONE',  ( -9.500000000000000000, -91.89999999999999147, 7.261899921535998111E-14 ) ) ;
#44976 = EDGE_CURVE ( 'NONE', #14764, #43451, #26783, .T. ) ;
#44977 = CARTESIAN_POINT ( 'NONE',  ( -1.382886570148999850, -54.16901780135000166, 12.65982054472000051 ) ) ;
#44978 = CARTESIAN_POINT ( 'NONE',  ( -1.798944584240000255, -60.01533228248000285, -12.61116916001999932 ) ) ;
#44979 = CARTESIAN_POINT ( 'NONE',  ( -1.897426238260999876, -3.722918480970999866, 3.187324685277999947 ) ) ;
#44980 = CARTESIAN_POINT ( 'NONE',  ( 11.19952915612999966, -77.94389204245099734, -0.6234238306063999424 ) ) ;
#44981 = CARTESIAN_POINT ( 'NONE',  ( 4.784380313523556083, -77.46666666666668277, -8.300970689365444244 ) ) ;
#44982 = CARTESIAN_POINT ( 'NONE',  ( -0.7999999997951999786, -23.14999999072999870, -11.99999999979999821 ) ) ;
#44983 = CARTESIAN_POINT ( 'NONE',  ( -1.890224871705999954, -60.54789247981999267, 12.68696160876999990 ) ) ;
#44984 = CARTESIAN_POINT ( 'NONE',  ( 12.43640296266999989, -17.08252466130999991, -0.05222744260230000046 ) ) ;
#44985 = CARTESIAN_POINT ( 'NONE',  ( -4.136841678191000682, -83.22424735065199286, 0.5622640331050000606 ) ) ;
#44986 = CARTESIAN_POINT ( 'NONE',  ( 0.000000000000000000, -6.100000000000000533, 0.000000000000000000 ) ) ;
#44987 = CARTESIAN_POINT ( 'NONE',  ( 12.06472673805143536, -76.70531092299836473, 0.3523124688570539731 ) ) ;
#44988 = FACE_OUTER_BOUND ( 'NONE', #49005, .T. ) ;
#44989 = CARTESIAN_POINT ( 'NONE',  ( 9.807952262865001103, -76.91945737050299670, -5.297043796141999827 ) ) ;
#44990 = CARTESIAN_POINT ( 'NONE',  ( 0.6544915521845998674, -81.05404539811999598, 1.531959166345999934 ) ) ;
#44991 = CARTESIAN_POINT ( 'NONE',  ( -1.595231864207000028, -77.80712252499999693, 0.4722078832578999741 ) ) ;
#44992 = CARTESIAN_POINT ( 'NONE',  ( -1.217390015640017253, -61.61893024898913040, 12.70229597944532252 ) ) ;
#44993 = CARTESIAN_POINT ( 'NONE',  ( 0.09701925739682260019, -82.37953645841547257, -1.543345753052644875 ) ) ;
#44994 = B_SPLINE_CURVE_WITH_KNOTS ( 'NONE', 3,
 ( #41366, #27475, #28348, #54935, #55523, #27769, #23058, #28644, #18647, #46694 ),
 .UNSPECIFIED., .F., .F.,
 ( 4, 2, 2, 2, 4 ),
 ( 0.000000000000000000, 0.2500000000000000000, 0.5000000000000000000, 0.7500000000000000000, 1.000000000000000000 ),
 .UNSPECIFIED. ) ;
#44995 = CARTESIAN_POINT ( 'NONE',  ( -12.66319951814999989, -61.98148258098999719, 0.1455783832297999902 ) ) ;
#44996 = CARTESIAN_POINT ( 'NONE',  ( 13.99999999996999911, -5.900000000026970781, -3.874887541704999824E-10 ) ) ;
#44997 = DIRECTION ( 'NONE',  ( -1.000000000000000000, 0.000000000000000000, 0.000000000000000000 ) ) ;
#44998 = CARTESIAN_POINT ( 'NONE',  ( -1.250000000000000000, -77.64999999999999147, 0.000000000000000000 ) ) ;
#44999 = B_SPLINE_CURVE_WITH_KNOTS ( 'NONE', 3,
 ( #20080, #56948, #16508, #33634, #34490, #38357, #15352, #25641, #20647, #15930, #51676, #19786, #55801, #33345, #47248, #51378, #6780, #16221, #42803, #2365, #33917, #7070, #25072, #51956, #43095, #2653, #56665, #31738, #35352, #27319, #39793, #786, #12646, #43666, #48390, #50075, #54778, #14320, #41197, #16798, #26219, #9912, #25928, #21505, #21212, #18766, #43952, #18479, #44235, #40912, #36759, #3503, #23192, #39512, #53376, #52806, #39220, #32314, #57517, #50362, #502, #5188, #3225, #22899, #17077, #12359, #53094, #57233, #3788, #35059, #21789, #34782, #30348, #27606, #7928, #36470, #30639, #48673, #8217, #14035, #9618, #57806, #17366, #12925, #49782, #9328, #45351, #45648, #4901, #54497, #56244, #20230, #15204, #5760, #10494, #50657, #6643, #55952, #37049, #33496, #1945, #46822, #37638, #19939, #5472, #37928, #55066, #2230, #24651, #6347, #24363, #42662, #42376, #23768, #15501, #14615, #6053, #15794, #28774, #38223, #33194, #33782, #51822, #51534, #14904, #27893, #23476, #47113, #45940, #41487, #1074, #10793, #29068, #11090, #19062, #32609, #41783, #42079, #10203, #28182, #46235, #51240, #55361, #1356, #55655, #37345, #19351, #32902, #1649, #50946, #28479 ),
 .UNSPECIFIED., .F., .F.,
 ( 4, 2, 2, 2, 1, 1, 1, 1, 2, 2, 2, 2, 1, 1, 2, 2, 2, 2, 1, 1, 1, 1, 1, 1, 2, 2, 2, 2, 2, 1, 1, 1, 1, 1, 2, 2, 2, 2, 1, 2, 2, 2, 2, 2, 1, 2, 2, 2, 2, 1, 2, 2, 1, 2, 2, 2, 1, 2, 2, 1, 1, 2, 2, 2, 1, 2, 2, 2, 1, 1, 1, 1, 1, 2, 2, 2, 2, 2, 2, 2, 2, 1, 1, 1, 2, 2, 2, 2, 2, 2, 2, 4 ),
 ( 0.000000000000000000, 0.03124999999989156590, 0.04687499999983734539, 0.05468749999981020737, 0.05859374999979660714, 0.06054687499978983478, 0.06152343749978646248, 0.06201171874978477633, 0.06225585937478389509, 0.06249999999978301385, 0.09374999999967163766, 0.1093749999996159461, 0.1171874999995880934, 0.1210937499995741601, 0.1230468749995671379, 0.1249999999995601296, 0.1562499999994484690, 0.1718749999993926247, 0.1796874999993647304, 0.1835937499993507693, 0.1855468749993438027, 0.1865234374993403055, 0.1870117187493385569, 0.1872558593743376687, 0.1873779296868371969, 0.1874999999993367250, 0.2187499999993724187, 0.2343749999993903210, 0.2421874999993992861, 0.2460937499994036992, 0.2480468749994058919, 0.2490234374994070021, 0.2495117187494075572, 0.2497558593744078348, 0.2498779296869079181, 0.2499999999994080291, 0.2812499999994439448, 0.2968749999994619304, 0.2988281249994641509, 0.2998046874994652611, 0.3007812499994663713, 0.3046874999994701461, 0.3124999999994775290, 0.3437499999995065614, 0.3476562499995102251, 0.3496093749995120570, 0.3515624999995138888, 0.3593749999995208833, 0.3749999999995349276, 0.3828124999995419220, 0.3867187499995454192, 0.3876953124995463074, 0.3886718749995471955, 0.3906249999995489164, 0.4062499999995626832, 0.4218749999995764499, 0.4238281249995781708, 0.4248046874995791145, 0.4257812499995800581, 0.4296874999995837774, 0.4374999999995911604, 0.4531249999996059818, 0.4609374999996134203, 0.4628906249996153077, 0.4648437499996171951, 0.4687499999996209143, 0.4843749999996359024, 0.4921874999996433409, 0.4960937499996470601, 0.4980468749996489475, 0.4990234374996498912, 0.4995117187496503908, 0.4997558593746505573, 0.4998779296871507238, 0.4999999999996508349, 0.5624999999996962430, 0.6249999999997415401, 0.6874999999997869482, 0.7187499999998095968, 0.7343749999998209210, 0.7421874999998265832, 0.7460937499998294697, 0.7480468749998309130, 0.7490234374998315792, 0.7495117187498319122, 0.7499999999998321343, 0.7812499999998532285, 0.8124999999998742117, 0.8437499999998951949, 0.8749999999999162892, 0.9374999999999580336, 1.000000000000000000 ),
 .UNSPECIFIED. ) ;
#45000 = CARTESIAN_POINT ( 'NONE',  ( 1.158141336542465760, -81.81941502368277952, -0.4701679534010050343 ) ) ;
#45001 = DIRECTION ( 'NONE',  ( 0.000000000000000000, -1.000000000000000000, 0.000000000000000000 ) ) ;
#45002 = CARTESIAN_POINT ( 'NONE',  ( -8.329953570067999635, -79.94897570143329801, -7.407190701775999919 ) ) ;
#45003 = DIRECTION ( 'NONE',  ( 0.000000000000000000, -1.000000000000000000, 0.000000000000000000 ) ) ;
#45004 = VERTEX_POINT ( 'NONE', #41798 ) ;
#45005 = VERTEX_POINT ( 'NONE', #14919 ) ;
#45006 = DIRECTION ( 'NONE',  ( 1.000000000000000000, 0.000000000000000000, 0.000000000000000000 ) ) ;
#45007 = ORIENTED_EDGE ( 'NONE', *, *, #41542, .F. ) ;
#45008 = SURFACE_STYLE_USAGE ( .BOTH. , #39690 ) ;
#45009 = AXIS2_PLACEMENT_3D ( 'NONE', #49471, #30844, #4595 ) ;
#45010 = VERTEX_POINT ( 'NONE', #32914 ) ;
#45011 = DIRECTION ( 'NONE',  ( 0.000000000000000000, -1.000000000000000000, 0.000000000000000000 ) ) ;
#45012 = DIRECTION ( 'NONE',  ( 0.000000000000000000, 1.000000000000000000, 1.567738888216000128E-14 ) ) ;
#45013 =( NAMED_UNIT ( * ) SI_UNIT ( $, .STERADIAN. ) SOLID_ANGLE_UNIT ( ) );
#45014 = EDGE_CURVE ( 'NONE', #10331, #36154, #15987, .T. ) ;
#45015 = CARTESIAN_POINT ( 'NONE',  ( 11.75000000000000000, -77.54999999999999716, 2.316376715183999699E-14 ) ) ;
#45016 = CARTESIAN_POINT ( 'NONE',  ( -1.751509483276000090, -79.75344838743700393, -10.89192126806999994 ) ) ;
#45017 = CARTESIAN_POINT ( 'NONE',  ( 1.667269374596999976, -23.20939883484999910, -12.49858097730999873 ) ) ;
#45018 = CARTESIAN_POINT ( 'NONE',  ( 3.481401630171999884, -82.62224128856598782, -0.2294689796840000129 ) ) ;
#45019 = CARTESIAN_POINT ( 'NONE',  ( 0.9218200799623692543, -80.22291666666664867, 1.199500263597272687 ) ) ;
#45020 = LINE ( 'NONE', #4867, #37536 ) ;
#45021 = CARTESIAN_POINT ( 'NONE',  ( -9.112421873709999787, -79.06464140765000082, -8.348385936088000392 ) ) ;
#45022 = AXIS2_PLACEMENT_3D ( 'NONE', #41006, #23573, #54869 ) ;
#45023 = VERTEX_POINT ( 'NONE', #11963 ) ;
#45024 = ORIENTED_EDGE ( 'NONE', *, *, #52773, .T. ) ;
#45025 = CARTESIAN_POINT ( 'NONE',  ( -7.601397897754999633, -18.75000000310999937, 10.07627163191000008 ) ) ;
#45026 = CARTESIAN_POINT ( 'NONE',  ( -1.423904377506317820, -17.69487194798944429, -12.50677628656574747 ) ) ;
#45027 = CIRCLE ( 'NONE', #34627, 0.5000000000000000000 ) ;
#45028 = CARTESIAN_POINT ( 'NONE',  ( -0.1698911186725000078, -80.60705187618100354, 1.322768475116000042 ) ) ;
#45029 = CARTESIAN_POINT ( 'NONE',  ( -9.022250383429000209, -78.73955560801599063, -3.573472734901999903 ) ) ;
#45030 = AXIS2_PLACEMENT_3D ( 'NONE', #22045, #4041, #17629 ) ;
#45031 = CARTESIAN_POINT ( 'NONE',  ( 3.451879464910937667, -86.39318692756698681, -1.536875756006140570 ) ) ;
#45032 = CARTESIAN_POINT ( 'NONE',  ( -1.186912087925585668, -86.00353166888481837, 3.216022959499840628 ) ) ;
#45033 = CARTESIAN_POINT ( 'NONE',  ( 6.861116763436999832, -76.59221882925000102, -9.781075755418999762 ) ) ;
#45034 = EDGE_CURVE ( 'NONE', #6045, #22190, #41896, .T. ) ;
#45035 = CARTESIAN_POINT ( 'NONE',  ( 0.6120151737828000149, -80.41762112988999434, 1.204744225600999918 ) ) ;
#45036 = CARTESIAN_POINT ( 'NONE',  ( -7.650190089120999737, -76.96361381506899590, 7.742423574132000219 ) ) ;
#45037 = CARTESIAN_POINT ( 'NONE',  ( -0.7482985437745418578, -79.17427425103403493, -1.003727883348249472 ) ) ;
#45038 = DIRECTION ( 'NONE',  ( -0.7071067811865475727, 0.000000000000000000, -0.7071067811865475727 ) ) ;
#45039 = CARTESIAN_POINT ( 'NONE',  ( 3.779826505644000356, -82.77871570665098488, 0.3812790984862000077 ) ) ;
#45040 = CARTESIAN_POINT ( 'NONE',  ( 3.228614917279000185, -80.98202518554889195, -10.79283437469000084 ) ) ;
#45041 = CARTESIAN_POINT ( 'NONE',  ( -10.38646360829000059, -56.02204592290999585, 7.655555357438999842 ) ) ;
#45042 = DIRECTION ( 'NONE',  ( 0.000000000000000000, -1.000000000000000000, 0.000000000000000000 ) ) ;
#45043 = CARTESIAN_POINT ( 'NONE',  ( -3.462036690261000249, -81.77132046129098342, -0.7738570222820000399 ) ) ;
#45044 = B_SPLINE_CURVE_WITH_KNOTS ( 'NONE', 3,
 ( #37244, #10392, #6242, #24259, #54681, #28672, #46424, #55550, #977, #14223, #41975, #1546, #27796, #18960, #31931, #36372, #9518, #54398 ),
 .UNSPECIFIED., .F., .F.,
 ( 4, 2, 2, 2, 2, 2, 2, 2, 4 ),
 ( 0.000000000000000000, 0.1250000000000000000, 0.2500000000000000000, 0.3750000000000000000, 0.5000000000000000000, 0.6250000000000000000, 0.7500000000000000000, 0.8750000000000000000, 1.000000000000000000 ),
 .UNSPECIFIED. ) ;
#45045 = CARTESIAN_POINT ( 'NONE',  ( -0.9420598709024999851, -79.27896011182599523, -0.8215979549846998964 ) ) ;
#45046 = DIRECTION ( 'NONE',  ( -1.000000000000000000, 0.000000000000000000, 0.000000000000000000 ) ) ;
#45047 = CARTESIAN_POINT ( 'NONE',  ( -10.34138800174999950, -80.86922762280332222, 4.468208825537999473 ) ) ;
#45048 = ADVANCED_FACE ( 'NONE', ( #57114 ), #12244, .F. ) ;
#45049 = CARTESIAN_POINT ( 'NONE',  ( 0.07399134906894000441, -2.190786218217000147, 3.805339572302000040 ) ) ;
#45050 = CARTESIAN_POINT ( 'NONE',  ( 1.274147325018575971, -80.50115893599860328, 0.01855956267719174532 ) ) ;
#45051 = ORIENTED_EDGE ( 'NONE', *, *, #56017, .F. ) ;
#45052 = CARTESIAN_POINT ( 'NONE',  ( 0.000000000000000000, 4.040000000000000036, 0.000000000000000000 ) ) ;
#45053 = ADVANCED_FACE ( 'NONE', ( #43843 ), #465, .F. ) ;
#45054 = CARTESIAN_POINT ( 'NONE',  ( -11.00000000000000888, -79.18958333333333144, 1.439896632895279360 ) ) ;
#45055 = CARTESIAN_POINT ( 'NONE',  ( 1.316231252753000014, -82.02853028149598913, 0.2147359707272000207 ) ) ;
#45056 = DIRECTION ( 'NONE',  ( 1.000000000000000000, 0.000000000000000000, 0.000000000000000000 ) ) ;
#45057 = CARTESIAN_POINT ( 'NONE',  ( 12.56884868898000107, -76.71184971201999758, -3.366471670097000324 ) ) ;
#45058 = CARTESIAN_POINT ( 'NONE',  ( 5.662870153706999865, -79.74636001420199705, -7.651606806962000462 ) ) ;
#45059 = CARTESIAN_POINT ( 'NONE',  ( 12.60552522436000089, -23.28917565320000094, -1.799501877760999902 ) ) ;
#45060 = EDGE_LOOP ( 'NONE', ( #52249, #20724, #17265, #15108 ) ) ;
#45061 = CARTESIAN_POINT ( 'NONE',  ( -13.86363636363000218, -69.16102867818000277, -1.277888281761000050E-05 ) ) ;
#45062 = DIRECTION ( 'NONE',  ( 0.7071067811865474617, 0.000000000000000000, -0.7071067811865474617 ) ) ;
#45063 = AXIS2_PLACEMENT_3D ( 'NONE', #24234, #42252, #27773 ) ;
#45064 = CARTESIAN_POINT ( 'NONE',  ( -1.111488374662999989, -81.24468314134999503, 0.8650934752202000810 ) ) ;
#45065 = DIRECTION ( 'NONE',  ( 0.000000000000000000, -1.000000000000000000, 0.000000000000000000 ) ) ;
#45066 = CARTESIAN_POINT ( 'NONE',  ( 8.286539809994000194, -78.24792830956099010, 4.690803151849999963 ) ) ;
#45068 = CARTESIAN_POINT ( 'NONE',  ( -1.182840957218999955, -1.453210179782000067, -3.838043326965000279 ) ) ;
#45067 = CARTESIAN_POINT ( 'NONE',  ( 4.045858611978000674, -83.95300820753398341, 1.029872831580999959 ) ) ;
#45069 = CARTESIAN_POINT ( 'NONE',  ( -2.062673488410000200, -60.12452273675999947, -12.82904109066000053 ) ) ;
#45070 = CARTESIAN_POINT ( 'NONE',  ( -1.312293291923000149, -79.58906442605000109, -0.7594922433479999180 ) ) ;
#45071 = ADVANCED_FACE ( 'NONE', ( #56542 ), #49490, .T. ) ;
#45072 = ORIENTED_EDGE ( 'NONE', *, *, #52097, .T. ) ;
#45073 = CARTESIAN_POINT ( 'NONE',  ( 0.4998953799361084971, -77.22882438990886556, -10.73929381184138698 ) ) ;
#45074 = CARTESIAN_POINT ( 'NONE',  ( -0.5999999999999999778, -23.15000000000000213, -12.00000000000000000 ) ) ;
#45075 = CARTESIAN_POINT ( 'NONE',  ( -3.914500761937000028, -78.91452044229970397, -1.642509933758750038E-14 ) ) ;
#45076 = ORIENTED_EDGE ( 'NONE', *, *, #49441, .T. ) ;
#45077 = VERTEX_POINT ( 'NONE', #29939 ) ;
#45078 = CARTESIAN_POINT ( 'NONE',  ( 9.663556473158999793, -79.58198580643298214, -5.128693071642000056 ) ) ;
#45079 = CARTESIAN_POINT ( 'NONE',  ( -4.000000000000000000, -75.00000000000001421, 0.5999999999999999778 ) ) ;
#45080 = CARTESIAN_POINT ( 'NONE',  ( 1.939955037980729990, -80.36060123837306435, 10.61985788779979423 ) ) ;
#45081 = EDGE_LOOP ( 'NONE', ( #58335, #28578, #52587, #20941 ) ) ;
#45082 = CARTESIAN_POINT ( 'NONE',  ( 8.737371597357999065, -78.93304436543799341, 8.129823451939000023 ) ) ;
#45083 = VERTEX_POINT ( 'NONE', #34946 ) ;
#45084 = ORIENTED_EDGE ( 'NONE', *, *, #26314, .T. ) ;
#45085 = CARTESIAN_POINT ( 'NONE',  ( 1.292332971236618944, -2.758531009554976876, -2.981824453458054691 ) ) ;
#45086 = CARTESIAN_POINT ( 'NONE',  ( -10.78616240765133227, -76.43596441176799772, -5.318014019118542102 ) ) ;
#45087 = CARTESIAN_POINT ( 'NONE',  ( -9.699833017908000343, -79.74065229497952600, 1.146274062705999963 ) ) ;
#45088 = B_SPLINE_SURFACE_WITH_KNOTS ( 'NONE', 3, 3, ( 
 ( #34260, #47881, #43149, #43429 ),
 ( #51725, #52011, #52580, #34835 ),
 ( #52865, #20132, #29543, #11277 ),
 ( #29255, #42856, #42565, #12419 ),
 ( #47012, #2131, #52292, #38120 ),
 ( #20988, #15691, #34548, #38412 ),
 ( #33687, #2416, #6830, #2989 ),
 ( #20418, #7412, #56432, #12131 ) ),
 .UNSPECIFIED., .F., .F., .F.,
 ( 4, 1, 1, 1, 1, 4 ),
 ( 4, 4 ),
 ( -0.01200407345746999990, 0.000000000000000000, 0.3333333333333000081, 0.6666666666667000474, 1.000000000000000000, 1.011997855551999947 ),
 ( -0.3559705542741999906, 1.355970554273999928 ),
 .UNSPECIFIED. ) ;
#45089 = ORIENTED_EDGE ( 'NONE', *, *, #35530, .T. ) ;
#45090 = CARTESIAN_POINT ( 'NONE',  ( 1.499741147044569178, -81.66063338586604914, 0.1964284907518392131 ) ) ;
#45091 = ORIENTED_EDGE ( 'NONE', *, *, #54291, .F. ) ;
#45092 = CARTESIAN_POINT ( 'NONE',  ( 3.250000000000000000, -2.350000000000000089, 0.000000000000000000 ) ) ;
#45093 = CARTESIAN_POINT ( 'NONE',  ( -11.77412505557000699, -79.80000000000001137, -2.187958323471518973 ) ) ;
#45094 = CARTESIAN_POINT ( 'NONE',  ( 1.500000000000000000, -81.75000000000000000, 0.000000000000000000 ) ) ;
#45095 = AXIS2_PLACEMENT_3D ( 'NONE', #16309, #52324, #47332 ) ;
#45096 = CARTESIAN_POINT ( 'NONE',  ( -7.655542440070999710, -22.77819125662999866, -10.38645071867999903 ) ) ;
#45097 = CARTESIAN_POINT ( 'NONE',  ( 5.917523019358037040, -77.13333333333329733, 10.26699006316254525 ) ) ;
#45098 = EDGE_CURVE ( 'NONE', #16529, #19092, #7528, .T. ) ;
#45099 = CARTESIAN_POINT ( 'NONE',  ( -1.704789468943344266, -55.09653838336419085, 12.53199752951682022 ) ) ;
#45100 = CARTESIAN_POINT ( 'NONE',  ( 7.641012386057000505, -60.08917565288000162, -10.18589234709999936 ) ) ;
#45101 = CARTESIAN_POINT ( 'NONE',  ( -0.4252449232878383056, -78.72143397250610519, -9.249944552399744779 ) ) ;
#45102 = EDGE_CURVE ( 'NONE', #3351, #33164, #21190, .T. ) ;
#45103 = CARTESIAN_POINT ( 'NONE',  ( -9.996770077869998161, -24.15065455350000079, 7.758602204116000323 ) ) ;
#45104 = CARTESIAN_POINT ( 'NONE',  ( -0.3926218265389189721, -80.00416666666666288, -1.460959015002473604 ) ) ;
#45105 = CARTESIAN_POINT ( 'NONE',  ( 8.777412155057099596, -77.82412362302341080, -2.980421710618992304 ) ) ;
#45106 = CARTESIAN_POINT ( 'NONE',  ( 7.220923959705223716, -76.62291666666662593, 9.396085398178630754 ) ) ;
#45107 = CARTESIAN_POINT ( 'NONE',  ( -4.005639385872000524, -81.64480496681198929, 1.168295999664000107 ) ) ;
#45108 = CARTESIAN_POINT ( 'NONE',  ( 3.755238055182999801, -78.09928667140098923, 8.648011040868999189 ) ) ;
#45109 = CARTESIAN_POINT ( 'NONE',  ( 0.9519702974794926886, -79.69303294589165887, -0.8296275306155781459 ) ) ;
#45110 = AXIS2_PLACEMENT_3D ( 'NONE', #12704, #35717, #54556 ) ;
#45111 = CARTESIAN_POINT ( 'NONE',  ( 9.063334061753160142, -77.12500000000001421, -2.943243628773176024 ) ) ;
#45112 = CARTESIAN_POINT ( 'NONE',  ( -0.8537148449481000156, -24.70498145908999987, 12.43377424872999981 ) ) ;
#45113 = CARTESIAN_POINT ( 'NONE',  ( 0.3565886142880393406, -81.10348178115825135, 1.276299026773298317 ) ) ;
#45114 = PLANE ( 'NONE',  #10000 ) ;
#45115 = CARTESIAN_POINT ( 'NONE',  ( -3.960388868909999971, -0.8168122488617000077, -1.146868004699999943 ) ) ;
#45116 = CARTESIAN_POINT ( 'NONE',  ( -1.499999999985999866, -82.00000000001401190, -1.019196462549000076E-10 ) ) ;
#45117 = CARTESIAN_POINT ( 'NONE',  ( 9.191325695085856395, -79.84005264655188228, -1.210935613487206908 ) ) ;
#45118 = EDGE_CURVE ( 'NONE', #37124, #35685, #6115, .T. ) ;
#45119 = APPLICATION_CONTEXT ( 'automotive_design' ) ;
#45120 = CARTESIAN_POINT ( 'NONE',  ( 0.3139938800012240794, -80.99102801640374594, -1.479408638137562182 ) ) ;
#45121 = CARTESIAN_POINT ( 'NONE',  ( 12.66319951814999989, -61.98148258098999719, -0.1455783832297999902 ) ) ;
#45122 = CARTESIAN_POINT ( 'NONE',  ( 0.7608607662309999631, -78.57210341376899976, -1.424185669224000028 ) ) ;
#45123 = CARTESIAN_POINT ( 'NONE',  ( -13.13047446164998711, -22.78578169018998878, 0.8260994316375004365 ) ) ;
#45124 = CARTESIAN_POINT ( 'NONE',  ( -10.91657421154000041, -78.02703838196799779, -0.06142861151470001280 ) ) ;
#45125 = CARTESIAN_POINT ( 'NONE',  ( 11.99621472858000004, -77.20440045069699408, 2.018255885614000267 ) ) ;
#45126 = CARTESIAN_POINT ( 'NONE',  ( -7.412025882568599400, -78.16672174443260701, -8.233944902729591675 ) ) ;
#45128 = CARTESIAN_POINT ( 'NONE',  ( 0.1534498121882000021, -78.16368429802710693, 1.409436946036999760 ) ) ;
#45127 = CARTESIAN_POINT ( 'NONE',  ( 0.7554284705563452107, -79.73333333333330586, 1.310679582531388609 ) ) ;
#45129 = CARTESIAN_POINT ( 'NONE',  ( 11.00000000000000000, -77.44999999999998863, 0.000000000000000000 ) ) ;
#45130 = VERTEX_POINT ( 'NONE', #39106 ) ;
#45131 = CARTESIAN_POINT ( 'NONE',  ( 0.2703784039104000225, -82.99532450217398605, 3.579196188411999824 ) ) ;
#45132 = CARTESIAN_POINT ( 'NONE',  ( -10.21850601694999838, -80.60801320267160008, 4.517287938863999486 ) ) ;
#45133 = DIRECTION ( 'NONE',  ( 0.000000000000000000, 0.000000000000000000, -1.000000000000000000 ) ) ;
#45134 = CARTESIAN_POINT ( 'NONE',  ( -2.641601459057217660, -84.86666667622432669, -2.210339097018351850 ) ) ;
#45135 = CARTESIAN_POINT ( 'NONE',  ( 11.08595418830999968, -77.07172445793599991, -1.708721840212999998 ) ) ;
#45136 = CARTESIAN_POINT ( 'NONE',  ( -10.01752098898000121, -59.99172009619000079, 7.660412494194000388 ) ) ;
#45137 = CARTESIAN_POINT ( 'NONE',  ( -4.832441116568999995, -78.74550106883198453, 8.456193503077001239 ) ) ;
#45138 = LINE ( 'NONE', #32400, #17607 ) ;
#45139 = CARTESIAN_POINT ( 'NONE',  ( -6.862215669877000046, -79.33480064555399736, -7.123593673834999862 ) ) ;
#45140 = CARTESIAN_POINT ( 'NONE',  ( -2.836899952100275790, -3.141950402152397626, -1.634619481798827545 ) ) ;
#45141 = CARTESIAN_POINT ( 'NONE',  ( -1.931043742978000077, -56.02204592290999585, 12.75763395696999858 ) ) ;
#45142 = VERTEX_POINT ( 'NONE', #47416 ) ;
#45143 = FACE_OUTER_BOUND ( 'NONE', #34089, .T. ) ;
#45144 = CARTESIAN_POINT ( 'NONE',  ( -7.601397897754999633, -55.55000000278000272, 10.07627163191000008 ) ) ;
#45145 = VECTOR ( 'NONE', #29126, 1000.000000000000114 ) ;
#45146 = CARTESIAN_POINT ( 'NONE',  ( 0.000000000000000000, -76.15000000005198899, -2.149999999947999729 ) ) ;
#45147 = CARTESIAN_POINT ( 'NONE',  ( 1.460959015002474493, -81.62916666666667709, -0.3926218265389176953 ) ) ;
#45148 = CARTESIAN_POINT ( 'NONE',  ( 3.546985177240999931, -82.42742953870899214, -0.05580604480424000702 ) ) ;
#45149 = CARTESIAN_POINT ( 'NONE',  ( 10.98521615365917725, -23.34051012009622283, 0.5703160980905067623 ) ) ;
#45150 = ORIENTED_EDGE ( 'NONE', *, *, #38046, .F. ) ;
#45151 = CARTESIAN_POINT ( 'NONE',  ( 10.02418919408999898, -78.14383715211899073, -4.770675716736000105 ) ) ;
#45152 = CARTESIAN_POINT ( 'NONE',  ( -2.062597299672999540, -22.78485473281999774, 12.87022657272000004 ) ) ;
#45153 = ORIENTED_EDGE ( 'NONE', *, *, #34364, .F. ) ;
#45154 = EDGE_CURVE ( 'NONE', #22042, #26124, #54207, .T. ) ;
#45155 = EDGE_LOOP ( 'NONE', ( #12592, #53794, #10581, #45051 ) ) ;
#45156 = AXIS2_PLACEMENT_3D ( 'NONE', #6749, #18161, #41165 ) ;
#45157 = CARTESIAN_POINT ( 'NONE',  ( -10.18127254042999930, -55.41355771686999532, -7.633407132363999814 ) ) ;
#45158 =( NAMED_UNIT ( * ) SI_UNIT ( $, .STERADIAN. ) SOLID_ANGLE_UNIT ( ) );
#45159 = CARTESIAN_POINT ( 'NONE',  ( -4.373213035511999358, -79.35790588805998880, -8.733596771889999388 ) ) ;
#45160 = ORIENTED_EDGE ( 'NONE', *, *, #16825, .T. ) ;
#45161 = CARTESIAN_POINT ( 'NONE',  ( -11.75756702865000136, -77.14570592927000803, -3.383315852985000038 ) ) ;
#45162 = CARTESIAN_POINT ( 'NONE',  ( -10.28385508244830149, -78.62383711279117904, -3.166186455522963072 ) ) ;
#45163 = CARTESIAN_POINT ( 'NONE',  ( 1.514178452211000225, -78.05229887042999337, 0.6512674748728999319 ) ) ;
#45164 = ORIENTED_EDGE ( 'NONE', *, *, #44498, .F. ) ;
#45165 = CARTESIAN_POINT ( 'NONE',  ( 1.529609450199000076, -76.99217694988499261, 9.371081266747001592 ) ) ;
#45166 = CARTESIAN_POINT ( 'NONE',  ( 0.4581446724472641452, -80.25495920898164570, -1.163148308167606171 ) ) ;
#45167 = CARTESIAN_POINT ( 'NONE',  ( -9.306321164319999895, -77.05658961653000461, -9.238944841226000904 ) ) ;
#45168 = CARTESIAN_POINT ( 'NONE',  ( -7.712695008784000272, -77.31466668148844690, -8.144473358846001432 ) ) ;
#45169 = CARTESIAN_POINT ( 'NONE',  ( 3.402340145821570072, -86.39318692614398287, 2.471221923361245576 ) ) ;
#45170 = CARTESIAN_POINT ( 'NONE',  ( -2.572125540837000290, -78.35365303490424083, -9.357076443458000270 ) ) ;
#45171 = CARTESIAN_POINT ( 'NONE',  ( 7.030819185249340464, -79.90638907312039407, 6.010730751432092234 ) ) ;
#45172 = CARTESIAN_POINT ( 'NONE',  ( -3.689614304937916422, -78.79635414669442639, -1.576161069557058703 ) ) ;
#45173 = ORIENTED_EDGE ( 'NONE', *, *, #55067, .F. ) ;
#45174 = DIRECTION ( 'NONE',  ( 0.000000000000000000, -1.000000000000000000, 0.000000000000000000 ) ) ;
#45175 = EDGE_CURVE ( 'NONE', #57178, #31856, #36283, .T. ) ;
#45176 = CARTESIAN_POINT ( 'NONE',  ( 11.65396969189999865, -75.74817663119999622, -2.860942225950000140 ) ) ;
#45177 = CARTESIAN_POINT ( 'NONE',  ( -1.597158643424000157, -80.39632141193499137, 0.2372724044997999993 ) ) ;
#45178 = CARTESIAN_POINT ( 'NONE',  ( -1.138524516885000004, -79.11590538786700222, 0.6666316858816999646 ) ) ;
#45179 = CARTESIAN_POINT ( 'NONE',  ( -11.00000000000000000, -79.09999999999999432, 0.000000000000000000 ) ) ;
#45180 = AXIS2_PLACEMENT_3D ( 'NONE', #21077, #25214, #12221 ) ;
#45181 = CARTESIAN_POINT ( 'NONE',  ( 12.82904109062999964, -18.67547726287999765, 2.062673488410000200 ) ) ;
#45182 = CARTESIAN_POINT ( 'NONE',  ( 8.174587033571999228, -77.32012175574699597, -8.440297792765999674 ) ) ;
#45183 = CARTESIAN_POINT ( 'NONE',  ( -9.199999999999999289, -77.00000000000000000, 0.000000000000000000 ) ) ;
#45184 = CARTESIAN_POINT ( 'NONE',  ( 0.6679705033387999258, -77.07363832859898878, -9.605423498967001095 ) ) ;
#45185 = CARTESIAN_POINT ( 'NONE',  ( 11.51565071235703464, -76.77562505554482186, -3.637760148594212151 ) ) ;
#45186 = CARTESIAN_POINT ( 'NONE',  ( 12.17658135360961147, -76.23143817709451753, 4.630469027495792034 ) ) ;
#45187 = EDGE_CURVE ( 'NONE', #44478, #19275, #38235, .T. ) ;
#45188 = ORIENTED_EDGE ( 'NONE', *, *, #50760, .T. ) ;
#45189 = CARTESIAN_POINT ( 'NONE',  ( 1.495758047513000122, -83.11641278936299670, -0.5264119980271999566 ) ) ;
#45190 = FACE_OUTER_BOUND ( 'NONE', #29246, .T. ) ;
#45191 = AXIS2_PLACEMENT_3D ( 'NONE', #38224, #7803, #43831 ) ;
#45192 = CARTESIAN_POINT ( 'NONE',  ( 0.000000000000000000, -76.79999999999999716, -5.100000000000001421 ) ) ;
#45193 = CARTESIAN_POINT ( 'NONE',  ( 7.247098260574433404, -76.95000000000000284, -6.187590336956020565 ) ) ;
#45194 = VECTOR ( 'NONE', #45012, 1000.000000000000000 ) ;
#45195 = CARTESIAN_POINT ( 'NONE',  ( 3.910274016995999968, -78.42502719647299614, 11.27587067850999958 ) ) ;
#45196 = CARTESIAN_POINT ( 'NONE',  ( 0.000000000000000000, -3.749999999256000027, 0.000000000000000000 ) ) ;
#45197 = CARTESIAN_POINT ( 'NONE',  ( 8.488869829350999652, -78.99276232907497786, 4.102512142575000631 ) ) ;
#45198 = CARTESIAN_POINT ( 'NONE',  ( 0.5528049087483969393, -76.07108491924718408, 11.73740210370585579 ) ) ;
#45199 = CARTESIAN_POINT ( 'NONE',  ( -8.157922760392999351, -80.08442983025919659, -7.254216858269000312 ) ) ;
#45200 = CARTESIAN_POINT ( 'NONE',  ( -0.8849062459890528753, -82.21372529178493949, -0.9173043153348533485 ) ) ;
#45201 = VERTEX_POINT ( 'NONE', #15807 ) ;
#45202 = CARTESIAN_POINT ( 'NONE',  ( -12.19234209666000091, -76.06101097214411766, -1.697737568323999913 ) ) ;
#45203 = CARTESIAN_POINT ( 'NONE',  ( -0.03239454126609288276, -78.54828564506388489, -3.437034970110011134 ) ) ;
#45204 = CARTESIAN_POINT ( 'NONE',  ( 0.9090372547675998893, -78.79855302811299111, 10.93790052299999971 ) ) ;
#45205 = LINE ( 'NONE', #31887, #55294 ) ;
#45206 = CARTESIAN_POINT ( 'NONE',  ( -2.626391644478000220, -76.26524937808599702, 12.22522157430999989 ) ) ;
#45207 = CYLINDRICAL_SURFACE ( 'NONE', #5729, 0.5000000000000006661 ) ;
#45208 = FACE_OUTER_BOUND ( 'NONE', #21182, .T. ) ;
#45209 = ORIENTED_EDGE ( 'NONE', *, *, #744, .F. ) ;
#45210 = CARTESIAN_POINT ( 'NONE',  ( -6.285096537930999538, -78.78619441778099031, -9.206093747065001054 ) ) ;
#45211 = DIRECTION ( 'NONE',  ( 0.000000000000000000, -1.000000000000000000, 0.000000000000000000 ) ) ;
#45212 = PRODUCT_RELATED_PRODUCT_CATEGORY ( 'part', '', ( #49847 ) ) ;
#45213 = CARTESIAN_POINT ( 'NONE',  ( -1.439896632895311335, -77.71458333333332291, -11.00000000000000178 ) ) ;
#45214 = CARTESIAN_POINT ( 'NONE',  ( 3.548349909811000291, -78.43735717367049176, -4.345475359304840494E-16 ) ) ;
#45215 = B_SPLINE_CURVE_WITH_KNOTS ( 'NONE', 3,
 ( #53692, #23558, #13528, #32401, #50156, #18272, #45732, #27687, #865, #31520 ),
 .UNSPECIFIED., .F., .F.,
 ( 4, 2, 2, 2, 4 ),
 ( 0.000000000000000000, 0.2499999999999999445, 0.4999999999999998890, 0.7499999999999998890, 1.000000000000000000 ),
 .UNSPECIFIED. ) ;
#45216 = CARTESIAN_POINT ( 'NONE',  ( 12.50680023857767154, -61.10414033366100739, 1.424451025847232044 ) ) ;
#45217 = CARTESIAN_POINT ( 'NONE',  ( 8.374122929021998729, -78.11349234901598493, 7.207772231549999908 ) ) ;
#45218 = DIRECTION ( 'NONE',  ( -0.7071067811865475727, 0.000000000000000000, 0.7071067811865475727 ) ) ;
#45219 = CARTESIAN_POINT ( 'NONE',  ( -0.4802501944169854653, -81.75012526588245976, 1.435307468129154440 ) ) ;
#45220 = EDGE_CURVE ( 'NONE', #58165, #27335, #53222, .T. ) ;
#45221 = VECTOR ( 'NONE', #51014, 1000.000000000000000 ) ;
#45222 = CARTESIAN_POINT ( 'NONE',  ( -8.082524092276901939, -79.95833333333331439, 4.658475568430788805 ) ) ;
#45223 = EDGE_CURVE ( 'NONE', #5279, #29318, #41399, .T. ) ;
#45224 = CARTESIAN_POINT ( 'NONE',  ( 0.000000000000000000, -90.39999999999999147, 0.000000000000000000 ) ) ;
#45225 = CARTESIAN_POINT ( 'NONE',  ( 7.374560639698954034, -77.12291666666664014, 9.596002108778181494 ) ) ;
#45226 = ORIENTED_EDGE ( 'NONE', *, *, #20685, .T. ) ;
#45227 = ORIENTED_EDGE ( 'NONE', *, *, #16816, .T. ) ;
#45228 = CARTESIAN_POINT ( 'NONE',  ( 9.252740428349001789, -78.62916666666666288, -2.486604901413144830 ) ) ;
#45229 = CARTESIAN_POINT ( 'NONE',  ( 4.106377143637999438, -77.78973998579799343, -8.613842362031000732 ) ) ;
#45230 = VECTOR ( 'NONE', #42894, 1000.000000000000000 ) ;
#45231 = ORIENTED_EDGE ( 'NONE', *, *, #50804, .T. ) ;
#45232 = CARTESIAN_POINT ( 'NONE',  ( 5.380788203752000953, -76.08505630325268498, 9.804131929786001010 ) ) ;
#45233 = ORIENTED_EDGE ( 'NONE', *, *, #53910, .T. ) ;
#45234 = CARTESIAN_POINT ( 'NONE',  ( 9.636781270573999691, -24.44031362782000016, 7.948066289838000564 ) ) ;
#45235 = CARTESIAN_POINT ( 'NONE',  ( -8.585712843602999911, -77.58711156713900436, 6.927284413728999724 ) ) ;
#45236 = CARTESIAN_POINT ( 'NONE',  ( 7.342331066867000544, -55.64999999967000122, -8.190859204290999784 ) ) ;
#45237 = CARTESIAN_POINT ( 'NONE',  ( -1.250000000000000000, -82.59999999999999432, 0.000000000000000000 ) ) ;
#45238 = CARTESIAN_POINT ( 'NONE',  ( -4.968906709420642720, -78.17991984054995669, -7.802392233778754793 ) ) ;
#45239 = CARTESIAN_POINT ( 'NONE',  ( 0.9578316561260999951, -78.89790929493999272, -11.17589679220000143 ) ) ;
#45240 = CARTESIAN_POINT ( 'NONE',  ( 6.723335045862328663, -79.23760275795656582, -6.670198521808291758 ) ) ;
#45241 = ORIENTED_EDGE ( 'NONE', *, *, #18549, .T. ) ;
#45242 = CARTESIAN_POINT ( 'NONE',  ( 2.321691164070382118, -79.80000000000001137, 11.71402344135003304 ) ) ;
#45243 = ORIENTED_EDGE ( 'NONE', *, *, #56248, .T. ) ;
#45244 = EDGE_CURVE ( 'NONE', #19797, #30600, #30077, .T. ) ;
#45245 = CARTESIAN_POINT ( 'NONE',  ( 1.445297155599249983, -77.46252827442208400, 9.136381658210661172 ) ) ;
#45246 = CARTESIAN_POINT ( 'NONE',  ( -9.177034484502000211, -77.38324421815998733, 6.137278520473000043 ) ) ;
#45247 = DIRECTION ( 'NONE',  ( -1.000000000000000000, 0.000000000000000000, 0.000000000000000000 ) ) ;
#45248 = CARTESIAN_POINT ( 'NONE',  ( -9.346518596363001308, -77.86878270725598838, 2.610229778083999808 ) ) ;
#45249 = CARTESIAN_POINT ( 'NONE',  ( -2.529679113815999969, -76.39605739169999765, 12.87721456411999910 ) ) ;
#45250 = CARTESIAN_POINT ( 'NONE',  ( -7.196477163768985719, -79.45634548972412858, -6.205214754808124233 ) ) ;
#45251 = CARTESIAN_POINT ( 'NONE',  ( -1.566959183383000109, -78.18940720036999892, 0.4396611996733000294 ) ) ;
#45252 = CARTESIAN_POINT ( 'NONE',  ( -8.744140569415000286, -80.43625931648698213, 7.086030162020000134 ) ) ;
#45253 = CARTESIAN_POINT ( 'NONE',  ( -10.87240354821999944, -78.93804972576597834, -1.216000584195999767 ) ) ;
#45254 = CARTESIAN_POINT ( 'NONE',  ( 1.217465845835394855, -78.22916666666665719, -0.3271848554490981997 ) ) ;
#45255 = CARTESIAN_POINT ( 'NONE',  ( -11.74964429611623729, -76.69742914047841964, 0.2920691019370554309 ) ) ;
#45256 = ADVANCED_FACE ( 'NONE', ( #12809 ), #18134, .F. ) ;
#45257 = CARTESIAN_POINT ( 'NONE',  ( -2.881647729895999710, -82.85917773387799912, 2.140058763724999924 ) ) ;
#45258 = AXIS2_PLACEMENT_3D ( 'NONE', #40067, #53661, #17347 ) ;
#45259 = VERTEX_POINT ( 'NONE', #31977 ) ;
#45260 = CARTESIAN_POINT ( 'NONE',  ( -9.700784073263999829, -78.95701179515099000, 7.398918521605999388 ) ) ;
#45261 = CARTESIAN_POINT ( 'NONE',  ( -9.225865441558999791, -76.12195766602600600, -6.449166915282999568 ) ) ;
#45262 = CARTESIAN_POINT ( 'NONE',  ( -4.239149814995500698, -78.00726517212316935, 9.879002636546259097 ) ) ;
#45263 = EDGE_CURVE ( 'NONE', #11057, #15123, #40565, .T. ) ;
#45264 = CARTESIAN_POINT ( 'NONE',  ( -11.96278216175999987, -78.12964977598299754, 0.6386762756999999624 ) ) ;
#45265 = DIRECTION ( 'NONE',  ( 0.000000000000000000, -1.000000000000000000, 0.000000000000000000 ) ) ;
#45266 = CARTESIAN_POINT ( 'NONE',  ( -10.20076653041301817, -79.07412882710335111, 3.463740470522618242 ) ) ;
#45267 = CARTESIAN_POINT ( 'NONE',  ( -1.103931346216595166, -54.17916251667382710, 12.50298439255883665 ) ) ;
#45268 = CARTESIAN_POINT ( 'NONE',  ( 3.922593800618577653, -80.94544671216375775, 10.00878386548077259 ) ) ;
#45269 = CARTESIAN_POINT ( 'NONE',  ( -4.206058715153999650, -80.52587970449398824, 10.59755966650999959 ) ) ;
#45270 = DIRECTION ( 'NONE',  ( 0.000000000000000000, 1.000000000000000000, 0.000000000000000000 ) ) ;
#45271 = CARTESIAN_POINT ( 'NONE',  ( 5.119217263405000828, -77.72816619513099567, 9.901929871541000239 ) ) ;
#45272 = CARTESIAN_POINT ( 'NONE',  ( -2.598917237794094337, -1.947916666666666741, 1.997276839918461722 ) ) ;
#45273 = CARTESIAN_POINT ( 'NONE',  ( 4.240563026683999759, -80.61527915106279352, -10.17766115582000097 ) ) ;
#45274 = ORIENTED_EDGE ( 'NONE', *, *, #15972, .F. ) ;
#45275 = CARTESIAN_POINT ( 'NONE',  ( 1.890224871708999999, -55.05210751953000425, 12.68696160870999989 ) ) ;
#45276 = CARTESIAN_POINT ( 'NONE',  ( -1.801750019961000149, -60.19007426689000084, -12.59656967656000148 ) ) ;
#45277 = CARTESIAN_POINT ( 'NONE',  ( 3.912230941219999369, -3.068769585190000093, 0.6523515869903999675 ) ) ;
#45278 = CARTESIAN_POINT ( 'NONE',  ( -9.457500717944000712, -78.31128036874700626, -6.031068363571000290 ) ) ;
#45279 = CARTESIAN_POINT ( 'NONE',  ( 8.796335266379992746, -79.89791666666666003, -6.760013919724047859 ) ) ;
#45280 = CONICAL_SURFACE ( 'NONE', #19818, 10.93038838648999977, 1.373400766944759877 ) ;
#45281 = CARTESIAN_POINT ( 'NONE',  ( -1.997276839918471714, -1.572916666666666741, -2.598917237794086788 ) ) ;
#45282 = DIRECTION ( 'NONE',  ( -1.000000000000000000, 0.000000000000000000, 0.000000000000000000 ) ) ;
#45283 = CARTESIAN_POINT ( 'NONE',  ( -5.045392105209124622, -78.58623691269025358, -9.528847481764330496 ) ) ;
#45284 = CARTESIAN_POINT ( 'NONE',  ( 12.66319948256999872, -16.81851729361000380, 0.1456213732515000137 ) ) ;
#45285 = CIRCLE ( 'NONE', #16992, 9.760776772971999193 ) ;
#45286 = CARTESIAN_POINT ( 'NONE',  ( 0.2052605617601000187, -85.79442953870898236, 4.167054658242999921 ) ) ;
#45287 = EDGE_CURVE ( 'NONE', #21041, #24542, #42882, .T. ) ;
#45288 = CARTESIAN_POINT ( 'NONE',  ( 5.173491034367821761, -77.36110484090335149, -10.64243316413162965 ) ) ;
#45289 = CARTESIAN_POINT ( 'NONE',  ( -12.80742885296000111, -79.00613957653999364, -1.906747295896999983 ) ) ;
#45290 = CARTESIAN_POINT ( 'NONE',  ( -5.774605976465999824, -77.85874741097399010, -9.668913608825000949 ) ) ;
#45291 = CARTESIAN_POINT ( 'NONE',  ( 0.4771943503223999850, -80.35929403190999665, -1.596102929133000004 ) ) ;
#45292 = CARTESIAN_POINT ( 'NONE',  ( -0.6467060841615001054, -78.98407060936000335, -1.407647497788000024 ) ) ;
#45293 = CARTESIAN_POINT ( 'NONE',  ( 0.9935076047078643668, -61.76816187723569129, 12.70250268220879875 ) ) ;
#45294 = CARTESIAN_POINT ( 'NONE',  ( 9.250000000000005329, -78.26041666666667140, 1.210822168571039192 ) ) ;
#45295 = DIRECTION ( 'NONE',  ( 0.000000000000000000, -1.000000000000000000, 0.000000000000000000 ) ) ;
#45296 = CARTESIAN_POINT ( 'NONE',  ( -7.311770087164275012, -80.16592078360770302, -7.880827117992419417 ) ) ;
#45297 = CARTESIAN_POINT ( 'NONE',  ( -8.838834764832000701, -23.25000000000000000, -8.838834764832000701 ) ) ;
#45298 = CARTESIAN_POINT ( 'NONE',  ( 1.232424253006426884, -77.92032519149937286, 0.3249715972912227135 ) ) ;
#45299 = ORIENTED_EDGE ( 'NONE', *, *, #40532, .F. ) ;
#45300 = EDGE_CURVE ( 'NONE', #42021, #37146, #27267, .T. ) ;
#45301 = CARTESIAN_POINT ( 'NONE',  ( 0.000000000000000000, -76.29999999995945359, 0.000000000000000000 ) ) ;
#45302 = CARTESIAN_POINT ( 'NONE',  ( 0.000000000000000000, -80.70000000003399521, 0.000000000000000000 ) ) ;
#45303 = CARTESIAN_POINT ( 'NONE',  ( 9.995598443669999611, -79.10464906837700028, -4.933823296771000955 ) ) ;
#45304 = CARTESIAN_POINT ( 'NONE',  ( 1.250000000000000222, -80.23958333333330017, -0.1636246173744659582 ) ) ;
#45305 = ORIENTED_EDGE ( 'NONE', *, *, #46337, .T. ) ;
#45306 = ORIENTED_EDGE ( 'NONE', *, *, #16367, .T. ) ;
#45307 = AXIS2_PLACEMENT_3D ( 'NONE', #17182, #43779, #4490 ) ;
#45308 = CARTESIAN_POINT ( 'NONE',  ( 1.085118080231999960, -81.30829811310599098, 1.195714296125000020 ) ) ;
#45309 = ORIENTED_EDGE ( 'NONE', *, *, #53583, .F. ) ;
#45310 = LINE ( 'NONE', #31695, #44329 ) ;
#45311 = ORIENTED_EDGE ( 'NONE', *, *, #2760, .T. ) ;
#45312 = CARTESIAN_POINT ( 'NONE',  ( 7.954951288349001004, -55.54999999966999980, -9.722718241315000398 ) ) ;
#45313 = CARTESIAN_POINT ( 'NONE',  ( 1.791008777272000030, -80.21228312261607130, 11.11143388882000060 ) ) ;
#45314 = CARTESIAN_POINT ( 'NONE',  ( -0.9218200799623775810, -78.42708333333332860, 1.199500263597266247 ) ) ;
#45315 = CARTESIAN_POINT ( 'NONE',  ( 0.005119011380242999981, -24.93813862189000119, -12.43705489344000092 ) ) ;
#45316 = CARTESIAN_POINT ( 'NONE',  ( 3.540977845989000006, -81.09906924513698812, -0.5875551853567000382 ) ) ;
#45317 = LINE ( 'NONE', #4574, #47942 ) ;
#45318 = CARTESIAN_POINT ( 'NONE',  ( 12.01346855044000073, -78.57433180934999939, -1.078935046565000277 ) ) ;
#45319 = VERTEX_POINT ( 'NONE', #158 ) ;
#45320 = VERTEX_POINT ( 'NONE', #8102 ) ;
#45321 = LINE ( 'NONE', #40293, #26328 ) ;
#45322 = CARTESIAN_POINT ( 'NONE',  ( -1.001315002179000047, -17.31477588286000113, -12.50000000000000000 ) ) ;
#45323 = CARTESIAN_POINT ( 'NONE',  ( 0.2659376973789999710, -79.86286252546500464, -1.306848610430999980 ) ) ;
#45324 = AXIS2_PLACEMENT_3D ( 'NONE', #54938, #46107, #46984 ) ;
#45325 = CARTESIAN_POINT ( 'NONE',  ( 7.890274420948999001, -78.91009858278999900, -5.649267206312000411 ) ) ;
#45326 = AXIS2_PLACEMENT_3D ( 'NONE', #9632, #31751, #14628 ) ;
#45327 = CARTESIAN_POINT ( 'NONE',  ( 3.654181830570063738, -86.12610001270965654, -1.626946572303013872 ) ) ;
#45328 = FACE_OUTER_BOUND ( 'NONE', #19605, .T. ) ;
#45329 = CARTESIAN_POINT ( 'NONE',  ( -10.59557217617999925, -76.86974203406001038, 7.456311996931999531 ) ) ;
#45330 = CARTESIAN_POINT ( 'NONE',  ( 0.3004848064042999756, -79.72286976367999500, -1.317452118262000038 ) ) ;
#45331 = CARTESIAN_POINT ( 'NONE',  ( -4.671753383259999559, -76.43689303329699669, 9.830826615545998237 ) ) ;
#45332 = DIRECTION ( 'NONE',  ( 0.000000000000000000, 1.000000000000000000, 0.000000000000000000 ) ) ;
#45333 = CARTESIAN_POINT ( 'NONE',  ( -0.4362624902269000016, -80.53743850270798532, -4.149668388003999731 ) ) ;
#45334 = CARTESIAN_POINT ( 'NONE',  ( 11.22355342542000045, -80.52296671422550389, 0.9700744431168999427 ) ) ;
#45335 = CARTESIAN_POINT ( 'NONE',  ( -10.01332844639000008, -60.08056692637000396, 7.654537085048000122 ) ) ;
#45336 = CARTESIAN_POINT ( 'NONE',  ( -7.489529519948906255, -78.22972517753335353, 9.112965939832363915 ) ) ;
#45337 = CARTESIAN_POINT ( 'NONE',  ( -1.194527725498000237, -82.00555496681198520, -3.339861958729000158 ) ) ;
#45338 = CARTESIAN_POINT ( 'NONE',  ( -1.150888948972000003, -79.17973486506399183, 0.6738713386821000295 ) ) ;
#45339 = DIRECTION ( 'NONE',  ( 4.762495317921000031E-11, 1.000000000000000000, 4.762531464717999529E-11 ) ) ;
#45340 = CARTESIAN_POINT ( 'NONE',  ( 7.551392188974999975, -80.14932253944839147, 8.117862728809001283 ) ) ;
#45341 = CARTESIAN_POINT ( 'NONE',  ( -0.4587696627765999735, -3.467384982432999863, -3.778272981138000031 ) ) ;
#45342 = DIRECTION ( 'NONE',  ( -0.9999999924279685537, 0.000000000000000000, -0.0001230612157848962919 ) ) ;
#45343 = ORIENTED_EDGE ( 'NONE', *, *, #27348, .T. ) ;
#45344 = DIRECTION ( 'NONE',  ( -0.7071067811865474617, -3.445410891336226740E-11, 0.7071067811865474617 ) ) ;
#45345 = CARTESIAN_POINT ( 'NONE',  ( -0.5705388283868735311, -18.65989902471411810, -10.98520465578141092 ) ) ;
#45346 = CARTESIAN_POINT ( 'NONE',  ( -2.879226727952071574, -79.30416666666667425, -10.71369944335147473 ) ) ;
#45347 = CARTESIAN_POINT ( 'NONE',  ( -1.321095329625999959, -82.27659339840100472, -0.1826337427822999904 ) ) ;
#45348 = AXIS2_PLACEMENT_3D ( 'NONE', #24709, #2286, #38568 ) ;
#45349 = CARTESIAN_POINT ( 'NONE',  ( 1.931086388578000079, -55.50221245779999890, 12.71798269383000068 ) ) ;
#45350 = CARTESIAN_POINT ( 'NONE',  ( -12.96685733093999993, -76.98937291683000694, -1.095351912296000041 ) ) ;
#45351 = CARTESIAN_POINT ( 'NONE',  ( -3.276646979637814372, -79.49970999519690906, 10.24253291459318582 ) ) ;
#45352 = B_SPLINE_CURVE_WITH_KNOTS ( 'NONE', 3,
 ( #17488, #13640, #8631, #18084, #13046, #26917, #36078, #21337, #109, #12479, #26048, #53505, #39917, #57933, #8053, #31044, #3906, #21908 ),
 .UNSPECIFIED., .F., .F.,
 ( 4, 2, 2, 2, 2, 2, 2, 2, 4 ),
 ( 0.000000000000000000, 0.1249999999999999445, 0.2499999999999998890, 0.3749999999999998335, 0.4999999999999997780, 0.6249999999999997780, 0.7499999999999997780, 0.8749999999999997780, 1.000000000000000000 ),
 .UNSPECIFIED. ) ;
#45353 = EDGE_CURVE ( 'NONE', #21333, #47059, #33420, .T. ) ;
#45354 = CARTESIAN_POINT ( 'NONE',  ( -7.610716808857792337, -60.32015489447598355, -10.41172350879243780 ) ) ;
#45355 = CARTESIAN_POINT ( 'NONE',  ( 12.75761570870000128, -19.22180874373999870, -1.931043762602999925 ) ) ;
#45356 = ORIENTED_EDGE ( 'NONE', *, *, #18492, .T. ) ;
#45357 = DIRECTION ( 'NONE',  ( -1.000000000000000000, 0.000000000000000000, 0.000000000000000000 ) ) ;
#45358 = CARTESIAN_POINT ( 'NONE',  ( -1.221962791321999919, -81.33873264782599222, -0.7004284825205000509 ) ) ;
#45359 = CARTESIAN_POINT ( 'NONE',  ( 2.426647618366999603E-14, -5.949999999936550488, 0.000000000000000000 ) ) ;
#45360 = TOROIDAL_SURFACE ( 'NONE', #24620, 17.50000000000000000, 5.000000000000000000 ) ;
#45361 = CARTESIAN_POINT ( 'NONE',  ( -8.606866362194999454, -77.99211384739999176, -4.073355822332000109 ) ) ;
#45363 = CARTESIAN_POINT ( 'NONE',  ( -1.180494763713999973, -0.6845217200523000534, 3.461421590595000097 ) ) ;
#45362 = CARTESIAN_POINT ( 'NONE',  ( 3.031414438364000041, -83.71250737700098909, -2.870563787844999659 ) ) ;
#45364 = CARTESIAN_POINT ( 'NONE',  ( -1.930989144707000005, -58.55365779174999830, -12.80900240954000147 ) ) ;
#45365 = CARTESIAN_POINT ( 'NONE',  ( 0.6275421466605000109, -80.49360977560299091, 1.160498354042999836 ) ) ;
#45366 = ORIENTED_EDGE ( 'NONE', *, *, #32927, .T. ) ;
#45367 = CARTESIAN_POINT ( 'NONE',  ( -0.04724284673262602735, -77.22472299400682516, -10.74995637182052022 ) ) ;
#45368 = CARTESIAN_POINT ( 'NONE',  ( 11.36512682855729572, -79.07683455540997386, 3.982123233433208398 ) ) ;
#45369 = AXIS2_PLACEMENT_3D ( 'NONE', #18831, #46591, #41549 ) ;
#45370 = CARTESIAN_POINT ( 'NONE',  ( 3.851650068367000745, -78.96264283715741783, 7.703300136734033465 ) ) ;
#45371 = ORIENTED_EDGE ( 'NONE', *, *, #4364, .T. ) ;
#45373 = EDGE_CURVE ( 'NONE', #12448, #10446, #39109, .T. ) ;
#45372 = VERTEX_POINT ( 'NONE', #48841 ) ;
#45374 = CARTESIAN_POINT ( 'NONE',  ( -5.246265831776000255, -79.79077097150499753, -10.82514862071000117 ) ) ;
#45375 = LINE ( 'NONE', #45079, #47253 ) ;
#45376 = B_SPLINE_CURVE_WITH_KNOTS ( 'NONE', 3,
 ( #45, #5022, #49910, #629, #17728, #31273, #26857, #14160, #338, #45186, #39855, #18612, #36600, #18020, #22734, #9745, #49617, #40745, #49021 ),
 .UNSPECIFIED., .F., .F.,
 ( 4, 1, 1, 1, 1, 1, 1, 1, 1, 1, 1, 1, 1, 1, 1, 1, 4 ),
 ( 0.000000000000000000, 0.04500236217446485637, 0.1100020431571605006, 0.1750017241396574219, 0.2400014051223532952, 0.3050010861050493904, 0.3700007670877452637, 0.4350004480702421850, 0.5000001290529377806, 0.5649998100356339314, 0.6299994910183297492, 0.6949991720008267260, 0.7599988529835225437, 0.8249985339662186945, 0.8899982149487153382, 0.9549978959314112670, 1.000000000000000000 ),
 .UNSPECIFIED. ) ;
#45377 = CARTESIAN_POINT ( 'NONE',  ( -0.03447279853675288414, -80.37527479222850957, 10.79553698213345925 ) ) ;
#45378 = EDGE_LOOP ( 'NONE', ( #46908, #7059, #2254, #44560, #25768, #30700 ) ) ;
#45379 = CARTESIAN_POINT ( 'NONE',  ( 6.071186539538999227, -78.02411607459599452, 10.40848046910999791 ) ) ;
#45380 = ORIENTED_EDGE ( 'NONE', *, *, #18116, .F. ) ;
#45381 = ORIENTED_EDGE ( 'NONE', *, *, #53262, .T. ) ;
#45382 = CARTESIAN_POINT ( 'NONE',  ( -1.960246996891127136, -2.673871147968344353, -2.594988089372104678 ) ) ;
#45383 = EDGE_CURVE ( 'NONE', #8467, #28197, #11094, .T. ) ;
#45384 = B_SPLINE_CURVE_WITH_KNOTS ( 'NONE', 3,
 ( #6391, #51285, #7267, #33539, #2557, #29111, #56571, #16130, #43000, #24977, #51863, #10839, #6975, #25268, #55402, #46864, #51576, #14949, #56286 ),
 .UNSPECIFIED., .F., .F.,
 ( 4, 1, 1, 1, 1, 1, 1, 1, 1, 1, 1, 1, 1, 1, 1, 1, 4 ),
 ( 0.000000000000000000, 0.01250073040970592873, 0.04500068264926284506, 0.07750063488862506123, 0.1100005871281820868, 0.1425005393677388765, 0.1750004916071013217, 0.2075004438466583334, 0.2400003960862151509, 0.2725003483255775683, 0.3050003005651346077, 0.3375002528046914252, 0.3700002050440538426, 0.4025001572836108821, 0.4350001095231676440, 0.4675000617625301169, 0.5000000000000000000 ),
 .UNSPECIFIED. ) ;
#45385 = CARTESIAN_POINT ( 'NONE',  ( 9.369164850722000892, -23.25000000000000000, 7.601397897754999633 ) ) ;
#45386 = DIRECTION ( 'NONE',  ( 0.000000000000000000, 1.000000000000000000, 0.000000000000000000 ) ) ;
#45387 = EDGE_CURVE ( 'NONE', #38967, #34794, #56767, .T. ) ;
#45388 = ORIENTED_EDGE ( 'NONE', *, *, #54890, .F. ) ;
#45389 = CARTESIAN_POINT ( 'NONE',  ( 1.157512255224546038, -82.81922399004812974, -0.4718293121365144671 ) ) ;
#45390 = COLOUR_RGB ( '', 0.66274510, 0.83137255, 0.94901961) ;
#45391 = ORIENTED_EDGE ( 'NONE', *, *, #12233, .F. ) ;
#45392 = CARTESIAN_POINT ( 'NONE',  ( -0.9503192246700015167, -80.59177414278872220, 0.8489797128931024783 ) ) ;
#45393 = CARTESIAN_POINT ( 'NONE',  ( -11.51732033666299237, -79.79999999999996874, -3.285645309957324844 ) ) ;
#45394 = DIRECTION ( 'NONE',  ( 1.000000000000000000, 0.000000000000000000, 0.000000000000000000 ) ) ;
#45395 = CARTESIAN_POINT ( 'NONE',  ( -7.682331425175999762, -22.76486430425999785, -10.04115011118000211 ) ) ;
#45396 = CARTESIAN_POINT ( 'NONE',  ( -1.165746613897999928E-14, -72.79999999999999716, 0.000000000000000000 ) ) ;
#45397 = CARTESIAN_POINT ( 'NONE',  ( 10.66325342011824162, -76.51486258876667534, -5.043235781625467595 ) ) ;
#45398 = CARTESIAN_POINT ( 'NONE',  ( -5.687706977064001634, -78.06436792976896299, 10.54353137131000118 ) ) ;
#45399 = CARTESIAN_POINT ( 'NONE',  ( -0.7887765935117789784, -78.71827052605868857, -9.221363235537282321 ) ) ;
#45400 = CARTESIAN_POINT ( 'NONE',  ( 9.057366737456000294, -77.34256001420199311, 2.557513664763999994 ) ) ;
#45401 = CARTESIAN_POINT ( 'NONE',  ( -13.98934701867000108, -9.421869816320000979, -1.420930503335999789E-05 ) ) ;
#45402 = DIRECTION ( 'NONE',  ( 1.000000000000000000, 0.000000000000000000, 0.000000000000000000 ) ) ;
#45403 = VECTOR ( 'NONE', #14074, 1000.000000000000000 ) ;
#45404 = CARTESIAN_POINT ( 'NONE',  ( 12.50000000000000000, -60.04999999725999515, -1.750000000000000000 ) ) ;
#45405 = CARTESIAN_POINT ( 'NONE',  ( 9.396085398178598780, -76.60208333333331154, 7.220923959705271677 ) ) ;
#45406 = CARTESIAN_POINT ( 'NONE',  ( -3.964990495786999691, -81.44392549782598678, 1.156440230559000026 ) ) ;
#45407 = AXIS2_PLACEMENT_3D ( 'NONE', #37578, #46467, #33139 ) ;
#45408 = CARTESIAN_POINT ( 'NONE',  ( -12.55485633994999795, -17.84594908780999845, 1.580761757392000089 ) ) ;
#45409 = DIRECTION ( 'NONE',  ( 0.000000000000000000, -1.000000000000000000, 0.000000000000000000 ) ) ;
#45410 = CARTESIAN_POINT ( 'NONE',  ( -0.4450739772391999471, -24.87813214802000061, 12.43586747594999942 ) ) ;
#45411 = CARTESIAN_POINT ( 'NONE',  ( -12.00000000000000888, -79.38958333333330586, 1.570796326794847264 ) ) ;
#45412 = CARTESIAN_POINT ( 'NONE',  ( -0.7058306598777001062, -1.946219782538000098, 3.554007990761999913 ) ) ;
#45413 = CARTESIAN_POINT ( 'NONE',  ( -2.717095171052049007, -78.20482081344383118, -10.43411631404385354 ) ) ;
#45414 = CARTESIAN_POINT ( 'NONE',  ( -1.464549325067485253, -80.86956512251046547, -0.3794217626884464623 ) ) ;
#45415 = CARTESIAN_POINT ( 'NONE',  ( 12.54705830253000087, -61.33699017322999936, -1.287129557046000183 ) ) ;
#45416 = CARTESIAN_POINT ( 'NONE',  ( -1.140226658635634216, -81.53775969004665569, -0.5918896188631093125 ) ) ;
#45417 = CARTESIAN_POINT ( 'NONE',  ( -10.01332852689000141, -23.28056535155999995, -7.654537165468999760 ) ) ;
#45418 = CARTESIAN_POINT ( 'NONE',  ( 1.217465845835394855, -80.72916666666665719, -0.3271848554490981997 ) ) ;
#45419 = CARTESIAN_POINT ( 'NONE',  ( -11.90546970521999981, -77.35370790967400012, 3.009247460619000059 ) ) ;
#45420 = CARTESIAN_POINT ( 'NONE',  ( 0.000000000000000000, -18.75000000000000000, -12.50000000000000000 ) ) ;
#45422 = CARTESIAN_POINT ( 'NONE',  ( -0.5750548074078000171, -79.20554938902999709, 1.295897153995000162 ) ) ;
#45421 = CARTESIAN_POINT ( 'NONE',  ( -0.9218200799623778030, -79.82708333333334849, 1.199500263597266914 ) ) ;
#45423 = CARTESIAN_POINT ( 'NONE',  ( 1.565347158977999920, -82.48777244601899383, -0.6704515100525999527 ) ) ;
#45424 = ORIENTED_EDGE ( 'NONE', *, *, #40760, .F. ) ;
#45425 = CARTESIAN_POINT ( 'NONE',  ( 3.589195565878999794, -85.64082450217398446, 0.03758747758428000046 ) ) ;
#45426 = CARTESIAN_POINT ( 'NONE',  ( 1.803762123692000063, -80.43536808024779816, 10.90775046864000153 ) ) ;
#45427 = B_SPLINE_CURVE_WITH_KNOTS ( 'NONE', 3,
 ( #13346, #22509, #8636, #8933, #40219, #26052 ),
 .UNSPECIFIED., .F., .F.,
 ( 4, 1, 1, 4 ),
 ( 0.000000000000000000, 0.3333333333333000081, 0.6666666666667000474, 1.000000000000000000 ),
 .UNSPECIFIED. ) ;
#45428 = DIRECTION ( 'NONE',  ( 0.000000000000000000, -1.000000000000000000, 0.000000000000000000 ) ) ;
#45429 = CARTESIAN_POINT ( 'NONE',  ( -2.505364920882746205, -84.51979167730389975, 2.363564369234580020 ) ) ;
#45430 = CARTESIAN_POINT ( 'NONE',  ( 12.66315144082999922, -53.62197088156000291, 0.06064144874944999569 ) ) ;
#45431 = CARTESIAN_POINT ( 'NONE',  ( 0.000000000000000000, -63.73717104351998586, 0.000000000000000000 ) ) ;
#45432 = DIRECTION ( 'NONE',  ( -0.3090169943750105119, 0.000000000000000000, -0.9510565162951329921 ) ) ;
#45433 = CARTESIAN_POINT ( 'NONE',  ( -11.75000000000000178, -76.30865979610494776, -1.278660935777401475 ) ) ;
#45434 = CARTESIAN_POINT ( 'NONE',  ( -9.019414221598461623, -61.79291943934574505, 8.666941069244513685 ) ) ;
#45435 = CARTESIAN_POINT ( 'NONE',  ( 10.55923481294568411, -81.00000000000001421, -3.083916981387107459 ) ) ;
#45436 = ORIENTED_EDGE ( 'NONE', *, *, #23726, .F. ) ;
#45437 = CARTESIAN_POINT ( 'NONE',  ( -0.1250341999720060160, -80.61872301050603085, -1.526447402715753965 ) ) ;
#45438 = CARTESIAN_POINT ( 'NONE',  ( 5.743105918089000284, -79.45213998579799863, 7.461884555157999976 ) ) ;
#45439 = LINE ( 'NONE', #45146, #37505 ) ;
#45440 = EDGE_CURVE ( 'NONE', #27909, #12885, #32477, .T. ) ;
#45441 = DIRECTION ( 'NONE',  ( 0.000000000000000000, 1.000000000000000000, 0.000000000000000000 ) ) ;
#45442 = CARTESIAN_POINT ( 'NONE',  ( -12.50745077490000057, -17.00005551713000074, 2.011909873286000185E-09 ) ) ;
#45443 = DIRECTION ( 'NONE',  ( 0.7071067811865474617, 0.000000000000000000, 0.7071067811865474617 ) ) ;
#45444 = ORIENTED_EDGE ( 'NONE', *, *, #16172, .T. ) ;
#45445 = CARTESIAN_POINT ( 'NONE',  ( 0.5770588204160999046, -77.36396459359899325, 11.19704361211000077 ) ) ;
#45446 = CARTESIAN_POINT ( 'NONE',  ( 10.41172477450676581, -60.32013115014468951, -7.610718073431629094 ) ) ;
#45447 = ORIENTED_EDGE ( 'NONE', *, *, #43097, .T. ) ;
#45448 = AXIS2_PLACEMENT_3D ( 'NONE', #14343, #53632, #32340 ) ;
#45449 = ORIENTED_EDGE ( 'NONE', *, *, #46589, .F. ) ;
#45450 = CARTESIAN_POINT ( 'NONE',  ( -10.36292447788999915, -55.59904187545999577, -7.633480004398999874 ) ) ;
#45451 = SURFACE_SIDE_STYLE ('',( #45750 ) ) ;
#45452 = CARTESIAN_POINT ( 'NONE',  ( 1.739862777674999972, -79.25120313159598595, 9.611119481339999382 ) ) ;
#45453 = EDGE_CURVE ( 'NONE', #20866, #16241, #35527, .T. ) ;
#45454 = ORIENTED_EDGE ( 'NONE', *, *, #16182, .T. ) ;
#45455 = CARTESIAN_POINT ( 'NONE',  ( 1.305706480705000061, -76.55770918080399667, 12.28344334786000047 ) ) ;
#45456 = CARTESIAN_POINT ( 'NONE',  ( 0.000000000000000000, -80.79999999999999716, 0.000000000000000000 ) ) ;
#45457 = CARTESIAN_POINT ( 'NONE',  ( 1.261551586316999707, -78.40843473990000234, -0.8742238293381999759 ) ) ;
#45458 = EDGE_LOOP ( 'NONE', ( #36889, #2404, #15169, #42211 ) ) ;
#45459 = CARTESIAN_POINT ( 'NONE',  ( -9.061228178001998756, -77.59409805011499373, -2.837532765875999896 ) ) ;
#45460 = DIRECTION ( 'NONE',  ( 0.7272727272724163194, -0.6863485850246158204, 6.703676227819155323E-07 ) ) ;
#45461 = CARTESIAN_POINT ( 'NONE',  ( 0.9060466714856187931, -80.29006661044611803, -0.8607755742940681465 ) ) ;
#45462 = CARTESIAN_POINT ( 'NONE',  ( 0.000000000000000000, -23.25000000000000000, 12.50000000000000000 ) ) ;
#45463 = CARTESIAN_POINT ( 'NONE',  ( -3.407095545933000569, -78.62148121115865251, -2.652612342793000192E-07 ) ) ;
#45464 = CARTESIAN_POINT ( 'NONE',  ( 9.051070938631999852, -77.52936199016376406, 3.499832029064999794 ) ) ;
#45465 = CARTESIAN_POINT ( 'NONE',  ( 8.236271263160999112, -79.88807656218412490, 4.209621724653113795 ) ) ;
#45466 = CARTESIAN_POINT ( 'NONE',  ( -3.960893013548711483, -78.73854164604992434, -0.6456742679201270541 ) ) ;
#45467 = VERTEX_POINT ( 'NONE', #17840 ) ;
#45468 = FACE_OUTER_BOUND ( 'NONE', #19830, .T. ) ;
#45469 = CARTESIAN_POINT ( 'NONE',  ( -3.438348731682000281, -76.65447324480000191, -11.82003900998999946 ) ) ;
#45470 = CARTESIAN_POINT ( 'NONE',  ( -1.511528582562000178, -79.40406894431399110, 0.07582444189424000780 ) ) ;
#45471 = EDGE_CURVE ( 'NONE', #30968, #26684, #8866, .T. ) ;
#45472 = DIRECTION ( 'NONE',  ( 0.000000000000000000, 1.000000000000000000, 0.000000000000000000 ) ) ;
#45473 = CARTESIAN_POINT ( 'NONE',  ( 7.620037246310000789, -60.00567269791999792, -10.53559750860999955 ) ) ;
#45474 = CARTESIAN_POINT ( 'NONE',  ( -1.777672186646999997, -78.90390915793000204, 12.13420648597999829 ) ) ;
#45475 = CARTESIAN_POINT ( 'NONE',  ( -12.00000000000000000, -78.39999999999999147, 0.000000000000000000 ) ) ;
#45476 = CARTESIAN_POINT ( 'NONE',  ( -3.453171399369999950, -1.863032031399000088, -0.5706200895263999762 ) ) ;
#45477 = CARTESIAN_POINT ( 'NONE',  ( 7.581939418254000529, -77.57536498579798945, -6.109555841837000401 ) ) ;
#45478 = CARTESIAN_POINT ( 'NONE',  ( 12.06634091025675204, -77.30042855182080075, 0.05712547007327853366 ) ) ;
#45479 = CARTESIAN_POINT ( 'NONE',  ( 9.050966799188000067, -55.64999999964999233, 7.919595949288999570 ) ) ;
#45480 = EDGE_LOOP ( 'NONE', ( #15311, #45674, #1738, #46332 ) ) ;
#45481 = CARTESIAN_POINT ( 'NONE',  ( -1.331776743724000234, -83.47447248197899228, -0.3115240295706999674 ) ) ;
#45482 = CARTESIAN_POINT ( 'NONE',  ( -0.9994823880747228939, -78.65231536704800419, -0.7681904385035477345 ) ) ;
#45483 = CARTESIAN_POINT ( 'NONE',  ( -0.7681833999686477066, -79.42708333333332860, 0.9995835529977223910 ) ) ;
#45484 = VECTOR ( 'NONE', #28158, 1000.000000000000000 ) ;
#45485 = DIRECTION ( 'NONE',  ( 0.000000000000000000, -1.000000000000000000, 0.000000000000000000 ) ) ;
#45486 = CARTESIAN_POINT ( 'NONE',  ( -5.088691759813757095E-08, -76.94999999999998863, -9.499908983443795307 ) ) ;
#45487 = EDGE_CURVE ( 'NONE', #34323, #34669, #44114, .T. ) ;
#45488 = CARTESIAN_POINT ( 'NONE',  ( 1.644133925033999910, -78.87275712511198833, 11.70364056775000172 ) ) ;
#45489 = CARTESIAN_POINT ( 'NONE',  ( 7.920136950582000068, -77.86314805011500084, 4.778486233528999705 ) ) ;
#45490 = CARTESIAN_POINT ( 'NONE',  ( 4.155310858692000231, -78.36743808823698032, -8.688302574878001394 ) ) ;
#45491 = CARTESIAN_POINT ( 'NONE',  ( 3.155060921293558085, -76.05290718790978133, 11.32013784086210961 ) ) ;
#45492 = CARTESIAN_POINT ( 'NONE',  ( 8.325251318307000048, -80.22061154526829796, -7.061554902978000037 ) ) ;
#45493 = CARTESIAN_POINT ( 'NONE',  ( 3.200957065930545742, -86.02148120184399716, 2.324951338796139133 ) ) ;
#45494 = VERTEX_POINT ( 'NONE', #6293 ) ;
#45495 = FACE_OUTER_BOUND ( 'NONE', #13352, .T. ) ;
#45496 = CIRCLE ( 'NONE', #5901, 0.5000000000000004441 ) ;
#45497 = CARTESIAN_POINT ( 'NONE',  ( -0.03630073495416798190, -78.43735716284258785, -3.851479002382501182 ) ) ;
#45498 = CARTESIAN_POINT ( 'NONE',  ( -9.393203674808288994, -77.45833333333330017, 5.413904038987134015 ) ) ;
#45499 = CARTESIAN_POINT ( 'NONE',  ( 0.9090372547675998893, -78.85885595378398705, 10.93790052299999971 ) ) ;
#45500 = FACE_OUTER_BOUND ( 'NONE', #55574, .T. ) ;
#45501 = CARTESIAN_POINT ( 'NONE',  ( -12.08282522424999961, -75.86276683616600280, 1.641596703183000105 ) ) ;
#45502 = FACE_OUTER_BOUND ( 'NONE', #52280, .T. ) ;
#45503 = CARTESIAN_POINT ( 'NONE',  ( 7.634437838915999919, -18.25219468451000182, -10.30764259110000047 ) ) ;
#45504 = VERTEX_POINT ( 'NONE', #37875 ) ;
#45506 = VECTOR ( 'NONE', #1352, 1000.000000000000000 ) ;
#45505 = CARTESIAN_POINT ( 'NONE',  ( 9.995598443669999611, -78.92237613279000641, -4.933823296771000955 ) ) ;
#45507 = CARTESIAN_POINT ( 'NONE',  ( 12.70255494774207961, -17.25391159036992050, 1.306413223736588858 ) ) ;
#45508 = CARTESIAN_POINT ( 'NONE',  ( 12.50728617048449465, -53.80024476432964065, 0.1757991156898129625 ) ) ;
#45509 = CARTESIAN_POINT ( 'NONE',  ( -0.03630051165549490200, -78.43735716284258785, 3.851479004487115443 ) ) ;
#45510 = AXIS2_PLACEMENT_3D ( 'NONE', #29195, #34192, #7920 ) ;
#45511 = ADVANCED_FACE ( 'NONE', ( #46770 ), #28718, .F. ) ;
#45512 = CARTESIAN_POINT ( 'NONE',  ( 11.45098972023387240, -76.43180119005340600, -2.636752081925491265 ) ) ;
#45513 = CARTESIAN_POINT ( 'NONE',  ( -9.152236916771000708, -78.75961649866798098, 6.189866966782000546 ) ) ;
#45514 = EDGE_CURVE ( 'NONE', #6488, #4486, #43374, .T. ) ;
#45515 = CARTESIAN_POINT ( 'NONE',  ( -9.875985572401248191, -76.46666666666662593, 4.392572548563077994 ) ) ;
#45516 = LINE ( 'NONE', #1232, #36498 ) ;
#45517 = LINE ( 'NONE', #54370, #28059 ) ;
#45518 = CARTESIAN_POINT ( 'NONE',  ( -10.75000000000000000, -79.50000000000000000, 0.000000000000000000 ) ) ;
#45519 = CARTESIAN_POINT ( 'NONE',  ( 0.5437984056370215313, -79.57105364439701134, 11.05137384886683094 ) ) ;
#45520 = SURFACE_SIDE_STYLE ('',( #52911 ) ) ;
#45521 = CARTESIAN_POINT ( 'NONE',  ( -12.66001556632000025, -24.63260856943000121, 1.381621105852999909 ) ) ;
#45522 = ORIENTED_EDGE ( 'NONE', *, *, #4777, .F. ) ;
#45523 = EDGE_CURVE ( 'NONE', #51133, #47356, #51398, .T. ) ;
#45524 = EDGE_LOOP ( 'NONE', ( #49868, #19964, #17111, #53602 ) ) ;
#45525 = CARTESIAN_POINT ( 'NONE',  ( 8.024414491358506041, -78.79212767763318936, -7.157144857178496800 ) ) ;
#45526 = CARTESIAN_POINT ( 'NONE',  ( 5.657431823768000356, -76.80693998579801018, -7.274622582025999762 ) ) ;
#45527 = AXIS2_PLACEMENT_3D ( 'NONE', #38051, #43353, #2913 ) ;
#45528 = EDGE_LOOP ( 'NONE', ( #34516, #6671, #23854 ) ) ;
#45529 = FACE_OUTER_BOUND ( 'NONE', #11539, .T. ) ;
#45530 = CARTESIAN_POINT ( 'NONE',  ( 7.753906807039999904, -24.28933445982999828, 10.31979621049999807 ) ) ;
#45531 = CARTESIAN_POINT ( 'NONE',  ( 7.622785526051999661, -60.58712283452999259, 10.47836401508999948 ) ) ;
#45532 = CARTESIAN_POINT ( 'NONE',  ( 4.494525810343096950, -77.20555113919044743, -10.87989057085453837 ) ) ;
#45533 = CARTESIAN_POINT ( 'NONE',  ( 6.445068773528756623, -77.72010726321535401, -10.09856820804314381 ) ) ;
#45534 = AXIS2_PLACEMENT_3D ( 'NONE', #28902, #42499, #46948 ) ;
#45535 = CARTESIAN_POINT ( 'NONE',  ( 11.15679540746000065, -79.52434518398199259, 1.159321710118000004 ) ) ;
#45536 = CARTESIAN_POINT ( 'NONE',  ( 1.814076166948946689, -79.40950282387937875, 9.381557441920369556 ) ) ;
#45537 = ORIENTED_EDGE ( 'NONE', *, *, #11017, .F. ) ;
#45538 = CARTESIAN_POINT ( 'NONE',  ( -10.42531125068999920, -23.26485145404000221, 7.624341767093000044 ) ) ;
#45539 = ORIENTED_EDGE ( 'NONE', *, *, #30024, .T. ) ;
#45540 = CARTESIAN_POINT ( 'NONE',  ( -1.534489406528057431, -77.48831705290680816, 9.121860746232874462 ) ) ;
#45541 = CARTESIAN_POINT ( 'NONE',  ( 3.792698199283999649, -78.02275488312699281, -10.36819406884000117 ) ) ;
#45542 = DIRECTION ( 'NONE',  ( 0.7071067811865475727, 0.000000000000000000, -0.7071067811865475727 ) ) ;
#45543 = CARTESIAN_POINT ( 'NONE',  ( -4.814859605045999302, -78.80676906851299179, 8.425427962446999430 ) ) ;
#45544 = AXIS2_PLACEMENT_3D ( 'NONE', #494, #10488, #23187 ) ;
#45545 = CARTESIAN_POINT ( 'NONE',  ( -12.96570439747000059, -75.91866156851000369, -0.01980505094338999919 ) ) ;
#45546 = FACE_OUTER_BOUND ( 'NONE', #50379, .T. ) ;
#45547 = CARTESIAN_POINT ( 'NONE',  ( 0.1198033158700999995, -79.19874496458000124, 1.623056241665000066 ) ) ;
#45548 = DIRECTION ( 'NONE',  ( 2.505275680394999719E-13, -1.000000000000000000, -2.029755673547999903E-12 ) ) ;
#45549 = CARTESIAN_POINT ( 'NONE',  ( 8.185910223524000884, -78.12337145011899509, -6.914387615432000977 ) ) ;
#45550 = CARTESIAN_POINT ( 'NONE',  ( -7.631889049354000143, -23.22121504852000129, -10.36222434949000082 ) ) ;
#45551 = CARTESIAN_POINT ( 'NONE',  ( -7.997114030248268612, -60.48581381147864988, 7.553727747482917643 ) ) ;
#45552 = CARTESIAN_POINT ( 'NONE',  ( -2.845775103139000173, -82.99100488540000242, 2.113417919158000036 ) ) ;
#45553 = ORIENTED_EDGE ( 'NONE', *, *, #50627, .F. ) ;
#45554 = CARTESIAN_POINT ( 'NONE',  ( 3.562868568952000548, -79.72528206836099685, 11.91204729721000000 ) ) ;
#45555 = CARTESIAN_POINT ( 'NONE',  ( -5.857867859648000497, -76.12642014291699866, 9.889045732754000895 ) ) ;
#45556 = CARTESIAN_POINT ( 'NONE',  ( -1.272095873948303257, -77.98448913755433409, 10.68035095373946675 ) ) ;
#45557 = CARTESIAN_POINT ( 'NONE',  ( -11.74098051674999965, -78.61797745361100453, 2.380218674853999961 ) ) ;
#45558 = DIRECTION ( 'NONE',  ( 0.000000000000000000, -1.000000000000000000, 0.000000000000000000 ) ) ;
#45559 = ADVANCED_FACE ( 'NONE', ( #9565 ), #55013, .F. ) ;
#45561 = CARTESIAN_POINT ( 'NONE',  ( 12.50000000000000000, -60.24678171298000251, 1.250000000000000000 ) ) ;
#45560 = CARTESIAN_POINT ( 'NONE',  ( -1.750000000001000089, -60.05000000958000328, -12.56594317859000043 ) ) ;
#45562 = LINE ( 'NONE', #13950, #32685 ) ;
#45563 = CARTESIAN_POINT ( 'NONE',  ( 1.664903097754173888, -80.96299215033094754, 10.62006420670805973 ) ) ;
#45564 = CARTESIAN_POINT ( 'NONE',  ( -1.146763852601999867, -78.69446787273398058, -9.343239705575001608 ) ) ;
#45565 = CARTESIAN_POINT ( 'NONE',  ( -3.647699722740957995, -86.02148118236289065, 1.624060551956000520 ) ) ;
#45566 = CARTESIAN_POINT ( 'NONE',  ( 0.2611009988843999707, -78.58574720659700574, -11.02876811737000118 ) ) ;
#45567 = CYLINDRICAL_SURFACE ( 'NONE', #29044, 12.50000000000000000 ) ;
#45568 = CARTESIAN_POINT ( 'NONE',  ( 4.284808111760000315, -80.54755208664988686, -10.28385259334999979 ) ) ;
#45569 = VERTEX_POINT ( 'NONE', #37581 ) ;
#45570 = CARTESIAN_POINT ( 'NONE',  ( 0.000000000000000000, -74.64999999999999147, 0.000000000000000000 ) ) ;
#45571 = CARTESIAN_POINT ( 'NONE',  ( -5.597970637881999778, -77.07517403538302858, 7.669424558767000022 ) ) ;
#45572 = CARTESIAN_POINT ( 'NONE',  ( -10.11462613662204468, -23.38712935484990751, 7.639894945624773115 ) ) ;
#45573 = CARTESIAN_POINT ( 'NONE',  ( -3.244487197725999916, -76.79996563637499207, -10.73738397614000029 ) ) ;
#45574 = CARTESIAN_POINT ( 'NONE',  ( 11.00000000000000711, -79.93958333333333144, -1.439896632895300010 ) ) ;
#45575 = CIRCLE ( 'NONE', #38005, 0.5000000000000004441 ) ;
#45576 = CARTESIAN_POINT ( 'NONE',  ( 7.633501923154999425, -23.20104675770999947, -10.36289748052999826 ) ) ;
#45577 = CARTESIAN_POINT ( 'NONE',  ( -7.624341766639000539, -23.26485146254000114, -10.42531125024000005 ) ) ;
#45578 = CARTESIAN_POINT ( 'NONE',  ( 11.00000000000000000, -79.94999999999998863, 0.000000000000000000 ) ) ;
#45579 = CARTESIAN_POINT ( 'NONE',  ( 12.70926961119000076, -18.59159259619999816, 1.933875435151000133 ) ) ;
#45580 = CARTESIAN_POINT ( 'NONE',  ( -1.831549031511999770, -85.91467953870898100, 3.748625133460000036 ) ) ;
#45581 = CARTESIAN_POINT ( 'NONE',  ( -0.5999999999999999778, -5.000000000000000000, 4.000000000000000000 ) ) ;
#45582 = VECTOR ( 'NONE', #25406, 1000.000000000000114 ) ;
#45583 = CARTESIAN_POINT ( 'NONE',  ( 10.53559655342999868, -55.59430957992999822, -7.620036381585000740 ) ) ;
#45584 = B_SPLINE_SURFACE_WITH_KNOTS ( 'NONE', 3, 3, ( 
 ( #47274, #1813, #11245, #6215, #42536, #29224, #50525, #33656, #46106, #19223, #10668, #33069, #51114, #1234, #24230, #55525, #15072, #33368, #10079, #28646, #46696, #37215, #10958, #24521, #949, #10363, #28350, #28060, #37803, #23930, #2103, #55228, #5630, #56114, #6803 ),
 ( #23642, #51697, #41655, #14775, #42249, #19810, #55823, #46398, #20102, #38093, #24811, #18934, #23146, #8992, #16255, #34233, #21247, #30670, #43125, #47576, #39250, #38966, #30090, #29800, #16540, #34520, #57265, #12393, #52552, #12107, #30383, #7962, #21538, #39543, #17109 ),
 ( #12678, #8250, #26252, #23296, #50177, #9138, #27423, #12958, #27123, #35690, #31247, #30954, #27711, #31845, #32136, #5288, #4713, #9722, #41304, #45457, #45755, #41015, #44859, #40724, #889, #49289, #18873, #9433, #13554, #40122, #18294, #8840, #607, #18, #4999 ),
 ( #53409, #22113, #18587, #35988, #26830, #48993, #23004, #8539, #17997, #13255, #36577, #54600, #4411, #54013, #26532, #44559, #4112, #58135, #49887, #36288, #17701, #14137, #53717, #22414, #40427, #31546, #49592, #45163, #22711, #316, #54310, #13848, #37450, #10605, #10312 ) ),
 .UNSPECIFIED., .F., .F., .F.,
 ( 4, 4 ),
 ( 4, 1, 1, 1, 1, 1, 1, 1, 1, 1, 1, 1, 1, 1, 1, 1, 1, 1, 1, 1, 1, 1, 1, 1, 1, 1, 1, 1, 1, 1, 1, 1, 4 ),
 ( -0.1331668876848000060, 1.133166887685000068 ),
 ( -0.01660298332971000060, 0.01037686458107000068, 0.03735671249184999848, 0.06433656040262999976, 0.09131640831340999409, 0.1182962562242000082, 0.1452761041350000004, 0.1722559520456999893, 0.1992357999565000093, 0.2262156478673000015, 0.2531954957780999660, 0.2801753436889000137, 0.3071551915995999749, 0.3341350395104000226, 0.3611148874212000148, 0.3880947353320000071, 0.4150745832427999993, 0.4420544311535000159, 0.4690342790643000082, 0.4960141269751000004, 0.5229939748859000481, 0.5499738227967000403, 0.5769536707074000015, 0.6039335186181999937, 0.6309133665289999859, 0.6578932144397999782, 0.6848730623505999704, 0.7118529102612999315, 0.7388327581721000348, 0.7658126060829000270, 0.7927924539937000192, 0.8197723019045000115, 0.8467521498151999726 ),
 .UNSPECIFIED. ) ;
#45585 = CARTESIAN_POINT ( 'NONE',  ( -11.21475409559999825, -76.76929369090099442, 1.031226285144000165 ) ) ;
#45586 = EDGE_CURVE ( 'NONE', #38447, #42021, #10152, .T. ) ;
#45587 = CARTESIAN_POINT ( 'NONE',  ( 1.551146335801999898, -81.05010250687999473, 0.6076261867840000441 ) ) ;
#45588 = CARTESIAN_POINT ( 'NONE',  ( 0.3327358950964000028, -78.66525142865999953, -1.277483743371999880 ) ) ;
#45589 = CARTESIAN_POINT ( 'NONE',  ( -0.5222397218926316809, -61.96298219375309912, 12.70447686588483194 ) ) ;
#45590 = CARTESIAN_POINT ( 'NONE',  ( -0.4470518900855922073, -83.14878330911811588, 1.443941350861193129 ) ) ;
#45591 = CARTESIAN_POINT ( 'NONE',  ( -12.54977961489000116, -61.84832888596000089, -0.03757501521675000317 ) ) ;
#45592 = CARTESIAN_POINT ( 'NONE',  ( -8.058638732054999920, -78.40938521931758487, -7.451332657186999775 ) ) ;
#45593 = CARTESIAN_POINT ( 'NONE',  ( 12.76303204517000012, -18.73514852243999940, -1.980584515753000208 ) ) ;
#45594 = AXIS2_PLACEMENT_3D ( 'NONE', #34573, #44032, #21298 ) ;
#45595 = EDGE_LOOP ( 'NONE', ( #1316, #38826, #35774, #1383 ) ) ;
#45596 = AXIS2_PLACEMENT_3D ( 'NONE', #4394, #40405, #13533 ) ;
#45597 = CARTESIAN_POINT ( 'NONE',  ( 9.019406120300617502, -53.80707871034709200, 8.666949038527242521 ) ) ;
#45598 = FACE_BOUND ( 'NONE', #52131, .T. ) ;
#45599 = CARTESIAN_POINT ( 'NONE',  ( -4.126717922116999837, -79.48595787040198957, -10.35494083817999922 ) ) ;
#45600 = DIRECTION ( 'NONE',  ( 0.7592504788686188499, -0.04890177850593128983, 0.6489586476785169644 ) ) ;
#45601 = ORIENTED_EDGE ( 'NONE', *, *, #30799, .T. ) ;
#45602 = EDGE_CURVE ( 'NONE', #14201, #14108, #10859, .T. ) ;
#45603 = EDGE_LOOP ( 'NONE', ( #21815, #7178, #52415, #50244 ) ) ;
#45604 = DIRECTION ( 'NONE',  ( -1.000000000000000000, 0.000000000000000000, 0.000000000000000000 ) ) ;
#45605 = EDGE_CURVE ( 'NONE', #7477, #35380, #7520, .T. ) ;
#45606 = ORIENTED_EDGE ( 'NONE', *, *, #3241, .T. ) ;
#45607 = ORIENTED_EDGE ( 'NONE', *, *, #4587, .T. ) ;
#45608 = PLANE ( 'NONE',  #39610 ) ;
#45609 = DIRECTION ( 'NONE',  ( -1.000000000000000000, 0.000000000000000000, 0.000000000000000000 ) ) ;
#45610 = CARTESIAN_POINT ( 'NONE',  ( 1.750000000001000089, -56.04899163641999849, 12.60354432391000046 ) ) ;
#45611 = CARTESIAN_POINT ( 'NONE',  ( 1.798954018882000128, -23.21530973387000074, -12.61117007302000026 ) ) ;
#45612 = CARTESIAN_POINT ( 'NONE',  ( -2.650649970517000131, -81.81671231080099460, 2.661846198621000248 ) ) ;
#45613 = DIRECTION ( 'NONE',  ( 0.07798810159604831205, 0.04890177472412891857, -0.9957542229075783125 ) ) ;
#45614 = CARTESIAN_POINT ( 'NONE',  ( -7.299466235464000086, -78.25818391050999878, 9.602332031690000491 ) ) ;
#45615 = ORIENTED_EDGE ( 'NONE', *, *, #9126, .F. ) ;
#45616 = ORIENTED_EDGE ( 'NONE', *, *, #4113, .T. ) ;
#45617 = DIRECTION ( 'NONE',  ( 0.000000000000000000, 1.000000000000000000, -8.313948728910000322E-11 ) ) ;
#45618 = DIRECTION ( 'NONE',  ( -0.3090169943748909964, 0.000000000000000000, 0.9510565162951718499 ) ) ;
#45619 = CARTESIAN_POINT ( 'NONE',  ( -3.600000000000000089, -0.2000000000000000111, 0.000000000000000000 ) ) ;
#45620 = CARTESIAN_POINT ( 'NONE',  ( -0.5668640725916784806, -17.08340305018563399, 12.50470739227127304 ) ) ;
#45621 = CARTESIAN_POINT ( 'NONE',  ( 4.186942200393000135, -78.37004582933998620, -8.754440266352000677 ) ) ;
#45622 = ADVANCED_FACE ( 'NONE', ( #20175, #47347 ), #47927, .F. ) ;
#45623 = FACE_OUTER_BOUND ( 'NONE', #17993, .T. ) ;
#45624 = CARTESIAN_POINT ( 'NONE',  ( -10.24998526317999925, -20.24916621771999914, 7.705142895619999877 ) ) ;
#45625 = CARTESIAN_POINT ( 'NONE',  ( -3.148725677322000482, -77.72624008069000467, 12.40542962523000092 ) ) ;
#45626 = CARTESIAN_POINT ( 'NONE',  ( 1.149971879181999945, -79.78602897879000011, -0.7096026395132000175 ) ) ;
#45627 = CARTESIAN_POINT ( 'NONE',  ( -12.53239398059000109, -22.76486430425999785, -1.667936688463999895 ) ) ;
#45628 = CARTESIAN_POINT ( 'NONE',  ( 9.722718241315000398, -23.25000000000000000, 7.247844507162001015 ) ) ;
#45629 = CARTESIAN_POINT ( 'NONE',  ( -3.741325830153999998, -80.29693765374598513, -1.847309861237000028 ) ) ;
#45630 = CARTESIAN_POINT ( 'NONE',  ( -6.711381441964999972, -80.19189216818548971, 9.048015653393999713 ) ) ;
#45631 = CARTESIAN_POINT ( 'NONE',  ( -12.00000000000000355, -76.78958333333331154, 1.570796326794848596 ) ) ;
#45632 = CARTESIAN_POINT ( 'NONE',  ( 0.000000000000000000, -75.15999999999999659, 0.000000000000000000 ) ) ;
#45633 = CARTESIAN_POINT ( 'NONE',  ( -2.658539373363999925, -81.89157046129098205, -2.348769664634999810 ) ) ;
#45634 = EDGE_CURVE ( 'NONE', #38307, #36279, #38144, .T. ) ;
#45635 = CARTESIAN_POINT ( 'NONE',  ( -0.1765672563250000049, -78.33632026758570532, -1.321892640673999919 ) ) ;
#45636 = PLANE ( 'NONE',  #14739 ) ;
#45637 = FACE_OUTER_BOUND ( 'NONE', #14508, .T. ) ;
#45638 = CARTESIAN_POINT ( 'NONE',  ( -2.963791440107999886, -3.298030605495000156, 2.387889716789000083 ) ) ;
#45639 = CARTESIAN_POINT ( 'NONE',  ( -0.9995835529977249445, -79.05208333333331439, -0.7681833999686439318 ) ) ;
#45640 = EDGE_CURVE ( 'NONE', #18023, #3036, #27889, .T. ) ;
#45641 = VERTEX_POINT ( 'NONE', #13022 ) ;
#45642 = CYLINDRICAL_SURFACE ( 'NONE', #21558, 11.75000000000000000 ) ;
#45643 = CARTESIAN_POINT ( 'NONE',  ( -0.5812841321855997112, -18.69583131523479480, -10.98463311464191605 ) ) ;
#45644 = DIRECTION ( 'NONE',  ( -0.7071067811865475727, 0.000000000000000000, -0.7071067811865475727 ) ) ;
#45645 = CARTESIAN_POINT ( 'NONE',  ( -0.2317941695893000198, -82.37581864516299390, -1.228320586388000013 ) ) ;
#45646 = CARTESIAN_POINT ( 'NONE',  ( 1.799502287691000069, -60.10716680829000325, 12.60413670423000099 ) ) ;
#45647 = CARTESIAN_POINT ( 'NONE',  ( -10.55511172854000002, -77.96761847984998894, 7.611100925114999249 ) ) ;
#45648 = CARTESIAN_POINT ( 'NONE',  ( -3.053122078541150142, -79.49795925471170221, 10.30883018202370671 ) ) ;
#45649 = CARTESIAN_POINT ( 'NONE',  ( -9.346069275187129932, -61.96527745658262631, -8.620894635752145874 ) ) ;
#45650 = CARTESIAN_POINT ( 'NONE',  ( 0.000000000000000000, -76.19999999999998863, -9.749999999999667821 ) ) ;
#45651 = ORIENTED_EDGE ( 'NONE', *, *, #39073, .T. ) ;
#45652 = CARTESIAN_POINT ( 'NONE',  ( -8.666912951382961694, -24.99291380871171597, -9.019442093130059845 ) ) ;
#45653 = CARTESIAN_POINT ( 'NONE',  ( 10.26236580194999881, -77.96083789290199206, -4.398705269624000103 ) ) ;
#45654 = CARTESIAN_POINT ( 'NONE',  ( -1.155705185623000064, -82.27088077809300160, -0.4398327176956999818 ) ) ;
#45655 = CARTESIAN_POINT ( 'NONE',  ( 7.678667886068000215, -20.24263462181000151, -10.59548767699999949 ) ) ;
#45656 = CARTESIAN_POINT ( 'NONE',  ( -8.431119552239000114, -78.41847128433398950, 4.425675013809000191 ) ) ;
#45658 = CARTESIAN_POINT ( 'NONE',  ( -3.858199361241999803, -0.7704335234539000377, -1.117275487237999965 ) ) ;
#45657 = CARTESIAN_POINT ( 'NONE',  ( 2.266606191906000323, -85.15551236020199610, -3.506010019137000278 ) ) ;
#45659 = FACE_OUTER_BOUND ( 'NONE', #56904, .T. ) ;
#45660 = CARTESIAN_POINT ( 'NONE',  ( -1.500000000000000888, -81.48958333333335702, 0.1963495408493559080 ) ) ;
#45661 = ORIENTED_EDGE ( 'NONE', *, *, #11379, .F. ) ;
#45662 = AXIS2_PLACEMENT_3D ( 'NONE', #9907, #5469, #41484 ) ;
#45663 = CARTESIAN_POINT ( 'NONE',  ( -2.429273012391383268, -77.20702660129524020, -10.47182961545118651 ) ) ;
#45664 = LINE ( 'NONE', #23492, #53028 ) ;
#45665 = CARTESIAN_POINT ( 'NONE',  ( 3.778552491321000240, -78.99318692756679638, -4.627392213906519702E-16 ) ) ;
#45666 = ORIENTED_EDGE ( 'NONE', *, *, #23990, .F. ) ;
#45667 = VERTEX_POINT ( 'NONE', #49354 ) ;
#45668 = CARTESIAN_POINT ( 'NONE',  ( -9.839875214663999614, -79.83481699542699062, 4.781661263485999847 ) ) ;
#45669 = LINE ( 'NONE', #13758, #11420 ) ;
#45670 = CYLINDRICAL_SURFACE ( 'NONE', #56735, 1.000000000000000000 ) ;
#45671 = ORIENTED_EDGE ( 'NONE', *, *, #58265, .F. ) ;
#45672 = B_SPLINE_CURVE_WITH_KNOTS ( 'NONE', 3,
 ( #15008, #27415, #55166, #5566, #23575, #45747, #51049, #10596, #4992, #5282, #23289, #41009, #50759, #36860, #28581, #41299, #32130, #46625, #19744, #19158, #6155, #24163, #14709, #32707, #42180, #37738, #47502, #56051, #20608, #33875, #51914, #29732, #46917, #42764, #6444, #24461, #11475, #16469, #28872, #43624, #29445, #33594, #20321, #20887, #34161, #42473, #56913, #47783, #43334, #43050, #7029, #38609, #25031, #52198, #2612, #2041, #2325, #2891, #24748, #38892, #33300, #56622, #29163, #25318, #3188, #16183, #11753, #30020, #34451, #7314, #15307, #52483, #56337, #12040, #51633, #48075, #7603, #55761, #47210, #6739, #51337, #21176, #25603, #10896, #20042, #38030, #15600, #11186, #38317, #15890, #14282, #25890, #58291, #49744, #13702, #31697, #39475, #4862, #18147, #36145, #13993, #34739, #30310, #9285, #39179 ),
 .UNSPECIFIED., .F., .F.,
 ( 4, 2, 2, 2, 2, 1, 1, 2, 2, 2, 2, 2, 2, 2, 1, 2, 2, 2, 2, 2, 1, 1, 1, 2, 2, 2, 1, 1, 1, 2, 2, 2, 2, 2, 2, 2, 2, 2, 1, 1, 2, 2, 2, 1, 1, 1, 2, 2, 2, 2, 2, 2, 2, 2, 1, 1, 1, 2, 2, 2, 4 ),
 ( 0.000000000000000000, 0.03124999999997688654, 0.04687499999996567329, 0.06249999999995446698, 0.09374999999993136046, 0.1093749999999194672, 0.1171874999999131528, 0.1210937499999096278, 0.1249999999999061029, 0.1562499999998830935, 0.1718749999998716582, 0.1874999999998602229, 0.2187499999998378242, 0.2343749999998269717, 0.2421874999998215316, 0.2460937499998188116, 0.2499999999998160916, 0.3124999999997497557, 0.3437499999997168376, 0.3593749999997004063, 0.3671874999996924127, 0.3710937499996884159, 0.3730468749996864175, 0.3740234374996853628, 0.3749999999996843081, 0.4062499999996578848, 0.4218749999996443956, 0.4296874999996373456, 0.4335937499996337929, 0.4355468749996320166, 0.4374999999996302402, 0.4687499999996005973, 0.4843749999995854982, 0.4921874999995774491, 0.4999999999995694000, 0.5624999999995077271, 0.5937499999994767519, 0.6093749999994613198, 0.6171874999994536592, 0.6210937499994495514, 0.6230468749994475530, 0.6249999999994455546, 0.6562499999994138022, 0.6718749999993975930, 0.6796874999993898214, 0.6835937499993859356, 0.6855468749993842703, 0.6874999999993826050, 0.7187499999993595123, 0.7343749999993479660, 0.7499999999993364197, 0.8124999999992913446, 0.8437499999992684740, 0.8593749999992571498, 0.8671874999992511546, 0.8710937499992481570, 0.8730468749992466027, 0.8740234374992456035, 0.8749999999992447153, 0.9374999999996223021, 1.000000000000000000 ),
 .UNSPECIFIED. ) ;
#45673 = CARTESIAN_POINT ( 'NONE',  ( -5.720894519599999839, -78.10550402086698796, 10.60505245481999914 ) ) ;
#45674 = ORIENTED_EDGE ( 'NONE', *, *, #52301, .T. ) ;
#45675 = B_SPLINE_CURVE_WITH_KNOTS ( 'NONE', 3,
 ( #52590, #12140, #57301, #52875, #56152, #6551, #20142, #20427, #38129, #24851, #6840, #15701, #33695, #51734, #42866, #2424, #56440, #33982, #15994, #50, #57581, #8283, #8575, #18026 ),
 .UNSPECIFIED., .F., .F.,
 ( 4, 2, 2, 2, 2, 2, 2, 2, 2, 2, 2, 4 ),
 ( 0.000000000000000000, 0.06249999999999991673, 0.1249999999999998335, 0.1874999999999997780, 0.2499999999999997224, 0.3749999999999997224, 0.4999999999999997780, 0.6249999999999997780, 0.7499999999999998890, 0.8749999999999998890, 0.9375000000000000000, 1.000000000000000000 ),
 .UNSPECIFIED. ) ;
#45676 = VERTEX_POINT ( 'NONE', #44920 ) ;
#45677 = CARTESIAN_POINT ( 'NONE',  ( -1.605981818850155562, -2.684253276126684629, -2.834025076496387463 ) ) ;
#45678 = CARTESIAN_POINT ( 'NONE',  ( -8.538789269653864977, -76.46197650723648565, -8.538663626634152237 ) ) ;
#45679 = CARTESIAN_POINT ( 'NONE',  ( 9.335966200621838240, -79.16452702242366968, 1.759126508296344760 ) ) ;
#45680 = EDGE_LOOP ( 'NONE', ( #52554, #36015, #8880, #9178 ) ) ;
#45681 = CARTESIAN_POINT ( 'NONE',  ( 0.8852892051488824299, -82.78829553564608545, -0.8819059964711186694 ) ) ;
#45682 = ORIENTED_EDGE ( 'NONE', *, *, #44608, .F. ) ;
#45683 = CARTESIAN_POINT ( 'NONE',  ( -4.657705497668140460, -79.18357720769643038, -8.081617589960574222 ) ) ;
#45684 = CARTESIAN_POINT ( 'NONE',  ( 1.487051409078008701, -77.48714799342995718, -9.589708388838586117 ) ) ;
#45685 = CARTESIAN_POINT ( 'NONE',  ( 3.914500761937000028, -78.91452044229970397, -1.429791614965258972E-15 ) ) ;
#45686 = CARTESIAN_POINT ( 'NONE',  ( 10.01676960210999923, -55.59061945207999855, 7.658895148190000057 ) ) ;
#45687 = ADVANCED_FACE ( 'NONE', ( #12456 ), #32057, .F. ) ;
#45688 = CARTESIAN_POINT ( 'NONE',  ( 11.06808393496999976, -76.52755534788698810, 1.603559079323000125 ) ) ;
#45689 = DIRECTION ( 'NONE',  ( -1.000000000000000000, 0.000000000000000000, 0.000000000000000000 ) ) ;
#45690 = ADVANCED_FACE ( 'NONE', ( #27915 ), #24026, .F. ) ;
#45691 = DIRECTION ( 'NONE',  ( 1.000000000000000000, 0.000000000000000000, 0.000000000000000000 ) ) ;
#45692 = AXIS2_PLACEMENT_3D ( 'NONE', #41087, #55246, #41381 ) ;
#45693 = CARTESIAN_POINT ( 'NONE',  ( -11.04404426307000087, -76.30895766602598940, 2.028007672696999997 ) ) ;
#45694 = CARTESIAN_POINT ( 'NONE',  ( 3.884926167828604449, -78.75961067256588422, -8.428911604562424387 ) ) ;
#45695 = CARTESIAN_POINT ( 'NONE',  ( 0.5245219981381742391, -23.45160423346249701, -10.98753021428673904 ) ) ;
#45696 = DIRECTION ( 'NONE',  ( 0.000000000000000000, -1.000000000000000000, 0.000000000000000000 ) ) ;
#45697 = CARTESIAN_POINT ( 'NONE',  ( -9.158362268698009956, -80.14686259273240410, -6.092845169229706315 ) ) ;
#45698 = CYLINDRICAL_SURFACE ( 'NONE', #24885, 1.750000000000000000 ) ;
#45699 = CARTESIAN_POINT ( 'NONE',  ( -4.030725660649999931, -81.56417549782598542, -0.9009740902403999829 ) ) ;
#45700 = CARTESIAN_POINT ( 'NONE',  ( 0.000000000000000000, -80.35000000001998899, -10.84999999997999964 ) ) ;
#45701 = CARTESIAN_POINT ( 'NONE',  ( -8.363462758383999329, -77.23471332859898553, -4.819309911362999799 ) ) ;
#45702 = CARTESIAN_POINT ( 'NONE',  ( 12.00000000000000000, 0.000000000000000000, 0.000000000000000000 ) ) ;
#45703 = CARTESIAN_POINT ( 'NONE',  ( 7.708428212361858378, -77.10000000000000853, -5.602396082758937190 ) ) ;
#45704 = CARTESIAN_POINT ( 'NONE',  ( 1.691611010928000036, -24.23082691229999952, 12.66722148969999928 ) ) ;
#45705 = CARTESIAN_POINT ( 'NONE',  ( 0.000000000000000000, -78.69999999999998863, -2.799999999999969180 ) ) ;
#45706 = CARTESIAN_POINT ( 'NONE',  ( 7.000000000000000000, -80.99999999999998579, 0.000000000000000000 ) ) ;
#45707 = EDGE_CURVE ( 'NONE', #2750, #15146, #23502, .T. ) ;
#45708 = CARTESIAN_POINT ( 'NONE',  ( -1.404568169276999789, -1.063321030358999941, -3.519501389975000283 ) ) ;
#45709 = CARTESIAN_POINT ( 'NONE',  ( 1.249999999999999778, -80.76041666666665719, 0.1636246173744711763 ) ) ;
#45710 = VECTOR ( 'NONE', #8110, 1000.000000000000000 ) ;
#45711 = CARTESIAN_POINT ( 'NONE',  ( 1.749722766162256304, -55.32411007028125738, -12.54673760671575877 ) ) ;
#45712 = CARTESIAN_POINT ( 'NONE',  ( 12.70253258974613608, -24.97063167672577677, -0.9890392130105698509 ) ) ;
#45713 = CARTESIAN_POINT ( 'NONE',  ( 1.508371072044173422, -79.59420473664194162, -0.09860998784024260777 ) ) ;
#45714 = CARTESIAN_POINT ( 'NONE',  ( -12.00000000000000000, -75.15999999999999659, 0.000000000000000000 ) ) ;
#45715 = CARTESIAN_POINT ( 'NONE',  ( 3.438102579189000085, -2.807527036004999754, 0.5732922487111999921 ) ) ;
#45716 = CARTESIAN_POINT ( 'NONE',  ( 5.329123786712647970, -79.52101871112249398, -8.124383524005093449 ) ) ;
#45717 = CARTESIAN_POINT ( 'NONE',  ( 8.048377923311001325, -77.05528544001199975, -9.274674788995000085 ) ) ;
#45718 = DIRECTION ( 'NONE',  ( 0.000000000000000000, -1.000000000000000000, 1.021405182655000003E-13 ) ) ;
#45720 = CARTESIAN_POINT ( 'NONE',  ( -1.488622005431999851, -78.36789385589818835, -0.2880046469693999800 ) ) ;
#45719 = CARTESIAN_POINT ( 'NONE',  ( -1.199999995295999877, -81.00000000470399186, -7.000000027760000521 ) ) ;
#45721 = CARTESIAN_POINT ( 'NONE',  ( -1.544355253863999966, -83.28778917074799892, -0.3612495668209000366 ) ) ;
#45722 = EDGE_LOOP ( 'NONE', ( #31403, #33946, #2391 ) ) ;
#45723 = CARTESIAN_POINT ( 'NONE',  ( 1.109183238629000146, -84.43832450217399810, 3.413714993235999806 ) ) ;
#45724 = CARTESIAN_POINT ( 'NONE',  ( 8.378345960010999960, -79.31039397479999309, -8.487589272848000022 ) ) ;
#45725 = EDGE_CURVE ( 'NONE', #2185, #46363, #41291, .T. ) ;
#45726 = CARTESIAN_POINT ( 'NONE',  ( 0.3771049344988000041, -80.08120460502280480, 11.28275838026000066 ) ) ;
#45727 = CARTESIAN_POINT ( 'NONE',  ( -9.250000000000000000, -79.99999999999998579, 2.662757480928999879E-14 ) ) ;
#45728 = CARTESIAN_POINT ( 'NONE',  ( 1.310679582531387943, -81.70833333333332860, -0.7554284705563468760 ) ) ;
#45729 = CARTESIAN_POINT ( 'NONE',  ( -7.712695008784000272, -77.39856057395799382, -8.144473358846001432 ) ) ;
#45730 = FACE_OUTER_BOUND ( 'NONE', #2299, .T. ) ;
#45731 = CARTESIAN_POINT ( 'NONE',  ( -10.75000000000000000, -77.50000000000000000, 0.000000000000000000 ) ) ;
#45732 = CARTESIAN_POINT ( 'NONE',  ( 10.79124685046503451, -79.80000000000002558, -4.813060917148021645 ) ) ;
#45733 = CARTESIAN_POINT ( 'NONE',  ( -7.195400558141864522, -77.00000000000001421, 5.833420715738014906 ) ) ;
#45734 = ORIENTED_EDGE ( 'NONE', *, *, #24747, .F. ) ;
#45735 = CARTESIAN_POINT ( 'NONE',  ( -0.5999999999999999778, -5.000000000000000000, 0.5999999999999999778 ) ) ;
#45736 = CARTESIAN_POINT ( 'NONE',  ( -8.559817476595000585, -79.59513998579799932, 3.923328416589000334 ) ) ;
#45737 = CARTESIAN_POINT ( 'NONE',  ( 0.9262492265155897186, -75.83078504772286976, -11.74884656353136947 ) ) ;
#45738 = CARTESIAN_POINT ( 'NONE',  ( 0.000000000000000000, -77.00000000000000000, 0.000000000000000000 ) ) ;
#45739 = CARTESIAN_POINT ( 'NONE',  ( 0.000000000000000000, -76.39999999999999147, -9.549999999999997158 ) ) ;
#45740 = CARTESIAN_POINT ( 'NONE',  ( 0.000000000000000000, -87.70000000000000284, -9.699999999999993960 ) ) ;
#45741 = ORIENTED_EDGE ( 'NONE', *, *, #48818, .T. ) ;
#45742 = CARTESIAN_POINT ( 'NONE',  ( -2.843296433296999659, -78.09765876690597963, -10.84539213913000033 ) ) ;
#45743 = VECTOR ( 'NONE', #56984, 1000.000000000000000 ) ;
#45744 = CARTESIAN_POINT ( 'NONE',  ( -1.931086388455000025, -18.70221404512000163, 12.71798280854999952 ) ) ;
#45745 = ORIENTED_EDGE ( 'NONE', *, *, #8219, .F. ) ;
#45746 = ORIENTED_EDGE ( 'NONE', *, *, #32564, .T. ) ;
#45747 = CARTESIAN_POINT ( 'NONE',  ( -1.233649858953178802, -80.58776855326779298, 0.2004323432050792997 ) ) ;
#45748 = B_SPLINE_CURVE_WITH_KNOTS ( 'NONE', 3,
 ( #2727, #2436, #47323, #25435, #20723, #38722, #15712, #20153, #25145, #56450, #20437, #52031, #3011, #43170, #56163, #7719, #16302, #24571, #52315, #21292, #51745, #33706, #16874, #11295, #29275, #28992, #25722, #6852, #43450, #33993, #7433, #48187, #24862, #30137, #42878, #56743, #2151, #47033, #39299, #38433, #43747, #3299, #12152, #51455, #29849, #16005, #38140, #11585, #57310, #29563, #47618, #7142, #11008, #6563, #34568, #42588, #21006, #34280, #11871, #39012, #57021, #16582, #52600, #45200, #13000 ),
 .UNSPECIFIED., .F., .F.,
 ( 4, 2, 2, 2, 2, 2, 2, 2, 2, 2, 2, 2, 2, 2, 2, 2, 1, 2, 2, 2, 2, 2, 2, 2, 2, 2, 2, 2, 2, 2, 2, 2, 4 ),
 ( 0.000000000000000000, 0.03125000000000006245, 0.06250000000000012490, 0.09375000000000019429, 0.1250000000000002220, 0.1562500000000002776, 0.1875000000000003331, 0.2187500000000004163, 0.2500000000000004441, 0.2812500000000004996, 0.3125000000000005551, 0.3437500000000005551, 0.3750000000000005551, 0.4062500000000006106, 0.4375000000000006106, 0.4687500000000006106, 0.5000000000000005551, 0.5312500000000006661, 0.5625000000000006661, 0.5937500000000007772, 0.6250000000000006661, 0.6562500000000006661, 0.6875000000000005551, 0.7187500000000005551, 0.7500000000000004441, 0.7812500000000004441, 0.8125000000000004441, 0.8437500000000003331, 0.8750000000000003331, 0.9062500000000002220, 0.9375000000000002220, 0.9687500000000001110, 1.000000000000000000 ),
 .UNSPECIFIED. ) ;
#45749 = AXIS2_PLACEMENT_3D ( 'NONE', #1634, #56513, #37621 ) ;
#45750 = SURFACE_STYLE_FILL_AREA ( #37153 ) ;
#45751 = CARTESIAN_POINT ( 'NONE',  ( 8.944729675425000082, -79.79320053239750621, 3.923329690209000908 ) ) ;
#45752 = ORIENTED_EDGE ( 'NONE', *, *, #43896, .F. ) ;
#45753 = CARTESIAN_POINT ( 'NONE',  ( -5.996189434307000354, -76.03917199503599988, 10.66434391554000172 ) ) ;
#45754 = LINE ( 'NONE', #33007, #36241 ) ;
#45755 = CARTESIAN_POINT ( 'NONE',  ( 0.4622620975400000276, -78.35600317011999039, -1.463589239453999991 ) ) ;
#45756 = ORIENTED_EDGE ( 'NONE', *, *, #30669, .F. ) ;
#45757 = CARTESIAN_POINT ( 'NONE',  ( 6.214091009702999102, -77.75172305011498963, -7.179311535719000048 ) ) ;
#45758 = FACE_OUTER_BOUND ( 'NONE', #43699, .T. ) ;
#45759 = DIRECTION ( 'NONE',  ( 0.000000000000000000, 1.000000000000000000, 0.000000000000000000 ) ) ;
#45760 = CARTESIAN_POINT ( 'NONE',  ( -1.689459950971515800, -17.70811746097506401, -12.71013585610241492 ) ) ;
#45761 = LINE ( 'NONE', #37166, #17430 ) ;
#45762 = CARTESIAN_POINT ( 'NONE',  ( 8.993105270996114342, -79.86890122386594726, 2.164559197160741633 ) ) ;
#45763 = CARTESIAN_POINT ( 'NONE',  ( -2.775612516598270130, -78.89270831443518261, -2.898029264795531024 ) ) ;
#45764 = ORIENTED_EDGE ( 'NONE', *, *, #10186, .T. ) ;
#45765 = CARTESIAN_POINT ( 'NONE',  ( 9.208615812369000508, -77.02473186629366353, 2.957800710608999850 ) ) ;
#45766 = CARTESIAN_POINT ( 'NONE',  ( 11.65396969189999865, -75.67884329787000297, -2.860942225950000140 ) ) ;
#45767 = CARTESIAN_POINT ( 'NONE',  ( 0.6263439973055000554, -79.75135730798099587, 1.488256452092999949 ) ) ;
#45768 = B_SPLINE_SURFACE_WITH_KNOTS ( 'NONE', 3, 3, ( 
 ( #49048, #23342, #28046, #9768 ),
 ( #15060, #54645, #51102, #19496 ),
 ( #6202, #24215, #28334, #10945 ),
 ( #41641, #45800, #37491, #55513 ),
 ( #1506, #41354, #33054, #14184 ),
 ( #33355, #46385, #55809, #50807 ),
 ( #18918, #36626, #5909, #32180 ),
 ( #55215, #19211, #37789, #50220 ),
 ( #27756, #1221, #10653, #5335 ),
 ( #36912, #14762, #936, #15361 ),
 ( #10351, #14476, #51388, #32759 ),
 ( #23918, #54923, #46682, #28632 ),
 ( #41936, #37203, #42234, #1798 ),
 ( #32467, #45503, #50513, #19795 ),
 ( #5050, #23048, #10066, #41063 ),
 ( #649, #46092, #5618, #18634 ),
 ( #23629, #29499, #38941, #20657 ) ),
 .UNSPECIFIED., .F., .F., .F.,
 ( 4, 1, 1, 1, 1, 1, 1, 1, 1, 1, 1, 1, 1, 1, 4 ),
 ( 4, 4 ),
 ( -0.01011398171662000051, 0.000000000000000000, 0.08333333333333001192, 0.1666666666667000196, 0.2500000000000000000, 0.3333333333333000081, 0.4166666666666999919, 0.5000000000000000000, 0.5833333333333000637, 0.6666666666667000474, 0.7500000000000000000, 0.8333333333333000637, 0.9166666666667000474, 1.000000000000000000, 1.010365777941000021 ),
 ( -0.3559705546970999834, 1.357612346730000086 ),
 .UNSPECIFIED. ) ;
#45769 = CARTESIAN_POINT ( 'NONE',  ( 3.362134302577637790, -2.075432297516660363, -1.039236911360384985 ) ) ;
#45770 = CARTESIAN_POINT ( 'NONE',  ( 12.64502302238000020, -19.22870851082999977, 1.799490220168999954 ) ) ;
#45771 = CARTESIAN_POINT ( 'NONE',  ( -9.356096982537000173, -78.96139059408000094, 7.928589704419000128 ) ) ;
#45772 = CARTESIAN_POINT ( 'NONE',  ( 12.07535958108000074, -76.93710018766900305, -2.237927141218000404 ) ) ;
#45773 = CARTESIAN_POINT ( 'NONE',  ( -1.250000000000000000, -77.10000000000000853, -0.5000000000000000000 ) ) ;
#45774 = EDGE_CURVE ( 'NONE', #32986, #35553, #57415, .T. ) ;
#45775 = CARTESIAN_POINT ( 'NONE',  ( -5.824354096285000004, -76.95331498579798790, -7.803164568795000200 ) ) ;
#45776 = FACE_OUTER_BOUND ( 'NONE', #50100, .T. ) ;
#45777 = CARTESIAN_POINT ( 'NONE',  ( -8.382198119002001846, -79.80783961780795721, -7.453647783897999979 ) ) ;
#45778 = AXIS2_PLACEMENT_3D ( 'NONE', #17019, #52177, #30582 ) ;
#45779 = ORIENTED_EDGE ( 'NONE', *, *, #35877, .F. ) ;
#45781 = B_SPLINE_CURVE_WITH_KNOTS ( 'NONE', 3,
 ( #8124, #26405, #35256, #3980, #51643, #51926 ),
 .UNSPECIFIED., .F., .F.,
 ( 4, 1, 1, 4 ),
 ( 0.000000000000000000, 0.3333333333333000081, 0.6666666666667000474, 1.000000000000000000 ),
 .UNSPECIFIED. ) ;
#45780 = CARTESIAN_POINT ( 'NONE',  ( -1.259718275736121162, -81.29651786598202534, -0.8346564987574691674 ) ) ;
#45782 = TOROIDAL_SURFACE ( 'NONE', #58018, 1.250000000000000000, 0.5000000000000000000 ) ;
#45783 = CARTESIAN_POINT ( 'NONE',  ( 7.685661446562000343, -76.94999999999998863, -5.583959896778000420 ) ) ;
#45784 = CARTESIAN_POINT ( 'NONE',  ( 0.6295237254636211199, -79.33333333333332860, 1.092232985442824322 ) ) ;
#45785 = CARTESIAN_POINT ( 'NONE',  ( 0.9995835529977233902, -82.80208333333331439, 0.7681833999686461523 ) ) ;
#45786 = CARTESIAN_POINT ( 'NONE',  ( 6.948503177820483323, -77.00000000000000000, 6.231838918554943874 ) ) ;
#45787 = CARTESIAN_POINT ( 'NONE',  ( -5.720894519599999839, -77.92323108527999409, 10.60505245481999914 ) ) ;
#45788 = CARTESIAN_POINT ( 'NONE',  ( -9.554254755627999529, -78.19689511346298616, 1.212198840764999952 ) ) ;
#45789 = CARTESIAN_POINT ( 'NONE',  ( 2.342546989920156530, -76.05880917198733471, 11.51398673525604011 ) ) ;
#45790 = CARTESIAN_POINT ( 'NONE',  ( 8.503062319121001522, -78.76383098776300073, 7.028489548493999983 ) ) ;
#45791 = CARTESIAN_POINT ( 'NONE',  ( 3.922208058606372116, -86.07390000031791999, 0.4502061935818455485 ) ) ;
#45792 = EDGE_LOOP ( 'NONE', ( #33332, #30010 ) ) ;
#45793 = CARTESIAN_POINT ( 'NONE',  ( 7.644092900773786781, -18.47619833611041429, -10.09634159701095690 ) ) ;
#45794 = EDGE_CURVE ( 'NONE', #35802, #26558, #1895, .T. ) ;
#45795 = CARTESIAN_POINT ( 'NONE',  ( -3.587191200520567502, -78.43735717367049176, -2.026888227377177998 ) ) ;
#45796 = CARTESIAN_POINT ( 'NONE',  ( 10.55657102546000026, -78.71839418212100270, -3.003801718854000047 ) ) ;
#45797 = CARTESIAN_POINT ( 'NONE',  ( -8.485281374238999419, -55.54999999966999980, -8.485281374238999419 ) ) ;
#45798 = CARTESIAN_POINT ( 'NONE',  ( 11.68767212001978173, -77.67083333333334849, 3.140974612311388192 ) ) ;
#45799 = CARTESIAN_POINT ( 'NONE',  ( 7.954951288349001004, -18.75000000000000000, -9.722718241315000398 ) ) ;
#45800 = CARTESIAN_POINT ( 'NONE',  ( 10.30457855492000085, -18.23665569414000132, -7.636266481018999741 ) ) ;
#45801 = CARTESIAN_POINT ( 'NONE',  ( 0.000000000000000000, -59.58578169018999660, -13.15643568216998638 ) ) ;
#45802 = ORIENTED_EDGE ( 'NONE', *, *, #14507, .F. ) ;
#45803 = CARTESIAN_POINT ( 'NONE',  ( -0.4120475804594999625, -79.33092127781698366, -11.13933648663000042 ) ) ;
#45804 = CARTESIAN_POINT ( 'NONE',  ( 12.71466563513520676, -54.66210710670185335, 1.778810201848326500 ) ) ;
#45805 = CARTESIAN_POINT ( 'NONE',  ( -8.970887557736743290, -79.49333017060097006, 7.719903917865763354 ) ) ;
#45806 = CARTESIAN_POINT ( 'NONE',  ( -3.620804152519746300, -78.40681307385639798, -0.06825882735791576061 ) ) ;
#45808 = CARTESIAN_POINT ( 'NONE',  ( -0.5949523839205194120, -81.51488924677137504, 1.099213967298130923 ) ) ;
#45807 = CARTESIAN_POINT ( 'NONE',  ( 0.7262865762285000137, -80.82944907233598997, -1.101387507969000090 ) ) ;
#45809 = CARTESIAN_POINT ( 'NONE',  ( -6.966543547089000477, -79.37764829398598465, -8.575847751312000611 ) ) ;
#45810 = CARTESIAN_POINT ( 'NONE',  ( -9.318810932414811177, -77.00000000000001421, -0.6804550629738583822 ) ) ;
#45811 = CARTESIAN_POINT ( 'NONE',  ( 10.45204383630000144, -19.23743350652000217, 7.651147548127999798 ) ) ;
#45812 = EDGE_CURVE ( 'NONE', #39893, #29440, #43552, .T. ) ;
#45813 = DIRECTION ( 'NONE',  ( 0.7071067811865475727, 0.000000000000000000, 0.7071067811865475727 ) ) ;
#45814 = CARTESIAN_POINT ( 'NONE',  ( -9.439017928876026531, -79.49271986116634992, -5.601139116439918908 ) ) ;
#45815 = AXIS2_PLACEMENT_3D ( 'NONE', #5177, #15491, #32891 ) ;
#45816 = CARTESIAN_POINT ( 'NONE',  ( -12.50745077494999968, -61.79994448255000350, -2.661703094427999907E-09 ) ) ;
#45817 = ORIENTED_EDGE ( 'NONE', *, *, #51087, .T. ) ;
#45818 = ORIENTED_EDGE ( 'NONE', *, *, #39358, .T. ) ;
#45819 = CARTESIAN_POINT ( 'NONE',  ( -7.837473280028000033, -78.32578998579799645, 6.246724465767999668 ) ) ;
#45820 = CARTESIAN_POINT ( 'NONE',  ( 6.916475164548741894, -78.78069308715726038, -8.229583957785196802 ) ) ;
#45821 = ORIENTED_EDGE ( 'NONE', *, *, #29018, .T. ) ;
#45822 = LINE ( 'NONE', #23366, #23679 ) ;
#45823 = CARTESIAN_POINT ( 'NONE',  ( 1.845937214730200226, -83.71041667982382251, -2.906560619503415044 ) ) ;
#45824 = AXIS2_PLACEMENT_3D ( 'NONE', #50421, #46000, #4953 ) ;
#45825 = AXIS2_PLACEMENT_3D ( 'NONE', #13314, #35749, #31607 ) ;
#45826 = CARTESIAN_POINT ( 'NONE',  ( 7.647093862774999806, -60.16895637605999525, 10.00844027277999970 ) ) ;
#45827 = CARTESIAN_POINT ( 'NONE',  ( 2.080730497819520242, -77.18813522852776998, -11.79602317567259995 ) ) ;
#45828 = DIRECTION ( 'NONE',  ( -1.000000000000000000, 0.000000000000000000, 0.000000000000000000 ) ) ;
#45829 = CARTESIAN_POINT ( 'NONE',  ( 10.89876807034000095, -79.49710884097999042, -2.652350870517000025 ) ) ;
#45830 = CARTESIAN_POINT ( 'NONE',  ( 6.010274707836598118, -81.00000000000000000, 9.066665045992072791 ) ) ;
#45831 = B_SPLINE_CURVE_WITH_KNOTS ( 'NONE', 3,
 ( #47822, #57514, #20927, #16505, #48387, #30345, #7925, #38928, #3500, #16795, #34779, #12643, #7352, #25638, #30055, #48106, #52803 ),
 .UNSPECIFIED., .F., .F.,
 ( 4, 2, 1, 2, 2, 1, 1, 2, 2, 4 ),
 ( 0.000000000000000000, 0.2500000000000005551, 0.3750000000000007772, 0.4375000000000007772, 0.5000000000000007772, 0.6250000000000006661, 0.6875000000000004441, 0.7187500000000002220, 0.7500000000000001110, 1.000000000000000000 ),
 .UNSPECIFIED. ) ;
#45832 = ORIENTED_EDGE ( 'NONE', *, *, #4076, .F. ) ;
#45833 = CARTESIAN_POINT ( 'NONE',  ( -9.175573575508092716, -25.22695822358256024, 8.792784719773246493 ) ) ;
#45834 = ORIENTED_EDGE ( 'NONE', *, *, #23650, .F. ) ;
#45835 = CARTESIAN_POINT ( 'NONE',  ( 7.482391911512093152, -77.40012167121783193, 5.438283650742095965 ) ) ;
#45836 = CARTESIAN_POINT ( 'NONE',  ( -10.84202097104999929, -77.41505392682599052, 2.082001701158999740 ) ) ;
#45837 = FACE_OUTER_BOUND ( 'NONE', #47307, .T. ) ;
#45838 = CARTESIAN_POINT ( 'NONE',  ( 1.592284932317999946, -78.25521359734770499, 0.2680347371437999948 ) ) ;
#45839 = CARTESIAN_POINT ( 'NONE',  ( -9.596002108778160178, -77.45208333333332007, -7.374560639698984232 ) ) ;
#45840 = DIRECTION ( 'NONE',  ( -1.000000000000000000, 0.000000000000000000, 0.000000000000000000 ) ) ;
#45841 = CARTESIAN_POINT ( 'NONE',  ( 0.1660104325307999729, -78.13726038467999047, 1.618982269915999916 ) ) ;
#45842 = B_SPLINE_CURVE_WITH_KNOTS ( 'NONE', 3,
 ( #56634, #51058, #16192, #15898, #24757, #29739, #5866, #2334, #23875, #1757 ),
 .UNSPECIFIED., .F., .F.,
 ( 4, 2, 2, 2, 4 ),
 ( 0.000000000000000000, 0.2500000000000000000, 0.5000000000000000000, 0.7500000000000000000, 1.000000000000000000 ),
 .UNSPECIFIED. ) ;
#45843 = CARTESIAN_POINT ( 'NONE',  ( -3.493617039247999934, -80.58938358939499835, -10.33892454317000187 ) ) ;
#45844 = CARTESIAN_POINT ( 'NONE',  ( -3.536853559812999759, -79.52798916675298813, -10.35270415072999839 ) ) ;
#45845 = ADVANCED_FACE ( 'NONE', ( #34090 ), #55126, .F. ) ;
#45846 = CARTESIAN_POINT ( 'NONE',  ( 1.799501877793999949, -60.08917723397000543, -12.60552511012999943 ) ) ;
#45847 = CARTESIAN_POINT ( 'NONE',  ( -7.401770473313917797, -60.25155696365191460, 8.137215171344811537 ) ) ;
#45848 = CARTESIAN_POINT ( 'NONE',  ( 3.435165100308000152, -83.95300820753398341, 0.8744208703508999925 ) ) ;
#45849 = ORIENTED_EDGE ( 'NONE', *, *, #42289, .F. ) ;
#45850 = EDGE_CURVE ( 'NONE', #52629, #35908, #4700, .T. ) ;
#45851 = CARTESIAN_POINT ( 'NONE',  ( 10.48543666025110355, -79.60833333333329165, -6.043427764450775008 ) ) ;
#45852 = CARTESIAN_POINT ( 'NONE',  ( -9.946140829862999411, -76.03462989806899941, 5.270939064036999966 ) ) ;
#45853 = CARTESIAN_POINT ( 'NONE',  ( -0.06653476265715067839, -77.97558014977887808, 10.74979742560490514 ) ) ;
#45854 = CARTESIAN_POINT ( 'NONE',  ( -5.261498566940000288, -77.79049859790299593, -10.76255997729999869 ) ) ;
#45855 = CARTESIAN_POINT ( 'NONE',  ( 3.250000000000000000, -3.250000000000000000, 0.000000000000000000 ) ) ;
#45857 = CARTESIAN_POINT ( 'NONE',  ( 0.000000000000000000, -87.64999999984398471, 0.000000000000000000 ) ) ;
#45856 = CARTESIAN_POINT ( 'NONE',  ( -1.405334851868360602, -61.11492947527288777, -12.50716844841877773 ) ) ;
#45858 = CARTESIAN_POINT ( 'NONE',  ( -3.043150799898603154, -3.291925712094595280, -1.769611200578169008 ) ) ;
#45859 = CARTESIAN_POINT ( 'NONE',  ( 1.222863591967999985, -77.44381939105899448, 9.333584474513999751 ) ) ;
#45860 = CARTESIAN_POINT ( 'NONE',  ( -5.871863728899527679, -86.07390000031791999, -4.829204525511850754 ) ) ;
#45861 = CARTESIAN_POINT ( 'NONE',  ( -11.14677829112999952, -77.89158425314199974, -0.06272399197936999460 ) ) ;
#45862 = DIRECTION ( 'NONE',  ( 0.000000000000000000, 1.000000000000000000, 0.000000000000000000 ) ) ;
#45863 = CARTESIAN_POINT ( 'NONE',  ( 10.86022371085000060, -80.72266989507731694, 1.903339784773000032 ) ) ;
#45864 = ORIENTED_EDGE ( 'NONE', *, *, #40249, .F. ) ;
#45865 = CARTESIAN_POINT ( 'NONE',  ( 8.979348251287998295, -77.92634903538301216, 3.086914251890999328 ) ) ;
#45866 = EDGE_CURVE ( 'NONE', #45077, #11731, #48513, .T. ) ;
#45867 = CARTESIAN_POINT ( 'NONE',  ( -3.943885540262999534, -3.314075421107999908, -0.4205739404420000271 ) ) ;
#45868 = CARTESIAN_POINT ( 'NONE',  ( -11.14038684213999986, -78.25680768274300192, 1.307628137226999998 ) ) ;
#45869 = CARTESIAN_POINT ( 'NONE',  ( 10.85730540529999999, -79.07124013742898683, 1.607151491820999922 ) ) ;
#45870 = CARTESIAN_POINT ( 'NONE',  ( 8.878335097414000288, -25.06963071744000260, -8.870344075630997693 ) ) ;
#45871 = DIRECTION ( 'NONE',  ( 0.000000000000000000, 1.000000000000000000, 8.313952627639000142E-11 ) ) ;
#45872 = CARTESIAN_POINT ( 'NONE',  ( 5.454964632513748413, -79.75000000000000000, -7.505574818958165473 ) ) ;
#45873 = CARTESIAN_POINT ( 'NONE',  ( -8.532671860894721405, -53.67201063361042657, -9.433519686823784056 ) ) ;
#45874 = CIRCLE ( 'NONE', #55290, 4.000000000000000000 ) ;
#45875 = CARTESIAN_POINT ( 'NONE',  ( 3.044637772279000121, -84.11719503318798274, 2.853111132616000134 ) ) ;
#45876 = CARTESIAN_POINT ( 'NONE',  ( -7.651160336708000109, -59.56232686183999903, 10.45205658995999976 ) ) ;
#45877 = CIRCLE ( 'NONE', #50592, 1.250000000000000444 ) ;
#45878 = CARTESIAN_POINT ( 'NONE',  ( 10.01749678874999994, -55.60819056964000140, -7.660430392551000445 ) ) ;
#45879 = FACE_OUTER_BOUND ( 'NONE', #14870, .T. ) ;
#45880 = CARTESIAN_POINT ( 'NONE',  ( 1.587978134902999994, -80.48561246212999265, 0.5035716945827000135 ) ) ;
#45881 = CARTESIAN_POINT ( 'NONE',  ( 1.016693945846000036, -78.76897944923000239, 1.012133007862000111 ) ) ;
#45882 = CARTESIAN_POINT ( 'NONE',  ( -12.00000000000000000, -79.29999999999999716, 0.000000000000000000 ) ) ;
#45883 = CARTESIAN_POINT ( 'NONE',  ( -0.7630392650730208892, -81.83296632765541290, -1.305528064125151655 ) ) ;
#45884 = CARTESIAN_POINT ( 'NONE',  ( 0.000000000000000000, -32.36102867817999851, 0.000000000000000000 ) ) ;
#45885 = CARTESIAN_POINT ( 'NONE',  ( -10.57946111658618449, -80.11494313127583666, -1.988425045866919927 ) ) ;
#45886 = CARTESIAN_POINT ( 'NONE',  ( 9.500000000000005329, -78.03958333333333997, -1.243547092045939939 ) ) ;
#45887 = ORIENTED_EDGE ( 'NONE', *, *, #15183, .T. ) ;
#45888 = CARTESIAN_POINT ( 'NONE',  ( -1.227645687060430424, -81.61625190046059686, -0.2506207581016212105 ) ) ;
#45889 = CARTESIAN_POINT ( 'NONE',  ( 0.000000000000000000, 0.000000000000000000, 0.000000000000000000 ) ) ;
#45890 = CARTESIAN_POINT ( 'NONE',  ( -5.236138783747000147, -78.80504929535699432, 9.840602177168999987 ) ) ;
#45891 = LINE ( 'NONE', #55310, #19562 ) ;
#45892 = ORIENTED_EDGE ( 'NONE', *, *, #30602, .T. ) ;
#45893 = ORIENTED_EDGE ( 'NONE', *, *, #11738, .F. ) ;
#45894 = CARTESIAN_POINT ( 'NONE',  ( 1.324686507300999905, -80.82369000798900061, -0.5052412751467000307 ) ) ;
#45895 = EDGE_LOOP ( 'NONE', ( #174, #46403, #6966 ) ) ;
#45897 = EDGE_CURVE ( 'NONE', #58122, #28795, #4215, .T. ) ;
#45896 = ORIENTED_EDGE ( 'NONE', *, *, #4707, .F. ) ;
#45898 = CARTESIAN_POINT ( 'NONE',  ( -1.930628539545000022, -18.77875555914000216, 12.72375828104000028 ) ) ;
#45899 = CARTESIAN_POINT ( 'NONE',  ( -7.407754918741036754, -80.41680592794931215, -8.285828061842591907 ) ) ;
#45900 = CARTESIAN_POINT ( 'NONE',  ( 1.750000000000000000, -58.54977139303999678, 12.65375411740000011 ) ) ;
#45901 = B_SPLINE_CURVE_WITH_KNOTS ( 'NONE', 3,
 ( #36542, #9685, #19419, #9981, #1430, #14389 ),
 .UNSPECIFIED., .F., .F.,
 ( 4, 1, 1, 4 ),
 ( 0.000000000000000000, 0.3333333333333000081, 0.6666666666667000474, 1.000000000000000000 ),
 .UNSPECIFIED. ) ;
#45902 = CARTESIAN_POINT ( 'NONE',  ( -9.273838249849999826, -79.28971001420200082, 3.800455380692000062 ) ) ;
#45903 = CARTESIAN_POINT ( 'NONE',  ( 5.896854890547934325, -78.28013406490441639, -7.126572464670269724 ) ) ;
#45904 = CARTESIAN_POINT ( 'NONE',  ( -2.813789756862251856, -78.10416666666665719, -10.47020627418439709 ) ) ;
#45905 = ORIENTED_EDGE ( 'NONE', *, *, #46042, .T. ) ;
#45906 = VERTEX_POINT ( 'NONE', #52699 ) ;
#45907 = DIRECTION ( 'NONE',  ( 1.000000000000000000, 0.000000000000000000, 0.000000000000000000 ) ) ;
#45908 = DIRECTION ( 'NONE',  ( -1.000000000000000000, 0.000000000000000000, 0.000000000000000000 ) ) ;
#45909 = CARTESIAN_POINT ( 'NONE',  ( -0.3271848554491046945, -81.39583333333327175, 1.217465845835393301 ) ) ;
#45910 = AXIS2_PLACEMENT_3D ( 'NONE', #31183, #57779, #40361 ) ;
#45911 = DIRECTION ( 'NONE',  ( 1.000000000000000000, 0.000000000000000000, 0.000000000000000000 ) ) ;
#45912 = CARTESIAN_POINT ( 'NONE',  ( -3.907230163516999699, -77.86187217243097791, -8.882807090995999744 ) ) ;
#45913 = CARTESIAN_POINT ( 'NONE',  ( 10.41144098945170171, -60.32546312028583202, 7.610433527984337587 ) ) ;
#45914 = CARTESIAN_POINT ( 'NONE',  ( 2.352936540351114658, -85.88541304819187872, 3.122209706914203409 ) ) ;
#45915 = VECTOR ( 'NONE', #42721, 1000.000000000000000 ) ;
#45916 = CARTESIAN_POINT ( 'NONE',  ( -12.91020013338000005, -76.92524667502999591, -1.090565897604000023 ) ) ;
#45917 = CARTESIAN_POINT ( 'NONE',  ( 0.4206423954835999401, -80.29146017332999463, -1.406949933701999944 ) ) ;
#45918 = CARTESIAN_POINT ( 'NONE',  ( -12.69616050742999924, -21.75171076523999858, -1.799475304559999822 ) ) ;
#45919 = AXIS2_PLACEMENT_3D ( 'NONE', #36099, #57951, #35200 ) ;
#45920 = CARTESIAN_POINT ( 'NONE',  ( 0.5805005430889391693, -76.57101688036192400, 11.73679383478257243 ) ) ;
#45921 = EDGE_CURVE ( 'NONE', #47903, #29770, #3944, .T. ) ;
#45922 = CARTESIAN_POINT ( 'NONE',  ( 3.496672618083999762, -79.64448742432209372, 2.280984592505000297 ) ) ;
#45923 = VECTOR ( 'NONE', #21187, 1000.000000000000000 ) ;
#45924 = CARTESIAN_POINT ( 'NONE',  ( 5.365883907697000410, -80.10159911017460388, 9.905345355165000143 ) ) ;
#45925 = CARTESIAN_POINT ( 'NONE',  ( 1.892857502466999797, -78.43001001420199714, 9.500437764121999251 ) ) ;
#45926 = DIRECTION ( 'NONE',  ( 0.000000000000000000, 1.000000000000000000, 0.000000000000000000 ) ) ;
#45927 = CARTESIAN_POINT ( 'NONE',  ( 3.499218162531000154, -80.92330496681199747, -0.5805468162371000274 ) ) ;
#45928 = CARTESIAN_POINT ( 'NONE',  ( 1.196963559360000096, -78.47931953192639298, -0.5880938590690999446 ) ) ;
#45929 = CARTESIAN_POINT ( 'NONE',  ( 11.68767212001978173, -78.17083333333334849, 3.140974612311388192 ) ) ;
#45930 = CARTESIAN_POINT ( 'NONE',  ( 11.80100040161109298, -79.24999999999997158, 2.513071073578707626 ) ) ;
#45931 = CARTESIAN_POINT ( 'NONE',  ( 1.911540947291000103, -3.150461020869000262, 3.291214574437999918 ) ) ;
#45932 = CARTESIAN_POINT ( 'NONE',  ( 0.1636246173744697330, -79.13541666666665719, -1.249999999999999778 ) ) ;
#45933 = ORIENTED_EDGE ( 'NONE', *, *, #42200, .T. ) ;
#45934 = CARTESIAN_POINT ( 'NONE',  ( 2.460715419384281066, -78.94166666666667709, -11.55514622821795889 ) ) ;
#45935 = CARTESIAN_POINT ( 'NONE',  ( -12.04999999926000243, -79.29999999926000953, -5.384918809984000181E-09 ) ) ;
#45936 = CARTESIAN_POINT ( 'NONE',  ( 10.27281115125161648, -77.48889879997290109, 5.919856814084291763 ) ) ;
#45937 = EDGE_CURVE ( 'NONE', #24195, #185, #8689, .T. ) ;
#45938 = CARTESIAN_POINT ( 'NONE',  ( -6.603669512656000329, -79.76338829707400180, 7.175056597861000363 ) ) ;
#45939 = CARTESIAN_POINT ( 'NONE',  ( -12.97861384075000046, -77.95378978747999099, -0.9459496016724999734 ) ) ;
#45940 = CARTESIAN_POINT ( 'NONE',  ( 6.772653575186247110, -79.42076571837985455, 8.352388374815941319 ) ) ;
#45941 = CARTESIAN_POINT ( 'NONE',  ( 1.869758079914999982, -79.23913998579800477, 9.669518374590998278 ) ) ;
#45942 = CARTESIAN_POINT ( 'NONE',  ( 11.19195407364522943, -78.47360375268350197, 3.576835338053799607 ) ) ;
#45943 = LINE ( 'NONE', #1358, #6146 ) ;
#45944 = CARTESIAN_POINT ( 'NONE',  ( -0.9873574601251999816, -77.29720827014600104, -11.23080870426000111 ) ) ;
#45945 = B_SPLINE_CURVE_WITH_KNOTS ( 'NONE', 3,
 ( #40070, #52586, #22363, #13503, #23825, #1706, #1418, #27663, #560, #10856, #55124, #33258, #46293, #55718, #50718, #54836, #18827, #36529, #5819, #32092, #5244, #6113, #14093, #54553, #1129 ),
 .UNSPECIFIED., .F., .F.,
 ( 4, 2, 2, 2, 2, 2, 2, 2, 1, 2, 2, 2, 4 ),
 ( 0.000000000000000000, 0.1249999840576382637, 0.1874999760864574372, 0.2499999681152765829, 0.3749999521729150409, 0.4374999442017342699, 0.4999999362305534989, 0.5312499322449630856, 0.5624999282593725614, 0.6249999202881917348, 0.7499999043458301928, 0.8749998884034685398, 0.9999998724611069978 ),
 .UNSPECIFIED. ) ;
#45946 = CARTESIAN_POINT ( 'NONE',  ( 1.215992416571999968, -82.05245088088400962, -0.8889676458159999628 ) ) ;
#45947 = DIRECTION ( 'NONE',  ( 0.000000000000000000, 0.000000000000000000, 1.000000000000000000 ) ) ;
#45948 = CARTESIAN_POINT ( 'NONE',  ( 6.053520011479999852, -78.34022787947299094, 7.208750930507999755 ) ) ;
#45950 = CARTESIAN_POINT ( 'NONE',  ( -1.488596180559999871, -0.9467806054949000627, -3.730054860412999940 ) ) ;
#45949 = CARTESIAN_POINT ( 'NONE',  ( 4.174647607761000856, -85.39601319073598518, 0.04390291789455000315 ) ) ;
#45951 = CARTESIAN_POINT ( 'NONE',  ( -2.317989000404999889, -79.79565584965399694, -9.269382932261999386 ) ) ;
#45952 = CARTESIAN_POINT ( 'NONE',  ( -0.7681833999686432657, -82.57291666666667140, -0.9995835529977258327 ) ) ;
#45953 = CARTESIAN_POINT ( 'NONE',  ( 0.1998609718125000101, -80.29515928207800357, -1.304078681214000168 ) ) ;
#45954 = CIRCLE ( 'NONE', #51598, 8.500000000000000000 ) ;
#45955 = CARTESIAN_POINT ( 'NONE',  ( -6.815894852583468833, -77.17042358260589197, -8.313150857696243179 ) ) ;
#45956 = DIRECTION ( 'NONE',  ( 0.000000000000000000, -1.000000000000000000, 1.273055734904000118E-13 ) ) ;
#45957 = PRODUCT_DEFINITION ( 'UNKNOWN', '', #48051, #17404 ) ;
#45958 = CARTESIAN_POINT ( 'NONE',  ( 3.851650068366999857, -78.96264283715740362, -4.716910927661330529E-16 ) ) ;
#45959 = VECTOR ( 'NONE', #18759, 1000.000000000000114 ) ;
#45960 = VERTEX_POINT ( 'NONE', #13399 ) ;
#45961 = CARTESIAN_POINT ( 'NONE',  ( 10.43959491470999978, -79.84251694161849855, -5.976816984917999953 ) ) ;
#45962 = CARTESIAN_POINT ( 'NONE',  ( -7.249533335624161801, -76.09557291620778585, -9.431925875569948658 ) ) ;
#45963 = FACE_OUTER_BOUND ( 'NONE', #6657, .T. ) ;
#45964 = CONICAL_SURFACE ( 'NONE', #21407, 3.399999999997999733, 0.9827937232471395390 ) ;
#45965 = ORIENTED_EDGE ( 'NONE', *, *, #25068, .F. ) ;
#45966 = CARTESIAN_POINT ( 'NONE',  ( 0.4826013546558999279, -77.49519064797900114, 11.92487309688999986 ) ) ;
#45967 = AXIS2_PLACEMENT_3D ( 'NONE', #45884, #5416, #36708 ) ;
#45968 = ORIENTED_EDGE ( 'NONE', *, *, #4344, .T. ) ;
#45970 = EDGE_CURVE ( 'NONE', #40049, #20675, #30581, .T. ) ;
#45969 = ORIENTED_EDGE ( 'NONE', *, *, #9490, .T. ) ;
#45971 = CARTESIAN_POINT ( 'NONE',  ( 0.02549637870113643373, -2.726424292193095678, -3.249520170519987428 ) ) ;
#45972 = EDGE_LOOP ( 'NONE', ( #53709, #37731 ) ) ;
#45973 = ADVANCED_FACE ( 'NONE', ( #4563 ), #1421, .F. ) ;
#45974 = CARTESIAN_POINT ( 'NONE',  ( 2.111723220701999804, -79.21468383341469632, -2.849946108166999892 ) ) ;
#45975 = CARTESIAN_POINT ( 'NONE',  ( -9.499653450934914645, -79.30027302004205580, 1.387647615217423080E-06 ) ) ;
#45976 = VERTEX_POINT ( 'NONE', #50029 ) ;
#45977 = CARTESIAN_POINT ( 'NONE',  ( -8.872949061359179268, -53.78989818412208024, -8.813905827841837848 ) ) ;
#45978 = EDGE_LOOP ( 'NONE', ( #23592, #37808, #44779, #9711 ) ) ;
#45979 = CARTESIAN_POINT ( 'NONE',  ( 8.596418555780450887, -80.69791666666667140, -6.606377239730321982 ) ) ;
#45980 = CARTESIAN_POINT ( 'NONE',  ( 5.928084975461002770, -78.02720074687999841, -7.683204820502274046 ) ) ;
#45981 = CARTESIAN_POINT ( 'NONE',  ( 3.914500761936999140, -78.91452044229970397, -2.310234204170795280 ) ) ;
#45982 = DIRECTION ( 'NONE',  ( 0.000000000000000000, 1.000000000000000000, 0.000000000000000000 ) ) ;
#45983 = CARTESIAN_POINT ( 'NONE',  ( -12.99510751537000353, -26.30294702886003222, 6.911973076623003642 ) ) ;
#45984 = CARTESIAN_POINT ( 'NONE',  ( 4.903943924252999409, -76.42722757993099947, -10.05113017056000047 ) ) ;
#45985 = FACE_BOUND ( 'NONE', #14290, .T. ) ;
#45986 = CARTESIAN_POINT ( 'NONE',  ( -7.726022376260000435, -76.25879378204800219, 8.148147461043999229 ) ) ;
#45987 = CARTESIAN_POINT ( 'NONE',  ( 7.179580682979864292, -78.79576402591504802, -5.832456873467035230 ) ) ;
#45988 = CARTESIAN_POINT ( 'NONE',  ( 2.311693661511226239, -76.55883260880376895, 11.52009055038358198 ) ) ;
#45989 = CARTESIAN_POINT ( 'NONE',  ( -9.186791650646000562, -77.08808501420200798, -2.044400565391000235 ) ) ;
#45990 = CARTESIAN_POINT ( 'NONE',  ( 0.9336649615752000697, -80.32105334749999770, -0.9522845488932000224 ) ) ;
#45991 = CARTESIAN_POINT ( 'NONE',  ( -9.698041772758232426, -80.13957045507287091, -5.198397055125564492 ) ) ;
#45992 = CARTESIAN_POINT ( 'NONE',  ( 0.5788847457760372128, -78.32421909374012614, 12.05596584941754834 ) ) ;
#45993 = VECTOR ( 'NONE', #28087, 1000.000000000000114 ) ;
#45994 = CARTESIAN_POINT ( 'NONE',  ( -0.05809966506197000030, -79.52378455456849338, 3.962651287612999784 ) ) ;
#45995 = CYLINDRICAL_SURFACE ( 'NONE', #56054, 10.25000000000000000 ) ;
#45996 = CARTESIAN_POINT ( 'NONE',  ( -1.750000000000000000, -58.55064714144999982, 12.65372179280999987 ) ) ;
#45997 = CARTESIAN_POINT ( 'NONE',  ( -1.181971670502384386, -83.07366182756899775, 0.4080206837518099428 ) ) ;
#45998 = DIRECTION ( 'NONE',  ( 0.7592504788685162653, 0.04890177849164110968, -0.6489586476797141179 ) ) ;
#45999 = CARTESIAN_POINT ( 'NONE',  ( -3.914500761937000028, -78.91452044229970397, -1.642509933758750038E-14 ) ) ;
#46000 = DIRECTION ( 'NONE',  ( 0.000000000000000000, 1.000000000000000000, 0.000000000000000000 ) ) ;
#46001 = CARTESIAN_POINT ( 'NONE',  ( -1.001315002179000047, -24.68522411714000242, 12.50000000000000000 ) ) ;
#46002 = TOROIDAL_SURFACE ( 'NONE', #6410, 1.250000000000000000, 0.5000000000000000000 ) ;
#46003 = CARTESIAN_POINT ( 'NONE',  ( 10.35747145890000098, -55.48415267986000288, 7.626500777218999438 ) ) ;
#46004 = CARTESIAN_POINT ( 'NONE',  ( 1.438147912481374968, -79.62457046011485318, 0.4697345871869623712 ) ) ;
#46005 = LINE ( 'NONE', #45714, #43880 ) ;
#46006 = CIRCLE ( 'NONE', #3536, 8.500000000000000000 ) ;
#46007 = CARTESIAN_POINT ( 'NONE',  ( 4.044903269867999640, -79.46000000000000796, -8.595856998426999240 ) ) ;
#46008 = EDGE_CURVE ( 'NONE', #57837, #57298, #52318, .T. ) ;
#46009 = CARTESIAN_POINT ( 'NONE',  ( 12.79972228482999874, -23.79021513454000214, 2.019125729023000027 ) ) ;
#46010 = CARTESIAN_POINT ( 'NONE',  ( -10.21587511493324207, -77.42472830502559589, 3.417954814639385663 ) ) ;
#46011 = CARTESIAN_POINT ( 'NONE',  ( -3.599999993293999889, -0.2000000067061999953, -5.600095662875000459E-09 ) ) ;
#46012 = CIRCLE ( 'NONE', #3540, 1.750000000000000000 ) ;
#46014 = CARTESIAN_POINT ( 'NONE',  ( -1.718598679968283971, -24.24962933044487912, -12.71111582768035220 ) ) ;
#46013 = DIRECTION ( 'NONE',  ( -1.000000000000000000, 0.000000000000000000, 0.000000000000000000 ) ) ;
#46015 = DIRECTION ( 'NONE',  ( 0.000000000000000000, 0.000000000000000000, -1.000000000000000000 ) ) ;
#46016 = SHAPE_REPRESENTATION ( 'Push Button Connector', ( #43526 ), #9600 ) ;
#46017 = ORIENTED_EDGE ( 'NONE', *, *, #40304, .T. ) ;
#46018 = CARTESIAN_POINT ( 'NONE',  ( -2.881626843934999904, -83.23582450217399753, 2.140085129360999705 ) ) ;
#46019 = CARTESIAN_POINT ( 'NONE',  ( -7.070160385238000167, -80.84838538950840814, -8.949886881840999564 ) ) ;
#46020 = CARTESIAN_POINT ( 'NONE',  ( 8.335168759715775977, -78.31433322054517987, -4.010873337216996681 ) ) ;
#46021 = CARTESIAN_POINT ( 'NONE',  ( 8.620934061238347823, -53.63470696644542812, 9.346030177867731936 ) ) ;
#46022 = CARTESIAN_POINT ( 'NONE',  ( -3.244487197725999916, -77.00333129620300099, -10.73738397614000029 ) ) ;
#46023 = CARTESIAN_POINT ( 'NONE',  ( 2.426647618366999603E-14, -6.000000000000000000, -13.00000000000343547 ) ) ;
#46024 = CARTESIAN_POINT ( 'NONE',  ( 7.830665294675000609, -79.09361510090498371, -5.606588350762000239 ) ) ;
#46025 = CARTESIAN_POINT ( 'NONE',  ( -3.726464253369000001, -0.8073096613111999664, -0.05413188946992000122 ) ) ;
#46026 = CARTESIAN_POINT ( 'NONE',  ( -9.342118770336998779, -79.29745298729598346, -3.249678031071000284 ) ) ;
#46027 = CARTESIAN_POINT ( 'NONE',  ( 7.415475502687034037, -81.00000000000000000, -8.207007851251338693 ) ) ;
#46028 = VERTEX_POINT ( 'NONE', #26974 ) ;
#46029 = PLANE ( 'NONE',  #5038 ) ;
#46030 = CARTESIAN_POINT ( 'NONE',  ( 4.070739930424000619, -79.35384666193300518, -8.460094790468001946 ) ) ;
#46031 = ADVANCED_FACE ( 'NONE', ( #53565 ), #2956, .F. ) ;
#46032 = DIRECTION ( 'NONE',  ( 1.000000000000000000, 0.000000000000000000, 0.000000000000000000 ) ) ;
#46033 = VERTEX_POINT ( 'NONE', #56109 ) ;
#46034 = CARTESIAN_POINT ( 'NONE',  ( 1.310679582531388387, -78.60833333333333428, -0.7554284705563470981 ) ) ;
#46035 = FACE_OUTER_BOUND ( 'NONE', #26757, .T. ) ;
#46036 = ORIENTED_EDGE ( 'NONE', *, *, #54587, .F. ) ;
#46037 = CARTESIAN_POINT ( 'NONE',  ( 11.99915429782999965, -78.59363925020198849, 2.610761444098000261 ) ) ;
#46038 = CARTESIAN_POINT ( 'NONE',  ( -1.320560947307999999, -77.81367477412999278, 11.02278443658000029 ) ) ;
#46039 = CARTESIAN_POINT ( 'NONE',  ( -2.062502994258999856, -20.24351820077000141, 12.92181194099999963 ) ) ;
#46040 = VERTEX_POINT ( 'NONE', #33062 ) ;
#46041 = FACE_OUTER_BOUND ( 'NONE', #15159, .T. ) ;
#46042 = EDGE_CURVE ( 'NONE', #24385, #7885, #38462, .T. ) ;
#46043 = CARTESIAN_POINT ( 'NONE',  ( -9.687172913667000174, -79.90065629675500247, -1.248753675804000096 ) ) ;
#46044 = EDGE_LOOP ( 'NONE', ( #39300, #25097, #13001, #33514, #39754, #54226 ) ) ;
#46045 = CARTESIAN_POINT ( 'NONE',  ( -7.648026768008000076, -55.55000001556999933, 10.12290050216000026 ) ) ;
#46046 = CARTESIAN_POINT ( 'NONE',  ( -9.050966798898000931, -59.94999999040999938, -7.919595949288999570 ) ) ;
#46047 = CARTESIAN_POINT ( 'NONE',  ( -12.43422056531000131, -24.43655741434000106, -1.197404442627999943 ) ) ;
#46048 = CARTESIAN_POINT ( 'NONE',  ( -1.269916711065999904, -77.24437694988499459, -9.409822520238998678 ) ) ;
#46049 = CARTESIAN_POINT ( 'NONE',  ( -17.49999999998999911, -65.72928575305999743, -1.613072092318999730E-05 ) ) ;
#46050 = AXIS2_PLACEMENT_3D ( 'NONE', #41119, #45862, #23404 ) ;
#46051 = CARTESIAN_POINT ( 'NONE',  ( -1.153438870374268843, -80.13165335068218553, -0.4814466031038698302 ) ) ;
#46052 = CARTESIAN_POINT ( 'NONE',  ( -7.710095619848000403, -57.04935285743999884, 10.18496935399999970 ) ) ;
#46053 = LINE ( 'NONE', #14143, #51385 ) ;
#46054 = CARTESIAN_POINT ( 'NONE',  ( 3.620209227049822953, -86.25171438276198899, -1.611820994701397725 ) ) ;
#46055 = CARTESIAN_POINT ( 'NONE',  ( -8.838834764832000701, -23.25000000000000000, -8.838834764832000701 ) ) ;
#46056 = CARTESIAN_POINT ( 'NONE',  ( 1.461966789315192861, -78.07977498547253958, -0.3730248769685299282 ) ) ;
#46057 = CARTESIAN_POINT ( 'NONE',  ( 0.2238869547411186378, -80.58854166667283891, -4.045564205103767463 ) ) ;
#46058 = ORIENTED_EDGE ( 'NONE', *, *, #26674, .F. ) ;
#46059 = CARTESIAN_POINT ( 'NONE',  ( -1.243547092045992564, -77.68541666666665435, 9.499999999999994671 ) ) ;
#46060 = CARTESIAN_POINT ( 'NONE',  ( 12.21199139566000014, -76.24271386089000657, 1.550091862394999964 ) ) ;
#46061 = CARTESIAN_POINT ( 'NONE',  ( -8.596418555780431348, -77.55208333333331439, -6.606377239730338857 ) ) ;
#46062 = CARTESIAN_POINT ( 'NONE',  ( 2.863104762478203558, -2.049854368984712405, -2.050083987754392822 ) ) ;
#46063 = CARTESIAN_POINT ( 'NONE',  ( 7.645398488040000551, -60.01531609111000165, -10.18948971875999909 ) ) ;
#46064 = CARTESIAN_POINT ( 'NONE',  ( 9.889431646000000242, -78.81768700370000147, 7.252463523969000292 ) ) ;
#46065 = CARTESIAN_POINT ( 'NONE',  ( 2.548493721447000038, -76.92447129603100109, 12.01365081398999912 ) ) ;
#46066 = DIRECTION ( 'NONE',  ( 0.000000000000000000, -1.000000000000000000, 0.000000000000000000 ) ) ;
#46067 = CARTESIAN_POINT ( 'NONE',  ( 11.26616169758000119, -78.37118338113400284, 0.05236123134324000700 ) ) ;
#46068 = CARTESIAN_POINT ( 'NONE',  ( 2.355521564011713309, -2.790126448396267111, -2.238901740357879699 ) ) ;
#46069 = CARTESIAN_POINT ( 'NONE',  ( 11.93997985869404310, -77.31377101359005621, 2.095138499075543059 ) ) ;
#46070 = CARTESIAN_POINT ( 'NONE',  ( 8.733858618705999888, -78.44602246771752618, -7.038306768505999678 ) ) ;
#46071 = B_SPLINE_SURFACE_WITH_KNOTS ( 'NONE', 3, 3, ( 
 ( #55344, #46218, #10476, #14017, #28167, #14598, #42060, #33177, #32885, #50929, #51224, #28462, #18750, #9603, #1927, #41766, #24346, #46511, #6331, #19334, #45925, #9895, #27589, #6035, #23175, #54762, #24044, #10189, #1631, #36745, #19620, #55636, #15187, #10776, #5172 ),
 ( #28754, #36455, #42357, #41183, #1057, #54482, #32015, #773, #14305, #32299, #50345, #27877, #5458, #24633, #20211, #55935, #7492, #7200, #29904, #43510, #38493, #47959, #21065, #43223, #25489, #56798, #15772, #16065, #3070, #38202, #39069, #25204, #24920, #29052, #52086 ),
 ( #16357, #33764, #19920, #42937, #56222, #47091, #34338, #6913, #51802, #37910, #52374, #15485, #2491, #11356, #11927, #33475, #20497, #29334, #51512, #34048, #11072, #2779, #6622, #42645, #2212, #47381, #56509, #11645, #29622, #47676, #20778, #38779, #10370, #36931, #54944 ),
 ( #10087, #15381, #32780, #27776, #55531, #14783, #46404, #50532, #6223, #24238, #14202, #46113, #23648, #9790, #51121, #37221, #42256, #28066, #45819, #10964, #956, #28947, #24527, #37809, #1240, #46989, #50240, #33375, #41374, #23363, #28358, #14495, #51411, #10674, #6517 ) ),
 .UNSPECIFIED., .F., .F., .F.,
 ( 4, 4 ),
 ( 4, 1, 1, 1, 1, 1, 1, 1, 1, 1, 1, 1, 1, 1, 1, 1, 1, 1, 1, 1, 1, 1, 1, 1, 1, 1, 1, 1, 1, 1, 1, 1, 4 ),
 ( -0.1377334280162000046, 1.137733428016000081 ),
 ( -0.02000000000000000042, 0.01250000000000000069, 0.04499999999999999833, 0.07749999999999999944, 0.1100000000000000006, 0.1424999999999999878, 0.1749999999999999889, 0.2074999999999999900, 0.2399999999999999911, 0.2725000000000000200, 0.3049999999999999933, 0.3375000000000000222, 0.3699999999999999956, 0.4025000000000000244, 0.4349999999999999978, 0.4675000000000000266, 0.5000000000000000000, 0.5324999999999999734, 0.5649999999999999467, 0.5975000000000000311, 0.6300000000000000044, 0.6624999999999999778, 0.6949999999999999512, 0.7275000000000000355, 0.7600000000000000089, 0.7924999999999999822, 0.8249999999999999556, 0.8575000000000000400, 0.8900000000000000133, 0.9224999999999999867, 0.9549999999999999600, 0.9875000000000000444, 1.020000000000000018 ),
 .UNSPECIFIED. ) ;
#46072 = ORIENTED_EDGE ( 'NONE', *, *, #42868, .T. ) ;
#46073 = CARTESIAN_POINT ( 'NONE',  ( -1.135826688880000157, -81.30663953507000485, -0.9797437077257000748 ) ) ;
#46074 = CARTESIAN_POINT ( 'NONE',  ( -9.483626256930000054, -77.39407522740199852, -0.1248487836051000166 ) ) ;
#46075 = CARTESIAN_POINT ( 'NONE',  ( -2.299999999999999822, -77.50000000000000000, 0.000000000000000000 ) ) ;
#46076 = DIRECTION ( 'NONE',  ( -0.7071067811865474617, 0.7071067811865474617, 1.027168116582069423E-09 ) ) ;
#46077 = CARTESIAN_POINT ( 'NONE',  ( 0.7203371404106000409, -1.934275774374000001, -3.802791496513000080 ) ) ;
#46078 = CARTESIAN_POINT ( 'NONE',  ( -11.12530226251999999, -77.97748971612699620, 4.628544181647000322 ) ) ;
#46079 = CARTESIAN_POINT ( 'NONE',  ( -8.012466620630000591, -78.25374277172099369, -5.343555802860000981 ) ) ;
#46080 = AXIS2_PLACEMENT_3D ( 'NONE', #24060, #14614, #32608 ) ;
#46081 = CARTESIAN_POINT ( 'NONE',  ( 8.345306581575338001, -76.01155566110702466, 8.271040368256810993 ) ) ;
#46082 = CARTESIAN_POINT ( 'NONE',  ( 5.825949712413000192, -80.35679326027729985, 9.232191225927998346 ) ) ;
#46083 = CARTESIAN_POINT ( 'NONE',  ( -2.350111744379518086, -86.07390000031791999, 3.172282531658503046 ) ) ;
#46084 = VERTEX_POINT ( 'NONE', #15654 ) ;
#46085 = DIRECTION ( 'NONE',  ( 0.000000000000000000, 1.000000000000000000, 0.000000000000000000 ) ) ;
#46086 = CARTESIAN_POINT ( 'NONE',  ( -0.2201363562291999698, -79.36327907013999550, -1.483758735329000045 ) ) ;
#46087 = CARTESIAN_POINT ( 'NONE',  ( -6.543376917090838241, -76.27791085602611076, -9.759379282097372155 ) ) ;
#46088 = CARTESIAN_POINT ( 'NONE',  ( -7.022507694776999543, -79.42070304043799922, 8.434951230355999030 ) ) ;
#46089 = DIRECTION ( 'NONE',  ( 0.000000000000000000, -1.000000000000000000, 0.000000000000000000 ) ) ;
#46090 = CARTESIAN_POINT ( 'NONE',  ( -11.53519992361999869, -75.85018925673099943, 3.464787243407999817 ) ) ;
#46091 = DIRECTION ( 'NONE',  ( 0.000000000000000000, 1.000000000000000000, 0.000000000000000000 ) ) ;
#46092 = CARTESIAN_POINT ( 'NONE',  ( 7.631889106325000505, -18.77878585407000145, -10.36222439674000029 ) ) ;
#46093 = CARTESIAN_POINT ( 'NONE',  ( -5.747123378374999980, -78.21567021303999923, 10.24856442990000005 ) ) ;
#46094 = EDGE_LOOP ( 'NONE', ( #40640, #29204, #17322, #40647 ) ) ;
#46095 = CARTESIAN_POINT ( 'NONE',  ( 11.14673908614000020, -78.45935830175899639, 0.06930530262389000828 ) ) ;
#46096 = CARTESIAN_POINT ( 'NONE',  ( 0.000000000000000000, 4.040000000000000036, 0.000000000000000000 ) ) ;
#46097 = COLOUR_RGB ( '', 0.66274510, 0.83137255, 0.94901961) ;
#46098 = CARTESIAN_POINT ( 'NONE',  ( 12.50485632861550833, -53.93407884522628137, 0.6924337384548601149 ) ) ;
#46099 = CARTESIAN_POINT ( 'NONE',  ( -0.03561159147831179095, -78.40681307243319509, 3.778384673934156002 ) ) ;
#46100 = EDGE_CURVE ( 'NONE', #39575, #16917, #5747, .T. ) ;
#46101 = CARTESIAN_POINT ( 'NONE',  ( -6.398554566410420641, -77.37244341094226741, 10.23462864614716139 ) ) ;
#46103 = CARTESIAN_POINT ( 'NONE',  ( -1.249625625013177643, -81.59763177894343755, 0.04702936436425671218 ) ) ;
#46102 = CARTESIAN_POINT ( 'NONE',  ( 1.208351632240000084, -81.37518792952799629, -0.5295771361605000616 ) ) ;
#46104 = CARTESIAN_POINT ( 'NONE',  ( -2.935661446561999899, -77.00000000000000000, -9.035036904803998681 ) ) ;
#46105 = DIRECTION ( 'NONE',  ( 0.000000000000000000, -1.000000000000000000, 0.000000000000000000 ) ) ;
#46106 = CARTESIAN_POINT ( 'NONE',  ( 1.224841740086000108, -78.85854862992999870, 0.4588522236800000043 ) ) ;
#46107 = DIRECTION ( 'NONE',  ( 0.000000000000000000, 1.000000000000000000, 0.000000000000000000 ) ) ;
#46108 = CARTESIAN_POINT ( 'NONE',  ( 7.318212639625410354, -79.63318163283004480, -8.179950038113810606 ) ) ;
#46109 = EDGE_CURVE ( 'NONE', #26404, #1613, #53901, .T. ) ;
#46110 = CARTESIAN_POINT ( 'NONE',  ( 6.043427764450761686, -77.13333333333329733, 10.48543666025110888 ) ) ;
#46111 = ORIENTED_EDGE ( 'NONE', *, *, #38049, .F. ) ;
#46112 = ORIENTED_EDGE ( 'NONE', *, *, #57691, .F. ) ;
#46113 = CARTESIAN_POINT ( 'NONE',  ( 10.02101539056000057, -78.63063998579799829, 0.1637206938138999757 ) ) ;
#46114 = CARTESIAN_POINT ( 'NONE',  ( 9.130635980787438655, -78.80587905097618773, -5.674270332481268220 ) ) ;
#46115 = VERTEX_POINT ( 'NONE', #27306 ) ;
#46116 = CARTESIAN_POINT ( 'NONE',  ( -10.31421052434999908, -76.72175206120299151, 3.823226550887000030 ) ) ;
#46117 = CARTESIAN_POINT ( 'NONE',  ( 2.064266695395271967, -82.66979168306330905, 2.715591382896376249 ) ) ;
#46118 = AXIS2_PLACEMENT_3D ( 'NONE', #9744, #27144, #41328 ) ;
#46119 = CARTESIAN_POINT ( 'NONE',  ( -9.500135819972072682, -79.39737933951445825, 0.3021342893088184156 ) ) ;
#46120 = EDGE_CURVE ( 'NONE', #54581, #34281, #23464, .T. ) ;
#46121 = B_SPLINE_CURVE_WITH_KNOTS ( 'NONE', 3,
 ( #30323, #8774, #35923, #22347, #17335, #35034, #17053, #49225, #48933, #25903, #8475, #57489, #39488, #43927, #4347, #8192, #43637, #44494 ),
 .UNSPECIFIED., .F., .F.,
 ( 4, 2, 2, 2, 2, 2, 2, 2, 4 ),
 ( 0.000000000000000000, 0.1250000000000000000, 0.2500000000000000000, 0.3750000000000000000, 0.5000000000000000000, 0.6250000000000000000, 0.7500000000000000000, 0.8750000000000000000, 1.000000000000000000 ),
 .UNSPECIFIED. ) ;
#46122 = CARTESIAN_POINT ( 'NONE',  ( 7.956422463042999382, -61.32889896150999931, 9.787948076380001083 ) ) ;
#46123 = CARTESIAN_POINT ( 'NONE',  ( -10.52651887844270640, -77.00721078521108609, 6.166402933938996966 ) ) ;
#46124 = CARTESIAN_POINT ( 'NONE',  ( -7.615957885411051009, -78.47972809508038949, 9.247549774705609238 ) ) ;
#46125 = CARTESIAN_POINT ( 'NONE',  ( -2.848564863371000122, -78.87067295193800476, -10.84913769893999991 ) ) ;
#46126 = EDGE_CURVE ( 'NONE', #8817, #1475, #50060, .T. ) ;
#46127 = ORIENTED_EDGE ( 'NONE', *, *, #58377, .F. ) ;
#46128 = CARTESIAN_POINT ( 'NONE',  ( 7.648026766753000416, -60.05000000550000294, -10.12290050090999927 ) ) ;
#46129 = VERTEX_POINT ( 'NONE', #15488 ) ;
#46130 = CARTESIAN_POINT ( 'NONE',  ( 7.481666628245163153, -77.40013210855786951, 5.439281462751108798 ) ) ;
#46131 = CARTESIAN_POINT ( 'NONE',  ( 2.604371601988999974, -77.51379954448199783, -10.72853197743999942 ) ) ;
#46132 = DIRECTION ( 'NONE',  ( 0.000000000000000000, -1.000000000000000000, 0.000000000000000000 ) ) ;
#46133 = FACE_OUTER_BOUND ( 'NONE', #22098, .T. ) ;
#46134 = CARTESIAN_POINT ( 'NONE',  ( 6.043427764450807871, -77.56666666666667709, -10.48543666025108756 ) ) ;
#46135 = AXIS2_PLACEMENT_3D ( 'NONE', #43210, #42926, #1615 ) ;
#46136 = CARTESIAN_POINT ( 'NONE',  ( -9.722718241315000398, -55.35321828636000419, -7.954951288349001004 ) ) ;
#46137 = CARTESIAN_POINT ( 'NONE',  ( -0.9156221410628999635, -78.13372563058999276, 1.345473579290000110 ) ) ;
#46138 = CARTESIAN_POINT ( 'NONE',  ( 10.07627163191000008, -55.55000000278000272, 7.601397897754999633 ) ) ;
#46139 = CARTESIAN_POINT ( 'NONE',  ( 6.064331118019999245, -78.60094147377398599, -9.105586440592000841 ) ) ;
#46140 = CARTESIAN_POINT ( 'NONE',  ( -7.658894224177999810, -23.20939395863999977, -10.01676912201999947 ) ) ;
#46141 = CARTESIAN_POINT ( 'NONE',  ( 12.53241208775999915, -59.56462890159999546, -1.667936697358999965 ) ) ;
#46142 = CARTESIAN_POINT ( 'NONE',  ( 3.270705966882999860, -85.26804551122299358, 1.847660810087999872 ) ) ;
#46143 = ORIENTED_EDGE ( 'NONE', *, *, #12879, .F. ) ;
#46144 = CARTESIAN_POINT ( 'NONE',  ( -9.886087410963998678, -78.82155766632499194, 7.540251870238000365 ) ) ;
#46145 = CARTESIAN_POINT ( 'NONE',  ( -10.85352824271999950, -76.76177769904698778, 2.043985636521999716 ) ) ;
#46146 = CARTESIAN_POINT ( 'NONE',  ( 4.666043224853492433, -77.93943897360074402, 9.684446864717223491 ) ) ;
#46147 = CARTESIAN_POINT ( 'NONE',  ( -5.261498566940000288, -77.72271004462599819, -10.76255997729999869 ) ) ;
#46148 = EDGE_CURVE ( 'NONE', #3255, #30832, #6334, .T. ) ;
#46149 = DIRECTION ( 'NONE',  ( -1.000000000000000000, 0.000000000000000000, 0.000000000000000000 ) ) ;
#46150 = DIRECTION ( 'NONE',  ( 0.7071067811865474617, 0.000000000000000000, 0.7071067811865474617 ) ) ;
#46151 = CARTESIAN_POINT ( 'NONE',  ( -2.822700266548876069, -3.300972420264427498, -2.107553880886188669 ) ) ;
#46152 = CARTESIAN_POINT ( 'NONE',  ( 9.340454417440403390, -80.89149709199956817, 5.322469657822352929 ) ) ;
#46153 = CARTESIAN_POINT ( 'NONE',  ( 9.400066902809999903, -78.32495809405799037, -0.4999367261865000356 ) ) ;
#46154 = CARTESIAN_POINT ( 'NONE',  ( 3.184161977317978565, -85.88547957940599531, -1.417680250971047773 ) ) ;
#46155 = CARTESIAN_POINT ( 'NONE',  ( 3.871217329169000188, -77.23791202109900667, 10.45314674924000009 ) ) ;
#46156 = CARTESIAN_POINT ( 'NONE',  ( 0.4479210110389621469, -0.8346353966065711560, -3.415364800656486288 ) ) ;
#46157 = CARTESIAN_POINT ( 'NONE',  ( 0.5267042291526000675, -80.83006063909182615, 11.01316230888000014 ) ) ;
#46158 = VERTEX_POINT ( 'NONE', #46514 ) ;
#46159 = DIRECTION ( 'NONE',  ( 1.000000000000000000, 0.000000000000000000, 0.000000000000000000 ) ) ;
#46160 = CARTESIAN_POINT ( 'NONE',  ( -6.606862979243170564, -80.52715448066929582, 8.596965208648541079 ) ) ;
#46161 = AXIS2_PLACEMENT_3D ( 'NONE', #50314, #27844, #47930 ) ;
#46162 = CARTESIAN_POINT ( 'NONE',  ( -11.12496554189999998, -77.20851078140199775, -1.432917402686000097 ) ) ;
#46163 = CARTESIAN_POINT ( 'NONE',  ( -1.297526016723000053, -78.42511598777798554, -10.89864408161000142 ) ) ;
#46164 = CARTESIAN_POINT ( 'NONE',  ( 7.646788277333999240, -23.37228598377000210, -10.00831419131999844 ) ) ;
#46165 = CARTESIAN_POINT ( 'NONE',  ( 1.298082172566151549, -82.74687498353479498, 3.823617033396692122 ) ) ;
#46166 = CARTESIAN_POINT ( 'NONE',  ( 3.248892733988256953, -1.861934577303119953, 0.4260366050094578916 ) ) ;
#46167 = CARTESIAN_POINT ( 'NONE',  ( -9.848035040979025823, -53.97131634255971022, -8.114786739965461848 ) ) ;
#46168 = CARTESIAN_POINT ( 'NONE',  ( 4.043204716307999824, -83.99067953870898862, 1.029097049655000040 ) ) ;
#46169 = VECTOR ( 'NONE', #42655, 1000.000000000000114 ) ;
#46170 = CARTESIAN_POINT ( 'NONE',  ( -7.686918321190000292, -21.75560170997999876, -10.48771805380000011 ) ) ;
#46171 = CARTESIAN_POINT ( 'NONE',  ( 6.196431984783000502, -79.15908388498999670, -11.36888734437999915 ) ) ;
#46172 = CARTESIAN_POINT ( 'NONE',  ( -7.880862184694999328, -76.71482100489700429, 7.737503720428000165 ) ) ;
#46173 = CARTESIAN_POINT ( 'NONE',  ( -1.603789611582999930, -80.23297560169000064, -0.4506860216877000558 ) ) ;
#46174 = CARTESIAN_POINT ( 'NONE',  ( 1.066267001953999927, -78.21979887042999735, -0.7783007006953001072 ) ) ;
#46175 = CARTESIAN_POINT ( 'NONE',  ( 9.000000000000000000, -80.79999999999999716, 0.000000000000000000 ) ) ;
#46176 = CARTESIAN_POINT ( 'NONE',  ( 0.04619448413486952620, -81.37749121868887414, -1.509966902698022251 ) ) ;
#46177 = VECTOR ( 'NONE', #52678, 999.9999999999998863 ) ;
#46178 = CARTESIAN_POINT ( 'NONE',  ( -1.500128069024530220, -83.33926479430419931, 0.1908857210655489633 ) ) ;
#46179 = CARTESIAN_POINT ( 'NONE',  ( -5.971441230830989433, -80.17821172891612491, -8.938866158933542749 ) ) ;
#46180 = CARTESIAN_POINT ( 'NONE',  ( -9.252740428348994683, -77.82083333333332575, -2.486604901413163926 ) ) ;
#46181 = CONICAL_SURFACE ( 'NONE', #34796, 0.6999999997694995590, 0.7853981633972997312 ) ;
#46182 = CARTESIAN_POINT ( 'NONE',  ( -0.9218200799623714747, -77.97291666666667709, -1.199500263597270466 ) ) ;
#46183 = VERTEX_POINT ( 'NONE', #15190 ) ;
#46184 = CARTESIAN_POINT ( 'NONE',  ( -0.4655645666672672545, -81.69477528390797261, -1.159972523025642799 ) ) ;
#46185 = ADVANCED_FACE ( 'NONE', ( #14890 ), #24047, .T. ) ;
#46186 =( NAMED_UNIT ( * ) PLANE_ANGLE_UNIT ( ) SI_UNIT ( $, .RADIAN. ) );
#46187 = CARTESIAN_POINT ( 'NONE',  ( 10.52346617262000095, -78.61439489434398808, -3.675769182893000142 ) ) ;
#46188 = FACE_OUTER_BOUND ( 'NONE', #56050, .T. ) ;
#46189 = ORIENTED_EDGE ( 'NONE', *, *, #39701, .F. ) ;
#46190 = EDGE_LOOP ( 'NONE', ( #53404, #14853, #37885, #39702 ) ) ;
#46191 = EDGE_CURVE ( 'NONE', #3682, #56978, #33181, .T. ) ;
#46192 = CARTESIAN_POINT ( 'NONE',  ( 1.399266414090999833, -81.86555509899200445, 0.2282827057232000301 ) ) ;
#46193 = ORIENTED_EDGE ( 'NONE', *, *, #14062, .F. ) ;
#46194 = ORIENTED_EDGE ( 'NONE', *, *, #738, .F. ) ;
#46195 = CARTESIAN_POINT ( 'NONE',  ( -1.500000000000000888, -81.98958333334674364, 0.1963495408493559080 ) ) ;
#46196 = DIRECTION ( 'NONE',  ( 0.000000000000000000, -1.000000000000000000, 0.000000000000000000 ) ) ;
#46197 = PRODUCT_CONTEXT ( 'NONE', #58302, 'mechanical' ) ;
#46198 = CARTESIAN_POINT ( 'NONE',  ( -2.442701056171530105, -81.51354165288981335, 2.427965435584034104 ) ) ;
#46199 = CARTESIAN_POINT ( 'NONE',  ( 7.050495581552580049, -78.29403130279574441, -5.987855718153151763 ) ) ;
#46200 = CARTESIAN_POINT ( 'NONE',  ( 6.606377239730347739, -78.17708333333328596, -8.596418555780422466 ) ) ;
#46201 = ADVANCED_FACE ( 'NONE', ( #29625 ), #16071, .F. ) ;
#46202 = ORIENTED_EDGE ( 'NONE', *, *, #6554, .F. ) ;
#46203 = VERTEX_POINT ( 'NONE', #38496 ) ;
#46204 = CARTESIAN_POINT ( 'NONE',  ( -8.449677353798556112, -77.56661759170884807, 3.770595868082258217 ) ) ;
#46205 = DIRECTION ( 'NONE',  ( 0.7071067811865975328, -0.7071067811864976127, -2.062935344748993860E-09 ) ) ;
#46206 = DIRECTION ( 'NONE',  ( 0.000000000000000000, 1.000000000000000000, 0.000000000000000000 ) ) ;
#46207 = CARTESIAN_POINT ( 'NONE',  ( 0.04193593612906149071, -16.98990258663310726, 12.50649570005709599 ) ) ;
#46208 = CARTESIAN_POINT ( 'NONE',  ( 5.091895231007000255, -78.60089172978399574, 8.260951054388000259 ) ) ;
#46209 = CARTESIAN_POINT ( 'NONE',  ( 3.938458446976999205, -79.30999999999998806, -8.369650235310999165 ) ) ;
#46210 = CARTESIAN_POINT ( 'NONE',  ( 3.326798747144231516, -85.83867307182441664, 1.964420495601435057 ) ) ;
#46211 = CARTESIAN_POINT ( 'NONE',  ( 7.255994938323000021, -78.09084413521999579, -10.73374472359000009 ) ) ;
#46212 = CARTESIAN_POINT ( 'NONE',  ( 1.340661125304000167, -80.85989310931999796, -0.5992281077721001159 ) ) ;
#46213 = CARTESIAN_POINT ( 'NONE',  ( -8.838834764832000701, -18.75000000000000000, -8.838834764832000701 ) ) ;
#46214 = CARTESIAN_POINT ( 'NONE',  ( 0.02731002720095722369, -76.57469656089436683, 11.74987924982600696 ) ) ;
#46215 = CARTESIAN_POINT ( 'NONE',  ( 2.485497987250000040, -79.28373615087838289, -3.354386240666999974 ) ) ;
#46217 = CIRCLE ( 'NONE', #49009, 2.600000000000000089 ) ;
#46216 = CARTESIAN_POINT ( 'NONE',  ( 7.496935112050000072, -80.58316208623270427, 8.408636027568000770 ) ) ;
#46218 = CARTESIAN_POINT ( 'NONE',  ( 5.259675013629999896, -79.24294334753599856, -7.751687108632999035 ) ) ;
#46219 = CARTESIAN_POINT ( 'NONE',  ( 10.20076089109330120, -76.82412226148122159, -3.463745884883634663 ) ) ;
#46220 = ADVANCED_FACE ( 'NONE', ( #19337 ), #24349, .T. ) ;
#46221 = CARTESIAN_POINT ( 'NONE',  ( 0.5658835715479000328, -82.12580496681198383, -3.501612269639000186 ) ) ;
#46222 = CIRCLE ( 'NONE', #37, 9.700000000000001066 ) ;
#46224 = CARTESIAN_POINT ( 'NONE',  ( -1.112801787005999854, -79.26242257069900177, -0.6258220204580999813 ) ) ;
#46223 = CARTESIAN_POINT ( 'NONE',  ( 5.136988255280226845, -77.27767399912663393, -10.56734161811198369 ) ) ;
#46225 = DIRECTION ( 'NONE',  ( 0.000000000000000000, 1.000000000000000000, 0.000000000000000000 ) ) ;
#46226 = CARTESIAN_POINT ( 'NONE',  ( -12.50240681836000078, -61.48234730679999416, 1.005418944265999981 ) ) ;
#46227 = CARTESIAN_POINT ( 'NONE',  ( -3.268529449828999844, -2.360140595155999943, -1.950076325099000085 ) ) ;
#46228 = DIRECTION ( 'NONE',  ( 1.000000000000000000, 0.000000000000000000, 0.000000000000000000 ) ) ;
#46229 = ORIENTED_EDGE ( 'NONE', *, *, #43089, .F. ) ;
#46230 = CARTESIAN_POINT ( 'NONE',  ( -3.399186938124999724, -80.19999999999998863, -10.46162167925000119 ) ) ;
#46231 = CARTESIAN_POINT ( 'NONE',  ( 0.5200379331660126558, -18.54844303601859679, -10.98772212209857102 ) ) ;
#46232 = CARTESIAN_POINT ( 'NONE',  ( -7.217346475716882814, -77.62574498632518782, 9.390375165279603920 ) ) ;
#46233 = CARTESIAN_POINT ( 'NONE',  ( 1.667917367065999912, -60.08056535122999975, 12.49306764019000049 ) ) ;
#46234 = CARTESIAN_POINT ( 'NONE',  ( -12.54981748959999877, -53.75163512338999539, -0.03767836620429999839 ) ) ;
#46235 = CARTESIAN_POINT ( 'NONE',  ( 9.171086888450156849, -79.39389370609096375, 5.639578953327716526 ) ) ;
#46236 = ADVANCED_FACE ( 'NONE', ( #20500 ), #42065, .F. ) ;
#46237 = CARTESIAN_POINT ( 'NONE',  ( 7.651633708404999901, -79.64221332859899860, -5.680134239085999681 ) ) ;
#46238 = DIRECTION ( 'NONE',  ( -0.9999999999999693578, 2.479738204331925575E-07, -1.114546890695966335E-12 ) ) ;
#46239 = CARTESIAN_POINT ( 'NONE',  ( -0.008314555494097999877, -77.61812138891799862, 11.16535427852999973 ) ) ;
#46240 = CARTESIAN_POINT ( 'NONE',  ( -1.520492615867999886, -82.42132092353099893, -0.2596922552208000279 ) ) ;
#46241 = FACE_OUTER_BOUND ( 'NONE', #35541, .T. ) ;
#46243 = CARTESIAN_POINT ( 'NONE',  ( 0.5999999999999999778, -5.000000000000000000, 0.5999999999999999778 ) ) ;
#46242 = CARTESIAN_POINT ( 'NONE',  ( -3.722292034697000318, -82.86303720588698241, 0.5058778948779999451 ) ) ;
#46244 = CARTESIAN_POINT ( 'NONE',  ( -6.053394164830000257, -79.76055584965399703, -7.392643757108000813 ) ) ;
#46245 = CARTESIAN_POINT ( 'NONE',  ( 0.7681833999686451531, -82.67708333333334281, -0.9995835529977240563 ) ) ;
#46246 = CARTESIAN_POINT ( 'NONE',  ( -0.1680659145979999936, -80.54322239898399971, 1.308557476745999981 ) ) ;
#46247 = LINE ( 'NONE', #33208, #50386 ) ;
#46248 = CARTESIAN_POINT ( 'NONE',  ( 7.954951288349001004, -60.24678171298000251, 9.722718241315000398 ) ) ;
#46249 = B_SPLINE_CURVE_WITH_KNOTS ( 'NONE', 3,
 ( #12034, #53047, #7308, #16752, #38600, #17034 ),
 .UNSPECIFIED., .F., .F.,
 ( 4, 2, 4 ),
 ( 0.000000000000000000, 0.5000000000000000000, 1.000000000000000000 ),
 .UNSPECIFIED. ) ;
#46250 = CARTESIAN_POINT ( 'NONE',  ( -3.778552491321031770, -78.99318692756679638, 7.557104982642018243 ) ) ;
#46251 = ORIENTED_EDGE ( 'NONE', *, *, #23582, .F. ) ;
#46252 = ORIENTED_EDGE ( 'NONE', *, *, #54364, .F. ) ;
#46253 = CARTESIAN_POINT ( 'NONE',  ( -6.309004353333000026, -79.28274924709700144, -10.24224633278999796 ) ) ;
#46254 = EDGE_CURVE ( 'NONE', #1613, #604, #47657, .T. ) ;
#46255 = CARTESIAN_POINT ( 'NONE',  ( -12.50385649911392605, -61.58436722984689027, -0.8579675320882300671 ) ) ;
#46256 = DIRECTION ( 'NONE',  ( 0.000000000000000000, 0.000000000000000000, -1.000000000000000000 ) ) ;
#46257 = ORIENTED_EDGE ( 'NONE', *, *, #44602, .T. ) ;
#46258 = EDGE_CURVE ( 'NONE', #19498, #46158, #49022, .T. ) ;
#46259 = CARTESIAN_POINT ( 'NONE',  ( -10.57592698605000159, -78.66175121120100755, -5.530395178621999364 ) ) ;
#46260 = VERTEX_POINT ( 'NONE', #7205 ) ;
#46261 = ORIENTED_EDGE ( 'NONE', *, *, #20636, .F. ) ;
#46262 = AXIS2_PLACEMENT_3D ( 'NONE', #17465, #31023, #21033 ) ;
#46263 = CARTESIAN_POINT ( 'NONE',  ( -8.596418555780466875, -78.94791666666665719, 6.606377239730298001 ) ) ;
#46264 = CIRCLE ( 'NONE', #55683, 0.5000000000000000000 ) ;
#46265 = ORIENTED_EDGE ( 'NONE', *, *, #46120, .T. ) ;
#46266 = CARTESIAN_POINT ( 'NONE',  ( -3.238101123710000362, -78.61343171100860161, 1.037346680369000129 ) ) ;
#46267 = CARTESIAN_POINT ( 'NONE',  ( -0.5999999999999999778, -18.84999999999000053, -11.79999999999999893 ) ) ;
#46268 = ORIENTED_EDGE ( 'NONE', *, *, #41580, .F. ) ;
#46270 = EDGE_CURVE ( 'NONE', #53710, #5930, #26878, .T. ) ;
#46269 = CARTESIAN_POINT ( 'NONE',  ( 1.250000000000000000, -82.84999999999999432, 0.000000000000000000 ) ) ;
#46271 = CARTESIAN_POINT ( 'NONE',  ( -7.705119999435999567, -57.04828923575999511, 10.24996238029999951 ) ) ;
#46272 = ORIENTED_EDGE ( 'NONE', *, *, #49041, .F. ) ;
#46273 = CARTESIAN_POINT ( 'NONE',  ( 1.001315002179999913, -17.31477588286000113, 12.50000000000000000 ) ) ;
#46274 = CARTESIAN_POINT ( 'NONE',  ( -8.592462595181881824, -78.31143903816993657, 4.510367428545268176 ) ) ;
#46275 = CARTESIAN_POINT ( 'NONE',  ( 0.000000000000000000, -77.70312499986998489, -1.546875000130000011 ) ) ;
#46276 = CARTESIAN_POINT ( 'NONE',  ( -12.50745077490000057, -17.00005551713000074, 2.011909873286000185E-09 ) ) ;
#46277 = CARTESIAN_POINT ( 'NONE',  ( 2.076475668830000121, -76.12624427606199617, 10.98918251355999942 ) ) ;
#46278 = DIRECTION ( 'NONE',  ( 0.000000000000000000, 1.000000000000000000, 0.000000000000000000 ) ) ;
#46279 = CARTESIAN_POINT ( 'NONE',  ( 1.217465845835394855, -81.22916666666665719, -0.3271848554490981997 ) ) ;
#46280 = CARTESIAN_POINT ( 'NONE',  ( -7.654537085048000122, -60.08056692637000396, -10.01332844639000008 ) ) ;
#46281 = CARTESIAN_POINT ( 'NONE',  ( 5.893929754856348957, -78.77983637771299641, -7.187357691034195639 ) ) ;
#46282 = AXIS2_PLACEMENT_3D ( 'NONE', #45196, #4744, #56015 ) ;
#46283 = CARTESIAN_POINT ( 'NONE',  ( -1.623939766302999965, -77.68186001420198750, -9.270360727776001397 ) ) ;
#46284 = FACE_OUTER_BOUND ( 'NONE', #29346, .T. ) ;
#46285 = CARTESIAN_POINT ( 'NONE',  ( -5.045463033963281774, -80.18718913546477722, -9.777363391122731784 ) ) ;
#46286 = CARTESIAN_POINT ( 'NONE',  ( 11.74999999999999289, -76.56041666666666856, 1.538071403320028452 ) ) ;
#46287 = CARTESIAN_POINT ( 'NONE',  ( -3.095242434087999595, -81.68442549782599826, -2.734588626640999998 ) ) ;
#46288 = DIRECTION ( 'NONE',  ( -1.000000000000000000, 0.000000000000000000, 0.000000000000000000 ) ) ;
#46289 = CARTESIAN_POINT ( 'NONE',  ( 0.8221611544660735182, -82.91846127699133717, 0.9412421169495641671 ) ) ;
#46290 = CARTESIAN_POINT ( 'NONE',  ( 11.99999999979999821, -18.85000000927000130, 0.7999999997951999786 ) ) ;
#46291 = CARTESIAN_POINT ( 'NONE',  ( 0.000000000000000000, -76.75499999999999545, 0.000000000000000000 ) ) ;
#46292 = CARTESIAN_POINT ( 'NONE',  ( 1.324099017018209867, -81.99695209267724749, -0.05344395349994826572 ) ) ;
#46293 = CARTESIAN_POINT ( 'NONE',  ( 5.220449009264826579, -79.99999999999997158, 7.789606664612244380 ) ) ;
#46294 = DIRECTION ( 'NONE',  ( -0.9999999924279685537, 0.000000000000000000, -0.0001230612157848962919 ) ) ;
#46295 = CARTESIAN_POINT ( 'NONE',  ( 0.000000000000000000, -76.75499999999999545, 0.000000000000000000 ) ) ;
#46296 = CARTESIAN_POINT ( 'NONE',  ( -1.807051837523000026, -24.30078415243000123, -12.77977401834999860 ) ) ;
#46297 = CIRCLE ( 'NONE', #28346, 12.50000000000000000 ) ;
#46298 = DIRECTION ( 'NONE',  ( 0.9999463328794432337, 0.000000000000000000, -0.01036008498777044214 ) ) ;
#46299 = CARTESIAN_POINT ( 'NONE',  ( -0.4716531882653000052, -2.930179953964000106, 3.453513650901000265 ) ) ;
#46300 = CARTESIAN_POINT ( 'NONE',  ( 12.55486071735000131, -24.15393633008000407, 1.580832792524999864 ) ) ;
#46301 = CARTESIAN_POINT ( 'NONE',  ( -0.9995835529977249445, -80.55208333333331439, -0.7681833999686439318 ) ) ;
#46302 = EDGE_CURVE ( 'NONE', #42030, #31323, #24996, .T. ) ;
#46303 = CARTESIAN_POINT ( 'NONE',  ( 6.187157694146999454, -77.70638901018298839, 10.60730214752000045 ) ) ;
#46304 = CARTESIAN_POINT ( 'NONE',  ( -10.76076152244900719, -78.11906335555218561, -2.634765227118816444 ) ) ;
#46306 = CARTESIAN_POINT ( 'NONE',  ( -7.357853812480288802, -79.78374948186821314, 8.079057253869311950 ) ) ;
#46305 = CARTESIAN_POINT ( 'NONE',  ( -1.199500263597270022, -80.05208333333334281, -0.9218200799623730290 ) ) ;
#46307 = CARTESIAN_POINT ( 'NONE',  ( -10.23598640736999954, -76.21444405523999421, -6.660190322323000345 ) ) ;
#46308 = VERTEX_POINT ( 'NONE', #24636 ) ;
#46309 = CARTESIAN_POINT ( 'NONE',  ( -3.315791941328000370, -83.23582450217399753, 2.462524611965999810 ) ) ;
#46310 = CARTESIAN_POINT ( 'NONE',  ( 7.560470358556999670, -81.02546712712090482, 8.383385420532000865 ) ) ;
#46311 = CARTESIAN_POINT ( 'NONE',  ( 7.864210892918562124, -78.30589158093161473, -4.886453465047767786 ) ) ;
#46312 = CARTESIAN_POINT ( 'NONE',  ( 9.355955347601371486, -53.62516908774130542, 8.610895743687590809 ) ) ;
#46313 = CARTESIAN_POINT ( 'NONE',  ( -5.751434148371999733, -77.98383964426899695, -9.630115047516998317 ) ) ;
#46314 = FACE_OUTER_BOUND ( 'NONE', #6745, .T. ) ;
#46315 = CARTESIAN_POINT ( 'NONE',  ( -7.148970245326999873, -78.95149595525998620, -6.453327391511999522 ) ) ;
#46316 = CARTESIAN_POINT ( 'NONE',  ( 1.496210884224999926, -83.17505483466200644, 0.7325374182646999799 ) ) ;
#46317 = CARTESIAN_POINT ( 'NONE',  ( -7.000000000000000000, -80.99999999999998579, -1.199999999999970424 ) ) ;
#46318 = CARTESIAN_POINT ( 'NONE',  ( -10.88020833321164638, -76.16979166665750256, 1.138827338097790687 ) ) ;
#46319 = ORIENTED_EDGE ( 'NONE', *, *, #19661, .T. ) ;
#46320 = DIRECTION ( 'NONE',  ( 1.000000000000000000, 0.000000000000000000, 0.000000000000000000 ) ) ;
#46321 = CARTESIAN_POINT ( 'NONE',  ( 11.14639666075000157, -80.93674113700730288, -1.632917082138999776 ) ) ;
#46322 = CARTESIAN_POINT ( 'NONE',  ( 12.05000000000000071, -79.29999999999999716, 0.000000000000000000 ) ) ;
#46323 = VERTEX_POINT ( 'NONE', #56227 ) ;
#46324 = CARTESIAN_POINT ( 'NONE',  ( 1.324344358081999795, -78.93751035396100235, 0.1571239973995999795 ) ) ;
#46325 = CARTESIAN_POINT ( 'NONE',  ( 6.365665562422999635, -78.73050366622999263, 10.17242851768000023 ) ) ;
#46326 = ORIENTED_EDGE ( 'NONE', *, *, #48256, .T. ) ;
#46327 = CIRCLE ( 'NONE', #16134, 12.05000000000000071 ) ;
#46328 = EDGE_CURVE ( 'NONE', #10831, #22736, #53265, .T. ) ;
#46329 = CARTESIAN_POINT ( 'NONE',  ( 1.764045786578000152, -77.46325110754499121, -11.99279291753999921 ) ) ;
#46330 = CARTESIAN_POINT ( 'NONE',  ( -12.50000000000000000, -18.75000000000000000, 1.250000000000000000 ) ) ;
#46331 = ORIENTED_EDGE ( 'NONE', *, *, #22764, .F. ) ;
#46332 = ORIENTED_EDGE ( 'NONE', *, *, #15556, .F. ) ;
#46333 = CARTESIAN_POINT ( 'NONE',  ( 0.000000000000000000, -75.10000000019110189, -5.199999999809000073 ) ) ;
#46334 = CARTESIAN_POINT ( 'NONE',  ( 9.226480760116999136, -79.06100957289298492, -2.263195259622999611 ) ) ;
#46335 = ORIENTED_EDGE ( 'NONE', *, *, #42508, .T. ) ;
#46337 = EDGE_CURVE ( 'NONE', #37515, #12596, #53521, .T. ) ;
#46336 = CARTESIAN_POINT ( 'NONE',  ( 12.54705919854999863, -54.26307476595999901, 1.287183453418999868 ) ) ;
#46338 = CARTESIAN_POINT ( 'NONE',  ( 10.91479203715999979, -79.82190303803308495, -0.2066369003937000015 ) ) ;
#46339 = ORIENTED_EDGE ( 'NONE', *, *, #22695, .F. ) ;
#46340 = VECTOR ( 'NONE', #9804, 999.9999999999998863 ) ;
#46341 = CARTESIAN_POINT ( 'NONE',  ( -12.66322140209000047, -25.18161935732999623, -0.1487435796151999889 ) ) ;
#46342 = ADVANCED_FACE ( 'NONE', ( #48523 ), #18885, .F. ) ;
#46343 = CARTESIAN_POINT ( 'NONE',  ( 2.962511214703000384, -77.72019805011500182, -9.021140561863999707 ) ) ;
#46344 = AXIS2_PLACEMENT_3D ( 'NONE', #49726, #155, #36414 ) ;
#46345 = CARTESIAN_POINT ( 'NONE',  ( -1.110657947776001686, -80.13830072341400523, -0.5734848811478387987 ) ) ;
#46346 = CARTESIAN_POINT ( 'NONE',  ( -1.980584515752000119, -18.73514853375999678, -12.76303204602000108 ) ) ;
#46347 = CARTESIAN_POINT ( 'NONE',  ( -12.00000000000000000, -78.79999999999999716, 0.000000000000000000 ) ) ;
#46348 = CARTESIAN_POINT ( 'NONE',  ( -12.70619604133053926, -17.53855724472153454, -1.571828507134811703 ) ) ;
#46349 = CARTESIAN_POINT ( 'NONE',  ( -1.440089456762498221, -78.32070828587532674, 0.5413449664772868042 ) ) ;
#46350 = CYLINDRICAL_SURFACE ( 'NONE', #11481, 1.750000000000001332 ) ;
#46351 = VERTEX_POINT ( 'NONE', #35493 ) ;
#46352 = CARTESIAN_POINT ( 'NONE',  ( -11.84062247810999935, -76.49528801428999714, 3.366775603358000080 ) ) ;
#46353 = FACE_OUTER_BOUND ( 'NONE', #39629, .T. ) ;
#46354 = EDGE_CURVE ( 'NONE', #40498, #22275, #48305, .T. ) ;
#46355 = CARTESIAN_POINT ( 'NONE',  ( 0.000000000000000000, -80.79999999999999716, 0.000000000000000000 ) ) ;
#46356 = CARTESIAN_POINT ( 'NONE',  ( -12.26143800982999998, -79.01887203022999984, -0.2371146996492999870 ) ) ;
#46357 = CARTESIAN_POINT ( 'NONE',  ( -6.620362748380999918, -76.21358782151399680, -10.34376132320999986 ) ) ;
#46358 = CARTESIAN_POINT ( 'NONE',  ( -10.12290050255000118, -55.55000002206000431, -7.648026768392999664 ) ) ;
#46359 = CARTESIAN_POINT ( 'NONE',  ( 12.50728321917716102, -24.99975184167002595, 0.1774118160392116339 ) ) ;
#46360 = CARTESIAN_POINT ( 'NONE',  ( 4.821392521053025959, -78.20771595215950356, -11.06363226005912637 ) ) ;
#46361 = CARTESIAN_POINT ( 'NONE',  ( -10.12290050124000018, -18.75000000007999645, 7.648026767085999822 ) ) ;
#46362 = COLOUR_RGB ( '', 0.66274510, 0.83137255, 0.94901961) ;
#46363 = VERTEX_POINT ( 'NONE', #16934 ) ;
#46364 = DIRECTION ( 'NONE',  ( 0.000000000000000000, -1.000000000000000000, 0.000000000000000000 ) ) ;
#46365 = CARTESIAN_POINT ( 'NONE',  ( -9.590711338355999871, -77.33019948661798537, -0.1262585230650999923 ) ) ;
#46366 = CARTESIAN_POINT ( 'NONE',  ( -1.750000000001000089, -60.05000000958000328, -12.56594317859000043 ) ) ;
#46367 = DIRECTION ( 'NONE',  ( -1.000000000000000000, 0.000000000000000000, 0.000000000000000000 ) ) ;
#46368 = CARTESIAN_POINT ( 'NONE',  ( -3.285477502895000068, -2.838700577026000094, -2.045963233116000257 ) ) ;
#46369 = EDGE_CURVE ( 'NONE', #51037, #56919, #34915, .T. ) ;
#46370 = CARTESIAN_POINT ( 'NONE',  ( 5.569438312554999548, -78.84562780968799700, 10.68535195481999978 ) ) ;
#46371 = CARTESIAN_POINT ( 'NONE',  ( 9.697485508432000856, -79.02821424072898537, 0.9045115177663000106 ) ) ;
#46372 = CARTESIAN_POINT ( 'NONE',  ( -10.83206147397086738, -76.16818589886489121, 4.552669838977208450 ) ) ;
#46373 = CARTESIAN_POINT ( 'NONE',  ( 9.200987374210999548, -79.32181222620799588, 5.875133813785999415 ) ) ;
#46374 = CARTESIAN_POINT ( 'NONE',  ( 1.441729589604688666, -85.80681307385599155, 3.322092378136410229 ) ) ;
#46375 = EDGE_LOOP ( 'NONE', ( #20481, #2754, #4329, #34026 ) ) ;
#46376 = ADVANCED_FACE ( 'NONE', ( #26064 ), #44089, .T. ) ;
#46377 = CARTESIAN_POINT ( 'NONE',  ( -9.662446363795996973, -76.49682594560466953, 7.627099640079997300 ) ) ;
#46378 = LINE ( 'NONE', #23911, #50310 ) ;
#46379 = CARTESIAN_POINT ( 'NONE',  ( 10.47020627418438643, -77.27083333333332860, 2.813789756862283387 ) ) ;
#46380 = AXIS2_PLACEMENT_3D ( 'NONE', #41179, #40890, #40601 ) ;
#46381 = CARTESIAN_POINT ( 'NONE',  ( 2.550499813263000348, -78.63411711912299040, -10.67515654612000020 ) ) ;
#46382 = CARTESIAN_POINT ( 'NONE',  ( -0.1834469635243000107, -79.21327907014000402, -1.236465612773999911 ) ) ;
#46383 = CARTESIAN_POINT ( 'NONE',  ( 7.374560639698954922, -77.72291666666666288, 9.596002108778179718 ) ) ;
#46384 = CARTESIAN_POINT ( 'NONE',  ( 5.784847688057999981, -79.31909213876200226, -7.749218217290000155 ) ) ;
#46385 = CARTESIAN_POINT ( 'NONE',  ( 9.929695104603000644, -17.36901065046999904, -7.973993995755001229 ) ) ;
#46386 = CARTESIAN_POINT ( 'NONE',  ( 12.99510751537000353, -63.10294702886003648, -6.911973076623003642 ) ) ;
#46387 = ORIENTED_EDGE ( 'NONE', *, *, #20043, .T. ) ;
#46388 = AXIS2_PLACEMENT_3D ( 'NONE', #4328, #54522, #36493 ) ;
#46389 = FACE_OUTER_BOUND ( 'NONE', #45680, .T. ) ;
#46390 = CARTESIAN_POINT ( 'NONE',  ( -6.883054871632158900, -79.47416539201856267, 9.627400492276409594 ) ) ;
#46391 = CARTESIAN_POINT ( 'NONE',  ( 3.437187628289000596, -78.54828564506389910, 2.028536598677995073 ) ) ;
#46392 = CARTESIAN_POINT ( 'NONE',  ( -7.842892531714791282, -77.88391165169997521, 9.250934933446409048 ) ) ;
#46394 = CARTESIAN_POINT ( 'NONE',  ( -1.059991318881813527, -81.55564210288132188, 0.6642688495852149266 ) ) ;
#46393 = CARTESIAN_POINT ( 'NONE',  ( -0.5872121148612000630, -82.06976465686300060, 1.181418957762000010 ) ) ;
#46395 = CARTESIAN_POINT ( 'NONE',  ( 4.653180395198093677, -79.00894815872477750, -10.20634710234630660 ) ) ;
#46396 = CARTESIAN_POINT ( 'NONE',  ( -7.726716709342911216, -77.00000000000000000, -5.381598819753512508 ) ) ;
#46397 = CARTESIAN_POINT ( 'NONE',  ( 0.000000000000000000, -15.06282895647999887, 0.000000000000000000 ) ) ;
#46398 = CARTESIAN_POINT ( 'NONE',  ( 0.7471696327285000105, -78.97429688847999785, 1.209193494017000159 ) ) ;
#46399 = CARTESIAN_POINT ( 'NONE',  ( 1.980584515752000119, -18.73514853375999678, 12.76303204602000108 ) ) ;
#46400 = CARTESIAN_POINT ( 'NONE',  ( 8.343860018000999190, -59.94999999967000548, -8.343860018000999190 ) ) ;
#46401 = CARTESIAN_POINT ( 'NONE',  ( 10.42531125068999920, -23.26485145404000221, -7.624341767093000044 ) ) ;
#46402 = ORIENTED_EDGE ( 'NONE', *, *, #10366, .T. ) ;
#46403 = ORIENTED_EDGE ( 'NONE', *, *, #8018, .F. ) ;
#46404 = CARTESIAN_POINT ( 'NONE',  ( -9.273838249849999826, -78.84838998579800773, 3.800455380692000062 ) ) ;
#46405 = STYLED_ITEM ( 'NONE', ( #29953 ), #35529 ) ;
#46406 = CARTESIAN_POINT ( 'NONE',  ( 6.868809838215960362, -78.78024190471647614, -8.269304102357615704 ) ) ;
#46407 = EDGE_LOOP ( 'NONE', ( #9793, #24019, #13251, #24540, #57872, #18969 ) ) ;
#46408 = CARTESIAN_POINT ( 'NONE',  ( 0.000000000000000000, -80.79999999999999716, 0.000000000000000000 ) ) ;
#46409 = CARTESIAN_POINT ( 'NONE',  ( -8.590227911348797818, -79.36453639063311982, 4.069435271439020951 ) ) ;
#46410 = CARTESIAN_POINT ( 'NONE',  ( 9.101516360845000264, -61.68066799025999813, 8.485522730770000521 ) ) ;
#46411 = CARTESIAN_POINT ( 'NONE',  ( 0.5999999999999999778, -23.15000000000000213, 12.00000000000000000 ) ) ;
#46412 = CARTESIAN_POINT ( 'NONE',  ( -11.06091447456626398, -78.01852973287638804, 4.601756440133207171 ) ) ;
#46413 = CARTESIAN_POINT ( 'NONE',  ( -1.639962962630000076, -78.65278220792400532, 11.09633417262999977 ) ) ;
#46414 = ORIENTED_EDGE ( 'NONE', *, *, #34883, .F. ) ;
#46415 = DIRECTION ( 'NONE',  ( 0.000000000000000000, 0.7071067811866525998, -0.7071067811864425456 ) ) ;
#46416 = ORIENTED_EDGE ( 'NONE', *, *, #43234, .T. ) ;
#46417 = CARTESIAN_POINT ( 'NONE',  ( 7.271493354192070768, -77.40312800509396141, 5.718980060901933449 ) ) ;
#46418 = CARTESIAN_POINT ( 'NONE',  ( 7.528714304401000312, -78.17517044313399310, -8.074838600060001426 ) ) ;
#46419 = AXIS2_PLACEMENT_3D ( 'NONE', #30177, #37894, #43492 ) ;
#46420 = CARTESIAN_POINT ( 'NONE',  ( 0.000000000000000000, -2.660000000000000142, 0.000000000000000000 ) ) ;
#46421 = CARTESIAN_POINT ( 'NONE',  ( -1.393431170853000056, -78.94979032468299351, 0.8158852592188999830 ) ) ;
#46422 = CARTESIAN_POINT ( 'NONE',  ( -12.00000000000000178, -77.41041666666669130, -1.570796326794897668 ) ) ;
#46423 = EDGE_CURVE ( 'NONE', #41938, #8229, #54412, .T. ) ;
#46424 = CARTESIAN_POINT ( 'NONE',  ( 6.043427764450807871, -78.56666666666666288, -10.48543666025108756 ) ) ;
#46425 = CARTESIAN_POINT ( 'NONE',  ( 1.328072050606999843, -78.41213347948999512, -0.9406846882429998891 ) ) ;
#46426 = CARTESIAN_POINT ( 'NONE',  ( 4.160588626246000565, -79.48657046129088144, 0.3099153621731999819 ) ) ;
#46427 = CARTESIAN_POINT ( 'NONE',  ( 9.601044633201999190, -79.21897326909299863, 5.244783912358999878 ) ) ;
#46428 = ADVANCED_FACE ( 'NONE', ( #8948 ), #2383, .F. ) ;
#46429 = CARTESIAN_POINT ( 'NONE',  ( 12.70299718804698763, -61.82583482779825346, 0.8845454260210772190 ) ) ;
#46430 = AXIS2_PLACEMENT_3D ( 'NONE', #6241, #14222, #10391 ) ;
#46431 = CARTESIAN_POINT ( 'NONE',  ( 9.500000000000000000, -79.04999999999999716, 0.000000000000000000 ) ) ;
#46432 = CARTESIAN_POINT ( 'NONE',  ( 3.546986249139000069, -82.46507062100899077, -0.05580368944623999988 ) ) ;
#46433 = ORIENTED_EDGE ( 'NONE', *, *, #41654, .F. ) ;
#46434 = CARTESIAN_POINT ( 'NONE',  ( -0.5671522757914000401, -78.75204040462999444, 12.42051695972000047 ) ) ;
#46435 = CARTESIAN_POINT ( 'NONE',  ( 1.623222485893000000, -80.60446191477998923, 0.5147482071316000773 ) ) ;
#46436 = CARTESIAN_POINT ( 'NONE',  ( 4.167258872662748637, -77.94352344884244133, 9.911697996766440255 ) ) ;
#46437 = CARTESIAN_POINT ( 'NONE',  ( 8.272973658470998970, -78.25176643067300120, -8.664523719228998999 ) ) ;
#46438 = CYLINDRICAL_SURFACE ( 'NONE', #10846, 12.00000000000000000 ) ;
#46439 = VECTOR ( 'NONE', #19366, 1000.000000000000227 ) ;
#46440 = CARTESIAN_POINT ( 'NONE',  ( 1.088860609755996744, -77.95691271763917030, -0.6622528567310277392 ) ) ;
#46441 = CARTESIAN_POINT ( 'NONE',  ( -1.630911441802957329, -3.337159252943526777, -3.168633379730300348 ) ) ;
#46442 = CARTESIAN_POINT ( 'NONE',  ( 9.565389234382577044, -80.88786508125609487, 4.905482548979066770 ) ) ;
#46443 = CARTESIAN_POINT ( 'NONE',  ( -0.5382333298950999767, -77.69963385321997862, -9.397951872088000869 ) ) ;
#46444 = LINE ( 'NONE', #13953, #49945 ) ;
#46445 = CARTESIAN_POINT ( 'NONE',  ( 0.1369776181910999924, -77.33287542851299179, 11.03100047655000004 ) ) ;
#46446 = CARTESIAN_POINT ( 'NONE',  ( 1.298131932841000147, -76.51656913009320249, 12.21218573294999921 ) ) ;
#46447 = CARTESIAN_POINT ( 'NONE',  ( 5.335937065057000162, -81.19311224954469708, -9.281131934233000536 ) ) ;
#46448 = EDGE_LOOP ( 'NONE', ( #954, #33734, #39840, #31538 ) ) ;
#46449 = EDGE_CURVE ( 'NONE', #48634, #30476, #21509, .T. ) ;
#46450 = CARTESIAN_POINT ( 'NONE',  ( -1.807051837523000026, -61.10078415209999747, -12.77977401837999949 ) ) ;
#46451 = CARTESIAN_POINT ( 'NONE',  ( 4.139857590833908141, -80.44388087869388926, 9.994141488024814279 ) ) ;
#46452 = CARTESIAN_POINT ( 'NONE',  ( -0.8253947190445000137, -77.38524470668500044, -11.18645762290999990 ) ) ;
#46453 = CARTESIAN_POINT ( 'NONE',  ( 10.97550047727999889, -78.12021830712397730, 0.05101033830554000531 ) ) ;
#46454 = CARTESIAN_POINT ( 'NONE',  ( 7.762981007049000404, -24.16089459216999913, -9.992000916352999695 ) ) ;
#46455 = CARTESIAN_POINT ( 'NONE',  ( 0.5575394168558645003, -85.79166668297689569, 3.974010456388519685 ) ) ;
#46456 = CARTESIAN_POINT ( 'NONE',  ( 3.167321027750415130, -1.872349564160396884, 0.8521775410308326526 ) ) ;
#46457 = CARTESIAN_POINT ( 'NONE',  ( -9.175589924910891426, -53.57304466829480560, -8.792768277102885222 ) ) ;
#46458 = CARTESIAN_POINT ( 'NONE',  ( 4.171886442359999947, -85.43367953870898646, 0.04368964723657999677 ) ) ;
#46459 = CARTESIAN_POINT ( 'NONE',  ( -0.3926218265389255779, -80.39583333333335702, 1.460959015002472494 ) ) ;
#46460 = EDGE_CURVE ( 'NONE', #30580, #36425, #20891, .T. ) ;
#46462 = EDGE_CURVE ( 'NONE', #15626, #43717, #55405, .T. ) ;
#46461 = FACE_OUTER_BOUND ( 'NONE', #44711, .T. ) ;
#46463 = CARTESIAN_POINT ( 'NONE',  ( 10.83766451684999943, -77.50467495194999401, -3.062514061775999608 ) ) ;
#46464 = CARTESIAN_POINT ( 'NONE',  ( -1.542698325316999908, -81.35801279995000357, 0.6290719308543000210 ) ) ;
#46465 = CARTESIAN_POINT ( 'NONE',  ( -0.6174246106352999641, -78.54625317011999641, -1.294938861597000113 ) ) ;
#46466 = CARTESIAN_POINT ( 'NONE',  ( -11.68767212001979594, -77.77916666666665435, 3.140974612311315806 ) ) ;
#46467 = DIRECTION ( 'NONE',  ( 0.000000000000000000, 1.000000000000000000, 0.000000000000000000 ) ) ;
#46468 = AXIS2_PLACEMENT_3D ( 'NONE', #47596, #20130, #38989 ) ;
#46469 = CARTESIAN_POINT ( 'NONE',  ( -12.66313299637999989, -61.97803434819999779, -0.06050769725595999543 ) ) ;
#46470 = ORIENTED_EDGE ( 'NONE', *, *, #11831, .F. ) ;
#46471 = CARTESIAN_POINT ( 'NONE',  ( -1.980464439859999981, -21.75472017459999918, -12.85144117154000121 ) ) ;
#46472 = CARTESIAN_POINT ( 'NONE',  ( 8.768124086712999699, -55.64999999965999677, 7.919595949288999570 ) ) ;
#46473 = B_SPLINE_CURVE_WITH_KNOTS ( 'NONE', 3,
 ( #41605, #615, #31855, #1185, #49896, #41899, #41024, #55478 ),
 .UNSPECIFIED., .F., .F.,
 ( 4, 2, 2, 4 ),
 ( 0.000000000000000000, 0.5000000000000000000, 0.7500000000000000000, 1.000000000000000000 ),
 .UNSPECIFIED. ) ;
#46474 = ORIENTED_EDGE ( 'NONE', *, *, #32990, .F. ) ;
#46475 = CARTESIAN_POINT ( 'NONE',  ( 0.2646997931788037661, -81.74224111115465519, -1.223373072239541726 ) ) ;
#46476 = AXIS2_PLACEMENT_3D ( 'NONE', #1841, #32797, #46725 ) ;
#46477 = SURFACE_STYLE_FILL_AREA ( #28428 ) ;
#46478 = CARTESIAN_POINT ( 'NONE',  ( -10.88242774903000054, -79.47197590580999815, -1.809558141819000099 ) ) ;
#46479 = LINE ( 'NONE', #24313, #32770 ) ;
#46480 = ORIENTED_EDGE ( 'NONE', *, *, #52416, .T. ) ;
#46481 = EDGE_LOOP ( 'NONE', ( #45391, #1665, #47590 ) ) ;
#46482 = CARTESIAN_POINT ( 'NONE',  ( 0.6617453507451001027, -81.76632985222998684, -1.253855045949999969 ) ) ;
#46483 = EDGE_CURVE ( 'NONE', #17174, #34958, #35325, .T. ) ;
#46484 = ORIENTED_EDGE ( 'NONE', *, *, #4722, .F. ) ;
#46485 = VERTEX_POINT ( 'NONE', #17806 ) ;
#46486 = CARTESIAN_POINT ( 'NONE',  ( 1.632307027708999936, -18.33072810443000122, 12.46200249212000166 ) ) ;
#46487 = CONICAL_SURFACE ( 'NONE', #3109, 13.94999999997000018, 0.7853981633972997312 ) ;
#46488 = CARTESIAN_POINT ( 'NONE',  ( 0.000000000000000000, -74.64999999999999147, 0.000000000000000000 ) ) ;
#46489 = DIRECTION ( 'NONE',  ( 0.000000000000000000, 0.000000000000000000, 1.000000000000000000 ) ) ;
#46490 = CARTESIAN_POINT ( 'NONE',  ( -1.031249463432703406, -81.39791665334102788, 3.286199682045575887 ) ) ;
#46491 = CIRCLE ( 'NONE', #55875, 1.250000000000000444 ) ;
#46492 = CARTESIAN_POINT ( 'NONE',  ( -9.193055583834000899, -78.28806001420198868, 3.991918584785999702 ) ) ;
#46493 = CARTESIAN_POINT ( 'NONE',  ( 7.468847837488564068, -78.29994358424977463, -5.456927524485993608 ) ) ;
#46494 = CARTESIAN_POINT ( 'NONE',  ( -8.596418555780431348, -78.05208333333331439, -6.606377239730338857 ) ) ;
#46495 = ORIENTED_EDGE ( 'NONE', *, *, #29887, .F. ) ;
#46496 = EDGE_LOOP ( 'NONE', ( #8990, #49936, #45756, #29490 ) ) ;
#46497 = CARTESIAN_POINT ( 'NONE',  ( -9.207928684727265889, -77.59252129394877784, 0.8882674814189085444 ) ) ;
#46498 = CARTESIAN_POINT ( 'NONE',  ( -12.00000000000000178, -76.90670863885249275, -1.011638905658492460 ) ) ;
#46499 = CARTESIAN_POINT ( 'NONE',  ( -1.460959015002474937, -79.47916666666667140, 0.3926218265389144757 ) ) ;
#46500 = CARTESIAN_POINT ( 'NONE',  ( 8.899186938124000079, -76.04999999999999716, -6.465637775218000094 ) ) ;
#46501 = CARTESIAN_POINT ( 'NONE',  ( 9.690463944985998168, -78.51562024239699156, -0.5153813127049999832 ) ) ;
#46502 = DIRECTION ( 'NONE',  ( 1.205798306211979422E-11, -1.868136817095964273E-07, 0.9999999999999824585 ) ) ;
#46503 = CARTESIAN_POINT ( 'NONE',  ( -3.654181822837000215, -86.09999999943198645, 1.626946589673999854 ) ) ;
#46504 = CARTESIAN_POINT ( 'NONE',  ( -11.36512682855694933, -77.32683455540997386, -3.982123233434258669 ) ) ;
#46505 = CARTESIAN_POINT ( 'NONE',  ( 1.330733645151999989, -79.34391447301999278, 0.2346736355698000043 ) ) ;
#46506 = CARTESIAN_POINT ( 'NONE',  ( -4.370596010382554297, -77.46312193750340214, 8.375126287499346844 ) ) ;
#46507 = CARTESIAN_POINT ( 'NONE',  ( -8.304142175982839547, -76.63735098509414456, 8.312756051645006750 ) ) ;
#46508 = CARTESIAN_POINT ( 'NONE',  ( 2.484104553507999746, -79.21468383341469632, -3.352505685947999581 ) ) ;
#46510 = VECTOR ( 'NONE', #48739, 1000.000000000000114 ) ;
#46509 = CARTESIAN_POINT ( 'NONE',  ( -1.510398065887423646, -79.74790249549140242, 0.03865242478268100107 ) ) ;
#46511 = CARTESIAN_POINT ( 'NONE',  ( -9.610781959738998736, -78.56066001420198575, 1.214124111355000091 ) ) ;
#46512 = CARTESIAN_POINT ( 'NONE',  ( -8.098718803560510437, -76.65741278108174583, -7.103718760442247593 ) ) ;
#46513 = CARTESIAN_POINT ( 'NONE',  ( -7.645398650971000798, -18.78468617155999709, -10.18948982068999953 ) ) ;
#46515 = CARTESIAN_POINT ( 'NONE',  ( -1.182296476285000120, -78.72738264883200543, 0.6170503964917000150 ) ) ;
#46514 = CARTESIAN_POINT ( 'NONE',  ( -1.500000000000000000, -78.89999999999999147, 0.000000000000000000 ) ) ;
#46516 = DIRECTION ( 'NONE',  ( 0.000000000000000000, 1.000000000000000000, 0.000000000000000000 ) ) ;
#46517 = DIRECTION ( 'NONE',  ( -0.07798810297638607281, 0.04890180917552757606, -0.9957542211075506300 ) ) ;
#46518 = DIRECTION ( 'NONE',  ( 1.000000000000000000, 0.000000000000000000, 0.000000000000000000 ) ) ;
#46519 = CARTESIAN_POINT ( 'NONE',  ( 0.9995835529977264988, -79.19791666666664298, -0.7681833999686417114 ) ) ;
#46520 = ORIENTED_EDGE ( 'NONE', *, *, #54755, .T. ) ;
#46521 = CARTESIAN_POINT ( 'NONE',  ( -2.848735472152420733, -3.499999999999999556, -1.711658475673403013 ) ) ;
#46522 = EDGE_CURVE ( 'NONE', #43183, #1186, #50464, .T. ) ;
#46523 = DIRECTION ( 'NONE',  ( -0.7071067811865474617, 0.000000000000000000, -0.7071067811865474617 ) ) ;
#46524 = AXIS2_PLACEMENT_3D ( 'NONE', #33025, #45472, #51071 ) ;
#46525 = FACE_OUTER_BOUND ( 'NONE', #50384, .T. ) ;
#46526 = CARTESIAN_POINT ( 'NONE',  ( 12.77656765298000074, -62.11198129881000085, -0.1555235816857000186 ) ) ;
#46527 = CARTESIAN_POINT ( 'NONE',  ( -1.478176540950000062, -79.50581479701997978, -9.528551035451000573 ) ) ;
#46528 = CARTESIAN_POINT ( 'NONE',  ( 5.512103878356000131, -76.78819232728000088, 11.78783395355999986 ) ) ;
#46529 = CARTESIAN_POINT ( 'NONE',  ( -12.50000000000000000, -15.06282895647999887, 0.000000000000000000 ) ) ;
#46530 = CARTESIAN_POINT ( 'NONE',  ( 3.343750000583999960, -0.9062499994161000716, -3.925818329445000231E-08 ) ) ;
#46531 = B_SPLINE_CURVE_WITH_KNOTS ( 'NONE', 3,
 ( #49248, #39789, #3221, #8499, #48668, #57802, #3498, #40081, #58097, #48105, #21501, #53673, #52802, #13213, #31208, #8798, #57512, #21208 ),
 .UNSPECIFIED., .F., .F.,
 ( 4, 2, 2, 2, 2, 2, 2, 2, 4 ),
 ( 0.000000000000000000, 0.1250000000000000833, 0.2500000000000001665, 0.3750000000000001665, 0.5000000000000002220, 0.6250000000000002220, 0.7500000000000001110, 0.8750000000000001110, 1.000000000000000000 ),
 .UNSPECIFIED. ) ;
#46532 = CIRCLE ( 'NONE', #37987, 12.90000000000000036 ) ;
#46533 = DIRECTION ( 'NONE',  ( 0.000000000000000000, -1.000000000000000000, 0.000000000000000000 ) ) ;
#46534 = CARTESIAN_POINT ( 'NONE',  ( -3.004044512312000315, -77.78272331745698409, -10.86653804020000003 ) ) ;
#46535 = EDGE_CURVE ( 'NONE', #18636, #20606, #52584, .T. ) ;
#46536 = CARTESIAN_POINT ( 'NONE',  ( -1.029597909886999840, -82.28757464707300073, 1.099498802994000046 ) ) ;
#46537 = DIRECTION ( 'NONE',  ( -1.000000000000000000, 0.000000000000000000, 0.000000000000000000 ) ) ;
#46538 = CARTESIAN_POINT ( 'NONE',  ( -1.250000000000000000, -81.09999999999999432, 0.000000000000000000 ) ) ;
#46540 = CARTESIAN_POINT ( 'NONE',  ( -3.431352783032999731, -1.308516015699999979, 2.086989923523999924 ) ) ;
#46539 = CARTESIAN_POINT ( 'NONE',  ( 0.2829448620830999905, -82.50228596008699355, 3.745841164862000028 ) ) ;
#46541 = CARTESIAN_POINT ( 'NONE',  ( 5.684029094576000141, -79.74564805011499402, -7.680196531179999120 ) ) ;
#46542 = FACE_OUTER_BOUND ( 'NONE', #9053, .T. ) ;
#46543 = FACE_BOUND ( 'NONE', #15062, .T. ) ;
#46544 = CARTESIAN_POINT ( 'NONE',  ( -6.307673058192007964, -77.17525117048977279, -8.704862286692511830 ) ) ;
#46545 = DIRECTION ( 'NONE',  ( -0.7071067811865475727, 0.000000000000000000, -0.7071067811865475727 ) ) ;
#46546 = VERTEX_POINT ( 'NONE', #32462 ) ;
#46547 = ORIENTED_EDGE ( 'NONE', *, *, #1400, .F. ) ;
#46548 = CARTESIAN_POINT ( 'NONE',  ( 8.348735229153000148, -79.01379656946899388, 8.268078378528999295 ) ) ;
#46549 = CARTESIAN_POINT ( 'NONE',  ( 1.250000000000000000, -78.35000000000000853, 0.000000000000000000 ) ) ;
#46550 = CYLINDRICAL_SURFACE ( 'NONE', #216, 14.00000000000000000 ) ;
#46551 = VERTEX_POINT ( 'NONE', #13595 ) ;
#46552 = CARTESIAN_POINT ( 'NONE',  ( 9.414842545117998895, -77.82074243306399808, -7.334592169791999794 ) ) ;
#46553 = EDGE_CURVE ( 'NONE', #41078, #8467, #15249, .T. ) ;
#46554 = ORIENTED_EDGE ( 'NONE', *, *, #26526, .F. ) ;
#46555 = ORIENTED_EDGE ( 'NONE', *, *, #14177, .T. ) ;
#46556 = CARTESIAN_POINT ( 'NONE',  ( 8.596418555780418913, -78.80208333333332860, 6.606377239730356621 ) ) ;
#46557 = ORIENTED_EDGE ( 'NONE', *, *, #53293, .T. ) ;
#46558 = VECTOR ( 'NONE', #21555, 1000.000000000000000 ) ;
#46559 = CARTESIAN_POINT ( 'NONE',  ( 3.344859295621999795, -81.01844020063299467, 1.180460146152999990 ) ) ;
#46560 = CARTESIAN_POINT ( 'NONE',  ( 10.48771805367000098, -57.04439828530000511, 7.686918321054999836 ) ) ;
#46561 = ORIENTED_EDGE ( 'NONE', *, *, #48378, .T. ) ;
#46562 = CARTESIAN_POINT ( 'NONE',  ( 1.170361114333020813, -82.82144115138102336, -0.4391466590958141292 ) ) ;
#46563 = CARTESIAN_POINT ( 'NONE',  ( -7.718368845781999887, -58.54800977479000323, 10.07722254367000048 ) ) ;
#46564 = EDGE_LOOP ( 'NONE', ( #31334, #4641, #28290, #58349 ) ) ;
#46565 = CARTESIAN_POINT ( 'NONE',  ( 1.668607604570606640, -18.20618368758884387, 12.52787843850908445 ) ) ;
#46566 = CARTESIAN_POINT ( 'NONE',  ( -0.6802376739418862783, -78.33817466101120885, -1.374165118460863866 ) ) ;
#46567 = FACE_OUTER_BOUND ( 'NONE', #10627, .T. ) ;
#46568 = CIRCLE ( 'NONE', #48440, 2.500000000000000000 ) ;
#46569 = CARTESIAN_POINT ( 'NONE',  ( 11.09903705321281464, -79.23326252747547471, 4.904546639011450715 ) ) ;
#46570 = CARTESIAN_POINT ( 'NONE',  ( -4.475245744599999576, -78.83685813009675769, -8.610626265545000990 ) ) ;
#46571 = CARTESIAN_POINT ( 'NONE',  ( 4.903943924252999409, -76.35943902665499650, -10.05113017056000047 ) ) ;
#46572 = CARTESIAN_POINT ( 'NONE',  ( 0.000000000000000000, 4.040000000000000036, 0.000000000000000000 ) ) ;
#46573 = CIRCLE ( 'NONE', #48407, 9.250000000000000000 ) ;
#46574 = CARTESIAN_POINT ( 'NONE',  ( -7.626500902197000720, -55.48415522678000400, -10.35747158360999975 ) ) ;
#46575 = CARTESIAN_POINT ( 'NONE',  ( -4.551864695536657734, -78.68412335589445661, -8.054303700184762604 ) ) ;
#46576 = CARTESIAN_POINT ( 'NONE',  ( 4.524948720244553968, -76.54318040950390412, 10.84353445346675748 ) ) ;
#46577 = CARTESIAN_POINT ( 'NONE',  ( -2.654111470047999966, -77.17291001420200303, -9.029532749234000732 ) ) ;
#46578 = CARTESIAN_POINT ( 'NONE',  ( 0.9788970803261000109, -79.82492711368898597, -0.9057243817226000582 ) ) ;
#46579 = CARTESIAN_POINT ( 'NONE',  ( -6.819272535855454009, -80.17227384770239951, -8.636012267496480987 ) ) ;
#46580 = CARTESIAN_POINT ( 'NONE',  ( -3.250000000000000000, -3.100000000000000089, 0.000000000000000000 ) ) ;
#46581 = CARTESIAN_POINT ( 'NONE',  ( 1.861773376307000127, -79.40353455456848053, 3.498539798548999880 ) ) ;
#46582 = CARTESIAN_POINT ( 'NONE',  ( 0.000000000000000000, -76.75499999999999545, 0.000000000000000000 ) ) ;
#46583 = CARTESIAN_POINT ( 'NONE',  ( 7.783076670315924872, -76.24921875000657678, 9.115310453498814525 ) ) ;
#46584 = CARTESIAN_POINT ( 'NONE',  ( 0.4742823758087600372, -82.94408184949666918, 1.156490669114161207 ) ) ;
#46585 = SURFACE_STYLE_USAGE ( .BOTH. , #28537 ) ;
#46586 = CARTESIAN_POINT ( 'NONE',  ( -3.485499217011999828, -78.91452042059380290, -1.462502484024984119E-14 ) ) ;
#46587 = CARTESIAN_POINT ( 'NONE',  ( 6.043427764450763462, -79.23333333333330586, 10.48543666025111065 ) ) ;
#46588 = CARTESIAN_POINT ( 'NONE',  ( -10.01749676171999859, -59.99181054660999735, -7.660430254678000317 ) ) ;
#46589 = EDGE_CURVE ( 'NONE', #25178, #40639, #44737, .T. ) ;
#46590 = CARTESIAN_POINT ( 'NONE',  ( -2.421146232948727217, -79.70460708974083275, -9.008471024255291226 ) ) ;
#46591 = DIRECTION ( 'NONE',  ( 0.000000000000000000, 1.000000000000000000, 0.000000000000000000 ) ) ;
#46593 = EDGE_CURVE ( 'NONE', #28511, #13326, #57984, .T. ) ;
#46592 = CARTESIAN_POINT ( 'NONE',  ( -1.929975092517999924, -23.20107256264000029, -12.72537404210999945 ) ) ;
#46594 = CARTESIAN_POINT ( 'NONE',  ( 13.13047446164998711, -19.21421830981000767, 0.8260994316375004365 ) ) ;
#46595 = CARTESIAN_POINT ( 'NONE',  ( -8.918806285220000518, -78.03734805011499986, 3.872830773119999570 ) ) ;
#46596 = CARTESIAN_POINT ( 'NONE',  ( -7.921335223404320836, -24.55094696616630401, -10.04563431748756130 ) ) ;
#46597 = CARTESIAN_POINT ( 'NONE',  ( -10.64366519981685322, -77.46551422760700234, -2.049234529886447831 ) ) ;
#46598 = CARTESIAN_POINT ( 'NONE',  ( 7.788493169598003085, -78.66221640831159334, 7.733265204867000087 ) ) ;
#46599 = CARTESIAN_POINT ( 'NONE',  ( 11.51413715134999904, -76.48154810978000739, -3.593459816516999972 ) ) ;
#46600 = ORIENTED_EDGE ( 'NONE', *, *, #39847, .T. ) ;
#46601 = CARTESIAN_POINT ( 'NONE',  ( -1.649098995971000070, -86.23821544543099549, 3.375205270238999411 ) ) ;
#46602 = CARTESIAN_POINT ( 'NONE',  ( -10.10188948264000075, -80.74568563909183183, -5.039239965656999942 ) ) ;
#46603 = ADVANCED_FACE ( 'NONE', ( #38362 ), #6785, .T. ) ;
#46604 = CARTESIAN_POINT ( 'NONE',  ( 7.703316849872579475, -78.30345904569475124, -5.123123729073115307 ) ) ;
#46605 = CARTESIAN_POINT ( 'NONE',  ( -1.460959015002473382, -81.52083333333332860, -0.3926218265389205819 ) ) ;
#46606 = CARTESIAN_POINT ( 'NONE',  ( -7.849238557987999521, -76.83991323819199692, 7.706455349885999340 ) ) ;
#46607 = CARTESIAN_POINT ( 'NONE',  ( 9.415855586929327004, -78.95131608867242790, 0.09954321913080461937 ) ) ;
#46608 = CARTESIAN_POINT ( 'NONE',  ( -2.552693750765000047, -78.49671468919598283, -9.286385980553001573 ) ) ;
#46609 = CARTESIAN_POINT ( 'NONE',  ( -4.134112256334000257, -83.18657311260999165, 0.5618462995190999232 ) ) ;
#46610 = CARTESIAN_POINT ( 'NONE',  ( 3.621447497675000182, -78.99318692614357929, 0.000000000000000000 ) ) ;
#46611 = CARTESIAN_POINT ( 'NONE',  ( 1.750000000001000089, -23.25000000990999993, 12.56594317857000043 ) ) ;
#46612 = ORIENTED_EDGE ( 'NONE', *, *, #3384, .T. ) ;
#46613 = FACE_OUTER_BOUND ( 'NONE', #2029, .T. ) ;
#46614 = LINE ( 'NONE', #1445, #46762 ) ;
#46615 = CARTESIAN_POINT ( 'NONE',  ( 2.732978708635966925, -78.98334398719974558, -2.638764568140384181 ) ) ;
#46616 = VERTEX_POINT ( 'NONE', #11517 ) ;
#46617 = CARTESIAN_POINT ( 'NONE',  ( -0.5996107393304999089, -78.59022199029399758, 1.191235959310000148 ) ) ;
#46618 = CARTESIAN_POINT ( 'NONE',  ( -11.38514561087999866, -79.66561849808098827, 1.960531219681000081 ) ) ;
#46619 = EDGE_LOOP ( 'NONE', ( #9819, #26321 ) ) ;
#46620 = CARTESIAN_POINT ( 'NONE',  ( -10.21414511300999983, -77.77975978748899877, 6.816672119949999775 ) ) ;
#46621 = CARTESIAN_POINT ( 'NONE',  ( 5.377062312294000002, -77.72131800370499377, -9.963906840203000215 ) ) ;
#46622 = CARTESIAN_POINT ( 'NONE',  ( 9.175573575496967393, -62.02695822328877995, -8.792784719842536845 ) ) ;
#46623 = VERTEX_POINT ( 'NONE', #5613 ) ;
#46624 = EDGE_LOOP ( 'NONE', ( #3566, #50531, #19422, #17320, #28976, #11820 ) ) ;
#46625 = CARTESIAN_POINT ( 'NONE',  ( -1.102620915002880730, -80.56095890462103171, 0.5891712059213058961 ) ) ;
#46626 = CARTESIAN_POINT ( 'NONE',  ( -10.47049301042761016, -77.62083827941357583, -2.813954463924708271 ) ) ;
#46627 = CARTESIAN_POINT ( 'NONE',  ( 3.366547962069000199, -79.54345705591799742, -9.168809063548000182 ) ) ;
#46628 = AXIS2_PLACEMENT_3D ( 'NONE', #5657, #24257, #28966 ) ;
#46629 = VERTEX_POINT ( 'NONE', #10648 ) ;
#46630 = CARTESIAN_POINT ( 'NONE',  ( 12.77306291382000047, -53.74129324268999852, 1.041150512314999999 ) ) ;
#46631 = CARTESIAN_POINT ( 'NONE',  ( 10.42531125068999920, -23.26485145404000221, -7.624341767093000044 ) ) ;
#46632 = ORIENTED_EDGE ( 'NONE', *, *, #24009, .T. ) ;
#46633 = CARTESIAN_POINT ( 'NONE',  ( -12.68703394091000014, -23.75066116476999767, -1.889962945499999991 ) ) ;
#46634 = CARTESIAN_POINT ( 'NONE',  ( -4.802567994450000377, -77.09264415034600404, -8.191018798270000900 ) ) ;
#46635 = ADVANCED_FACE ( 'NONE', ( #42807 ), #41931, .T. ) ;
#46636 = DIRECTION ( 'NONE',  ( 0.000000000000000000, 0.000000000000000000, 1.000000000000000000 ) ) ;
#46637 = CARTESIAN_POINT ( 'NONE',  ( -0.7681743634654464303, -80.17267673354702140, -0.9864499039395765445 ) ) ;
#46638 = CARTESIAN_POINT ( 'NONE',  ( -1.501534314733827147, -17.44847048338573359, -12.70455943739971794 ) ) ;
#46639 = CARTESIAN_POINT ( 'NONE',  ( 3.441702665804598382, -77.89481086934992504, 8.844266313550066982 ) ) ;
#46640 = AXIS2_PLACEMENT_3D ( 'NONE', #23003, #41014, #606 ) ;
#46641 = CARTESIAN_POINT ( 'NONE',  ( -9.467663399184001349, -77.16228479622688496, 0.6244416360999999194 ) ) ;
#46642 = CARTESIAN_POINT ( 'NONE',  ( 1.252773319961611787, -79.05243164265034750, -0.8433518312087610047 ) ) ;
#46643 = CARTESIAN_POINT ( 'NONE',  ( 0.000000000000000000, -75.15999999999999659, 0.000000000000000000 ) ) ;
#46644 = CARTESIAN_POINT ( 'NONE',  ( -7.685416442687999172, -76.58867693717000691, -9.616126112745998711 ) ) ;
#46645 = CARTESIAN_POINT ( 'NONE',  ( 10.75000000000000000, -77.75000000000000000, 0.000000000000000000 ) ) ;
#46646 = AXIS2_PLACEMENT_3D ( 'NONE', #55810, #24216, #51389 ) ;
#46647 = CARTESIAN_POINT ( 'NONE',  ( -3.392118867033536489, -1.870808869262021501, -0.9407460553073063725 ) ) ;
#46648 = CARTESIAN_POINT ( 'NONE',  ( 10.01676948373999920, -60.00938276551000428, -7.658894993385999328 ) ) ;
#46649 = CARTESIAN_POINT ( 'NONE',  ( 12.16303714866999997, -79.31220515959000750, 1.568404430622000190 ) ) ;
#46650 = CARTESIAN_POINT ( 'NONE',  ( -9.801255020792000394, -76.51464391298200951, 7.399866681860999940 ) ) ;
#46651 = CARTESIAN_POINT ( 'NONE',  ( 12.72966282071409161, -18.23110224985535055, -1.931329623869578072 ) ) ;
#46652 = CARTESIAN_POINT ( 'NONE',  ( 9.850507816072846978, -61.10508874482292185, -7.836744050180014298 ) ) ;
#46653 = CARTESIAN_POINT ( 'NONE',  ( 12.18176164782117965, -78.30556067180121715, 0.8546284421110175167 ) ) ;
#46654 = CARTESIAN_POINT ( 'NONE',  ( 10.05828973332000054, -78.96351298475168790, -4.964767691657000270 ) ) ;
#46655 = ORIENTED_EDGE ( 'NONE', *, *, #39304, .T. ) ;
#46657 = EDGE_CURVE ( 'NONE', #11745, #15123, #16526, .T. ) ;
#46656 = CARTESIAN_POINT ( 'NONE',  ( -0.7107282322889000303, -81.60090657403999614, -1.148979047684000054 ) ) ;
#46658 = CARTESIAN_POINT ( 'NONE',  ( 0.000000000000000000, -18.75000000000000000, -12.50000000000000000 ) ) ;
#46659 = CARTESIAN_POINT ( 'NONE',  ( -1.217465845835396188, -79.47916666666668561, 0.3271848554490955907 ) ) ;
#46660 = CARTESIAN_POINT ( 'NONE',  ( -12.50000000000000000, -55.54999999966999980, 0.000000000000000000 ) ) ;
#46661 = CARTESIAN_POINT ( 'NONE',  ( 0.2119930951406999997, -3.510997475527999789, -3.707774086492000354 ) ) ;
#46662 = CARTESIAN_POINT ( 'NONE',  ( 8.821626479137000487, -78.81849849426399146, 8.208219718620000549 ) ) ;
#46663 = CARTESIAN_POINT ( 'NONE',  ( 8.584722543520001636, -79.05663806985799624, 4.148835967969999317 ) ) ;
#46665 = CARTESIAN_POINT ( 'NONE',  ( -8.160216723678894724, -77.11145833334454380, 4.702279489708627302 ) ) ;
#46664 = CARTESIAN_POINT ( 'NONE',  ( -1.728878934773139475, -76.08638080640866974, 11.64666186654994284 ) ) ;
#46666 = CARTESIAN_POINT ( 'NONE',  ( -1.259088972310000054, -82.55045924015399805, 0.4905773767712000577 ) ) ;
#46667 = CARTESIAN_POINT ( 'NONE',  ( 3.184161977317979897, -85.88547957940599531, -1.417680250971043998 ) ) ;
#46668 = ORIENTED_EDGE ( 'NONE', *, *, #1582, .T. ) ;
#46669 = CARTESIAN_POINT ( 'NONE',  ( 12.71536556657276584, -24.12544729045777459, 1.781281568995779940 ) ) ;
#46670 = CARTESIAN_POINT ( 'NONE',  ( -10.12416963781999968, -79.71218441210199046, 6.728766219208999644 ) ) ;
#46671 = VECTOR ( 'NONE', #26560, 1000.000000000000000 ) ;
#46672 = CARTESIAN_POINT ( 'NONE',  ( -9.008856688516557298, -78.07931792999902143, 2.421010749684254115 ) ) ;
#46673 = EDGE_CURVE ( 'NONE', #47780, #21405, #57064, .T. ) ;
#46674 = B_SPLINE_CURVE_WITH_KNOTS ( 'NONE', 3,
 ( #50916, #19323, #10465, #9883, #33167, #51211, #54468, #45909, #5443, #50044, #10764, #37024, #46793, #23449, #9591, #6317, #20690, #24333 ),
 .UNSPECIFIED., .F., .F.,
 ( 4, 2, 2, 2, 2, 2, 2, 2, 4 ),
 ( 0.000000000000000000, 0.1249999999999999722, 0.2500000000000000000, 0.3750000000000000000, 0.5000000000000001110, 0.6250000000000001110, 0.7500000000000000000, 0.8750000000000000000, 1.000000000000000000 ),
 .UNSPECIFIED. ) ;
#46675 = CARTESIAN_POINT ( 'NONE',  ( 3.165411199172024848, -2.270833333333332593, 0.8506806241676669877 ) ) ;
#46676 = CARTESIAN_POINT ( 'NONE',  ( -4.985523414424999800, -78.57793241045699517, -9.777963635945001286 ) ) ;
#46677 = AXIS2_PLACEMENT_3D ( 'NONE', #51853, #11408, #11124 ) ;
#46678 = EDGE_CURVE ( 'NONE', #23001, #20606, #8009, .T. ) ;
#46679 = CARTESIAN_POINT ( 'NONE',  ( -0.5979264001123455463, -79.18538552819090626, -1.097664844063911183 ) ) ;
#46680 = DIRECTION ( 'NONE',  ( -0.7071067811865475727, 0.000000000000000000, 0.7071067811865475727 ) ) ;
#46681 = CARTESIAN_POINT ( 'NONE',  ( -4.460001432529999477, -79.72991637959898981, -8.580398187795999831 ) ) ;
#46682 = CARTESIAN_POINT ( 'NONE',  ( 7.956418361382000981, -17.47110680143000039, -9.787952249849000808 ) ) ;
#46683 = CARTESIAN_POINT ( 'NONE',  ( 0.000000000000000000, -56.01421830981000483, -13.15643568216998638 ) ) ;
#46684 = ORIENTED_EDGE ( 'NONE', *, *, #25590, .F. ) ;
#46685 = CARTESIAN_POINT ( 'NONE',  ( 10.58513040395000004, -78.55432170917399048, 3.845644306921999878 ) ) ;
#46686 = CARTESIAN_POINT ( 'NONE',  ( -5.007265642980745390, -76.76182877174545638, 10.00026998867437911 ) ) ;
#46687 = CARTESIAN_POINT ( 'NONE',  ( -8.596418555780466875, -79.94791666666667140, 6.606377239730298001 ) ) ;
#46688 = DIRECTION ( 'NONE',  ( 0.7071067811864976127, 0.7071067811865975328, -1.603641050304993672E-09 ) ) ;
#46689 = CARTESIAN_POINT ( 'NONE',  ( 5.205657071218882770, -77.29238751238693794, 10.83901206616341106 ) ) ;
#46691 = CARTESIAN_POINT ( 'NONE',  ( 0.3573905483915326697, -81.45234743160045809, 1.197690458606871733 ) ) ;
#46690 = AXIS2_PLACEMENT_3D ( 'NONE', #7814, #24951, #39398 ) ;
#46692 = CARTESIAN_POINT ( 'NONE',  ( -6.324603895332759684, -78.92723912971976574, -9.263962139975491894 ) ) ;
#46693 = DIRECTION ( 'NONE',  ( 0.000000000000000000, -1.433670265775999799E-08, -0.9999999999999998890 ) ) ;
#46694 = CARTESIAN_POINT ( 'NONE',  ( -9.546815224142999767, -17.31472046677999899, -8.130854305520999858 ) ) ;
#46695 = EDGE_CURVE ( 'NONE', #26753, #12183, #40058, .T. ) ;
#46696 = CARTESIAN_POINT ( 'NONE',  ( 0.3939293589371000159, -78.22936979258000179, -1.247237820087999882 ) ) ;
#46697 = DIRECTION ( 'NONE',  ( -1.000000000000000000, 0.000000000000000000, 0.000000000000000000 ) ) ;
#46698 = CARTESIAN_POINT ( 'NONE',  ( 10.94426510211266645, -78.70613393985135531, 0.8311920584813466961 ) ) ;
#46699 = CARTESIAN_POINT ( 'NONE',  ( 0.000000000000000000, -76.15000000005198899, 0.000000000000000000 ) ) ;
#46700 = ORIENTED_EDGE ( 'NONE', *, *, #3177, .T. ) ;
#46701 = EDGE_LOOP ( 'NONE', ( #32276, #24904, #54003, #3046 ) ) ;
#46702 = CARTESIAN_POINT ( 'NONE',  ( 8.379346636603999698, -77.51281807572799210, -8.651713001682999504 ) ) ;
#46703 = CARTESIAN_POINT ( 'NONE',  ( 9.936221582198456304, -78.81890434637429621, -4.102805168011096626 ) ) ;
#46704 = ORIENTED_EDGE ( 'NONE', *, *, #26215, .T. ) ;
#46705 = CARTESIAN_POINT ( 'NONE',  ( 7.605690612615000568, -18.57434870741999688, 10.52682230157000021 ) ) ;
#46706 = EDGE_CURVE ( 'NONE', #27787, #42393, #3834, .T. ) ;
#46707 = DIRECTION ( 'NONE',  ( -0.9999548435846228323, 0.000000000000000000, -0.009503199022040218977 ) ) ;
#46708 = CARTESIAN_POINT ( 'NONE',  ( 6.964475361433999367, -79.00544258048999779, -9.848025321434999313 ) ) ;
#46709 = EDGE_CURVE ( 'NONE', #39177, #21876, #4588, .T. ) ;
#46710 = CARTESIAN_POINT ( 'NONE',  ( 10.36221643470000053, -60.02123873632999818, 7.631895748967999715 ) ) ;
#46711 = DIRECTION ( 'NONE',  ( -1.000000000000000000, 0.000000000000000000, 0.000000000000000000 ) ) ;
#46712 = CARTESIAN_POINT ( 'NONE',  ( -5.687784790578547245, -77.96427110202938593, 10.54367561735933734 ) ) ;
#46713 = CARTESIAN_POINT ( 'NONE',  ( 7.808618912244999599, -79.02017053422000004, -8.052551227705000869 ) ) ;
#46714 = AXIS2_PLACEMENT_3D ( 'NONE', #51245, #51536, #6350 ) ;
#46715 = VERTEX_POINT ( 'NONE', #47550 ) ;
#46716 = CARTESIAN_POINT ( 'NONE',  ( 1.250000000000000000, -77.10000000000000853, 0.000000000000000000 ) ) ;
#46717 = VERTEX_POINT ( 'NONE', #48679 ) ;
#46718 = CARTESIAN_POINT ( 'NONE',  ( 9.209373452604401322, -77.35755538323695646, 0.8669182893996996153 ) ) ;
#46719 = CARTESIAN_POINT ( 'NONE',  ( 2.604371601988999974, -77.63440539582299493, -10.72853197743999942 ) ) ;
#46720 = AXIS2_PLACEMENT_3D ( 'NONE', #33084, #5362, #46711 ) ;
#46721 = CARTESIAN_POINT ( 'NONE',  ( -11.12512020565017323, -77.36010185546032858, -1.432937323680165909 ) ) ;
#46722 = UNCERTAINTY_MEASURE_WITH_UNIT (LENGTH_MEASURE( 1.000000000000000082E-05 ), #31315, 'distance_accuracy_value', 'NONE');
#46723 = CARTESIAN_POINT ( 'NONE',  ( -9.685922776715001348, -77.38557761206399732, 0.5943755449006998814 ) ) ;
#46724 = AXIS2_PLACEMENT_3D ( 'NONE', #18544, #1135, #32098 ) ;
#46725 = DIRECTION ( 'NONE',  ( -0.7071067811865474617, 0.000000000000000000, -0.7071067811865474617 ) ) ;
#46726 = DIRECTION ( 'NONE',  ( 0.000000000000000000, -1.000000000000000000, 0.000000000000000000 ) ) ;
#46727 = CARTESIAN_POINT ( 'NONE',  ( 1.314530797355000225, -78.08864832307999393, -0.9595159925157999981 ) ) ;
#46728 = CARTESIAN_POINT ( 'NONE',  ( -10.98042387750000159, -79.00192546654999148, -1.228081885531999928 ) ) ;
#46729 = CARTESIAN_POINT ( 'NONE',  ( -7.647093862755999893, -23.36895637638999901, -10.00844027276999881 ) ) ;
#46730 = CARTESIAN_POINT ( 'NONE',  ( 12.58338334669999981, -58.54800977479000323, -1.667961445601999992 ) ) ;
#46731 = CARTESIAN_POINT ( 'NONE',  ( -1.489945701322999971, -84.98406384713199202, -3.218948819672999839 ) ) ;
#46732 = ORIENTED_EDGE ( 'NONE', *, *, #22033, .F. ) ;
#46733 = CARTESIAN_POINT ( 'NONE',  ( 0.000000000000000000, -49.87071424677999687, 0.000000000000000000 ) ) ;
#46734 = CARTESIAN_POINT ( 'NONE',  ( 9.898793482178998460, -76.06315555539499940, 4.898044527662000824 ) ) ;
#46735 = CARTESIAN_POINT ( 'NONE',  ( 10.50208737532821246, -77.86721208996137022, 2.298434098163355088 ) ) ;
#46736 = CARTESIAN_POINT ( 'NONE',  ( -11.74098051674999965, -78.55018890033399259, 2.380218674853999961 ) ) ;
#46737 = CARTESIAN_POINT ( 'NONE',  ( -9.389188763474001220, -17.28956227326999695, 8.194870530173000489 ) ) ;
#46738 = CARTESIAN_POINT ( 'NONE',  ( -8.596128373981846593, -79.04808367254781842, 6.606141465317036499 ) ) ;
#46739 = CARTESIAN_POINT ( 'NONE',  ( -3.362520228900586439, -3.273832295754924182, -1.040226447706077639 ) ) ;
#46740 = CARTESIAN_POINT ( 'NONE',  ( 8.619088907633837948, -80.90150449142340960, 6.437677892227573473 ) ) ;
#46741 = CARTESIAN_POINT ( 'NONE',  ( 1.825776387079000029, -78.43865341057399121, 9.234594473601999809 ) ) ;
#46742 = CARTESIAN_POINT ( 'NONE',  ( -3.576074390005993475, -85.88547955769999476, 1.592170899228015024 ) ) ;
#46743 = CARTESIAN_POINT ( 'NONE',  ( -10.77981876821000107, -77.44182080052098627, 2.344619735928000104 ) ) ;
#46744 = CARTESIAN_POINT ( 'NONE',  ( 4.438566736185393324, -77.30575194093574964, -10.90548974299855622 ) ) ;
#46745 = CARTESIAN_POINT ( 'NONE',  ( -1.766199577971000023, -80.41452935543939873, 10.76680414263000074 ) ) ;
#46746 = ORIENTED_EDGE ( 'NONE', *, *, #19243, .F. ) ;
#46747 = CARTESIAN_POINT ( 'NONE',  ( 0.9432352957733999288, -82.07814290487699793, 0.9428059748164999698 ) ) ;
#46748 = CARTESIAN_POINT ( 'NONE',  ( -1.669849926066999890, -60.17228600383999293, -12.48404299555999941 ) ) ;
#46749 = CARTESIAN_POINT ( 'NONE',  ( -7.553727747516310487, -55.11418618784217927, 7.997114030217357339 ) ) ;
#46750 = EDGE_CURVE ( 'NONE', #51790, #47018, #29699, .T. ) ;
#46751 = CARTESIAN_POINT ( 'NONE',  ( 4.013660496580000903, -78.48801429402999474, -10.47417304634999979 ) ) ;
#46752 = CARTESIAN_POINT ( 'NONE',  ( -4.985523414424999800, -78.39702363344498792, -9.777963635945001286 ) ) ;
#46753 = CARTESIAN_POINT ( 'NONE',  ( 7.624757096123999212, -23.80351363819999833, -10.47516529248999895 ) ) ;
#46754 = ADVANCED_FACE ( 'NONE', ( #43101 ), #54917, .F. ) ;
#46755 = CARTESIAN_POINT ( 'NONE',  ( 2.217082214997963874, -85.21354167675372082, -3.391499533005605915 ) ) ;
#46756 = DIRECTION ( 'NONE',  ( 0.000000000000000000, -1.000000000000000000, 0.000000000000000000 ) ) ;
#46757 = CARTESIAN_POINT ( 'NONE',  ( 9.199999999968001774, -80.60000000003199716, -3.388768808660000233E-10 ) ) ;
#46758 = ORIENTED_EDGE ( 'NONE', *, *, #33418, .T. ) ;
#46759 = DIRECTION ( 'NONE',  ( -3.675129381003999189E-09, -0.9999999999999997780, 2.168720766502999921E-08 ) ) ;
#46760 = FACE_OUTER_BOUND ( 'NONE', #1499, .T. ) ;
#46761 = CARTESIAN_POINT ( 'NONE',  ( 8.188285776285999518, -54.09506253957000155, -9.395726099541001020 ) ) ;
#46762 = VECTOR ( 'NONE', #6141, 999.9999999999998863 ) ;
#46763 = CARTESIAN_POINT ( 'NONE',  ( 9.909229536192000865, -76.98718443491598862, -5.351741263869000065 ) ) ;
#46764 = CARTESIAN_POINT ( 'NONE',  ( 0.7545134501129999727, -80.66720432497999127, 1.485250302772000097 ) ) ;
#46765 = CARTESIAN_POINT ( 'NONE',  ( -1.306286088552999880, -78.49057160033999025, -0.5930400157040000009 ) ) ;
#46766 = CARTESIAN_POINT ( 'NONE',  ( -7.764010764696696931, -24.12280919933758128, 9.931043767187555105 ) ) ;
#46767 = CARTESIAN_POINT ( 'NONE',  ( -1.416309796911555674, -81.72162796768579085, 0.5272991973399487886 ) ) ;
#46768 = CARTESIAN_POINT ( 'NONE',  ( -9.469606800734000629, -80.05752053325198858, 5.597012331546999953 ) ) ;
#46769 = ORIENTED_EDGE ( 'NONE', *, *, #45287, .F. ) ;
#46770 = FACE_OUTER_BOUND ( 'NONE', #53788, .T. ) ;
#46771 = EDGE_CURVE ( 'NONE', #16168, #56208, #45496, .T. ) ;
#46772 = CARTESIAN_POINT ( 'NONE',  ( 0.7554284705563509839, -78.06666666666669130, -1.310679582531386167 ) ) ;
#46773 = ORIENTED_EDGE ( 'NONE', *, *, #19222, .T. ) ;
#46774 = CARTESIAN_POINT ( 'NONE',  ( -1.125627005581746554, -81.63605386171199996, -0.5432748768604414025 ) ) ;
#46775 = CARTESIAN_POINT ( 'NONE',  ( 5.530078818784999406, -80.12564813785350282, -9.545677681241999224 ) ) ;
#46776 = PLANE ( 'NONE',  #55380 ) ;
#46777 = ORIENTED_EDGE ( 'NONE', *, *, #32881, .F. ) ;
#46778 = ORIENTED_EDGE ( 'NONE', *, *, #41341, .T. ) ;
#46779 = CARTESIAN_POINT ( 'NONE',  ( -1.474644042471999983, -81.06599406054799317, -0.3526571989726999812 ) ) ;
#46780 = EDGE_LOOP ( 'NONE', ( #50031, #45356, #6082, #9588 ) ) ;
#46781 = ORIENTED_EDGE ( 'NONE', *, *, #50020, .T. ) ;
#46782 = CARTESIAN_POINT ( 'NONE',  ( 1.582498447119000229, -17.84913877521999837, 12.55493832972999968 ) ) ;
#46783 = DIRECTION ( 'NONE',  ( 0.000000000000000000, -1.000000000000000000, 0.000000000000000000 ) ) ;
#46784 = SHAPE_DEFINITION_REPRESENTATION ( #47926, #1422 ) ;
#46785 = CARTESIAN_POINT ( 'NONE',  ( 1.199500263597271799, -78.19791666666667140, -0.9218200799623701425 ) ) ;
#46786 = ADVANCED_FACE ( 'NONE', ( #56954 ), #30354, .T. ) ;
#46787 = CARTESIAN_POINT ( 'NONE',  ( 5.874230328676101287, -78.27988767441337359, -7.145232025174067303 ) ) ;
#46788 = CARTESIAN_POINT ( 'NONE',  ( 9.393203674808285442, -78.20833333333334281, -5.413904038987152667 ) ) ;
#46789 = ORIENTED_EDGE ( 'NONE', *, *, #25850, .F. ) ;
#46790 = ORIENTED_EDGE ( 'NONE', *, *, #56491, .F. ) ;
#46791 = CARTESIAN_POINT ( 'NONE',  ( -3.000000000000000000, -80.79999999999999716, 0.000000000000000000 ) ) ;
#46792 = CARTESIAN_POINT ( 'NONE',  ( 0.000000000000000000, -39.49523982883999906, 0.000000000000000000 ) ) ;
#46793 = CARTESIAN_POINT ( 'NONE',  ( 0.7681833999686413783, -81.32291666666667140, 0.9995835529977274980 ) ) ;
#46794 = CARTESIAN_POINT ( 'NONE',  ( -0.8804656548076286171, -61.82803394674684228, -12.70299681155893268 ) ) ;
#46795 = CARTESIAN_POINT ( 'NONE',  ( -9.702231720816998362, -78.77143470455798990, -0.1934140619087000024 ) ) ;
#46796 = DIRECTION ( 'NONE',  ( 0.000000000000000000, 0.000000000000000000, 1.000000000000000000 ) ) ;
#46797 = CARTESIAN_POINT ( 'NONE',  ( 1.249999999999999778, -79.76041666666665719, 0.1636246173744711763 ) ) ;
#46798 = FACE_OUTER_BOUND ( 'NONE', #21063, .T. ) ;
#46799 = CARTESIAN_POINT ( 'NONE',  ( 1.539929345890999945, -79.97582157143999382, 0.3781723503825999422 ) ) ;
#46800 = CARTESIAN_POINT ( 'NONE',  ( 2.150476488323003199, -77.40657193750340070, 9.198929323063223862 ) ) ;
#46801 = B_SPLINE_CURVE_WITH_KNOTS ( 'NONE', 3,
 ( #23385, #18381, #36084, #18091, #36667, #13938 ),
 .UNSPECIFIED., .F., .F.,
 ( 4, 1, 1, 4 ),
 ( 0.000000000000000000, 0.3333333333333000081, 0.6666666666667000474, 1.000000000000000000 ),
 .UNSPECIFIED. ) ;
#46802 = CARTESIAN_POINT ( 'NONE',  ( 6.277130266346461873, -79.23046873804318579, -10.24763708790730554 ) ) ;
#46803 = CARTESIAN_POINT ( 'NONE',  ( -10.00831378476999944, -55.42769332259999260, 7.646786280026000249 ) ) ;
#46804 = CARTESIAN_POINT ( 'NONE',  ( -10.24999999991999999, -82.10000000007899246, 6.817355505960000646E-10 ) ) ;
#46805 = CARTESIAN_POINT ( 'NONE',  ( 2.062503053667999797, -21.75736537952000305, -12.92177931904999966 ) ) ;
#46806 = AXIS2_PLACEMENT_3D ( 'NONE', #7141, #42298, #19558 ) ;
#46808 = CARTESIAN_POINT ( 'NONE',  ( 1.929975092517999924, -18.79892743736000327, -12.72537404210999945 ) ) ;
#46807 = CARTESIAN_POINT ( 'NONE',  ( 1.310679582531385501, -78.69166666666669130, 0.7554284705563518720 ) ) ;
#46809 = CARTESIAN_POINT ( 'NONE',  ( 9.500000000000000000, -78.64999999999999147, 0.000000000000000000 ) ) ;
#46810 = CARTESIAN_POINT ( 'NONE',  ( 0.000000000000000000, -13.07071424677999971, 0.000000000000000000 ) ) ;
#46811 = CARTESIAN_POINT ( 'NONE',  ( -10.09586848912000079, -78.28687501975998941, 4.990731814912999553 ) ) ;
#46812 = AXIS2_PLACEMENT_3D ( 'NONE', #1231, #50232, #23057 ) ;
#46813 = CARTESIAN_POINT ( 'NONE',  ( 2.862077683958035301, -1.551983691494210005, 2.221749198134896464 ) ) ;
#46814 = AXIS2_PLACEMENT_3D ( 'NONE', #21563, #57571, #22434 ) ;
#46815 = ORIENTED_EDGE ( 'NONE', *, *, #42973, .T. ) ;
#46816 = CARTESIAN_POINT ( 'NONE',  ( -5.911015991356902255, -78.88333333333332575, -10.22919423418180074 ) ) ;
#46817 = CARTESIAN_POINT ( 'NONE',  ( 7.342331066867000544, -59.94999999967000548, -8.190859204290999784 ) ) ;
#46818 = DIRECTION ( 'NONE',  ( 0.7071067811865474617, 0.000000000000000000, -0.7071067811865474617 ) ) ;
#46819 = CARTESIAN_POINT ( 'NONE',  ( -3.765737196849845869, -77.19487930045538349, -8.507847610243468139 ) ) ;
#46820 = CARTESIAN_POINT ( 'NONE',  ( 9.582741442650998920, -79.65192808831000093, 1.072080763990999941 ) ) ;
#46821 = CARTESIAN_POINT ( 'NONE',  ( 12.55432891853855004, -18.61272687758708599, -1.749897736042411944 ) ) ;
#46822 = CARTESIAN_POINT ( 'NONE',  ( -1.293318857230095320, -79.48473999591016081, 10.67184061187126431 ) ) ;
#46823 = CARTESIAN_POINT ( 'NONE',  ( -8.796272286055000222, -79.47841332859898955, -4.179787317773000943 ) ) ;
#46824 = DIRECTION ( 'NONE',  ( 0.000000000000000000, 1.000000000000000000, 0.000000000000000000 ) ) ;
#46825 = CARTESIAN_POINT ( 'NONE',  ( -0.008395553423636001322, -77.55424564813398547, 11.27412384287999991 ) ) ;
#46826 = CARTESIAN_POINT ( 'NONE',  ( 1.515699252679999942, -81.68459978947099387, 0.5251668156352999883 ) ) ;
#46827 = CARTESIAN_POINT ( 'NONE',  ( -3.039602602085999639, -79.24969514476062216, -9.236151215514999180 ) ) ;
#46828 = CARTESIAN_POINT ( 'NONE',  ( 1.500000000000000000, -81.15000000000000568, 0.000000000000000000 ) ) ;
#46830 = CARTESIAN_POINT ( 'NONE',  ( -9.722718241315000398, -18.75000000000000000, -7.954951288349001004 ) ) ;
#46829 = CARTESIAN_POINT ( 'NONE',  ( 3.962859227717999921, -85.14779509595699380, 0.04167563340643000436 ) ) ;
#46831 = CARTESIAN_POINT ( 'NONE',  ( 5.684029094576000141, -79.86585584965399676, -7.680196531179999120 ) ) ;
#46832 = CARTESIAN_POINT ( 'NONE',  ( 1.217465845835394855, -82.72916666666667140, -0.3271848554490981997 ) ) ;
#46833 = CARTESIAN_POINT ( 'NONE',  ( 4.993368691432944040, -80.26375664158507561, -9.522208454640370690 ) ) ;
#46834 = CARTESIAN_POINT ( 'NONE',  ( -6.863878448621095529, -77.16995529938667175, -8.273635171295007140 ) ) ;
#46835 = CARTESIAN_POINT ( 'NONE',  ( -7.596835002782739821, -77.34791666666667709, 5.838193839761659731 ) ) ;
#46836 = EDGE_CURVE ( 'NONE', #50939, #54943, #7395, .T. ) ;
#46837 = ORIENTED_EDGE ( 'NONE', *, *, #50654, .F. ) ;
#46838 = ORIENTED_EDGE ( 'NONE', *, *, #46522, .F. ) ;
#46839 = CARTESIAN_POINT ( 'NONE',  ( 2.377756013412999803, -79.27472795551499019, -11.79209151100000064 ) ) ;
#46840 = DIRECTION ( 'NONE',  ( 0.000000000000000000, -1.000000000000000000, 0.000000000000000000 ) ) ;
#46841 = CARTESIAN_POINT ( 'NONE',  ( -10.12290050253000118, -23.24999997822999731, 7.648026768374000639 ) ) ;
#46842 = ORIENTED_EDGE ( 'NONE', *, *, #44473, .F. ) ;
#46843 = CARTESIAN_POINT ( 'NONE',  ( 7.889971116623999414, -77.44093201713099006, 8.954543982858998774 ) ) ;
#46844 = ORIENTED_EDGE ( 'NONE', *, *, #22695, .T. ) ;
#46845 = ORIENTED_EDGE ( 'NONE', *, *, #54106, .T. ) ;
#46846 = ORIENTED_EDGE ( 'NONE', *, *, #28163, .T. ) ;
#46847 = EDGE_CURVE ( 'NONE', #3549, #41145, #1777, .T. ) ;
#46848 = CARTESIAN_POINT ( 'NONE',  ( 3.440741810271999768, -82.41509632510098982, -0.2267889765191999918 ) ) ;
#46849 = CARTESIAN_POINT ( 'NONE',  ( 9.019879307700605864, -79.17500127585684311, 2.981309166188937265 ) ) ;
#46850 = EDGE_LOOP ( 'NONE', ( #9295, #28496, #31233, #9770 ) ) ;
#46851 = CARTESIAN_POINT ( 'NONE',  ( 0.3708152058599178957, -82.74916602882588279, -1.193631158523653424 ) ) ;
#46852 = ORIENTED_EDGE ( 'NONE', *, *, #14913, .T. ) ;
#46853 = CARTESIAN_POINT ( 'NONE',  ( 3.188330803860000007, -2.833935831311999998, 1.184873324962000041 ) ) ;
#46854 = ORIENTED_EDGE ( 'NONE', *, *, #3749, .T. ) ;
#46855 = DIRECTION ( 'NONE',  ( 1.000000000000000000, 0.000000000000000000, 0.000000000000000000 ) ) ;
#46856 = CARTESIAN_POINT ( 'NONE',  ( -1.374356897932604848, -78.71628694306663476, 0.6198793800460191683 ) ) ;
#46857 = AXIS2_PLACEMENT_3D ( 'NONE', #51125, #28659, #46707 ) ;
#46858 = CARTESIAN_POINT ( 'NONE',  ( 11.75000000000000000, -79.79999999999999716, -4.009019365174000020E-13 ) ) ;
#46859 = CARTESIAN_POINT ( 'NONE',  ( -10.60742839163532736, -80.08734568579502877, 1.743969048105956876 ) ) ;
#46860 = CARTESIAN_POINT ( 'NONE',  ( 11.93290200807439660, -79.18167642368507586, -2.830846369544400609 ) ) ;
#46861 = CARTESIAN_POINT ( 'NONE',  ( -9.022250383429000209, -78.78001047183876437, -3.573472734901999903 ) ) ;
#46863 = ADVANCED_FACE ( 'NONE', ( #53983 ), #14113, .F. ) ;
#46862 = CARTESIAN_POINT ( 'NONE',  ( 9.886069181790999139, -76.47739146390900089, -5.228720670581999741 ) ) ;
#46864 = CARTESIAN_POINT ( 'NONE',  ( 9.655991824031183057, -79.60868651084126668, 1.080275738811528718 ) ) ;
#46865 = EDGE_CURVE ( 'NONE', #7685, #36041, #26800, .T. ) ;
#46866 = CARTESIAN_POINT ( 'NONE',  ( -1.971120042941999939, -76.43436737597099295, -11.05433917436000080 ) ) ;
#46867 = CARTESIAN_POINT ( 'NONE',  ( -2.116425671828475519, -78.70676334617536440, -9.010145557416606721 ) ) ;
#46868 = CARTESIAN_POINT ( 'NONE',  ( 6.715696511375072397, -76.52634182472844770, 9.641850707901006956 ) ) ;
#46869 = CARTESIAN_POINT ( 'NONE',  ( 0.5173218454072999739, -79.56518678517799970, 1.229208833401000067 ) ) ;
#46870 = DIRECTION ( 'NONE',  ( -1.000000000000000000, 0.000000000000000000, 0.000000000000000000 ) ) ;
#46871 = CARTESIAN_POINT ( 'NONE',  ( -0.3664097495403158544, -61.77190017435498959, -12.50575740046304674 ) ) ;
#46872 = CARTESIAN_POINT ( 'NONE',  ( -1.778395558963000056, -79.76042549782599167, 3.117859321502000292 ) ) ;
#46873 = CARTESIAN_POINT ( 'NONE',  ( 12.07833837140000099, -79.82418736905719925, -0.3648754035837999954 ) ) ;
#46874 = CARTESIAN_POINT ( 'NONE',  ( -8.845454740156757367, -78.05205573245035566, 6.111140252778515247 ) ) ;
#46875 = CARTESIAN_POINT ( 'NONE',  ( 0.6069111558698970788, -82.93513506220737952, 1.101446694455507913 ) ) ;
#46876 = PLANE ( 'NONE',  #41536 ) ;
#46877 = CARTESIAN_POINT ( 'NONE',  ( 10.04115011120000034, -19.23513569609999863, 7.682331425195999763 ) ) ;
#46878 = CARTESIAN_POINT ( 'NONE',  ( -10.15323304115999825, -61.03079615981999950, -7.760925857031000241 ) ) ;
#46879 = CARTESIAN_POINT ( 'NONE',  ( 0.000000000000000000, -91.29999999999999716, 0.000000000000000000 ) ) ;
#46880 = CARTESIAN_POINT ( 'NONE',  ( -1.500000000000000000, -77.50000000000000000, 0.000000000000000000 ) ) ;
#46881 = CARTESIAN_POINT ( 'NONE',  ( -0.06244121081497999715, -3.420791625799999736, 3.484461396181999682 ) ) ;
#46882 = CARTESIAN_POINT ( 'NONE',  ( -4.000000000000000000, -5.000000000000000000, -0.5999999999999999778 ) ) ;
#46883 = CARTESIAN_POINT ( 'NONE',  ( 12.43647262253000108, -24.91807034734999959, -0.03492325570150000419 ) ) ;
#46884 = ADVANCED_FACE ( 'NONE', ( #5262, #36551 ), #40092, .F. ) ;
#46885 = CIRCLE ( 'NONE', #58191, 0.5000000000000006661 ) ;
#46886 = CARTESIAN_POINT ( 'NONE',  ( -1.148062820858973154, -78.06710658568482586, -10.77713783125740044 ) ) ;
#46887 = CARTESIAN_POINT ( 'NONE',  ( 0.000000000000000000, -18.75000000000000000, -12.00000000000000000 ) ) ;
#46888 = CARTESIAN_POINT ( 'NONE',  ( 10.71556987377000070, -79.61735645562259833, 2.374990294079000197 ) ) ;
#46889 = CARTESIAN_POINT ( 'NONE',  ( -8.992856345071000845, -76.69757595554999341, 8.038460196811000102 ) ) ;
#46890 = ORIENTED_EDGE ( 'NONE', *, *, #56903, .T. ) ;
#46891 = CIRCLE ( 'NONE', #6323, 0.5000000000000004441 ) ;
#46892 = CARTESIAN_POINT ( 'NONE',  ( 3.308763867269000070, -85.63696544543098810, -1.778607282991000016 ) ) ;
#46893 = CARTESIAN_POINT ( 'NONE',  ( 3.773599593829000121, -80.36098609305189200, -10.63964551222000132 ) ) ;
#46894 = VECTOR ( 'NONE', #30660, 1000.000000000000227 ) ;
#46895 = CARTESIAN_POINT ( 'NONE',  ( 8.278135427829594661, -78.31322909081512762, -4.127880705928267169 ) ) ;
#46896 = CARTESIAN_POINT ( 'NONE',  ( 7.635939924770683618, -55.02474192263417763, 10.36595855978725744 ) ) ;
#46897 = CARTESIAN_POINT ( 'NONE',  ( 9.070694317316998934, -78.20173038828299639, 6.598531290616000078 ) ) ;
#46898 = DIRECTION ( 'NONE',  ( 0.7071067811865475727, 0.000000000000000000, 0.7071067811865475727 ) ) ;
#46899 = CARTESIAN_POINT ( 'NONE',  ( 4.561861969681999973, -77.66539556192998361, 8.605179316909000065 ) ) ;
#46900 = VECTOR ( 'NONE', #10076, 1000.000000000000000 ) ;
#46901 = CARTESIAN_POINT ( 'NONE',  ( 3.044259723400999817, -84.14857643474398685, 2.852899930898999958 ) ) ;
#46902 = DIRECTION ( 'NONE',  ( 0.000000000000000000, 0.000000000000000000, 1.000000000000000000 ) ) ;
#46903 = CARTESIAN_POINT ( 'NONE',  ( 1.185193155257999953, -79.68253060846500091, -1.096599795159000079 ) ) ;
#46904 = VERTEX_POINT ( 'NONE', #9402 ) ;
#46905 = CARTESIAN_POINT ( 'NONE',  ( -1.081559480311999888, -0.7500000000000000000, 3.328697807033000000 ) ) ;
#46906 = CARTESIAN_POINT ( 'NONE',  ( -9.250000000000000000, -79.09999999999999432, 1.813240672189999963E-14 ) ) ;
#46907 = CARTESIAN_POINT ( 'NONE',  ( 2.589388593803659600, -78.97650220697799739, -2.803363233735876481 ) ) ;
#46908 = ORIENTED_EDGE ( 'NONE', *, *, #21054, .T. ) ;
#46909 = CARTESIAN_POINT ( 'NONE',  ( -1.150888948972000003, -79.09218682990699278, 0.6738713386821000295 ) ) ;
#46910 = CARTESIAN_POINT ( 'NONE',  ( 0.2040051533403345885, -80.73872320341082798, -1.234301858716469580 ) ) ;
#46911 = ORIENTED_EDGE ( 'NONE', *, *, #27540, .T. ) ;
#46912 = CARTESIAN_POINT ( 'NONE',  ( -3.132815200277000223, -78.36313629324600072, -11.75448848339000030 ) ) ;
#46913 = CARTESIAN_POINT ( 'NONE',  ( -1.359921359492999970, -78.00530199648000007, 11.35132765128000010 ) ) ;
#46914 = CARTESIAN_POINT ( 'NONE',  ( 5.195844325042688006, -78.66486225622416839, -9.480952556279184762 ) ) ;
#46915 = EDGE_LOOP ( 'NONE', ( #28904, #21237, #40416, #36902 ) ) ;
#46916 = ORIENTED_EDGE ( 'NONE', *, *, #3651, .T. ) ;
#46917 = CARTESIAN_POINT ( 'NONE',  ( -0.7411337730108847888, -80.52597511522522211, 1.006651954983204700 ) ) ;
#46918 = EDGE_CURVE ( 'NONE', #52919, #51909, #49859, .T. ) ;
#46919 = CARTESIAN_POINT ( 'NONE',  ( 10.47018369756723288, -77.82921409177868100, -2.813855853172428478 ) ) ;
#46920 = CARTESIAN_POINT ( 'NONE',  ( -9.687172913667000174, -80.26021482710652322, -1.248753675804000096 ) ) ;
#46921 = ORIENTED_EDGE ( 'NONE', *, *, #38456, .F. ) ;
#46922 = CARTESIAN_POINT ( 'NONE',  ( 12.59651451715000015, -55.40944962329000134, 1.801708894189000043 ) ) ;
#46923 = CARTESIAN_POINT ( 'NONE',  ( 10.26057445098000187, -78.35114051593500051, 3.727731092327000173 ) ) ;
#46924 = EDGE_CURVE ( 'NONE', #34639, #22699, #36032, .T. ) ;
#46925 = ORIENTED_EDGE ( 'NONE', *, *, #17552, .T. ) ;
#46926 = CARTESIAN_POINT ( 'NONE',  ( -12.43647262253000108, -24.91807034734999959, 0.03492325570151000314 ) ) ;
#46927 = CARTESIAN_POINT ( 'NONE',  ( 1.974456364585935431, -78.69999999999998863, -3.418760544058775164 ) ) ;
#46928 = CIRCLE ( 'NONE', #10163, 12.05000000000000071 ) ;
#46929 = CARTESIAN_POINT ( 'NONE',  ( 0.000000000000000000, -75.19999999999998863, 0.000000000000000000 ) ) ;
#46930 = CARTESIAN_POINT ( 'NONE',  ( -12.50000000000000000, -13.07071422275999950, 0.000000000000000000 ) ) ;
#46931 = CARTESIAN_POINT ( 'NONE',  ( -9.500000000000000000, -87.20000000000000284, 0.000000000000000000 ) ) ;
#46932 = CARTESIAN_POINT ( 'NONE',  ( -8.873325971494777420, -78.58267913613843803, -3.979643097409233832 ) ) ;
#46933 = CARTESIAN_POINT ( 'NONE',  ( -6.089781427445000617, -77.04533417779047966, 7.498689922205000080 ) ) ;
#46934 = EDGE_CURVE ( 'NONE', #3531, #9865, #50212, .T. ) ;
#46935 = VECTOR ( 'NONE', #23433, 999.9999999999998863 ) ;
#46936 = CARTESIAN_POINT ( 'NONE',  ( -1.265047507048352449, -79.30228839861766232, 0.8556988754165529842 ) ) ;
#46937 = CARTESIAN_POINT ( 'NONE',  ( 0.7265058034139308951, -81.28229167440642300, 3.986460672241819214 ) ) ;
#46938 = CARTESIAN_POINT ( 'NONE',  ( -7.450482419345999752, -76.09060268177999831, -9.799277032148999922 ) ) ;
#46939 = VECTOR ( 'NONE', #42569, 1000.000000000000000 ) ;
#46940 = CARTESIAN_POINT ( 'NONE',  ( 2.905710011617722355, -77.07499999989397566, -8.943793187339698747 ) ) ;
#46941 = DIRECTION ( 'NONE',  ( 1.000000000000000000, 0.000000000000000000, 0.000000000000000000 ) ) ;
#46942 = AXIS2_PLACEMENT_3D ( 'NONE', #11166, #6423, #24727 ) ;
#46943 = CARTESIAN_POINT ( 'NONE',  ( 0.4482635754052999855, -78.57590936191000708, -12.25553529036999834 ) ) ;
#46944 = CARTESIAN_POINT ( 'NONE',  ( -12.27595451887999900, -76.13162234490400238, 0.3505736730271999391 ) ) ;
#46945 = DIRECTION ( 'NONE',  ( 0.000000000000000000, -1.000000000000000000, 0.000000000000000000 ) ) ;
#46946 = CARTESIAN_POINT ( 'NONE',  ( 1.705242708866661738, -2.770368159655117957, -2.767455873028740854 ) ) ;
#46947 = CARTESIAN_POINT ( 'NONE',  ( 8.193144588781670734, -78.23440087569812817, -8.866198533586608477 ) ) ;
#46948 = DIRECTION ( 'NONE',  ( 0.000000000000000000, 0.000000000000000000, -1.000000000000000000 ) ) ;
#46949 = ORIENTED_EDGE ( 'NONE', *, *, #500, .T. ) ;
#46950 = CARTESIAN_POINT ( 'NONE',  ( 1.274651354540000003, -83.24304616690000103, -0.4485964608026000167 ) ) ;
#46951 = CARTESIAN_POINT ( 'NONE',  ( -3.802343155576000111, -76.98502847823358763, -8.627496936359001722 ) ) ;
#46952 = DIRECTION ( 'NONE',  ( 1.000000000000000000, 0.000000000000000000, 0.000000000000000000 ) ) ;
#46953 = CARTESIAN_POINT ( 'NONE',  ( 1.250000000000000000, -78.75000000000000000, 0.000000000000000000 ) ) ;
#46954 = CARTESIAN_POINT ( 'NONE',  ( -3.558211308106999926, -3.404594557569000202, -1.064603940041000119 ) ) ;
#46955 = CARTESIAN_POINT ( 'NONE',  ( -1.368150018649999966, -77.62480861561799372, -11.97179757597999838 ) ) ;
#46956 = CARTESIAN_POINT ( 'NONE',  ( -7.735308924444000311, -77.32278449298998169, -5.918161214274000770 ) ) ;
#46958 = CARTESIAN_POINT ( 'NONE',  ( 1.750000000000000000, -23.25000000000000000, 12.00000000000000000 ) ) ;
#46957 = CARTESIAN_POINT ( 'NONE',  ( -10.85381960069883611, -76.16858560240085296, 4.500525175705931247 ) ) ;
#46959 = CARTESIAN_POINT ( 'NONE',  ( 0.5113695407423999306, -82.42414080993400205, 1.250788716666000111 ) ) ;
#46960 = CARTESIAN_POINT ( 'NONE',  ( 9.505949683906999681, -79.00000000000000000, 6.906476714433999575 ) ) ;
#46961 = ORIENTED_EDGE ( 'NONE', *, *, #22891, .T. ) ;
#46962 = CARTESIAN_POINT ( 'NONE',  ( -0.1250341999720059050, -81.01872301050605074, -1.526447402715753965 ) ) ;
#46963 = CARTESIAN_POINT ( 'NONE',  ( -7.396685970965884316, -78.04807098620916861, 5.684396067267562636 ) ) ;
#46964 = CARTESIAN_POINT ( 'NONE',  ( -2.598917237794094337, -2.447916666666666519, 1.997276839918461722 ) ) ;
#46965 = CARTESIAN_POINT ( 'NONE',  ( -0.4877242113430015902, -82.25000000000000000, -1.155856577702833343 ) ) ;
#46966 = CARTESIAN_POINT ( 'NONE',  ( 0.000000000000000000, -75.67500000000001137, 0.000000000000000000 ) ) ;
#46967 = CARTESIAN_POINT ( 'NONE',  ( -2.801260334388999684, -79.18052108146299872, -9.140240961675001330 ) ) ;
#46968 = CARTESIAN_POINT ( 'NONE',  ( 3.250000000000000000, -3.350000000000000089, 0.000000000000000000 ) ) ;
#46969 = CARTESIAN_POINT ( 'NONE',  ( 7.714303428875997959, -63.10294702886003648, -12.53545825868000385 ) ) ;
#46970 = ORIENTED_EDGE ( 'NONE', *, *, #53943, .F. ) ;
#46971 = EDGE_CURVE ( 'NONE', #33522, #21810, #34162, .T. ) ;
#46972 = CARTESIAN_POINT ( 'NONE',  ( 11.20174477810000013, -79.53483005723899169, 1.163992476170999879 ) ) ;
#46973 = CARTESIAN_POINT ( 'NONE',  ( 7.958776492191999452, -24.47699850276000078, -9.723157982392999443 ) ) ;
#46974 = DIRECTION ( 'NONE',  ( -0.7071067811865475727, 0.000000000000000000, -0.7071067811865475727 ) ) ;
#46975 = CARTESIAN_POINT ( 'NONE',  ( 3.400000000000109601, -78.67390000031815589, 2.006589450846672840 ) ) ;
#46976 = CARTESIAN_POINT ( 'NONE',  ( 0.2838762717877208464, -77.82609350274218230, 12.06818374436646124 ) ) ;
#46977 = B_SPLINE_SURFACE_WITH_KNOTS ( 'NONE', 3, 3, ( 
 ( #21362, #33488, #51528, #20225 ),
 ( #11371, #29348, #47394, #42950 ),
 ( #2507, #20511, #35504, #17221 ),
 ( #27236, #12506, #16944, #53533 ),
 ( #49109, #21934, #44380, #17513 ),
 ( #48533, #44977, #57960, #26645 ),
 ( #31071, #26944, #58257, #48821 ),
 ( #4824, #30505, #36107, #4234 ),
 ( #4532, #22532, #22823, #8659 ),
 ( #40542, #137, #57664, #17817 ),
 ( #49706, #13074, #44100, #26075 ),
 ( #3649, #40243, #12788, #18113 ),
 ( #9252, #22231, #44681, #35804 ),
 ( #13368, #45275, #53833, #31366 ),
 ( #54124, #21652, #13665, #31660 ),
 ( #35210, #49411, #40833, #8959 ),
 ( #34925, #52957, #8078, #53240 ) ),
 .UNSPECIFIED., .F., .F., .F.,
 ( 4, 1, 1, 1, 1, 1, 1, 1, 1, 1, 1, 1, 1, 1, 4 ),
 ( 4, 4 ),
 ( -0.01011408452864000045, 0.000000000000000000, 0.08333333333333001192, 0.1666666666667000196, 0.2500000000000000000, 0.3333333333333000081, 0.4166666666666999919, 0.5000000000000000000, 0.5833333333333000637, 0.6666666666667000474, 0.7500000000000000000, 0.8333333333333000637, 0.9166666666667000474, 1.000000000000000000, 1.010362559107000013 ),
 ( -0.3559705546267999954, 1.357612419580000118 ),
 .UNSPECIFIED. ) ;
#46978 = VECTOR ( 'NONE', #12546, 1000.000000000000000 ) ;
#46979 = CARTESIAN_POINT ( 'NONE',  ( -0.07738748721609896297, -81.48033942009458030, 1.247494957338889821 ) ) ;
#46980 = CARTESIAN_POINT ( 'NONE',  ( -1.271001786909834452, -79.14473929417310671, 0.08712350718595020249 ) ) ;
#46981 = CARTESIAN_POINT ( 'NONE',  ( 0.9995416268372391277, -82.29857430458693557, -0.7677867857872645585 ) ) ;
#46982 = CARTESIAN_POINT ( 'NONE',  ( -7.639893274927808342, -23.38715751204584237, -10.11462445490720974 ) ) ;
#46983 = AXIS2_PLACEMENT_3D ( 'NONE', #9051, #232, #18211 ) ;
#46984 = DIRECTION ( 'NONE',  ( 1.000000000000000000, 0.000000000000000000, 0.000000000000000000 ) ) ;
#46985 = CARTESIAN_POINT ( 'NONE',  ( -8.758933146614412024, -79.90041885450349923, 6.307249761326839455 ) ) ;
#46986 = CARTESIAN_POINT ( 'NONE',  ( -10.48543666025111420, -77.25833333333331154, 6.043427764450754580 ) ) ;
#46987 = VERTEX_POINT ( 'NONE', #9109 ) ;
#46988 = VERTEX_POINT ( 'NONE', #579 ) ;
#46989 = CARTESIAN_POINT ( 'NONE',  ( 2.075550720420999973, -78.02093998579799461, -9.805082477504999616 ) ) ;
#46990 = CARTESIAN_POINT ( 'NONE',  ( 1.669271706869820404, -78.73747607613988464, -10.62851245282890744 ) ) ;
#46991 = EDGE_CURVE ( 'NONE', #47432, #15756, #50150, .T. ) ;
#46992 = ORIENTED_EDGE ( 'NONE', *, *, #3886, .T. ) ;
#46993 = CARTESIAN_POINT ( 'NONE',  ( 7.646788101826000883, -18.62771363264999991, 10.00831428591000005 ) ) ;
#46994 = CARTESIAN_POINT ( 'NONE',  ( -9.471485474656741843, -79.39369676562593270, 0.7342151353995368668 ) ) ;
#46995 = CARTESIAN_POINT ( 'NONE',  ( -3.361591574393000048, -78.22944319244000155, 11.31358112888999834 ) ) ;
#46996 = CARTESIAN_POINT ( 'NONE',  ( 10.75000000000000000, -79.84999999999999432, -2.184490103126999767E-14 ) ) ;
#46997 = FACE_BOUND ( 'NONE', #50899, .T. ) ;
#46998 = CARTESIAN_POINT ( 'NONE',  ( 1.353569424327082826, -86.12609999968211127, 3.118950113984548800 ) ) ;
#46999 = CARTESIAN_POINT ( 'NONE',  ( 2.039250879084999912, -80.04123109255959889, -11.02993955029000084 ) ) ;
#47000 = EDGE_CURVE ( 'NONE', #28385, #7685, #31218, .T. ) ;
#47001 = ORIENTED_EDGE ( 'NONE', *, *, #40352, .T. ) ;
#47002 = CARTESIAN_POINT ( 'NONE',  ( 12.05000000000000071, -74.80000000000001137, 0.000000000000000000 ) ) ;
#47003 = VERTEX_POINT ( 'NONE', #54850 ) ;
#47004 = CARTESIAN_POINT ( 'NONE',  ( 8.796548128639548381, -77.37506330577387814, 2.860527516076478260 ) ) ;
#47005 = CARTESIAN_POINT ( 'NONE',  ( 8.680753609988000719, -77.79345393914999818, 6.821192461343000168 ) ) ;
#47006 = CARTESIAN_POINT ( 'NONE',  ( 2.855009615267027900, -78.20442848851632789, 10.84760476142250418 ) ) ;
#47007 = LINE ( 'NONE', #6537, #48502 ) ;
#47008 = CARTESIAN_POINT ( 'NONE',  ( -9.546815224142999767, -17.31472046677999899, -8.130854305520999858 ) ) ;
#47009 = CONICAL_SURFACE ( 'NONE', #9274, 0.6999999997695030007, 0.7853981633972997312 ) ;
#47010 = CARTESIAN_POINT ( 'NONE',  ( 10.47020627418438643, -80.77083333333332860, 2.813789756862283387 ) ) ;
#47011 = CARTESIAN_POINT ( 'NONE',  ( -0.6794254437148999903, -78.92033711567999887, -1.478865823597000029 ) ) ;
#47012 = CARTESIAN_POINT ( 'NONE',  ( -7.678690995204998870, -21.75648180056000314, 10.59551070212000035 ) ) ;
#47013 = CARTESIAN_POINT ( 'NONE',  ( 10.62704985177000161, -78.72100192322298540, -3.023855997759000047 ) ) ;
#47014 = CARTESIAN_POINT ( 'NONE',  ( 0.000000000000000000, -0.7781249991808000255, -3.471875000818999801 ) ) ;
#47015 = CARTESIAN_POINT ( 'NONE',  ( -0.7406579117306999471, -79.52990259888842672, 12.00660533699000077 ) ) ;
#47016 = FACE_OUTER_BOUND ( 'NONE', #25322, .T. ) ;
#47017 = CARTESIAN_POINT ( 'NONE',  ( -3.315867686165999917, -86.07743221058099437, 0.9362964062973999635 ) ) ;
#47018 = VERTEX_POINT ( 'NONE', #30927 ) ;
#47019 = CARTESIAN_POINT ( 'NONE',  ( -9.993863819922085057, -77.19999999999998863, 4.482211430344825054 ) ) ;
#47020 = CARTESIAN_POINT ( 'NONE',  ( -0.6472661464068000248, -81.23605406588998790, 1.575051776950999960 ) ) ;
#47021 = CARTESIAN_POINT ( 'NONE',  ( 10.10912517728393567, -60.27586858096238132, 7.634643689465026917 ) ) ;
#47022 = CARTESIAN_POINT ( 'NONE',  ( -11.92766985523999956, -77.64132209835500475, -1.116582401450000095 ) ) ;
#47023 = CARTESIAN_POINT ( 'NONE',  ( -8.813906587716449081, -53.78989792558626704, 8.872948314128050740 ) ) ;
#47024 = CARTESIAN_POINT ( 'NONE',  ( -0.5694255183457415104, -78.33855170281904634, -1.140105177683416127 ) ) ;
#47025 = VECTOR ( 'NONE', #6546, 1000.000000000000000 ) ;
#47026 = CARTESIAN_POINT ( 'NONE',  ( 3.500000000000000000, -3.500000000000000000, 1.049058100190999900E-13 ) ) ;
#47027 = CARTESIAN_POINT ( 'NONE',  ( 8.219513559211000242, -78.98500584965400151, 5.194554602171000290 ) ) ;
#47028 = CARTESIAN_POINT ( 'NONE',  ( -5.574784109570000368, -78.21829086006698617, -7.719595738358999704 ) ) ;
#47029 = CARTESIAN_POINT ( 'NONE',  ( 1.249469270068990001, -81.33640427608399648, -0.2274969907241829736 ) ) ;
#47030 = CARTESIAN_POINT ( 'NONE',  ( 11.00720109383000000, -77.71418423053899005, 0.7370606905150999255 ) ) ;
#47031 = DIRECTION ( 'NONE',  ( 0.7071067811865474617, -0.7071067811865474617, 3.873929780297256383E-09 ) ) ;
#47032 = CARTESIAN_POINT ( 'NONE',  ( -10.02512094469000026, -81.05887381952659609, -4.305871809879999290 ) ) ;
#47033 = CARTESIAN_POINT ( 'NONE',  ( -0.9692428243007442656, -81.59356749952172549, 0.8270901151029305121 ) ) ;
#47034 = VERTEX_POINT ( 'NONE', #58106 ) ;
#47035 = CARTESIAN_POINT ( 'NONE',  ( 1.289124607492999841, -81.03627781387399409, 0.3416633729347999804 ) ) ;
#47036 = CARTESIAN_POINT ( 'NONE',  ( -1.382886570147999983, -61.43098219798999793, -12.65982054480000052 ) ) ;
#47037 = CYLINDRICAL_SURFACE ( 'NONE', #37088, 1.750000000000001332 ) ;
#47038 = CARTESIAN_POINT ( 'NONE',  ( -10.93308570624999909, -78.35183257902099285, -2.507139558745000052 ) ) ;
#47039 = CARTESIAN_POINT ( 'NONE',  ( 0.1291013223160000223, -79.18360955475999674, 10.97485077029999978 ) ) ;
#47040 = CARTESIAN_POINT ( 'NONE',  ( 9.523353692535000192, -24.81947015623000041, -8.220363114681999761 ) ) ;
#47041 = CARTESIAN_POINT ( 'NONE',  ( 3.973714814374760262, -85.48333334632451397, 0.5577315370174421583 ) ) ;
#47042 = CARTESIAN_POINT ( 'NONE',  ( -10.43912668352000139, -76.61936152454400428, -6.221750613054999768 ) ) ;
#47043 = CARTESIAN_POINT ( 'NONE',  ( 6.519098162841222788, -78.52704705454330281, 9.775845571359413455 ) ) ;
#47044 = CARTESIAN_POINT ( 'NONE',  ( -1.043587583837393806, -81.14777710806242794, -0.7040735577254533251 ) ) ;
#47045 = VERTEX_POINT ( 'NONE', #40395 ) ;
#47046 = EDGE_CURVE ( 'NONE', #4000, #17032, #48966, .T. ) ;
#47047 = CARTESIAN_POINT ( 'NONE',  ( -0.5187597050509943353, -80.00936726310753500, 1.137174289053646703 ) ) ;
#47048 = CARTESIAN_POINT ( 'NONE',  ( 2.421167930323324224, -78.14583333333331439, -9.009247259181924150 ) ) ;
#47049 = EDGE_CURVE ( 'NONE', #32490, #21905, #7762, .T. ) ;
#47050 = CARTESIAN_POINT ( 'NONE',  ( 7.658894278873999539, -55.59060682883999505, -10.01676917980999981 ) ) ;
#47051 = CARTESIAN_POINT ( 'NONE',  ( 7.410162453131999172, -78.99706562342599625, 8.486367113423000319 ) ) ;
#47052 = CARTESIAN_POINT ( 'NONE',  ( -12.50000000000000000, -18.55321828668999729, 1.250000000000000000 ) ) ;
#47053 = CARTESIAN_POINT ( 'NONE',  ( -7.648026766735999793, -23.25000000582000226, 10.12290050089000104 ) ) ;
#47054 = CARTESIAN_POINT ( 'NONE',  ( -0.2340378853370451706, -82.13661640029980049, 1.530701560988515064 ) ) ;
#47055 = DIRECTION ( 'NONE',  ( 1.000000000000000000, 0.000000000000000000, 0.000000000000000000 ) ) ;
#47056 = CARTESIAN_POINT ( 'NONE',  ( -0.8258380295080043343, -79.66783667981496819, -0.9386737271208877020 ) ) ;
#47057 = AXIS2_PLACEMENT_3D ( 'NONE', #32963, #9973, #6114 ) ;
#47058 = CARTESIAN_POINT ( 'NONE',  ( -9.073547343405500953, -53.57191135162067752, 8.894853367357773877 ) ) ;
#47059 = VERTEX_POINT ( 'NONE', #13224 ) ;
#47060 = CARTESIAN_POINT ( 'NONE',  ( -0.4746745519540126468, -81.69413255355395620, -1.156278043614258566 ) ) ;
#47061 = SURFACE_STYLE_USAGE ( .BOTH. , #50607 ) ;
#47062 = CARTESIAN_POINT ( 'NONE',  ( -6.103876716051000351, -79.88052105083718857, 9.189364690594999274 ) ) ;
#47063 = CARTESIAN_POINT ( 'NONE',  ( -0.9465222407332000154, -81.55663953507000485, -0.8164530897714000757 ) ) ;
#47064 = ORIENTED_EDGE ( 'NONE', *, *, #17899, .T. ) ;
#47065 = ORIENTED_EDGE ( 'NONE', *, *, #17520, .T. ) ;
#47066 = CARTESIAN_POINT ( 'NONE',  ( 1.370449731437000107, -80.87330263137000941, 0.3632173918321999762 ) ) ;
#47067 = ADVANCED_FACE ( 'NONE', ( #17967 ), #27097, .T. ) ;
#47068 = ORIENTED_EDGE ( 'NONE', *, *, #23705, .T. ) ;
#47069 = ORIENTED_EDGE ( 'NONE', *, *, #36109, .F. ) ;
#47070 = CARTESIAN_POINT ( 'NONE',  ( 1.798954018882000128, -18.78469026612999926, 12.61117007302000026 ) ) ;
#47071 = DIRECTION ( 'NONE',  ( 0.000000000000000000, 0.000000000000000000, 1.000000000000000000 ) ) ;
#47072 = VECTOR ( 'NONE', #25478, 1000.000000000000000 ) ;
#47073 = CARTESIAN_POINT ( 'NONE',  ( -0.9218200799623716968, -78.07291666666667140, -1.199500263597270910 ) ) ;
#47074 = CARTESIAN_POINT ( 'NONE',  ( 6.786979366286999493, -78.63646001420198672, 7.374582364394999701 ) ) ;
#47075 = CARTESIAN_POINT ( 'NONE',  ( 3.541191267721896185, -78.25630510186675792, -8.545282945131162933 ) ) ;
#47076 = CARTESIAN_POINT ( 'NONE',  ( -2.710423231297999891, -79.59273834571499151, 10.88447134676999895 ) ) ;
#47077 = ADVANCED_FACE ( 'NONE', ( #287 ), #1725, .T. ) ;
#47078 = ORIENTED_EDGE ( 'NONE', *, *, #15329, .F. ) ;
#47079 = ORIENTED_EDGE ( 'NONE', *, *, #40204, .F. ) ;
#47080 = CARTESIAN_POINT ( 'NONE',  ( -8.814863682110420484, -77.57551665829541321, 2.803737005584837849 ) ) ;
#47081 = CARTESIAN_POINT ( 'NONE',  ( -12.71106812364130789, -24.25135172969568131, 1.717582538841718520 ) ) ;
#47082 = EDGE_CURVE ( 'NONE', #45667, #15896, #47405, .T. ) ;
#47083 = CARTESIAN_POINT ( 'NONE',  ( -12.66322140213000047, -61.98161935699999958, -0.1487435796151000134 ) ) ;
#47084 = CARTESIAN_POINT ( 'NONE',  ( 0.8618009059429999619, -78.40192492588099071, -9.665816497589000633 ) ) ;
#47085 = DIRECTION ( 'NONE',  ( 0.000000000000000000, -0.7071067811866525998, -0.7071067811864425456 ) ) ;
#47086 = CARTESIAN_POINT ( 'NONE',  ( -1.092232985442824100, -79.95833333333330017, 0.6295237254636200097 ) ) ;
#47087 = CARTESIAN_POINT ( 'NONE',  ( 10.51493804038999968, -79.03332460306999963, 5.600620773984999801 ) ) ;
#47088 = CARTESIAN_POINT ( 'NONE',  ( -1.551612880221999946, -79.72318471100000181, -0.3269472641410000047 ) ) ;
#47089 = CARTESIAN_POINT ( 'NONE',  ( 2.570900958241000289, -82.21467895096598966, -3.285915534916000080 ) ) ;
#47090 = CARTESIAN_POINT ( 'NONE',  ( 1.024262641765716131, -79.56571245190475850, 1.112022483175320708 ) ) ;
#47091 = CARTESIAN_POINT ( 'NONE',  ( -9.786657985941999982, -78.95571332859898916, -1.562668305794999934 ) ) ;
#47092 = CARTESIAN_POINT ( 'NONE',  ( 10.68110037031465254, -76.83975127526852589, -1.407209699235823397 ) ) ;
#47093 = CARTESIAN_POINT ( 'NONE',  ( -10.69999999997999929, -81.80000000002199556, 2.760601855093000384E-10 ) ) ;
#47095 = CARTESIAN_POINT ( 'NONE',  ( 1.933650113856000052, -18.59213746974000259, -12.70909635754000000 ) ) ;
#47094 = DIRECTION ( 'NONE',  ( 0.000000000000000000, -1.000000000000000000, 0.000000000000000000 ) ) ;
#47097 = EDGE_CURVE ( 'NONE', #20752, #29379, #28510, .T. ) ;
#47096 = AXIS2_PLACEMENT_3D ( 'NONE', #17266, #21695, #30833 ) ;
#47098 = DIRECTION ( 'NONE',  ( 0.000000000000000000, -1.000000000000000000, 0.000000000000000000 ) ) ;
#47099 = CARTESIAN_POINT ( 'NONE',  ( -10.83098670370000072, -80.42828225638099582, 0.1115786215289999994 ) ) ;
#47100 = B_SPLINE_CURVE_WITH_KNOTS ( 'NONE', 3,
 ( #56883, #20578, #29704, #15565, #7575, #25573, #47751, #7284, #37704, #11154, #43306, #20007, #52171, #2862, #38861, #33559, #33264, #34422 ),
 .UNSPECIFIED., .F., .F.,
 ( 4, 2, 2, 2, 2, 2, 2, 2, 4 ),
 ( 0.000000000000000000, 0.1250000000000000000, 0.2500000000000000000, 0.3750000000000000000, 0.5000000000000000000, 0.6250000000000000000, 0.7500000000000000000, 0.8750000000000000000, 1.000000000000000000 ),
 .UNSPECIFIED. ) ;
#47101 = CARTESIAN_POINT ( 'NONE',  ( 12.00000000000000000, -55.54999999966999980, 1.250000000000000000 ) ) ;
#47102 = CARTESIAN_POINT ( 'NONE',  ( 10.75000000000000000, -79.75000000000000000, 0.000000000000000000 ) ) ;
#47103 = CARTESIAN_POINT ( 'NONE',  ( 3.034718321201248070, -1.045467675721396095, 1.979367435497295435 ) ) ;
#47104 = ORIENTED_EDGE ( 'NONE', *, *, #7570, .T. ) ;
#47105 = CARTESIAN_POINT ( 'NONE',  ( 0.03170276877622815043, -3.500000000000000444, -3.470587695368843040 ) ) ;
#47106 = CARTESIAN_POINT ( 'NONE',  ( -0.4635254915625000027, -82.00000000000000000, -1.426584774443000025 ) ) ;
#47107 = CARTESIAN_POINT ( 'NONE',  ( -1.980584515756000030, -23.26485150094000076, -12.76303204340999997 ) ) ;
#47108 = CARTESIAN_POINT ( 'NONE',  ( -0.0005049683876466860800, -78.47525317868688433, 1.249867733114310431 ) ) ;
#47109 = CARTESIAN_POINT ( 'NONE',  ( 6.321655259472999333, -79.77424914560899083, 7.136321001271999975 ) ) ;
#47110 = CIRCLE ( 'NONE', #15976, 10.34999999999999964 ) ;
#47111 = CARTESIAN_POINT ( 'NONE',  ( -12.96685733093999993, -76.95470625016000099, -1.095351912296000041 ) ) ;
#47112 = DIRECTION ( 'NONE',  ( 1.000000000000000000, 0.000000000000000000, 0.000000000000000000 ) ) ;
#47113 = CARTESIAN_POINT ( 'NONE',  ( 6.562466215526181479, -79.42274286776711278, 8.517979315676269536 ) ) ;
#47114 = EDGE_CURVE ( 'NONE', #22275, #53170, #47587, .T. ) ;
#47115 = AXIS2_PLACEMENT_3D ( 'NONE', #23440, #55028, #19597 ) ;
#47116 = DIRECTION ( 'NONE',  ( 0.9957542233912697327, -0.04890176544230847439, -0.07798810124034757929 ) ) ;
#47117 = EDGE_CURVE ( 'NONE', #55491, #38967, #32683, .T. ) ;
#47118 = DIRECTION ( 'NONE',  ( 0.000000000000000000, -1.000000000000000000, 0.000000000000000000 ) ) ;
#47119 = CARTESIAN_POINT ( 'NONE',  ( 9.730158407969000223, -77.59631800370499377, 5.250919032787999541 ) ) ;
#47120 = CARTESIAN_POINT ( 'NONE',  ( -1.188678760311000060, -81.30005482907799319, 0.9251722853060999618 ) ) ;
#47121 = LINE ( 'NONE', #34077, #6936 ) ;
#47122 = CARTESIAN_POINT ( 'NONE',  ( -5.190928442694000111, -77.94229427166699509, 7.852735600434000318 ) ) ;
#47124 = CARTESIAN_POINT ( 'NONE',  ( 1.980584515752000119, -18.73514853375999678, 12.76303204602000108 ) ) ;
#47123 = CARTESIAN_POINT ( 'NONE',  ( -3.193873729499000280, -84.54654301962300167, -2.346307860450000060 ) ) ;
#47125 = CARTESIAN_POINT ( 'NONE',  ( 5.645287065787000458, -79.45475194988499368, 7.708789581145000014 ) ) ;
#47126 = CYLINDRICAL_SURFACE ( 'NONE', #27045, 1.750000000000001332 ) ;
#47127 = CARTESIAN_POINT ( 'NONE',  ( 4.222689032385934738, -80.25723640890934973, -9.885936313453116853 ) ) ;
#47128 = CARTESIAN_POINT ( 'NONE',  ( -6.440114635396656517, -77.17402085401280942, -8.608282088332575910 ) ) ;
#47129 = CARTESIAN_POINT ( 'NONE',  ( -5.148784662568076406E-06, -79.56241750339395935, -9.437165819784945953 ) ) ;
#47130 = ORIENTED_EDGE ( 'NONE', *, *, #16434, .F. ) ;
#47131 = ORIENTED_EDGE ( 'NONE', *, *, #54939, .F. ) ;
#47132 = CARTESIAN_POINT ( 'NONE',  ( -8.850953919802000414, -79.62531023410498676, -8.146641040006999290 ) ) ;
#47133 = CARTESIAN_POINT ( 'NONE',  ( -8.838834764832000701, -55.54999999966999980, 8.838834764832000701 ) ) ;
#47134 = DIRECTION ( 'NONE',  ( 0.000000000000000000, 1.000000000000000000, 0.000000000000000000 ) ) ;
#47135 = ORIENTED_EDGE ( 'NONE', *, *, #6048, .T. ) ;
#47136 = CARTESIAN_POINT ( 'NONE',  ( 3.910274016995999968, -78.47184600323399195, 11.27587067850999958 ) ) ;
#47137 = ORIENTED_EDGE ( 'NONE', *, *, #51070, .T. ) ;
#47138 = ORIENTED_EDGE ( 'NONE', *, *, #39681, .T. ) ;
#47139 = VERTEX_POINT ( 'NONE', #17781 ) ;
#47140 = CARTESIAN_POINT ( 'NONE',  ( 3.499622226389000001, -80.89192428167199012, -0.5806930388547999478 ) ) ;
#47141 = CARTESIAN_POINT ( 'NONE',  ( 7.677756733616925011, -79.19981116400037990, 5.594508313773394192 ) ) ;
#47142 = EDGE_LOOP ( 'NONE', ( #29152, #52256, #3339, #26721 ) ) ;
#47143 = CARTESIAN_POINT ( 'NONE',  ( -10.45204383628000144, -56.03743350618999841, -7.651147548114000330 ) ) ;
#47144 = ORIENTED_EDGE ( 'NONE', *, *, #56179, .F. ) ;
#47145 = CARTESIAN_POINT ( 'NONE',  ( -1.151238488875999888, -3.153144585189999738, -3.200629320682000234 ) ) ;
#47147 = EDGE_LOOP ( 'NONE', ( #36138, #50503, #48342 ) ) ;
#47146 = B_SPLINE_CURVE_WITH_KNOTS ( 'NONE', 3,
 ( #29514, #21241, #7667, #25380, #42826, #2678, #34514, #47849, #6512, #16534, #24523, #15662, #52544, #47569, #2389, #57258, #38958, #25668, #51982, #6805 ),
 .UNSPECIFIED., .F., .F.,
 ( 4, 2, 2, 2, 2, 2, 2, 2, 2, 4 ),
 ( 0.000000000000000000, 0.1250000000000000555, 0.2500000000000001110, 0.3750000000000001665, 0.5000000000000002220, 0.5625000000000002220, 0.6250000000000002220, 0.7500000000000002220, 0.8750000000000001110, 1.000000000000000000 ),
 .UNSPECIFIED. ) ;
#47148 = CARTESIAN_POINT ( 'NONE',  ( 0.3445775672978685367, -79.45339798296083700, 1.202313393638915873 ) ) ;
#47149 = CARTESIAN_POINT ( 'NONE',  ( 1.051388242708131360, -77.93485489348125839, -1.116012858508012018 ) ) ;
#47150 = AXIS2_PLACEMENT_3D ( 'NONE', #26586, #39887, #53474 ) ;
#47151 = CARTESIAN_POINT ( 'NONE',  ( 10.31138940913660385, -79.80000000000002558, 5.792230958630865345 ) ) ;
#47152 = CARTESIAN_POINT ( 'NONE',  ( -8.414570695956999913, -60.64999999943950826, 8.414570695956999913 ) ) ;
#47153 = AXIS2_PLACEMENT_3D ( 'NONE', #20467, #25460, #56766 ) ;
#47154 = CARTESIAN_POINT ( 'NONE',  ( 0.4482767731681003287, -78.57812134408507632, -12.25589611745950869 ) ) ;
#47155 = CARTESIAN_POINT ( 'NONE',  ( 5.417083560472998549, -78.92212961748376188, -8.051455326762999576 ) ) ;
#47156 = CARTESIAN_POINT ( 'NONE',  ( 11.01994305158000031, -76.57026195917399036, -1.906499110313000234 ) ) ;
#47157 = CARTESIAN_POINT ( 'NONE',  ( 9.530288639337330281, -76.31250477656314501, -5.032706227462631965 ) ) ;
#47158 = CARTESIAN_POINT ( 'NONE',  ( -2.935661446561999899, -76.94999999999998863, -9.035036904803998681 ) ) ;
#47159 = CARTESIAN_POINT ( 'NONE',  ( -10.49640831179000067, -76.93768998730399744, 2.856326049988000104 ) ) ;
#47160 = CARTESIAN_POINT ( 'NONE',  ( -7.373862043355542184, -78.65167919242699668, -5.586005179260620679 ) ) ;
#47161 = CARTESIAN_POINT ( 'NONE',  ( 5.516207834483522809, -76.53601079641730109, 10.37660978597248018 ) ) ;
#47162 = CARTESIAN_POINT ( 'NONE',  ( -10.90052211673698324, -80.11089183211095133, -1.475228759022814584 ) ) ;
#47163 = CARTESIAN_POINT ( 'NONE',  ( 4.784380313523521444, -77.13333333333332575, 8.300970689365463784 ) ) ;
#47164 = CARTESIAN_POINT ( 'NONE',  ( 2.387772752419999645, -80.96292549782599224, 2.679977387145999757 ) ) ;
#47165 = CARTESIAN_POINT ( 'NONE',  ( -0.5512063501708999169, -78.95522159786899863, 12.07130450291999857 ) ) ;
#47166 = CARTESIAN_POINT ( 'NONE',  ( -8.425013773427030728, -78.04682285271482556, 6.676943546907208926 ) ) ;
#47167 = ADVANCED_FACE ( 'NONE', ( #101 ), #18076, .F. ) ;
#47168 = CARTESIAN_POINT ( 'NONE',  ( 0.7966631500014442757, -82.92057275665307259, 0.9633609681394961211 ) ) ;
#47169 = CARTESIAN_POINT ( 'NONE',  ( -12.51072239526000196, -52.49705297114005020, -0.7871079366006996647 ) ) ;
#47170 = CARTESIAN_POINT ( 'NONE',  ( -0.6295237254636286695, -80.41666666666665719, 1.092232985442819881 ) ) ;
#47171 = CARTESIAN_POINT ( 'NONE',  ( 1.250000000000000000, -78.25000000000000000, 0.000000000000000000 ) ) ;
#47172 = CARTESIAN_POINT ( 'NONE',  ( -10.13402523426999835, -60.52303809408999768, -7.647751776506999555 ) ) ;
#47173 = EDGE_CURVE ( 'NONE', #34745, #7885, #48917, .T. ) ;
#47174 = CARTESIAN_POINT ( 'NONE',  ( -0.9200108141794000050, -81.69875773523600060, -0.9654823929056000065 ) ) ;
#47175 = CIRCLE ( 'NONE', #31100, 2.500000000000000000 ) ;
#47176 = CARTESIAN_POINT ( 'NONE',  ( 12.52582254643368209, -54.99059700767242731, 1.680974932891769358 ) ) ;
#47177 = CARTESIAN_POINT ( 'NONE',  ( 12.66761950490999844, -24.22355206198999866, 1.696827901577000031 ) ) ;
#47178 = CARTESIAN_POINT ( 'NONE',  ( -9.726444407485992372, -77.91415937600359598, 4.784104274147578550 ) ) ;
#47179 = SURFACE_SIDE_STYLE ('',( #6416 ) ) ;
#47180 = CARTESIAN_POINT ( 'NONE',  ( -0.6514878906251001522, -79.72972587295357982, 10.95625855609000077 ) ) ;
#47181 = CARTESIAN_POINT ( 'NONE',  ( 0.7656296041185000067, -76.62556667361999985, 12.03752960824999896 ) ) ;
#47182 = EDGE_LOOP ( 'NONE', ( #49952, #2583, #3407, #57620 ) ) ;
#47183 = ADVANCED_FACE ( 'NONE', ( #11261 ), #48318, .F. ) ;
#47184 = CARTESIAN_POINT ( 'NONE',  ( -3.926971269994000480, -83.47246544543099844, 0.5337392329503000132 ) ) ;
#47185 = DIRECTION ( 'NONE',  ( -1.000000000000000000, 0.000000000000000000, 0.000000000000000000 ) ) ;
#47186 = CARTESIAN_POINT ( 'NONE',  ( 0.000000000000000000, -79.99999999999998579, 0.000000000000000000 ) ) ;
#47187 = CARTESIAN_POINT ( 'NONE',  ( 8.274781782443849210, -53.82110650083671288, 9.689260013493322887 ) ) ;
#47188 = CARTESIAN_POINT ( 'NONE',  ( -0.8253947190445000137, -77.52082181323800114, -11.18645762290999990 ) ) ;
#47189 = CARTESIAN_POINT ( 'NONE',  ( 12.78037507859000144, -54.50670131396999807, -1.812742845509000000 ) ) ;
#47190 = CARTESIAN_POINT ( 'NONE',  ( 3.260206397764000119, -78.17702448625199452, 9.177731198418999981 ) ) ;
#47191 = CARTESIAN_POINT ( 'NONE',  ( -1.508789225394999933, -82.35398503822999317, 0.7062677124845000431 ) ) ;
#47192 = DIRECTION ( 'NONE',  ( -1.000000000000000000, 0.000000000000000000, 0.000000000000000000 ) ) ;
#47193 = CARTESIAN_POINT ( 'NONE',  ( -1.273775855157000203, -79.09293819223900357, -0.8223283506838999779 ) ) ;
#47194 = VERTEX_POINT ( 'NONE', #11551 ) ;
#47195 = CARTESIAN_POINT ( 'NONE',  ( -3.250000000000000000, -1.000000000000000000, 1.223542571470000149E-13 ) ) ;
#47196 = VECTOR ( 'NONE', #41368, 1000.000000000000000 ) ;
#47197 = AXIS2_PLACEMENT_3D ( 'NONE', #29310, #41451, #1036 ) ;
#47198 = CARTESIAN_POINT ( 'NONE',  ( 0.8262517789086295528, -78.91601566066201201, -3.392806836647565216 ) ) ;
#47199 = EDGE_CURVE ( 'NONE', #43096, #11325, #1213, .T. ) ;
#47200 = VERTEX_POINT ( 'NONE', #56986 ) ;
#47201 = CARTESIAN_POINT ( 'NONE',  ( -1.295435361468000091, -77.69719476943419068, -0.3166359884281000348 ) ) ;
#47202 = EDGE_CURVE ( 'NONE', #42409, #35842, #32065, .T. ) ;
#47203 = DIRECTION ( 'NONE',  ( -0.7071067811865474617, -0.7071067811865474617, 9.259177001912613574E-10 ) ) ;
#47204 = CARTESIAN_POINT ( 'NONE',  ( 1.093630560900841653, -80.80912397737533581, -0.6301138695088878139 ) ) ;
#47205 = ORIENTED_EDGE ( 'NONE', *, *, #33377, .T. ) ;
#47206 = CARTESIAN_POINT ( 'NONE',  ( -11.23155942826000064, -78.22748971612699620, 4.672751159098000429 ) ) ;
#47207 = CARTESIAN_POINT ( 'NONE',  ( -8.741845958662000982, -77.56508549249599582, 7.367642417069999894 ) ) ;
#47208 = ORIENTED_EDGE ( 'NONE', *, *, #20760, .T. ) ;
#47209 = ORIENTED_EDGE ( 'NONE', *, *, #46695, .T. ) ;
#47210 = CARTESIAN_POINT ( 'NONE',  ( 0.6852450043578414141, -80.42895784771916112, 1.045337512399482582 ) ) ;
#47211 = CARTESIAN_POINT ( 'NONE',  ( 5.782158712927999211, -76.95253998579799770, 7.591266289414999591 ) ) ;
#47212 = CARTESIAN_POINT ( 'NONE',  ( 5.411006671257999834, -79.45843616023900324, 8.131518144102999557 ) ) ;
#47213 = ORIENTED_EDGE ( 'NONE', *, *, #21420, .T. ) ;
#47214 = CARTESIAN_POINT ( 'NONE',  ( -1.634907902065669383, -2.517778331623519605, 2.839622281756045030 ) ) ;
#47215 = CARTESIAN_POINT ( 'NONE',  ( -2.772348231745000113, -78.67797663195699442, -10.55885653242000011 ) ) ;
#47216 = CIRCLE ( 'NONE', #9474, 10.69999999999999929 ) ;
#47217 = ORIENTED_EDGE ( 'NONE', *, *, #22608, .F. ) ;
#47218 = CARTESIAN_POINT ( 'NONE',  ( 8.595272398064562225, -80.79796620898505921, -6.605316870660081108 ) ) ;
#47219 = CARTESIAN_POINT ( 'NONE',  ( 5.807838419657000095, -77.18721915034599590, -7.511754867730999763 ) ) ;
#47220 = CARTESIAN_POINT ( 'NONE',  ( 8.485281374238999419, -60.04999999966999980, -8.485281374238999419 ) ) ;
#47221 = CARTESIAN_POINT ( 'NONE',  ( 1.499999999999999778, -81.16041666666666288, 0.1963495408493654004 ) ) ;
#47222 = DIRECTION ( 'NONE',  ( 0.000000000000000000, 1.000000000000000000, 0.000000000000000000 ) ) ;
#47223 = B_SPLINE_CURVE_WITH_KNOTS ( 'NONE', 3,
 ( #34137, #11733, #49491, #53615, #22614, #4615, #36190, #30865, #44460, #40024 ),
 .UNSPECIFIED., .F., .F.,
 ( 4, 2, 2, 2, 4 ),
 ( 0.000000000000000000, 0.2500000000000000000, 0.5000000000000000000, 0.7500000000000000000, 1.000000000000000000 ),
 .UNSPECIFIED. ) ;
#47224 = CARTESIAN_POINT ( 'NONE',  ( -9.489900988576000174, -77.27852983129099584, -0.9230819386030000295 ) ) ;
#47225 = CARTESIAN_POINT ( 'NONE',  ( -1.119858561985657586, -78.40994284158009009, -1.052207020318775443 ) ) ;
#47226 = CARTESIAN_POINT ( 'NONE',  ( 1.439896632895333539, -79.73541666666666572, -10.99999999999999822 ) ) ;
#47227 = CARTESIAN_POINT ( 'NONE',  ( -7.760939450736999312, -24.23085356333000107, 10.15321588359000060 ) ) ;
#47228 = CARTESIAN_POINT ( 'NONE',  ( 1.407171709420440342, -77.63541666666667140, -10.74999999999999822 ) ) ;
#47229 = AXIS2_PLACEMENT_3D ( 'NONE', #9398, #24722, #37123 ) ;
#47230 = VECTOR ( 'NONE', #20440, 1000.000000000000000 ) ;
#47231 = CARTESIAN_POINT ( 'NONE',  ( 3.595196481342544548, -77.09062499990726280, -8.672428026956840341 ) ) ;
#47232 = DIRECTION ( 'NONE',  ( 0.000000000000000000, -1.000000000000000000, -9.095580416467000435E-12 ) ) ;
#47233 = CARTESIAN_POINT ( 'NONE',  ( 7.914613980750001332, -79.30035326240999893, 9.019916049260999102 ) ) ;
#47234 = CARTESIAN_POINT ( 'NONE',  ( -10.51110168222999874, -76.09063960659899806, 6.351495789100000344 ) ) ;
#47235 = DIRECTION ( 'NONE',  ( 0.000000000000000000, -1.000000000000000000, 0.000000000000000000 ) ) ;
#47236 = CARTESIAN_POINT ( 'NONE',  ( 11.19183857952876338, -77.82967953535423078, 4.379999559240030926 ) ) ;
#47237 = FACE_OUTER_BOUND ( 'NONE', #43326, .T. ) ;
#47238 = ORIENTED_EDGE ( 'NONE', *, *, #58046, .T. ) ;
#47239 = CARTESIAN_POINT ( 'NONE',  ( 1.458792785548086002, -80.02118756087138252, 0.3985484442472759792 ) ) ;
#47240 = CARTESIAN_POINT ( 'NONE',  ( 1.666698456700999920, -23.19181739840000134, 12.50018138921000066 ) ) ;
#47241 = CARTESIAN_POINT ( 'NONE',  ( 1.500000000000000888, -78.73958333333332860, -0.1963495408493590444 ) ) ;
#47242 = CARTESIAN_POINT ( 'NONE',  ( 3.533935378582000020, -2.606572672876999786, -1.142694998219000002 ) ) ;
#47243 = CARTESIAN_POINT ( 'NONE',  ( 2.713377469415999776, -77.65193793104199926, -11.74024507335000145 ) ) ;
#47244 = CARTESIAN_POINT ( 'NONE',  ( 6.263319273733999992, -78.09022787947299094, 7.458587492396000052 ) ) ;
#47246 = CARTESIAN_POINT ( 'NONE',  ( -7.412025882568599400, -77.76672174443258712, -8.233944902729593451 ) ) ;
#47245 = CARTESIAN_POINT ( 'NONE',  ( -8.399527302420572994, -76.13838338929400607, 8.217467006092146420 ) ) ;
#47247 = CARTESIAN_POINT ( 'NONE',  ( 0.4072933538588000002, -81.72938944371999526, -1.288442219433000080 ) ) ;
#47248 = CARTESIAN_POINT ( 'NONE',  ( -10.54394959781209806, -79.58451761008286951, 2.094245364761433414 ) ) ;
#47249 = ORIENTED_EDGE ( 'NONE', *, *, #38361, .T. ) ;
#47250 = EDGE_CURVE ( 'NONE', #26247, #49440, #12316, .T. ) ;
#47251 = CARTESIAN_POINT ( 'NONE',  ( -3.438348731681998949, -76.65247415041467605, -11.82003900998999946 ) ) ;
#47252 = CARTESIAN_POINT ( 'NONE',  ( 3.399999999999979927, -78.70000000000000284, -2.006589542798784986 ) ) ;
#47253 = VECTOR ( 'NONE', #807, 1000.000000000000000 ) ;
#47254 = CARTESIAN_POINT ( 'NONE',  ( 0.8506806241676515556, -2.354166666666666963, 3.165411199172028844 ) ) ;
#47255 = CARTESIAN_POINT ( 'NONE',  ( -8.541150802335000236, -61.80800189248000009, 9.205830468622998808 ) ) ;
#47256 = CARTESIAN_POINT ( 'NONE',  ( -10.96076829013453136, -80.09369723771236238, 0.9252934957875924571 ) ) ;
#47257 = CARTESIAN_POINT ( 'NONE',  ( 9.526202310737001966, -79.87930701263098854, -1.663220358726000159 ) ) ;
#47258 = DIRECTION ( 'NONE',  ( 0.000000000000000000, 0.000000000000000000, -1.000000000000000000 ) ) ;
#47259 = DIRECTION ( 'NONE',  ( 0.000000000000000000, 0.000000000000000000, -1.000000000000000000 ) ) ;
#47260 = ORIENTED_EDGE ( 'NONE', *, *, #11514, .F. ) ;
#47261 = CARTESIAN_POINT ( 'NONE',  ( 9.492027143945000134, -79.07181222620799588, 6.060972302936999512 ) ) ;
#47262 = CARTESIAN_POINT ( 'NONE',  ( 7.850076763456510953, -24.31471441247266796, -9.837736658173248827 ) ) ;
#47263 = CARTESIAN_POINT ( 'NONE',  ( 9.019638247444307311, -79.24418804902973079, -7.564637645086659923 ) ) ;
#47264 = CARTESIAN_POINT ( 'NONE',  ( 1.250000000000000000, -77.10000000000000853, -0.5000000000000000000 ) ) ;
#47265 = B_SPLINE_CURVE_WITH_KNOTS ( 'NONE', 3,
 ( #38579, #51885, #42148, #16154, #7000, #20581, #2296, #6711, #15861, #11158, #11442, #29132, #55730, #2013, #56595, #29422, #1717, #34131, #25002, #52173, #20292, #20011, #42445, #15568 ),
 .UNSPECIFIED., .F., .F.,
 ( 4, 2, 2, 2, 2, 2, 2, 2, 2, 2, 2, 4 ),
 ( 0.000000000000000000, 0.1250000000000000555, 0.2500000000000001110, 0.3750000000000001665, 0.4375000000000002220, 0.5000000000000002220, 0.6250000000000002220, 0.6875000000000003331, 0.7500000000000003331, 0.8750000000000001110, 0.9375000000000001110, 1.000000000000000000 ),
 .UNSPECIFIED. ) ;
#47267 = DIRECTION ( 'NONE',  ( 0.000000000000000000, -1.000000000000000000, 9.283980536439000051E-14 ) ) ;
#47266 = CARTESIAN_POINT ( 'NONE',  ( -1.306902306487000009, -82.16898990362500399, -0.1806716399126999939 ) ) ;
#47268 = EDGE_CURVE ( 'NONE', #51486, #11972, #25396, .T. ) ;
#47269 = CARTESIAN_POINT ( 'NONE',  ( 0.9947802209974141441, -78.95392151193854602, 0.7966053719781494014 ) ) ;
#47270 = AXIS2_PLACEMENT_3D ( 'NONE', #53288, #34102, #52143 ) ;
#47271 = CARTESIAN_POINT ( 'NONE',  ( -1.001315001699999874, -54.11477588220000001, -12.50000000000000000 ) ) ;
#47272 = CARTESIAN_POINT ( 'NONE',  ( -7.678657038172577387, -23.79377623515384954, -10.03844138475501957 ) ) ;
#47273 = CONICAL_SURFACE ( 'NONE', #11440, 1.099999997149000430, 0.7853981633972997312 ) ;
#47274 = CARTESIAN_POINT ( 'NONE',  ( 0.3106417784598000109, -79.22556961838999712, -1.176384596728999865 ) ) ;
#47275 = CARTESIAN_POINT ( 'NONE',  ( 1.980584515756000030, -23.26485150094000076, 12.76303204340999997 ) ) ;
#47276 = CARTESIAN_POINT ( 'NONE',  ( 0.000000000000000000, -87.20000000000000284, 0.000000000000000000 ) ) ;
#47277 = CARTESIAN_POINT ( 'NONE',  ( -5.726462542197000793, -79.78469283625899777, -7.912542777261000637 ) ) ;
#47278 = EDGE_LOOP ( 'NONE', ( #43371, #11184, #51919, #13988 ) ) ;
#47279 = EDGE_LOOP ( 'NONE', ( #53345, #1900, #53643, #8911 ) ) ;
#47280 = CARTESIAN_POINT ( 'NONE',  ( -11.12828319551999812, -76.36530140318998860, -5.885103109553999623 ) ) ;
#47281 = CARTESIAN_POINT ( 'NONE',  ( 4.725312280198877168, -78.76122478628501256, -9.657371511130047992 ) ) ;
#47282 = ORIENTED_EDGE ( 'NONE', *, *, #57618, .T. ) ;
#47283 = EDGE_CURVE ( 'NONE', #2251, #6738, #56128, .T. ) ;
#47284 = CARTESIAN_POINT ( 'NONE',  ( 10.30768118225000052, -18.25239703915999812, 7.634415485503000198 ) ) ;
#47285 = CARTESIAN_POINT ( 'NONE',  ( -0.8804656548849725262, -53.77196605263301166, 12.70299681147155191 ) ) ;
#47286 = CARTESIAN_POINT ( 'NONE',  ( -1.285688189784000013, -78.94796114434001311, -11.99310356001000066 ) ) ;
#47287 = CARTESIAN_POINT ( 'NONE',  ( 9.392928023032661500, -79.80834514118080847, -5.413658657368042526 ) ) ;
#47288 = DIRECTION ( 'NONE',  ( 1.000000000000000000, 0.000000000000000000, 0.000000000000000000 ) ) ;
#47289 = CARTESIAN_POINT ( 'NONE',  ( 0.7554284705563453217, -79.83333333333335702, 1.310679582531389276 ) ) ;
#47290 = CARTESIAN_POINT ( 'NONE',  ( -9.735611069857000643, -79.29253396423798961, 5.570995215215999607 ) ) ;
#47291 = VERTEX_POINT ( 'NONE', #38686 ) ;
#47292 = CARTESIAN_POINT ( 'NONE',  ( -2.899999999413999774, -80.69999999940999658, -1.301622169156000167E-09 ) ) ;
#47293 = AXIS2_PLACEMENT_3D ( 'NONE', #7239, #16968, #52982 ) ;
#47294 = ORIENTED_EDGE ( 'NONE', *, *, #52763, .T. ) ;
#47295 = CARTESIAN_POINT ( 'NONE',  ( 4.201985891154212283, -77.26254768197554768, -8.240472212907164362 ) ) ;
#47296 = DIRECTION ( 'NONE',  ( -0.7071067811865473507, -1.433669009702094715E-08, -0.7071067811865473507 ) ) ;
#47297 = DIRECTION ( 'NONE',  ( -1.000000000000000000, 0.000000000000000000, 0.000000000000000000 ) ) ;
#47298 = CARTESIAN_POINT ( 'NONE',  ( 2.187346494202816682, -78.49075902077704825, -10.82308098013309205 ) ) ;
#47299 = UNCERTAINTY_MEASURE_WITH_UNIT (LENGTH_MEASURE( 1.000000000000000082E-05 ), #5710, 'distance_accuracy_value', 'NONE');
#47300 = CARTESIAN_POINT ( 'NONE',  ( 1.240545393080999981, -78.81247058323299370, -0.6863720704128000172 ) ) ;
#47301 = CARTESIAN_POINT ( 'NONE',  ( -12.00000000000000000, -76.89999999999999147, 0.000000000000000000 ) ) ;
#47302 = DIRECTION ( 'NONE',  ( -0.7071067811865475727, 0.000000000000000000, 0.7071067811865475727 ) ) ;
#47303 = CARTESIAN_POINT ( 'NONE',  ( 0.1742577344548000007, -77.69534258052999576, 1.489843697164999980 ) ) ;
#47304 = DIRECTION ( 'NONE',  ( 1.000000000000000000, 0.000000000000000000, 0.000000000000000000 ) ) ;
#47305 = CARTESIAN_POINT ( 'NONE',  ( 6.124581921013000141, -78.66481721455799914, -9.196052954390001588 ) ) ;
#47306 = CARTESIAN_POINT ( 'NONE',  ( 3.124342397322000586, -85.34481509293298984, -1.679301754202999986 ) ) ;
#47307 = EDGE_LOOP ( 'NONE', ( #13219, #55251, #4915, #1466 ) ) ;
#47308 = CARTESIAN_POINT ( 'NONE',  ( 0.2063173652470433606, -77.19999999999998863, 10.79676918780386075 ) ) ;
#47309 = VECTOR ( 'NONE', #7906, 1000.000000000000000 ) ;
#47310 = CARTESIAN_POINT ( 'NONE',  ( 0.8701072296501000114, -80.16234740900999611, 1.463806805601000072 ) ) ;
#47311 = CARTESIAN_POINT ( 'NONE',  ( 9.837756817801476927, -61.11467795335811815, 7.850057933454666959 ) ) ;
#47312 = CARTESIAN_POINT ( 'NONE',  ( 11.53501176087999980, -78.79435273914799609, -3.234124663588000104 ) ) ;
#47313 = CARTESIAN_POINT ( 'NONE',  ( -9.516265623875000301, -17.17460635740999919, 8.227505979428000771 ) ) ;
#47314 = AXIS2_PLACEMENT_3D ( 'NONE', #39322, #42609, #39035 ) ;
#47315 = CARTESIAN_POINT ( 'NONE',  ( -0.8707220695187634085, -78.81560043429374218, -0.9317800878112861840 ) ) ;
#47316 = CARTESIAN_POINT ( 'NONE',  ( -2.617062270065174001, -1.808265572247988562, -2.353168472005194634 ) ) ;
#47317 = CARTESIAN_POINT ( 'NONE',  ( 5.279327442448000340, -79.36243918298698929, -7.780650776298999816 ) ) ;
#47318 = CARTESIAN_POINT ( 'NONE',  ( 3.187402732789999860, -77.99090022703498448, 8.972783294553000388 ) ) ;
#47319 = CARTESIAN_POINT ( 'NONE',  ( 1.929975092519000013, -55.59892743702999240, -12.72537404207999856 ) ) ;
#47320 = CARTESIAN_POINT ( 'NONE',  ( -2.271373002040000255, -77.85036594554799194, 10.79548975578000025 ) ) ;
#47321 = DIRECTION ( 'NONE',  ( -1.000000000000000000, 0.000000000000000000, 0.000000000000000000 ) ) ;
#47322 = CARTESIAN_POINT ( 'NONE',  ( 9.568449708939001042, -80.73670158748298320, -5.242933980235000568 ) ) ;
#47323 = CARTESIAN_POINT ( 'NONE',  ( -0.6127213972747047599, -80.73488747946474575, -1.116963982030347635 ) ) ;
#47324 = ORIENTED_EDGE ( 'NONE', *, *, #29568, .T. ) ;
#47325 = CARTESIAN_POINT ( 'NONE',  ( 10.98384528668755244, -18.77109020608506995, -0.5959859912293845596 ) ) ;
#47326 = ADVANCED_FACE ( 'NONE', ( #57276 ), #7110, .F. ) ;
#47327 = CARTESIAN_POINT ( 'NONE',  ( -1.629367637654999923, -60.48263643365999798, -12.46114270829000148 ) ) ;
#47328 = CARTESIAN_POINT ( 'NONE',  ( -8.180687091746479567, -55.49344856148417904, 7.353725627630893769 ) ) ;
#47329 = ADVANCED_FACE ( 'NONE', ( #38108 ), #5631, .F. ) ;
#47330 = CARTESIAN_POINT ( 'NONE',  ( 11.19180402071999936, -77.52142642169400233, 0.7494220128532999015 ) ) ;
#47331 = CARTESIAN_POINT ( 'NONE',  ( 0.1291013223160000223, -79.24391248043099267, 10.97485077029999978 ) ) ;
#47332 = DIRECTION ( 'NONE',  ( -1.000000000000000000, 0.000000000000000000, 0.000000000000000000 ) ) ;
#47333 = CARTESIAN_POINT ( 'NONE',  ( 3.991454038972588325, -85.42552084570225190, -0.4111825025862656524 ) ) ;
#47334 = CARTESIAN_POINT ( 'NONE',  ( -9.998727717549755312, -60.72738947565338208, 7.709134076929469614 ) ) ;
#47335 = CARTESIAN_POINT ( 'NONE',  ( 9.758259394072377191, -78.49507498617447254, 6.543158735238040258 ) ) ;
#47336 = CARTESIAN_POINT ( 'NONE',  ( -8.803747447685278615, -62.01568152305762283, 9.164340453807367837 ) ) ;
#47337 = ORIENTED_EDGE ( 'NONE', *, *, #9866, .T. ) ;
#47338 = CARTESIAN_POINT ( 'NONE',  ( -1.113964114829858021, -80.06227650713580601, 0.5734498748148272318 ) ) ;
#47339 = CARTESIAN_POINT ( 'NONE',  ( 11.00000000000000000, -77.94999999999998863, 0.000000000000000000 ) ) ;
#47340 = ADVANCED_FACE ( 'NONE', ( #25481 ), #43505, .F. ) ;
#47341 = COLOUR_RGB ( '', 0.40784314, 0.44705882, 0.49803922) ;
#47342 = CARTESIAN_POINT ( 'NONE',  ( -10.93895610016999953, -78.65995737143398969, 2.695955081989000135 ) ) ;
#47343 = DIRECTION ( 'NONE',  ( 0.000000000000000000, -1.000000000000000000, 0.000000000000000000 ) ) ;
#47344 = CARTESIAN_POINT ( 'NONE',  ( 0.000000000000000000, -80.79999999999999716, 0.000000000000000000 ) ) ;
#47345 = DIRECTION ( 'NONE',  ( -0.7071067811865475727, 0.000000000000000000, -0.7071067811865475727 ) ) ;
#47346 = CARTESIAN_POINT ( 'NONE',  ( -1.064943818649878970, -81.91207579107143033, -1.072564683137462893 ) ) ;
#47347 = FACE_OUTER_BOUND ( 'NONE', #38999, .T. ) ;
#47348 = CARTESIAN_POINT ( 'NONE',  ( -9.689263856727277968, -53.82111184930475645, 8.274777958929785626 ) ) ;
#47349 = ORIENTED_EDGE ( 'NONE', *, *, #1215, .F. ) ;
#47350 = CARTESIAN_POINT ( 'NONE',  ( 1.667917367065999912, -23.28056535155999995, 12.49306764015999960 ) ) ;
#47351 = CARTESIAN_POINT ( 'NONE',  ( 11.00000000000000000, -79.34999999999999432, -1.064824513673000067E-14 ) ) ;
#47352 = ORIENTED_EDGE ( 'NONE', *, *, #57496, .F. ) ;
#47353 = ORIENTED_EDGE ( 'NONE', *, *, #29073, .T. ) ;
#47354 = CARTESIAN_POINT ( 'NONE',  ( -12.54902617714999913, -53.79030198112999273, -0.4617931494615999943 ) ) ;
#47355 = AXIS2_PLACEMENT_3D ( 'NONE', #28745, #46796, #41757 ) ;
#47356 = VERTEX_POINT ( 'NONE', #43501 ) ;
#47357 = CARTESIAN_POINT ( 'NONE',  ( -0.05512383893429553122, -79.87451577342567077, -9.559639413446380019 ) ) ;
#47358 = ORIENTED_EDGE ( 'NONE', *, *, #41341, .F. ) ;
#47359 = CONICAL_SURFACE ( 'NONE', #52980, 1.099999997148999986, 0.7853981633972997312 ) ;
#47360 = CARTESIAN_POINT ( 'NONE',  ( -0.4356486348717999446, -17.11935044189999999, 12.43591427121000237 ) ) ;
#47361 = CARTESIAN_POINT ( 'NONE',  ( 2.778581917922999800, -77.92792964775300391, 10.55721783972000161 ) ) ;
#47362 = LINE ( 'NONE', #29313, #1381 ) ;
#47363 = CARTESIAN_POINT ( 'NONE',  ( -9.832476300866000329, -78.74688667140098630, 1.242130619674999936 ) ) ;
#47364 = CARTESIAN_POINT ( 'NONE',  ( 0.6905870083389051839, -78.23098341495615671, -9.225493071672193679 ) ) ;
#47365 = CARTESIAN_POINT ( 'NONE',  ( 1.999999999936000084, -76.30000000006400285, -2.601307164620000538E-10 ) ) ;
#47366 = EDGE_LOOP ( 'NONE', ( #10761, #21260, #6768, #50799 ) ) ;
#47367 = VERTEX_POINT ( 'NONE', #3061 ) ;
#47368 = DIRECTION ( 'NONE',  ( -1.000000000000000000, 0.000000000000000000, 0.000000000000000000 ) ) ;
#47369 = LINE ( 'NONE', #33753, #30992 ) ;
#47370 = ADVANCED_FACE ( 'NONE', ( #48235 ), #23123, .F. ) ;
#47371 = CARTESIAN_POINT ( 'NONE',  ( -12.66761950495000022, -61.02355206165999846, -1.696827901577000031 ) ) ;
#47372 = CARTESIAN_POINT ( 'NONE',  ( -1.565122400816999937, -78.71804231371298499, 9.577113408380000692 ) ) ;
#47373 = CARTESIAN_POINT ( 'NONE',  ( 7.613962827178999859, -18.69360374348000065, 10.53101998747000145 ) ) ;
#47374 = PLANE ( 'NONE',  #8677 ) ;
#47375 = DIRECTION ( 'NONE',  ( 1.000000000000000000, 0.000000000000000000, 0.000000000000000000 ) ) ;
#47376 = CARTESIAN_POINT ( 'NONE',  ( -1.649952397703835283, -77.41404686049249051, -11.92900123064598183 ) ) ;
#47377 = CARTESIAN_POINT ( 'NONE',  ( 0.6690176526880000640, -81.11284491707999678, 1.565960205386000004 ) ) ;
#47378 = DIRECTION ( 'NONE',  ( 0.000000000000000000, -1.000000000000000000, 0.000000000000000000 ) ) ;
#47379 = DIRECTION ( 'NONE',  ( 0.000000000000000000, -1.000000000000000000, 0.000000000000000000 ) ) ;
#47380 = CARTESIAN_POINT ( 'NONE',  ( -10.36289663187000087, -55.59893657650000165, 7.633501051906999457 ) ) ;
#47381 = CARTESIAN_POINT ( 'NONE',  ( 2.052412689622999942, -78.08471332859899405, -9.695776403646000574 ) ) ;
#47382 = CARTESIAN_POINT ( 'NONE',  ( -8.111819378804783653, -80.34583333334180111, -7.301249762614178351 ) ) ;
#47383 = CARTESIAN_POINT ( 'NONE',  ( 1.931043762602999925, -22.77819125662999866, -12.75761570867000039 ) ) ;
#47385 = CARTESIAN_POINT ( 'NONE',  ( 2.065550207748000133, -18.57434920668999823, -12.82162303854000029 ) ) ;
#47384 = DIRECTION ( 'NONE',  ( 0.000000000000000000, -1.000000000000000000, 0.000000000000000000 ) ) ;
#47386 = CARTESIAN_POINT ( 'NONE',  ( -2.000078442263883094, -1.174552220937325364, -2.601275589776585573 ) ) ;
#47387 = CARTESIAN_POINT ( 'NONE',  ( -10.61587359353999993, -80.44003597815999740, -1.456403148199000075 ) ) ;
#47388 = CARTESIAN_POINT ( 'NONE',  ( 1.001315002179999913, -17.31477588286000113, 12.50000000000000000 ) ) ;
#47389 = CARTESIAN_POINT ( 'NONE',  ( 0.000000000000000000, -80.79999999999999716, 0.000000000000000000 ) ) ;
#47390 = CARTESIAN_POINT ( 'NONE',  ( 0.7085295082841903680, -1.108782177693018456, 3.546401372608706914 ) ) ;
#47391 = ORIENTED_EDGE ( 'NONE', *, *, #24918, .F. ) ;
#47392 = LINE ( 'NONE', #42948, #7497 ) ;
#47393 = DIRECTION ( 'NONE',  ( 0.000000000000000000, 0.000000000000000000, 1.000000000000000000 ) ) ;
#47394 = CARTESIAN_POINT ( 'NONE',  ( -1.798944584246999989, -55.58466771687000119, 12.61116915997000021 ) ) ;
#47395 = CARTESIAN_POINT ( 'NONE',  ( 1.250000000000000000, -78.35000000000000853, 0.000000000000000000 ) ) ;
#47396 = EDGE_CURVE ( 'NONE', #12674, #31055, #18707, .T. ) ;
#47397 = CARTESIAN_POINT ( 'NONE',  ( -9.280666835437999751, -79.91493201263098456, -2.616774452598999989 ) ) ;
#47398 = CIRCLE ( 'NONE', #37965, 3.000000000000000000 ) ;
#47399 = CARTESIAN_POINT ( 'NONE',  ( -12.46164872704999915, -55.12834420008999814, 1.631615798669999950 ) ) ;
#47400 = CARTESIAN_POINT ( 'NONE',  ( 3.031642507359964878, -79.19956947028450145, 9.231160939620027150 ) ) ;
#47401 = CARTESIAN_POINT ( 'NONE',  ( 2.015551294784000191, -60.60347704811000824, 12.79857978897999971 ) ) ;
#47402 = CARTESIAN_POINT ( 'NONE',  ( 3.250000000000000444, -3.239583333333332593, -0.4254240051736113415 ) ) ;
#47403 = CARTESIAN_POINT ( 'NONE',  ( 11.00000000000000711, -77.43958333333331723, -1.439896632895300010 ) ) ;
#47404 = CARTESIAN_POINT ( 'NONE',  ( 0.000000000000000000, -75.15999999999999659, 0.000000000000000000 ) ) ;
#47405 = CIRCLE ( 'NONE', #53954, 9.549999999999998934 ) ;
#47406 = CARTESIAN_POINT ( 'NONE',  ( -10.84896630757000047, -77.86011170514498758, 1.467873659019000021 ) ) ;
#47407 = EDGE_CURVE ( 'NONE', #31775, #30023, #33435, .T. ) ;
#47408 = CARTESIAN_POINT ( 'NONE',  ( -0.02218730529862296408, -76.32463168808217802, -11.74982668617501602 ) ) ;
#47409 = CARTESIAN_POINT ( 'NONE',  ( 0.5383385070467999745, -76.77002127708399826, -11.01870799087000030 ) ) ;
#47410 = CARTESIAN_POINT ( 'NONE',  ( -1.823750004803999641E-14, -80.79999999999999716, 0.000000000000000000 ) ) ;
#47411 = EDGE_CURVE ( 'NONE', #53718, #308, #15883, .T. ) ;
#47412 = CARTESIAN_POINT ( 'NONE',  ( 5.491552160713999875, -77.09679918850338254, 7.961786551375001686 ) ) ;
#47413 = CARTESIAN_POINT ( 'NONE',  ( 2.421167930323344653, -78.35416666666665719, 9.009247259181915268 ) ) ;
#47414 = CARTESIAN_POINT ( 'NONE',  ( 1.636761686205427058, -2.666666666666666519, -2.839805762151336399 ) ) ;
#47415 = CARTESIAN_POINT ( 'NONE',  ( 6.980956135117539318, -80.28139258642764275, -8.175132495031112612 ) ) ;
#47416 = CARTESIAN_POINT ( 'NONE',  ( -12.56594317823000040, -18.74999998606000062, -1.750000000000000000 ) ) ;
#47417 = CARTESIAN_POINT ( 'NONE',  ( 0.000000000000000000, -75.09999999979599750, 0.000000000000000000 ) ) ;
#47418 = CARTESIAN_POINT ( 'NONE',  ( -0.7406579117306999471, -79.44600844901900416, 12.00660533699000077 ) ) ;
#47419 = CARTESIAN_POINT ( 'NONE',  ( 1.001315002657000131, -61.48522411647999775, -12.50000000000000000 ) ) ;
#47420 = CARTESIAN_POINT ( 'NONE',  ( 0.000000000000000000, -76.39999999999899671, 0.000000000000000000 ) ) ;
#47421 = B_SPLINE_CURVE_WITH_KNOTS ( 'NONE', 3,
 ( #45236, #99, #3128, #17779, #4783, #25545, #9211, #26908, #7833, #56850, #13331, #25834, #36068, #22194, #31325, #40793, #8918, #44938 ),
 .UNSPECIFIED., .F., .F.,
 ( 4, 2, 2, 2, 2, 2, 2, 2, 4 ),
 ( 0.000000000000000000, 0.06250000000000004163, 0.1250000000000000833, 0.2499999999999991118, 0.4999999999999977796, 0.7499999999999963363, 0.8124999999999972244, 0.8749999999999980016, 1.000000000000000000 ),
 .UNSPECIFIED. ) ;
#47422 = ORIENTED_EDGE ( 'NONE', *, *, #22102, .T. ) ;
#47423 = CARTESIAN_POINT ( 'NONE',  ( 0.5135400119441678735, -25.17868533861081914, 12.70453250098436904 ) ) ;
#47424 = ORIENTED_EDGE ( 'NONE', *, *, #28852, .T. ) ;
#47425 = ORIENTED_EDGE ( 'NONE', *, *, #31348, .F. ) ;
#47426 = CARTESIAN_POINT ( 'NONE',  ( 3.000000000000000000, -86.20000000000000284, 0.000000000000000000 ) ) ;
#47427 = EDGE_CURVE ( 'NONE', #43451, #53718, #31329, .T. ) ;
#47428 =( NAMED_UNIT ( * ) SI_UNIT ( $, .STERADIAN. ) SOLID_ANGLE_UNIT ( ) );
#47429 = CARTESIAN_POINT ( 'NONE',  ( -11.75000000000000000, -77.29999999999999716, 0.000000000000000000 ) ) ;
#47430 = CARTESIAN_POINT ( 'NONE',  ( 0.5658688935430999933, -82.10069402096399926, -3.501615713813999609 ) ) ;
#47431 = CARTESIAN_POINT ( 'NONE',  ( 6.174209039929378307, -79.21856170414847043, 7.219943151181964502 ) ) ;
#47432 = VERTEX_POINT ( 'NONE', #41974 ) ;
#47433 = CARTESIAN_POINT ( 'NONE',  ( 0.7382888704586531015, -82.77565560264896760, -1.008472483837859368 ) ) ;
#47434 = VERTEX_POINT ( 'NONE', #28377 ) ;
#47435 = CARTESIAN_POINT ( 'NONE',  ( -1.574774750116000099, -2.142316864579000057, -3.014985959147999939 ) ) ;
#47436 = ORIENTED_EDGE ( 'NONE', *, *, #27416, .T. ) ;
#47437 = CARTESIAN_POINT ( 'NONE',  ( 9.050966799188000067, -55.64999999964999233, 7.919595949288999570 ) ) ;
#47438 = CARTESIAN_POINT ( 'NONE',  ( 1.470702262612896716, -78.52302955446236865, 0.4327831235184762537 ) ) ;
#47439 = AXIS2_PLACEMENT_3D ( 'NONE', #36605, #5890, #23899 ) ;
#47440 = CARTESIAN_POINT ( 'NONE',  ( -10.04068294437870890, -79.80000000000001137, -6.437684011260381922 ) ) ;
#47441 = B_SPLINE_SURFACE_WITH_KNOTS ( 'NONE', 3, 3, ( 
 ( #57668, #39948, #21655, #48824, #8366, #17224, #53243, #16663, #21082, #16947, #52961, #12510, #39662, #12792, #26364, #431, #41420, #44980, #18117, #49414, #50002, #718, #31959, #50581, #54705, #36980, #4827, #41710, #18407, #22826, #14249, #4535, #9548, #32535, #36399, #10135, #54127, #28111, #31664, #23117, #22536, #8962, #1285, #9255, #46162, #27822, #27531, #1003, #18988, #14542, #27240, #40837, #54427, #5687, #50288, #18696, #31369, #23697, #54993, #45573, #36690, #19279, #37269, #36111, #13373, #26947, #32245 ),
 ( #5121, #40545, #41124, #140, #13668, #49710, #45278, #13962, #45868, #9842, #5401, #23409, #38440, #55580, #42885, #34000, #1870, #56169, #56457, #24579, #42303, #43176, #15717, #2731, #52036, #7148, #33713, #51750, #11593, #11300, #51168, #29281, #23987, #33423, #20730, #47330, #25150, #2157, #6270, #28700, #46452, #6859, #1571, #29569, #55284, #24286, #47625, #5980, #19864, #19564, #51460, #24867, #42003, #37858, #42595, #2442, #11014, #20444, #16011, #20158, #38147, #37565, #14832, #32829, #50874, #15128, #10420 ),
 ( #33126, #28405, #46751, #10722, #55879, #15429, #28998, #47038, #6568, #26577, #39307, #43459, #34288, #39594, #13005, #11876, #12158, #39019, #53463, #44611, #57031, #35434, #38728, #4166, #44314, #52322, #57317, #30718, #29854, #16881, #16590, #34862, #8300, #9404, #26802, #40094, #40397, #54852, #49565, #8810, #9111, #30928, #45729, #32111, #48967, #40989, #9694, #35961, #49258, #18561, #36553, #58406, #13226, #8509, #45135, #54575, #289, #50152, #4083, #58108, #17671, #22386, #4970, #35657, #53687, #13820, #31220 ),
 ( #53985, #49861, #4387, #18268, #17969, #27395, #15282, #2304, #51610, #24728, #51317, #10875, #29142, #28846, #10278, #46897, #41569, #51026, #20301, #33276, #42741, #19720, #23844, #46313, #5543, #6424, #19135, #11167, #38296, #41861, #6720, #23553, #1438, #37130, #10575, #24439, #1150, #19429, #14687, #14399, #47188, #1727, #32397, #37421, #55441, #50441, #42453, #37716, #9993, #33572, #2021, #32980, #55738, #27972, #20019, #55141, #38002, #56028, #15577, #46022, #28558, #32688, #50738, #28259, #5838, #14982, #46606 ) ),
 .UNSPECIFIED., .F., .F., .F.,
 ( 4, 4 ),
 ( 4, 1, 1, 1, 1, 1, 1, 1, 1, 1, 1, 1, 1, 1, 1, 1, 1, 1, 1, 1, 1, 1, 1, 1, 1, 1, 1, 1, 1, 1, 1, 1, 1, 1, 1, 1, 1, 1, 1, 1, 1, 1, 1, 1, 1, 1, 1, 1, 1, 1, 1, 1, 1, 1, 1, 1, 1, 1, 1, 1, 1, 1, 1, 1, 4 ),
 ( -0.5168282991433000850, 1.516828299142999992 ),
 ( -0.02000000000000000042, -0.003749999999999999861, 0.01250000000000000069, 0.02875000000000000125, 0.04499999999999999833, 0.06124999999999999889, 0.07749999999999999944, 0.09375000000000000000, 0.1100000000000000006, 0.1262500000000000011, 0.1424999999999999878, 0.1587500000000000022, 0.1749999999999999889, 0.1912500000000000033, 0.2074999999999999900, 0.2237500000000000044, 0.2399999999999999911, 0.2562499999999999778, 0.2725000000000000200, 0.2887500000000000067, 0.3049999999999999933, 0.3212499999999999800, 0.3375000000000000222, 0.3537500000000000089, 0.3699999999999999956, 0.3862499999999999822, 0.4025000000000000244, 0.4187500000000000111, 0.4349999999999999978, 0.4512499999999999845, 0.4675000000000000266, 0.4837500000000000133, 0.5000000000000000000, 0.5162499999999999867, 0.5324999999999999734, 0.5487499999999999600, 0.5649999999999999467, 0.5812500000000000444, 0.5975000000000000311, 0.6137500000000000178, 0.6300000000000000044, 0.6462499999999999911, 0.6624999999999999778, 0.6787499999999999645, 0.6949999999999999512, 0.7112500000000000488, 0.7275000000000000355, 0.7437500000000000222, 0.7600000000000000089, 0.7762499999999999956, 0.7924999999999999822, 0.8087499999999999689, 0.8249999999999999556, 0.8412500000000000533, 0.8575000000000000400, 0.8737500000000000266, 0.8900000000000000133, 0.9062500000000000000, 0.9224999999999999867, 0.9387499999999999734, 0.9549999999999999600, 0.9712499999999999467, 0.9875000000000000444, 1.003749999999999920, 1.020000000000000018 ),
 .UNSPECIFIED. ) ;
#47442 = ADVANCED_FACE ( 'NONE', ( #50844 ), #50262, .F. ) ;
#47443 = CARTESIAN_POINT ( 'NONE',  ( -10.09223574029775783, -80.07210543507824241, 3.703295250976208486 ) ) ;
#47444 = CARTESIAN_POINT ( 'NONE',  ( 11.03923301813926727, -78.66434349831403949, -5.342590761205005201 ) ) ;
#47445 = CARTESIAN_POINT ( 'NONE',  ( 2.389814808304494775, -86.36264282632902223, -3.356337498275545173 ) ) ;
#47446 = CARTESIAN_POINT ( 'NONE',  ( 1.849737152796000039, -76.76346022239599165, 11.02961253862999946 ) ) ;
#47447 = CARTESIAN_POINT ( 'NONE',  ( 10.13752626742690666, -76.38035237456122672, 3.893437952651892076 ) ) ;
#47448 = EDGE_CURVE ( 'NONE', #16901, #19957, #32220, .T. ) ;
#47449 = B_SPLINE_CURVE_WITH_KNOTS ( 'NONE', 3,
 ( #40476, #31301, #49344, #12730, #4756, #54065, #9185, #8890, #53771, #44909, #58189, #18341, #31010, #21593, #8305, #27171, #13896, #31890 ),
 .UNSPECIFIED., .F., .F.,
 ( 4, 2, 2, 2, 2, 2, 2, 2, 4 ),
 ( 0.000000000000000000, 0.1250000000000000278, 0.2500000000000000555, 0.3750000000000001110, 0.5000000000000001110, 0.6250000000000001110, 0.7500000000000002220, 0.8750000000000001110, 1.000000000000000000 ),
 .UNSPECIFIED. ) ;
#47450 = CARTESIAN_POINT ( 'NONE',  ( 0.000000000000000000, -74.70999999999999375, 0.000000000000000000 ) ) ;
#47451 = CONICAL_SURFACE ( 'NONE', #18186, 4.199999999630000147, 0.7853981633972997312 ) ;
#47452 = CARTESIAN_POINT ( 'NONE',  ( 5.145480625322999657, -76.72783191828600025, 9.851073647752999207 ) ) ;
#47453 = CARTESIAN_POINT ( 'NONE',  ( -5.007122319500682650, -78.67959078829761665, -7.777765833668380147 ) ) ;
#47454 = CARTESIAN_POINT ( 'NONE',  ( 0.2020314717676000016, -80.31521474169700525, -1.318241039644999946 ) ) ;
#47455 = DIRECTION ( 'NONE',  ( -0.7071067811865474617, 3.445410891336226740E-11, -0.7071067811865474617 ) ) ;
#47456 = CARTESIAN_POINT ( 'NONE',  ( -3.055408317354031844, -3.073761893863659722, 1.105607771687054264 ) ) ;
#47457 = B_SPLINE_CURVE_WITH_KNOTS ( 'NONE', 3,
 ( #40267, #5419, #23428, #19006, #58279, #17843, #13392, #40567 ),
 .UNSPECIFIED., .F., .F.,
 ( 4, 2, 2, 4 ),
 ( 0.000000000000000000, 0.5000000000000000000, 0.7500000000000000000, 1.000000000000000000 ),
 .UNSPECIFIED. ) ;
#47458 = CARTESIAN_POINT ( 'NONE',  ( 3.540989726729000253, -80.72242549782599497, -0.5874770353539999768 ) ) ;
#47459 = CARTESIAN_POINT ( 'NONE',  ( 6.473318383219999639, -79.33935673447399495, 10.34143508852999815 ) ) ;
#47460 = CIRCLE ( 'NONE', #24801, 0.5999999999999999778 ) ;
#47461 = CARTESIAN_POINT ( 'NONE',  ( -10.74994593004994137, -78.09660187553588173, 0.4712215136974609586 ) ) ;
#47462 = CARTESIAN_POINT ( 'NONE',  ( 0.4094730476285221021, -82.94845345813016024, 1.181202292546965182 ) ) ;
#47463 = CARTESIAN_POINT ( 'NONE',  ( -7.714303428875997959, -63.10294702886003648, 12.53545825868000385 ) ) ;
#47464 = CARTESIAN_POINT ( 'NONE',  ( -2.265198070799999908, -84.54699735065199206, 2.726507195704999997 ) ) ;
#47465 = CARTESIAN_POINT ( 'NONE',  ( -11.75000000000000000, -76.20000000000000284, -1.391479524197000231E-14 ) ) ;
#47466 = CARTESIAN_POINT ( 'NONE',  ( -1.181111693982000110, -79.27654225787900089, -0.4092372983238000139 ) ) ;
#47467 = CIRCLE ( 'NONE', #36132, 12.05000000000000071 ) ;
#47468 = CARTESIAN_POINT ( 'NONE',  ( 6.606377239730315765, -80.17708333333334281, -8.596418555780452664 ) ) ;
#47469 = CARTESIAN_POINT ( 'NONE',  ( -3.882040082920266588, -79.20112713863417753, 11.40455788431460249 ) ) ;
#47470 = CARTESIAN_POINT ( 'NONE',  ( 1.246077061130999919, -80.85534313775698934, -0.4752592857455000264 ) ) ;
#47471 = PLANE ( 'NONE',  #105 ) ;
#47472 = CARTESIAN_POINT ( 'NONE',  ( 12.51033564907000084, -78.27980835132001403, -3.582046052171000028 ) ) ;
#47473 = CARTESIAN_POINT ( 'NONE',  ( -10.67274964942681414, -77.93965057761698745, 1.462407073126524848 ) ) ;
#47474 = CARTESIAN_POINT ( 'NONE',  ( 9.837756816588985487, -24.31467795598597093, 7.850057934554545369 ) ) ;
#47475 = DIRECTION ( 'NONE',  ( 0.000000000000000000, -1.000000000000000000, 0.000000000000000000 ) ) ;
#47476 = CARTESIAN_POINT ( 'NONE',  ( -12.02449095972999871, -76.68250438773999633, -2.131941081079999911 ) ) ;
#47477 = ORIENTED_EDGE ( 'NONE', *, *, #47821, .F. ) ;
#47478 = CARTESIAN_POINT ( 'NONE',  ( 5.620590082324000036, -80.41656716774588176, -9.763102121971000358 ) ) ;
#47479 = CARTESIAN_POINT ( 'NONE',  ( 3.654181830570000233, -86.09999999999999432, -1.626946572303000105 ) ) ;
#47480 = CARTESIAN_POINT ( 'NONE',  ( 12.43647262256999930, -61.71807034702999317, -0.03492325570155000586 ) ) ;
#47481 = CARTESIAN_POINT ( 'NONE',  ( -9.821634722185001110, -78.80854920034998656, -7.703425204176999941 ) ) ;
#47482 = CARTESIAN_POINT ( 'NONE',  ( 0.000000000000000000, -76.00000000000000000, 0.000000000000000000 ) ) ;
#47483 = CARTESIAN_POINT ( 'NONE',  ( 8.393017115181999444, -79.24276232907497786, 4.056188317180000169 ) ) ;
#47484 = CIRCLE ( 'NONE', #19179, 12.90000000000000036 ) ;
#47485 = CARTESIAN_POINT ( 'NONE',  ( -1.561527218546999940, -82.41714425333900351, -0.5804237711334999661 ) ) ;
#47486 = CARTESIAN_POINT ( 'NONE',  ( 0.6999999999999999556, -21.00000000000000000, 11.90000000000000036 ) ) ;
#47487 = FACE_OUTER_BOUND ( 'NONE', #19307, .T. ) ;
#47488 = ORIENTED_EDGE ( 'NONE', *, *, #12887, .T. ) ;
#47489 = CARTESIAN_POINT ( 'NONE',  ( 0.000000000000000000, -3.500000000000000000, 0.000000000000000000 ) ) ;
#47490 = CARTESIAN_POINT ( 'NONE',  ( 0.7962146461373009743, -78.91497093336721491, -3.398928107770800455 ) ) ;
#47491 = EDGE_LOOP ( 'NONE', ( #9985, #19259, #50311 ) ) ;
#47492 = AXIS2_PLACEMENT_3D ( 'NONE', #19108, #50411, #14369 ) ;
#47493 = CARTESIAN_POINT ( 'NONE',  ( 9.250000000000003553, -77.73965344036420788, -1.202673002443502170 ) ) ;
#47494 = DIRECTION ( 'NONE',  ( -0.9957542233912675123, -0.04890176544233841571, 0.07798810124035751579 ) ) ;
#47495 = ORIENTED_EDGE ( 'NONE', *, *, #10797, .F. ) ;
#47496 = CARTESIAN_POINT ( 'NONE',  ( -7.347140770713999736, -77.75263047206500744, 9.839476697348001011 ) ) ;
#47497 = CARTESIAN_POINT ( 'NONE',  ( 10.83522510763000035, -77.34497724050399370, -3.646917633351999921 ) ) ;
#47498 = VERTEX_POINT ( 'NONE', #24258 ) ;
#47499 = ORIENTED_EDGE ( 'NONE', *, *, #17943, .F. ) ;
#47500 = ORIENTED_EDGE ( 'NONE', *, *, #14163, .F. ) ;
#47501 = EDGE_CURVE ( 'NONE', #8280, #891, #22848, .T. ) ;
#47502 = CARTESIAN_POINT ( 'NONE',  ( -0.8989222131784045944, -80.53948156304845440, 0.8681004554801105000 ) ) ;
#47503 = AXIS2_PLACEMENT_3D ( 'NONE', #39100, #25809, #35223 ) ;
#47504 = ADVANCED_FACE ( 'NONE', ( #1545 ), #37002, .F. ) ;
#47505 = CARTESIAN_POINT ( 'NONE',  ( 5.414045489727194571, -77.76670134806883539, -9.393387330184902240 ) ) ;
#47506 = CARTESIAN_POINT ( 'NONE',  ( 5.411006671257999834, -79.33858331678850107, 8.131518144102999557 ) ) ;
#47507 = ORIENTED_EDGE ( 'NONE', *, *, #53293, .F. ) ;
#47508 = CARTESIAN_POINT ( 'NONE',  ( -12.76303204522000101, -23.26485147686999966, -1.980584515753000208 ) ) ;
#47509 = CARTESIAN_POINT ( 'NONE',  ( 2.120986319506000140, -78.43284954493999805, 10.70872462160000005 ) ) ;
#47510 = ORIENTED_EDGE ( 'NONE', *, *, #25068, .T. ) ;
#47511 = CARTESIAN_POINT ( 'NONE',  ( 4.750030159171999777, -78.70665068745630322, -11.30647155123999958 ) ) ;
#47512 = DIRECTION ( 'NONE',  ( 0.000000000000000000, -1.000000000000000000, 0.000000000000000000 ) ) ;
#47513 = CARTESIAN_POINT ( 'NONE',  ( 9.650965486062000664, -53.86598967493999623, 8.252456811976999873 ) ) ;
#47514 = CARTESIAN_POINT ( 'NONE',  ( -7.247844507162001015, -60.04999999966999980, 9.722718241315000398 ) ) ;
#47515 = CARTESIAN_POINT ( 'NONE',  ( 0.7554284705563452107, -78.23333333333330586, 1.310679582531388609 ) ) ;
#47516 = FACE_OUTER_BOUND ( 'NONE', #32516, .T. ) ;
#47517 = EDGE_CURVE ( 'NONE', #31168, #10827, #30367, .T. ) ;
#47518 = CARTESIAN_POINT ( 'NONE',  ( -5.374516262939114775, -80.26463862341171307, 9.838658862348587775 ) ) ;
#47519 = CARTESIAN_POINT ( 'NONE',  ( 0.4630162960789051541, -77.99946388533825825, -1.437486996108025217 ) ) ;
#47520 = CARTESIAN_POINT ( 'NONE',  ( 3.696996952934347824, -81.05104167182884112, 1.659147455894784295 ) ) ;
#47521 = CARTESIAN_POINT ( 'NONE',  ( -7.450482419345999752, -76.02126934844999084, -9.799277032148999922 ) ) ;
#47522 = CARTESIAN_POINT ( 'NONE',  ( 1.620786422037999941, -80.68907046129099569, -3.844424077763000103 ) ) ;
#47523 = CARTESIAN_POINT ( 'NONE',  ( 7.396918292183153554, -77.80208333333332860, 5.684557159767984480 ) ) ;
#47524 = CARTESIAN_POINT ( 'NONE',  ( 9.966224254750001066, -60.46904904752999954, -7.657729124028000101 ) ) ;
#47525 = CARTESIAN_POINT ( 'NONE',  ( -9.042566447131001439, -79.04168679971999723, -8.284387575507999202 ) ) ;
#47526 = DIRECTION ( 'NONE',  ( 1.000000000000000000, 0.000000000000000000, 0.000000000000000000 ) ) ;
#47527 = CARTESIAN_POINT ( 'NONE',  ( 0.000000000000000000, -80.39687500001899423, 0.000000000000000000 ) ) ;
#47528 = CARTESIAN_POINT ( 'NONE',  ( 7.383247350150824673, -77.72738732844908327, -9.556516804512405372 ) ) ;
#47529 = CARTESIAN_POINT ( 'NONE',  ( -0.3271848554490991434, -78.60416666666665719, -1.217465845835395299 ) ) ;
#47530 = AXIS2_PLACEMENT_3D ( 'NONE', #15742, #53488, #26322 ) ;
#47531 = ADVANCED_FACE ( 'NONE', ( #2705 ), #12415, .F. ) ;
#47532 = B_SPLINE_SURFACE_WITH_KNOTS ( 'NONE', 3, 3, ( 
 ( #44736, #31424, #4287, #57717, #22287, #13423, #17874, #35864, #53893, #49467, #9014, #27000, #35265, #45035, #4586, #25844, #3421, #195, #34977, #18170, #39429, #33173, #50051, #45626, #45330, #42054, #9597, #1335, #50339, #5739, #46505, #55629, #19330, #1625, #55338 ),
 ( #18457, #37322, #4880, #9890, #19616, #28457, #9304, #46212, #5167, #36448, #18745, #15181, #27871, #23167, #54477, #14883, #45917, #41175, #37614, #32878, #6030, #14299, #27583, #50922, #10471, #36738, #768, #27293, #5452, #24039, #41467, #22877, #40887, #478, #14012 ),
 ( #55044, #23455, #54756, #32010, #50635, #1053, #10183, #19038, #37030, #14593, #32586, #28161, #23746, #34045, #51797, #24915, #29049, #43219, #2776, #51218, #24628, #2206, #46799, #29616, #15766, #20775, #47088, #6325, #47957, #37905, #7488, #3065, #16354, #38197, #25486 ),
 ( #42934, #2488, #51509, #16060, #29330, #47377, #25199, #42353, #56217, #42639, #20492, #55929, #21061, #24342, #39062, #6907, #6617, #11352, #11067, #16638, #57076, #38489, #56505, #52083, #15480, #33760, #56794, #10770, #28749, #43506, #1920, #11641, #33471, #19914, #20205 ) ),
 .UNSPECIFIED., .F., .F., .F.,
 ( 4, 4 ),
 ( 4, 1, 1, 1, 1, 1, 1, 1, 1, 1, 1, 1, 1, 1, 1, 1, 1, 1, 1, 1, 1, 1, 1, 1, 1, 1, 1, 1, 1, 1, 1, 1, 4 ),
 ( -0.1331668876848000060, 1.133166887685000068 ),
 ( -0.02000000000000000042, 0.01250000000000000069, 0.04499999999999999833, 0.07749999999999999944, 0.1100000000000000006, 0.1424999999999999878, 0.1749999999999999889, 0.2074999999999999900, 0.2399999999999999911, 0.2725000000000000200, 0.3049999999999999933, 0.3375000000000000222, 0.3699999999999999956, 0.4025000000000000244, 0.4349999999999999978, 0.4675000000000000266, 0.5000000000000000000, 0.5324999999999999734, 0.5649999999999999467, 0.5975000000000000311, 0.6300000000000000044, 0.6624999999999999778, 0.6949999999999999512, 0.7275000000000000355, 0.7600000000000000089, 0.7924999999999999822, 0.8249999999999999556, 0.8575000000000000400, 0.8900000000000000133, 0.9224999999999999867, 0.9549999999999999600, 0.9875000000000000444, 1.020000000000000018 ),
 .UNSPECIFIED. ) ;
#47533 = B_SPLINE_CURVE_WITH_KNOTS ( 'NONE', 3,
 ( #52772, #12327, #2046, #56341, #11759, #6743, #15894, #56056, #33598, #30314, #51637, #11191, #33880, #51920, #25035, #47508 ),
 .UNSPECIFIED., .F., .F.,
 ( 4, 2, 2, 2, 2, 2, 2, 4 ),
 ( 0.000000000000000000, 0.2500000000000004996, 0.3750000000000001110, 0.4999999999999997780, 0.6249999999999993339, 0.6875000000000004441, 0.7500000000000017764, 1.000000000000000000 ),
 .UNSPECIFIED. ) ;
#47534 = ORIENTED_EDGE ( 'NONE', *, *, #48945, .T. ) ;
#47535 = CARTESIAN_POINT ( 'NONE',  ( 0.3137356748008011120, -80.89165110245198775, -1.478359838030668172 ) ) ;
#47536 = CARTESIAN_POINT ( 'NONE',  ( 12.61271904362000029, -59.99692351013000291, -1.798332623270000097 ) ) ;
#47537 = CARTESIAN_POINT ( 'NONE',  ( 0.000000000000000000, -78.49999999999998579, 0.000000000000000000 ) ) ;
#47538 = CARTESIAN_POINT ( 'NONE',  ( -0.1963495408493605987, -78.61458333333332860, -1.500000000000000444 ) ) ;
#47539 = CARTESIAN_POINT ( 'NONE',  ( 2.686313133137999909, -2.161638932810000302, -2.332641043696000338 ) ) ;
#47540 = AXIS2_PLACEMENT_3D ( 'NONE', #6398, #56578, #43006 ) ;
#47541 = CARTESIAN_POINT ( 'NONE',  ( -0.08650930969203998733, -78.31670238307098941, 12.16449944406000050 ) ) ;
#47542 = LINE ( 'NONE', #38644, #30679 ) ;
#47544 = CARTESIAN_POINT ( 'NONE',  ( -9.312499999988999022, -77.13750000001088836, -2.050180145195999796E-09 ) ) ;
#47543 = CARTESIAN_POINT ( 'NONE',  ( -3.271883600065454090, -76.09715442452088041, 11.29549362133648671 ) ) ;
#47545 = CARTESIAN_POINT ( 'NONE',  ( -1.512180334517000180, -83.18236633857299012, 0.4761993468540999808 ) ) ;
#47546 = DIRECTION ( 'NONE',  ( 0.000000000000000000, -1.000000000000000000, 0.000000000000000000 ) ) ;
#47547 = EDGE_LOOP ( 'NONE', ( #24161, #44889, #30241 ) ) ;
#47548 = CARTESIAN_POINT ( 'NONE',  ( 0.000000000000000000, -80.79999999999999716, 0.000000000000000000 ) ) ;
#47549 = CARTESIAN_POINT ( 'NONE',  ( 7.257622347668946539, -79.44361411732418787, -6.227379948060659309 ) ) ;
#47550 = CARTESIAN_POINT ( 'NONE',  ( -11.99999999979999821, -18.85000000927000130, -0.7999999997951999786 ) ) ;
#47551 = CARTESIAN_POINT ( 'NONE',  ( -8.194866293469999619, -61.51043252617999713, 9.389192598819999347 ) ) ;
#47552 = CARTESIAN_POINT ( 'NONE',  ( -10.47624881337006109, -80.07551940951682923, 3.353468735377274079 ) ) ;
#47553 = CARTESIAN_POINT ( 'NONE',  ( 6.970637445331999693, -79.95400232914698790, 6.702596717548000349 ) ) ;
#47554 = CARTESIAN_POINT ( 'NONE',  ( -12.00000000000000178, -77.91041666666669130, -1.570796326794897668 ) ) ;
#47555 = CARTESIAN_POINT ( 'NONE',  ( 4.658475568430830549, -79.16666666666665719, -8.082524092276877070 ) ) ;
#47556 = ORIENTED_EDGE ( 'NONE', *, *, #8876, .T. ) ;
#47557 = CARTESIAN_POINT ( 'NONE',  ( -2.860041384466000203, -78.88115782519599861, -10.89284755413000028 ) ) ;
#47558 = CARTESIAN_POINT ( 'NONE',  ( -12.50000000000000000, -26.93717104351999936, 0.000000000000000000 ) ) ;
#47559 = CARTESIAN_POINT ( 'NONE',  ( 8.681769470831671498, -79.35917672052410410, 8.041084891514902466 ) ) ;
#47560 = CARTESIAN_POINT ( 'NONE',  ( 9.322139347202742954, -79.52083333333069959, -1.984632903365618928 ) ) ;
#47561 = CARTESIAN_POINT ( 'NONE',  ( -0.1487011411093689672, -81.48479960741362049, 1.241381877223513897 ) ) ;
#47562 = AXIS2_PLACEMENT_3D ( 'NONE', #7264, #29968, #39129 ) ;
#47563 = CARTESIAN_POINT ( 'NONE',  ( 0.4270232520405565224, -78.30196075596913374, -1.201314851622765634 ) ) ;
#47564 = CARTESIAN_POINT ( 'NONE',  ( -1.249826857837516236, -82.11106099827752303, -0.1638645779436204153 ) ) ;
#47565 = CARTESIAN_POINT ( 'NONE',  ( -7.709155920968131070, -23.92747430419197485, -9.998700314110912757 ) ) ;
#47566 = B_SPLINE_CURVE_WITH_KNOTS ( 'NONE', 3,
 ( #5505, #55394, #37380, #14940, #45979, #42412, #33531, #23514, #28808, #28216, #32643, #55989, #23229, #24398, #32356, #54815, #1393, #1110 ),
 .UNSPECIFIED., .F., .F.,
 ( 4, 2, 2, 2, 2, 2, 2, 2, 4 ),
 ( 0.000000000000000000, 0.1250000000000000000, 0.2499999999999999722, 0.3750000000000000000, 0.5000000000000000000, 0.6250000000000000000, 0.7500000000000000000, 0.8750000000000000000, 1.000000000000000000 ),
 .UNSPECIFIED. ) ;
#47567 = EDGE_CURVE ( 'NONE', #54533, #18787, #39275, .T. ) ;
#47568 = DIRECTION ( 'NONE',  ( 0.9999896828222031298, 0.000000000000000000, 0.004542493714850020202 ) ) ;
#47569 = CARTESIAN_POINT ( 'NONE',  ( 5.413886177876668704, -78.43335082942924430, 9.393028503726839062 ) ) ;
#47570 = CIRCLE ( 'NONE', #37168, 1.199999999999999734 ) ;
#47571 = CARTESIAN_POINT ( 'NONE',  ( -8.396223008680999911, -79.75222017800098229, -4.990405176070999538 ) ) ;
#47572 = ORIENTED_EDGE ( 'NONE', *, *, #28091, .T. ) ;
#47573 = VERTEX_POINT ( 'NONE', #16560 ) ;
#47574 = CARTESIAN_POINT ( 'NONE',  ( 5.543805526018000585, -76.42052255369199543, -11.17061805242999917 ) ) ;
#47575 = CARTESIAN_POINT ( 'NONE',  ( 2.531064403381080297, -78.74405570548175604, -10.44842218354998842 ) ) ;
#47576 = CARTESIAN_POINT ( 'NONE',  ( 1.168308732057000032, -78.34511805113000094, -0.8096088536258000401 ) ) ;
#47577 = VERTEX_POINT ( 'NONE', #30113 ) ;
#47578 = DIRECTION ( 'NONE',  ( -0.7071067811865474617, 0.7071067811865474617, 1.545233129589103907E-10 ) ) ;
#47579 = CARTESIAN_POINT ( 'NONE',  ( 0.000000000000000000, -76.19999999999998863, 0.000000000000000000 ) ) ;
#47580 = CARTESIAN_POINT ( 'NONE',  ( -1.208267227064446780, -53.97409317820400787, 12.70228502419021765 ) ) ;
#47581 = CARTESIAN_POINT ( 'NONE',  ( 7.139902610388999982, -77.92838321630000564, -10.43201753306000157 ) ) ;
#47582 = CARTESIAN_POINT ( 'NONE',  ( 10.98362417419999915, -18.84999999999999787, -0.5999999999999999778 ) ) ;
#47584 = ADVANCED_FACE ( 'NONE', ( #56428 ), #14363, .F. ) ;
#47583 = FACE_OUTER_BOUND ( 'NONE', #15077, .T. ) ;
#47585 = CARTESIAN_POINT ( 'NONE',  ( 10.12290050256999940, -18.75000002239000096, 7.648026768411000376 ) ) ;
#47586 = CARTESIAN_POINT ( 'NONE',  ( 8.645668071321999548, -78.63886173219398756, 7.146365085715999044 ) ) ;
#47587 = B_SPLINE_CURVE_WITH_KNOTS ( 'NONE', 3,
 ( #15280, #6718, #2019, #38000, #19427, #32978, #24726, #32686, #51608, #14397, #11165, #56026, #15575, #28257, #19718, #9991, #55439, #42739, #33570, #50439, #51315, #10276, #23842, #37419, #2302, #10873, #37714, #27970, #20299, #38293, #51024, #33273, #46020, #5541, #55139, #23551, #41566, #46895, #1148, #28556, #50736, #46311, #46604, #5836, #41859, #1436, #14980, #24137, #6422, #42156, #24437, #46493, #24325, #41455, #28737, #19901, #46199, #42040, #42341, #10457, #28147, #24027, #1907, #37893, #1609, #6603, #19601, #37307, #1040, #33160, #51206, #41159, #14579, #10758, #45903, #55617, #46787, #6311, #37018, #36726, #55917, #50620, #32572, #32282, #37601, #5435, #15468, #51497, #10170, #33459, #50325, #5724, #23443, #55323, #15165, #9877, #23734, #41748, #28444, #19025, #11054, #29036, #6017, #47075, #753, #18732, #54740, #14286, #27857, #55032, #1323, #19317, #14867, #32864, #50909, #20762, #7761, #7475, #47364, #39049, #25765, #56205, #16624, #12472, #42920, #43785, #47658, #38185, #34609, #39343, #57350, #24615, #15753, #29602, #2764, #51787, #20479, #11337, #29315, #16047, #52070, #11628, #7184, #25184, #34320, #52357, #11908, #54092, #36070, #9214, #3897, #17481, #13039, #390, #44941, #53799, #26042, #27200, #13630, #26608, #13333, #45238, #31037, #26330, #31627, #49669, #35468, #48786, #18367, #44645, #4785, #40208, #22787, #40795, #36360, #54387, #57924, #40506, #12756, #30752, #31328, #21900, #13924, #17187, #31919, #35177, #8044, #44066, #3614, #49373, #21620, #4497, #39624, #57632, #39910, #22197, #53208, #8331, #44344, #22495 ),
 .UNSPECIFIED., .F., .F.,
 ( 4, 2, 2, 2, 1, 1, 2, 2, 2, 2, 2, 2, 2, 2, 1, 2, 2, 1, 2, 2, 1, 1, 2, 2, 2, 2, 2, 2, 1, 2, 2, 2, 2, 1, 2, 1, 1, 1, 2, 2, 2, 1, 1, 1, 2, 2, 2, 2, 1, 1, 1, 1, 2, 2, 2, 2, 2, 1, 1, 1, 1, 1, 2, 2, 2, 2, 1, 1, 1, 1, 2, 2, 2, 2, 1, 1, 2, 2, 2, 2, 1, 1, 1, 1, 1, 2, 2, 2, 2, 2, 1, 1, 1, 1, 1, 2, 2, 2, 2, 2, 1, 1, 1, 1, 2, 2, 2, 1, 1, 1, 1, 2, 2, 2, 2, 1, 1, 1, 1, 1, 2, 2, 2, 2, 2, 4 ),
 ( 0.000000000000000000, 0.03125000000000939526, 0.03515625000001058181, 0.03613281250001086631, 0.03710937500001114386, 0.03906250000001169898, 0.04687500000001394718, 0.06250000000001841582, 0.07031250000002067790, 0.07812500000002293998, 0.09375000000002757516, 0.1015625000000298650, 0.1054687500000310307, 0.1074218750000315997, 0.1093750000000321687, 0.1250000000000367206, 0.1406250000000412725, 0.1425781250000418277, 0.1428222656250419109, 0.1430664062500419942, 0.1435546875000421330, 0.1445312500000424105, 0.1484375000000435485, 0.1562500000000458245, 0.1875000000000551503, 0.1953125000000574818, 0.1962890625000577871, 0.1972656250000581202, 0.1992187500000587586, 0.2031250000000600631, 0.2187500000000654476, 0.2226562500000668077, 0.2265625000000681399, 0.2343750000000707490, 0.2421875000000733025, 0.2460937500000746070, 0.2480468750000752176, 0.2490234375000754674, 0.2495117187500755784, 0.2500000000000756617, 0.2656250000000759393, 0.2734375000000760503, 0.2773437500000761058, 0.2792968750000762168, 0.2802734375000762723, 0.2812500000000763278, 0.2968750000000785483, 0.3046875000000796585, 0.3085937500000802136, 0.3105468750000805467, 0.3115234375000806577, 0.3120117187500807687, 0.3122558593750808242, 0.3125000000000808797, 0.3437500000000918154, 0.3593750000000973110, 0.3671875000001000866, 0.3710937500001014189, 0.3730468750001020295, 0.3740234375001024736, 0.3745117187501025291, 0.3747558593751025846, 0.3748779296876025846, 0.3750000000001026401, 0.4062500000001136868, 0.4218750000001192380, 0.4296875000001220135, 0.4335937500001234013, 0.4355468750001241229, 0.4365234375001244560, 0.4370117187501246780, 0.4375000000001248446, 0.4687500000001362799, 0.4843750000001419420, 0.4921875000001448286, 0.4960937500001462164, 0.4980468750001468825, 0.5000000000001475486, 0.5312500000001589839, 0.5468750000001646461, 0.5546875000001674216, 0.5585937500001688649, 0.5605468750001695311, 0.5615234375001699751, 0.5620117187501700862, 0.5622558593751701972, 0.5625000000001701972, 0.5937500000001844080, 0.6093750000001915135, 0.6171875000001950662, 0.6210937500001968425, 0.6230468750001977307, 0.6240234375001981748, 0.6245117187501982858, 0.6247558593751983969, 0.6248779296876983969, 0.6250000000001985079, 0.6562500000001916245, 0.6718750000001881828, 0.6796875000001866285, 0.6835937500001857403, 0.6855468750001852962, 0.6865234375001851852, 0.6870117187501850742, 0.6872558593751850742, 0.6875000000001850742, 0.7031250000001876277, 0.7109375000001888489, 0.7148437500001895151, 0.7167968750001898481, 0.7177734375001900702, 0.7182617187501900702, 0.7187500000001900702, 0.7343750000001922906, 0.7421875000001932898, 0.7460937500001938449, 0.7480468750001942890, 0.7490234375001942890, 0.7495117187501944001, 0.7497558593751944001, 0.7498779296876944001, 0.7500000000001942890, 0.8125000000001457723, 0.8750000000000971445, 0.9375000000000486278, 1.000000000000000000 ),
 .UNSPECIFIED. ) ;
#47588 = ORIENTED_EDGE ( 'NONE', *, *, #27890, .F. ) ;
#47589 = CARTESIAN_POINT ( 'NONE',  ( -1.250000000000000000, -18.75000000000000000, -12.00000000000000000 ) ) ;
#47590 = ORIENTED_EDGE ( 'NONE', *, *, #55632, .T. ) ;
#47591 = CARTESIAN_POINT ( 'NONE',  ( 4.346385276184861368, -77.26393889505689572, -8.165376318784744569 ) ) ;
#47592 = CARTESIAN_POINT ( 'NONE',  ( 1.250000000000000000, -83.24999999999998579, 0.000000000000000000 ) ) ;
#47593 = CARTESIAN_POINT ( 'NONE',  ( -11.21684559259269065, -77.85035602949233180, -0.06311826741395569484 ) ) ;
#47594 = CARTESIAN_POINT ( 'NONE',  ( 1.013266355313000133, -77.86407167464599866, 1.127933319133000101 ) ) ;
#47595 = CARTESIAN_POINT ( 'NONE',  ( 14.00000000000000000, -5.900000000000010125, 0.000000000000000000 ) ) ;
#47596 = CARTESIAN_POINT ( 'NONE',  ( 0.000000000000000000, -76.30000000005068728, 0.000000000000000000 ) ) ;
#47597 = CARTESIAN_POINT ( 'NONE',  ( -0.8961266428360998848, -77.75102415030998770, 1.358359200922999888 ) ) ;
#47598 = ADVANCED_FACE ( 'NONE', ( #47877 ), #39812, .F. ) ;
#47599 = FACE_OUTER_BOUND ( 'NONE', #32242, .T. ) ;
#47600 = CARTESIAN_POINT ( 'NONE',  ( 10.34967326289000056, -78.27152425389999735, 3.868085496227999798 ) ) ;
#47601 =( NAMED_UNIT ( * ) PLANE_ANGLE_UNIT ( ) SI_UNIT ( $, .RADIAN. ) );
#47602 = EDGE_CURVE ( 'NONE', #36570, #33521, #34830, .T. ) ;
#47603 =( NAMED_UNIT ( * ) SI_UNIT ( $, .STERADIAN. ) SOLID_ANGLE_UNIT ( ) );
#47604 = CARTESIAN_POINT ( 'NONE',  ( -3.517172751179999945, -84.74356301659899771, -0.4594186973889000103 ) ) ;
#47605 = EDGE_LOOP ( 'NONE', ( #790, #27486, #8113, #27914, #9441 ) ) ;
#47606 = CARTESIAN_POINT ( 'NONE',  ( -5.496145386621526185, -77.20000000000000284, 9.413364287384716533 ) ) ;
#47607 = CARTESIAN_POINT ( 'NONE',  ( 0.5538255850406000880, -81.04673389420999285, -1.485824439479999981 ) ) ;
#47608 = FACE_OUTER_BOUND ( 'NONE', #16111, .T. ) ;
#47609 = CARTESIAN_POINT ( 'NONE',  ( -7.167604382870000457, -77.49214559880800834, 9.599037027053000770 ) ) ;
#47610 = CARTESIAN_POINT ( 'NONE',  ( -8.870405106263998363, -16.93036971772000143, 8.878274241758997931 ) ) ;
#47611 = CARTESIAN_POINT ( 'NONE',  ( 8.547507901081861093, -78.90223080703543701, 6.557426330200511799 ) ) ;
#47612 = CARTESIAN_POINT ( 'NONE',  ( 0.000000000000000000, -80.99999999999998579, -7.000000000000000000 ) ) ;
#47613 = CARTESIAN_POINT ( 'NONE',  ( -8.997179024602999675, -79.09910194988499654, 3.687079342327000298 ) ) ;
#47614 = CARTESIAN_POINT ( 'NONE',  ( 8.286539809994000194, -77.93405256877699117, 4.690803151849999963 ) ) ;
#47615 = CARTESIAN_POINT ( 'NONE',  ( 0.5926408534130915839, -81.26475886697264173, -1.100658270916459847 ) ) ;
#47616 = CARTESIAN_POINT ( 'NONE',  ( -3.190971086128000067, -77.06051199849498801, -10.56027646911999973 ) ) ;
#47617 = DIRECTION ( 'NONE',  ( 0.000000000000000000, 1.000000000000000000, 0.000000000000000000 ) ) ;
#47618 = CARTESIAN_POINT ( 'NONE',  ( 1.261602909406688955, -81.91159713657988561, 0.1820348148243792208 ) ) ;
#47619 = VERTEX_POINT ( 'NONE', #52576 ) ;
#47620 = CARTESIAN_POINT ( 'NONE',  ( -11.18238235180553630, -78.67127684549025446, 4.147843596343820494 ) ) ;
#47621 = CARTESIAN_POINT ( 'NONE',  ( 9.394120223593105834, -76.99930578456108776, 7.218235409050908657 ) ) ;
#47622 = VECTOR ( 'NONE', #21101, 1000.000000000000000 ) ;
#47623 = CARTESIAN_POINT ( 'NONE',  ( 0.4450739772378000114, -61.67813214767999597, -12.43586747599000120 ) ) ;
#47624 = CARTESIAN_POINT ( 'NONE',  ( -0.03769889196559850220, -78.67389998729011324, -3.999822345247525224 ) ) ;
#47625 = CARTESIAN_POINT ( 'NONE',  ( -9.524774638983998898, -77.22182664867399637, 5.924253427062000199 ) ) ;
#47626 = CARTESIAN_POINT ( 'NONE',  ( 7.318097147681000614, -79.55292837808998740, -8.179820946710000484 ) ) ;
#47627 = CARTESIAN_POINT ( 'NONE',  ( -1.211372597667456974, -79.40044640989285085, -0.9001875127581699942 ) ) ;
#47628 = CARTESIAN_POINT ( 'NONE',  ( -3.961164824809206841, -84.75104167177519798, -0.8542422772179285584 ) ) ;
#47629 = EDGE_CURVE ( 'NONE', #35538, #22602, #43996, .T. ) ;
#47630 = CARTESIAN_POINT ( 'NONE',  ( -12.13371464510999864, -77.07215438420399778, 0.6771217750942000180 ) ) ;
#47631 = CARTESIAN_POINT ( 'NONE',  ( 0.000000000000000000, -74.64999999999999147, 0.000000000000000000 ) ) ;
#47632 = CARTESIAN_POINT ( 'NONE',  ( -8.121699804379593601, -61.63626205714820827, 9.841121124294026856 ) ) ;
#47633 = ORIENTED_EDGE ( 'NONE', *, *, #48957, .T. ) ;
#47634 = CARTESIAN_POINT ( 'NONE',  ( -0.02557347534276610546, -79.97707957153141933, 1.249510814140374126 ) ) ;
#47635 = CARTESIAN_POINT ( 'NONE',  ( -4.658475568430826996, -78.08333333333330017, -8.082524092276880623 ) ) ;
#47636 = CARTESIAN_POINT ( 'NONE',  ( 11.15746894976000014, -77.99343189956698552, 0.05185606496389000286 ) ) ;
#47637 = DIRECTION ( 'NONE',  ( 0.000000000000000000, 1.000000000000000000, 0.000000000000000000 ) ) ;
#47638 = CARTESIAN_POINT ( 'NONE',  ( -7.220923959705292994, -77.72708333333335418, 9.396085398178589898 ) ) ;
#47639 = CARTESIAN_POINT ( 'NONE',  ( -7.651160336697000020, -56.03767313780999615, -10.45205658995000064 ) ) ;
#47640 = CARTESIAN_POINT ( 'NONE',  ( -1.509086691184912343, -82.85341321873580966, -0.07812501990390177675 ) ) ;
#47641 = CARTESIAN_POINT ( 'NONE',  ( -1.109799271607774029, -79.63855864794726358, -0.5747890205896009075 ) ) ;
#47642 = ORIENTED_EDGE ( 'NONE', *, *, #53424, .F. ) ;
#47643 = CARTESIAN_POINT ( 'NONE',  ( 1.799501877793999949, -18.71082276572999703, 12.60552511010000032 ) ) ;
#47644 =( NAMED_UNIT ( * ) SI_UNIT ( $, .STERADIAN. ) SOLID_ANGLE_UNIT ( ) );
#47645 = CARTESIAN_POINT ( 'NONE',  ( 11.44417895085270054, -76.07083333333332575, 3.075537641221564922 ) ) ;
#47646 = VERTEX_POINT ( 'NONE', #25980 ) ;
#47647 = EDGE_LOOP ( 'NONE', ( #14413, #50839, #20886, #47352 ) ) ;
#47648 = CARTESIAN_POINT ( 'NONE',  ( -12.66737112512999985, -54.56697834100999955, -1.690666607834999891 ) ) ;
#47649 = AXIS2_PLACEMENT_3D ( 'NONE', #2968, #56126, #16546 ) ;
#47650 = ORIENTED_EDGE ( 'NONE', *, *, #30602, .F. ) ;
#47651 = ORIENTED_EDGE ( 'NONE', *, *, #14682, .T. ) ;
#47652 = CARTESIAN_POINT ( 'NONE',  ( 10.00831380745999866, -23.37230364585000331, 7.646786653130999589 ) ) ;
#47653 = CARTESIAN_POINT ( 'NONE',  ( 10.47129194184999967, -77.84622061874799215, 3.086650459461000473 ) ) ;
#47654 = CARTESIAN_POINT ( 'NONE',  ( -7.655984445742507027, -60.50337239307266657, 10.06694410270485918 ) ) ;
#47656 = EDGE_CURVE ( 'NONE', #29440, #46485, #15980, .T. ) ;
#47655 = CARTESIAN_POINT ( 'NONE',  ( 9.418360348373997937, -78.46536332859899687, 2.704229673158000224 ) ) ;
#47657 = CIRCLE ( 'NONE', #20285, 2.600000000000000089 ) ;
#47658 = CARTESIAN_POINT ( 'NONE',  ( -0.2780177897949673294, -78.22274903711796412, -9.249907059576116808 ) ) ;
#47659 = CARTESIAN_POINT ( 'NONE',  ( 0.8479846733620011179, -76.25703125043162345, -10.79296874152367991 ) ) ;
#47660 = ORIENTED_EDGE ( 'NONE', *, *, #5812, .T. ) ;
#47662 = ORIENTED_EDGE ( 'NONE', *, *, #151, .T. ) ;
#47661 = ADVANCED_FACE ( 'NONE', ( #15688 ), #11273, .F. ) ;
#47663 = CARTESIAN_POINT ( 'NONE',  ( -4.013128615792370901, -77.51086162448915218, 8.336612707408551870 ) ) ;
#47664 = CARTESIAN_POINT ( 'NONE',  ( 8.002843206562671341, -77.69666666666665833, 5.305121725754474937 ) ) ;
#47665 = CARTESIAN_POINT ( 'NONE',  ( -12.54981857179000038, -61.84836586168999872, 0.03768635776142000016 ) ) ;
#47666 = CARTESIAN_POINT ( 'NONE',  ( -4.475245744599999576, -78.91700911761597581, -8.610626265545000990 ) ) ;
#47667 = CARTESIAN_POINT ( 'NONE',  ( 7.678667886032999768, -21.75736537952000305, 10.59548767697000038 ) ) ;
#47668 = CARTESIAN_POINT ( 'NONE',  ( 7.921335223427023564, -61.35094696583096407, 10.04563431751979508 ) ) ;
#47669 = CARTESIAN_POINT ( 'NONE',  ( 1.250000000000000000, -79.75000000000000000, 0.000000000000000000 ) ) ;
#47670 = CARTESIAN_POINT ( 'NONE',  ( -7.179058446792000225, -79.87950005142698728, -8.667882172381000672 ) ) ;
#47671 = CARTESIAN_POINT ( 'NONE',  ( -1.276771495430000038E-14, -69.50420297070000686, 0.000000000000000000 ) ) ;
#47672 = CARTESIAN_POINT ( 'NONE',  ( -0.9995835529977249445, -81.05208333333334281, -0.7681833999686439318 ) ) ;
#47673 = EDGE_CURVE ( 'NONE', #4324, #28272, #29826, .T. ) ;
#47674 = CARTESIAN_POINT ( 'NONE',  ( -10.43474250408442217, -76.66142246521233972, 5.404247698127043975 ) ) ;
#47675 = CARTESIAN_POINT ( 'NONE',  ( -10.01676221090000141, -55.59058563439999290, 7.658899961832999814 ) ) ;
#47676 = CARTESIAN_POINT ( 'NONE',  ( -9.090572324265000503, -77.91051332859899503, 3.947417077667999763 ) ) ;
#47677 = CARTESIAN_POINT ( 'NONE',  ( 4.899854808515000215, -78.36021422180199636, -10.93194800986000104 ) ) ;
#47678 = CARTESIAN_POINT ( 'NONE',  ( 1.799490220168999954, -19.22870851082999977, -12.64502302238000020 ) ) ;
#47680 = CARTESIAN_POINT ( 'NONE',  ( -0.4929706056563897265, -82.23302231136467810, -1.172003319111136754 ) ) ;
#47679 = CARTESIAN_POINT ( 'NONE',  ( -1.460959015002474493, -78.87916666666666288, 0.3926218265389144757 ) ) ;
#47681 = CARTESIAN_POINT ( 'NONE',  ( -1.750000000000000000, -60.04999999657000131, 12.50000000000000000 ) ) ;
#47682 = CARTESIAN_POINT ( 'NONE',  ( 10.67969489444999986, -80.15794665545099917, -2.920153015311000022 ) ) ;
#47683 = DIRECTION ( 'NONE',  ( 0.000000000000000000, -1.000000000000000000, 0.000000000000000000 ) ) ;
#47684 = CARTESIAN_POINT ( 'NONE',  ( -2.588619782347023168, -1.309278100603108008, -2.388616040639797156 ) ) ;
#47685 = VERTEX_POINT ( 'NONE', #38409 ) ;
#47686 = CARTESIAN_POINT ( 'NONE',  ( -3.271260265871036577, -3.500000000000000000, -0.5209705415795669037 ) ) ;
#47687 = CARTESIAN_POINT ( 'NONE',  ( 0.5999999999999999778, -5.000000000000000000, -4.000000000000000000 ) ) ;
#47688 = CARTESIAN_POINT ( 'NONE',  ( 0.9450313017535940663, -78.40681886214652252, 0.8189801504775520158 ) ) ;
#47689 = AXIS2_PLACEMENT_3D ( 'NONE', #49086, #57365, #36086 ) ;
#47690 = CARTESIAN_POINT ( 'NONE',  ( -6.734246782101999784, -79.39435458825498415, 6.748357038843000311 ) ) ;
#47691 = CARTESIAN_POINT ( 'NONE',  ( 5.413775304621431417, -76.93349803630370332, 9.393090362380020153 ) ) ;
#47692 = DIRECTION ( 'NONE',  ( 0.000000000000000000, -1.000000000000000000, 0.000000000000000000 ) ) ;
#47693 = CARTESIAN_POINT ( 'NONE',  ( 3.250000000000000000, -3.250000000000000000, 0.000000000000000000 ) ) ;
#47694 = DIRECTION ( 'NONE',  ( 0.000000000000000000, -1.000000000000000000, 0.000000000000000000 ) ) ;
#47695 = CARTESIAN_POINT ( 'NONE',  ( -2.398287285837117810, -78.69999999999998863, 3.977573602256943008 ) ) ;
#47696 = CARTESIAN_POINT ( 'NONE',  ( -3.852910167356999871, -77.77443257914897856, 10.24742925129999982 ) ) ;
#47697 = CARTESIAN_POINT ( 'NONE',  ( 9.278274563759739024, -76.39710617612774968, -7.210752084677405804 ) ) ;
#47698 = CARTESIAN_POINT ( 'NONE',  ( -9.833855776131001036, -77.17856642211100393, -4.999701486664000605 ) ) ;
#47699 = CARTESIAN_POINT ( 'NONE',  ( -0.8980135761429828278, -82.03944583936498702, 0.8691029177942691808 ) ) ;
#47700 = LINE ( 'NONE', #48550, #16094 ) ;
#47701 = CARTESIAN_POINT ( 'NONE',  ( -8.324924863653999196, -77.28764894901499360, 4.923709561474999497 ) ) ;
#47702 = CARTESIAN_POINT ( 'NONE',  ( -9.250000000000005329, -78.48958333333331439, 1.210822168571030977 ) ) ;
#47703 = CARTESIAN_POINT ( 'NONE',  ( 0.8506806241676642122, -2.645833333333333037, -3.165411199172024848 ) ) ;
#47704 = CARTESIAN_POINT ( 'NONE',  ( 0.000000000000000000, -76.39999999999999147, 0.000000000000000000 ) ) ;
#47705 = ADVANCED_FACE ( 'NONE', ( #33970 ), #13477, .F. ) ;
#47706 = CARTESIAN_POINT ( 'NONE',  ( -1.178447680628000205, -80.95308451575900222, -0.9280415206345000723 ) ) ;
#47707 = CARTESIAN_POINT ( 'NONE',  ( 5.622902522875882880, -80.01669284979236352, -9.705904178814742878 ) ) ;
#47708 = CARTESIAN_POINT ( 'NONE',  ( -2.112861425255000203, -79.17705577139200557, -11.84242215301999934 ) ) ;
#47709 = CARTESIAN_POINT ( 'NONE',  ( 1.092232985442820992, -81.79166666666667140, 0.6295237254636267821 ) ) ;
#47710 = CARTESIAN_POINT ( 'NONE',  ( 8.588590363140999884, -80.01743035202939325, -7.284921508032001114 ) ) ;
#47711 = VERTEX_POINT ( 'NONE', #47595 ) ;
#47712 = DIRECTION ( 'NONE',  ( -2.678926851037000120E-11, -1.000000000000000000, -2.678911359553000079E-11 ) ) ;
#47713 = VERTEX_POINT ( 'NONE', #56719 ) ;
#47714 = EDGE_LOOP ( 'NONE', ( #45818, #51967, #7246, #28068, #56451 ) ) ;
#47715 = CYLINDRICAL_SURFACE ( 'NONE', #10338, 11.59999999999999964 ) ;
#47716 = ORIENTED_EDGE ( 'NONE', *, *, #13188, .T. ) ;
#47717 = CARTESIAN_POINT ( 'NONE',  ( -1.297011388420000078, -79.17506245343760440, -3.346857603051000218 ) ) ;
#47718 = CARTESIAN_POINT ( 'NONE',  ( 3.025362517619666125, -79.24890232342751517, 9.005302098445666203 ) ) ;
#47719 = ORIENTED_EDGE ( 'NONE', *, *, #11880, .F. ) ;
#47720 = LINE ( 'NONE', #38543, #8242 ) ;
#47721 = CARTESIAN_POINT ( 'NONE',  ( 9.250000000000000000, -77.84999999999999432, 0.000000000000000000 ) ) ;
#47722 = B_SPLINE_CURVE_WITH_KNOTS ( 'NONE', 3,
 ( #13800, #10264, #54560, #566, #55128, #50137 ),
 .UNSPECIFIED., .F., .F.,
 ( 4, 1, 1, 4 ),
 ( 0.000000000000000000, 0.3333333333333000081, 0.6666666666667000474, 1.000000000000000000 ),
 .UNSPECIFIED. ) ;
#47724 = ADVANCED_FACE ( 'NONE', ( #7122 ), #43425, .T. ) ;
#47723 = ORIENTED_EDGE ( 'NONE', *, *, #33846, .F. ) ;
#47725 = CARTESIAN_POINT ( 'NONE',  ( 0.4576869496836571405, -79.44562341424763474, 1.163108042213991444 ) ) ;
#47726 = CARTESIAN_POINT ( 'NONE',  ( -1.058013582825246601, -78.18692974818745256, 1.074266245500460570 ) ) ;
#47727 = AXIS2_PLACEMENT_3D ( 'NONE', #54982, #8949, #19267 ) ;
#47728 = CARTESIAN_POINT ( 'NONE',  ( -8.123805058510761512, -80.04318495892768226, 7.052709536781835098 ) ) ;
#47729 = CARTESIAN_POINT ( 'NONE',  ( 4.000000000000000000, -76.79999999999999716, 0.000000000000000000 ) ) ;
#47730 = CARTESIAN_POINT ( 'NONE',  ( -3.929996950241438913, -86.09999999999996589, -0.3761983785358135046 ) ) ;
#47731 = CARTESIAN_POINT ( 'NONE',  ( 4.903943924252999409, -76.56280468648299120, -10.05113017056000047 ) ) ;
#47732 = AXIS2_PLACEMENT_3D ( 'NONE', #53190, #18058, #4180 ) ;
#47733 = CARTESIAN_POINT ( 'NONE',  ( 0.000000000000000000, -80.70000000000000284, 0.000000000000000000 ) ) ;
#47734 = CARTESIAN_POINT ( 'NONE',  ( 8.796335266379964324, -78.50208333333334565, 6.760013919724087827 ) ) ;
#47735 = CARTESIAN_POINT ( 'NONE',  ( 8.366417051415998785, -76.01633500948599931, -7.302494661396999653 ) ) ;
#47736 = EDGE_CURVE ( 'NONE', #23864, #57123, #55901, .T. ) ;
#47737 = CARTESIAN_POINT ( 'NONE',  ( -3.506546898566349935, -78.69415870367357968, -8.559525909970664870 ) ) ;
#47738 = CARTESIAN_POINT ( 'NONE',  ( -0.9102058945833000347, -80.61289048198399598, 0.9747214924314999696 ) ) ;
#47739 = DIRECTION ( 'NONE',  ( -0.9999813732757145690, 0.000000000000000000, 0.006103531896856088240 ) ) ;
#47740 = CARTESIAN_POINT ( 'NONE',  ( 1.239372798835131739, -2.944998029927256677, 3.003655695478087750 ) ) ;
#47741 = CARTESIAN_POINT ( 'NONE',  ( 3.146181864693999852, -79.28328455456849611, 2.052535432853999975 ) ) ;
#47742 = CARTESIAN_POINT ( 'NONE',  ( 1.250000000000000000, -82.34999999999999432, 0.000000000000000000 ) ) ;
#47743 = CARTESIAN_POINT ( 'NONE',  ( 9.700000000000001066, -87.20000000000000284, 0.000000000000000000 ) ) ;
#47744 = CARTESIAN_POINT ( 'NONE',  ( 8.096452064242996016, -59.58578169018998949, 13.15643568217000769 ) ) ;
#47745 = CARTESIAN_POINT ( 'NONE',  ( -1.489081774397999824, -85.02799735065198661, -3.216768448715999984 ) ) ;
#47746 = CARTESIAN_POINT ( 'NONE',  ( -11.74507272963526638, -76.20387938085427493, -0.6100094135503494330 ) ) ;
#47747 = CARTESIAN_POINT ( 'NONE',  ( -0.9448991540836102487, -79.30853710731122419, -0.8550289145944398594 ) ) ;
#47748 = CARTESIAN_POINT ( 'NONE',  ( 1.407171709420409478, -80.13541666666665719, -10.75000000000000000 ) ) ;
#47749 = CARTESIAN_POINT ( 'NONE',  ( 9.250000000000000000, -78.24999999999998579, -1.152201742116999973E-14 ) ) ;
#47750 = CARTESIAN_POINT ( 'NONE',  ( 1.500000000000000888, -77.73958333333332860, -0.1963495408493590444 ) ) ;
#47751 = CARTESIAN_POINT ( 'NONE',  ( -0.7554284705563483193, -80.48333333333333428, -1.310679582531387721 ) ) ;
#47752 = CARTESIAN_POINT ( 'NONE',  ( 12.83677138648000060, -23.22737696056999823, 2.062839765281999860 ) ) ;
#47753 = CARTESIAN_POINT ( 'NONE',  ( 10.10912517723447124, -23.47586858184537206, 7.634643689412686562 ) ) ;
#47754 = LINE ( 'NONE', #7289, #20696 ) ;
#47755 = CARTESIAN_POINT ( 'NONE',  ( 11.43133530979999968, -76.89853223350999656, -2.936322344009000052 ) ) ;
#47756 = ORIENTED_EDGE ( 'NONE', *, *, #1100, .T. ) ;
#47757 = FACE_OUTER_BOUND ( 'NONE', #53635, .T. ) ;
#47758 = CARTESIAN_POINT ( 'NONE',  ( -10.94304050380999982, -80.25384972744670620, 3.215197110691000226 ) ) ;
#47759 = B_SPLINE_CURVE_WITH_KNOTS ( 'NONE', 3,
 ( #48825, #8367, #31371, #44686, #49415, #26650, #8963, #4536, #50004, #9257, #26366, #27242, #45281, #22538, #53538, #40548, #44384, #18119 ),
 .UNSPECIFIED., .F., .F.,
 ( 4, 2, 2, 2, 2, 2, 2, 2, 4 ),
 ( 0.000000000000000000, 0.1250000000000000000, 0.2500000000000000000, 0.3750000000000000000, 0.5000000000000000000, 0.6250000000000000000, 0.7500000000000000000, 0.8750000000000000000, 1.000000000000000000 ),
 .UNSPECIFIED. ) ;
#47760 = CARTESIAN_POINT ( 'NONE',  ( 12.43652404748999984, -61.72065244505999715, 0.1284256373645000227 ) ) ;
#47761 = CARTESIAN_POINT ( 'NONE',  ( 4.693157761522999571, -78.73635037319999697, -11.90123672215999839 ) ) ;
#47762 = FACE_OUTER_BOUND ( 'NONE', #6516, .T. ) ;
#47763 = CARTESIAN_POINT ( 'NONE',  ( 8.982692273745001899, -77.67242364445598923, 3.473391639513999429 ) ) ;
#47764 = CARTESIAN_POINT ( 'NONE',  ( -3.976122264605000733, -86.18656799980000471, 0.4345342749550000216 ) ) ;
#47765 = CARTESIAN_POINT ( 'NONE',  ( 4.314091565978001697, -79.94225553412998408, 9.846348350499049218 ) ) ;
#47766 = CARTESIAN_POINT ( 'NONE',  ( -1.434155062425999994, -79.05986310998500244, -0.2237658014421000097 ) ) ;
#47767 = VERTEX_POINT ( 'NONE', #45179 ) ;
#47768 = AXIS2_PLACEMENT_3D ( 'NONE', #281, #27673, #54273 ) ;
#47769 = EDGE_CURVE ( 'NONE', #16112, #35060, #41913, .T. ) ;
#47770 = CARTESIAN_POINT ( 'NONE',  ( 10.44328705206031316, -77.33088393209217770, -2.574374161856753052 ) ) ;
#47771 = CARTESIAN_POINT ( 'NONE',  ( -11.00000000000000000, -78.69999999999998863, 0.000000000000000000 ) ) ;
#47772 = CARTESIAN_POINT ( 'NONE',  ( 2.428538520610905138, -78.97637148647436334, -2.635006473292730966 ) ) ;
#47773 = CIRCLE ( 'NONE', #25106, 1.250000000000000000 ) ;
#47774 = ORIENTED_EDGE ( 'NONE', *, *, #2056, .F. ) ;
#47775 = EDGE_CURVE ( 'NONE', #45976, #8616, #41609, .T. ) ;
#47776 = CARTESIAN_POINT ( 'NONE',  ( 1.678937288468000055, -78.23355279846498433, 10.81059606312000021 ) ) ;
#47777 = CARTESIAN_POINT ( 'NONE',  ( 12.92181194098999875, -57.04351820043999766, 2.062502994258999856 ) ) ;
#47778 = CARTESIAN_POINT ( 'NONE',  ( 11.17912310309000112, -80.04393697167898836, -1.842803918785000272 ) ) ;
#47779 = CIRCLE ( 'NONE', #57188, 14.00000000000000000 ) ;
#47780 = VERTEX_POINT ( 'NONE', #28303 ) ;
#47781 = EDGE_LOOP ( 'NONE', ( #20107, #31659, #16252, #19080 ) ) ;
#47782 = ORIENTED_EDGE ( 'NONE', *, *, #46750, .T. ) ;
#47783 = CARTESIAN_POINT ( 'NONE',  ( -0.2838824429006977512, -80.49333599480686985, 1.217375917920300532 ) ) ;
#47784 = CARTESIAN_POINT ( 'NONE',  ( -11.28006698294270471, -78.17317328678146282, 3.842900084313429776 ) ) ;
#47785 = CARTESIAN_POINT ( 'NONE',  ( 9.767191983224998708, -79.88058071758803180, 0.05162932631433000269 ) ) ;
#47786 = ORIENTED_EDGE ( 'NONE', *, *, #30318, .T. ) ;
#47787 = CARTESIAN_POINT ( 'NONE',  ( 12.66313295592999921, -53.62196533848999991, -0.06049275240488000138 ) ) ;
#47789 = ADVANCED_FACE ( 'NONE', ( #46353 ), #37461, .F. ) ;
#47788 = EDGE_LOOP ( 'NONE', ( #25835, #19240, #45188, #13875 ) ) ;
#47790 = CARTESIAN_POINT ( 'NONE',  ( 12.21456857099000004, -78.79287284168630379, -1.096995930408000142 ) ) ;
#47791 = CARTESIAN_POINT ( 'NONE',  ( -3.474812103689401965, -78.85171435493610659, -1.963390115445670991 ) ) ;
#47792 = CARTESIAN_POINT ( 'NONE',  ( 9.934825859729000896, -54.17633188858999915, 7.968960864672001598 ) ) ;
#47793 = CARTESIAN_POINT ( 'NONE',  ( 1.199500263597268246, -80.70208333333333428, 0.9218200799623752495 ) ) ;
#47794 = CARTESIAN_POINT ( 'NONE',  ( -1.500000000000000000, -81.40000000000000568, 0.000000000000000000 ) ) ;
#47795 = CARTESIAN_POINT ( 'NONE',  ( -9.648205698377651629, -78.53912913613841340, 1.218851828996400766 ) ) ;
#47796 = CARTESIAN_POINT ( 'NONE',  ( 7.413727788746441227, -80.66735391346617234, 8.409593088671112326 ) ) ;
#47797 = CARTESIAN_POINT ( 'NONE',  ( 3.249499231399000099, -78.79685944621013505, -11.53069031867000049 ) ) ;
#47798 = ADVANCED_FACE ( 'NONE', ( #15028 ), #6879, .T. ) ;
#47799 = CARTESIAN_POINT ( 'NONE',  ( 3.758258207583866195, -80.85833333634744235, -1.512211360522490722 ) ) ;
#47800 = CARTESIAN_POINT ( 'NONE',  ( -7.646966600018000548, -23.19642081717000082, 10.19019745247000053 ) ) ;
#47801 = EDGE_CURVE ( 'NONE', #18799, #36499, #57385, .T. ) ;
#47802 = VECTOR ( 'NONE', #19755, 1000.000000000000000 ) ;
#47803 = CARTESIAN_POINT ( 'NONE',  ( 3.793820962314999878, -79.36005496681158888, -1.736947023676999935 ) ) ;
#47804 = CARTESIAN_POINT ( 'NONE',  ( -4.658475568430852753, -77.91666666666665719, 8.082524092276868188 ) ) ;
#47805 = CARTESIAN_POINT ( 'NONE',  ( 9.835223439052001027, -60.88138927622999574, -7.760980897183999971 ) ) ;
#47806 = CARTESIAN_POINT ( 'NONE',  ( 10.16243366810999937, -79.18539039009999669, -6.864696462387000153 ) ) ;
#47807 = DIRECTION ( 'NONE',  ( -1.000000000000000000, 0.000000000000000000, 0.000000000000000000 ) ) ;
#47808 = DIRECTION ( 'NONE',  ( 0.000000000000000000, -1.000000000000000000, 0.000000000000000000 ) ) ;
#47809 = AXIS2_PLACEMENT_3D ( 'NONE', #45738, #45441, #41000 ) ;
#47810 = DIRECTION ( 'NONE',  ( 1.000000000000000000, 0.000000000000000000, 0.000000000000000000 ) ) ;
#47811 = CARTESIAN_POINT ( 'NONE',  ( -1.092232985442822102, -78.54166666666664298, -0.6295237254636245616 ) ) ;
#47812 = AXIS2_PLACEMENT_3D ( 'NONE', #21191, #44214, #20623 ) ;
#47813 = CARTESIAN_POINT ( 'NONE',  ( -0.4436761913305327099, -80.64873104433648621, 1.445706986503831892 ) ) ;
#47814 = CARTESIAN_POINT ( 'NONE',  ( 12.83675988122999989, -60.02754371127999633, -2.062832873794000044 ) ) ;
#47815 = CARTESIAN_POINT ( 'NONE',  ( -1.250000000000000000, -79.00000000000000000, 0.000000000000000000 ) ) ;
#47816 = VECTOR ( 'NONE', #53640, 1000.000000000000000 ) ;
#47817 = CARTESIAN_POINT ( 'NONE',  ( 10.98749645531832364, -78.68354319426249788, 4.929334125397527799 ) ) ;
#47818 = CARTESIAN_POINT ( 'NONE',  ( -3.201679521582999843, -1.948833096892000016, 0.8095118808495000984 ) ) ;
#47819 = CARTESIAN_POINT ( 'NONE',  ( 10.48586718643000104, -77.21786888426198914, -5.936521791247999502 ) ) ;
#47820 = CARTESIAN_POINT ( 'NONE',  ( 1.265244864176999995, -77.63544661340898756, 9.657062241701000360 ) ) ;
#47821 = EDGE_CURVE ( 'NONE', #15231, #57621, #35124, .T. ) ;
#47823 = CARTESIAN_POINT ( 'NONE',  ( -1.138524516885000004, -79.19979032468299351, 0.6666316858816999646 ) ) ;
#47822 = CARTESIAN_POINT ( 'NONE',  ( 3.708203932500000022, -75.80000000000001137, 11.41267819554000162 ) ) ;
#47824 = CARTESIAN_POINT ( 'NONE',  ( 1.308628125960000110, -81.85586534759998756, -0.6662886516973000051 ) ) ;
#47825 = CARTESIAN_POINT ( 'NONE',  ( 8.485281374238999419, -55.64999999967000122, -8.485281374238999419 ) ) ;
#47826 = ORIENTED_EDGE ( 'NONE', *, *, #46593, .T. ) ;
#47827 = CARTESIAN_POINT ( 'NONE',  ( -10.24996238031000040, -20.24828923609000242, -7.705119999441000012 ) ) ;
#47828 = CARTESIAN_POINT ( 'NONE',  ( 7.730712852075999564, -79.57901625786399791, 9.381427633351998807 ) ) ;
#47829 = CARTESIAN_POINT ( 'NONE',  ( -8.483652677471663850, -79.28772561977511657, -4.355244364560813430 ) ) ;
#47830 = CARTESIAN_POINT ( 'NONE',  ( 2.808087910937577814, -79.75624999999999432, 11.70482407730010799 ) ) ;
#47831 = CARTESIAN_POINT ( 'NONE',  ( -7.618394338655000375, -60.02713821237000502, 10.53494418060999926 ) ) ;
#47832 = DIRECTION ( 'NONE',  ( -1.000000000000000000, 0.000000000000000000, 0.000000000000000000 ) ) ;
#47833 = CARTESIAN_POINT ( 'NONE',  ( 7.920804980698999742, -79.96971083593997776, -5.924224909051000409 ) ) ;
#47834 = CYLINDRICAL_SURFACE ( 'NONE', #9785, 12.80000000000000071 ) ;
#47835 = CARTESIAN_POINT ( 'NONE',  ( 6.760013919724077169, -78.77708333333333712, -8.796335266379973206 ) ) ;
#47836 = EDGE_LOOP ( 'NONE', ( #21683, #28717, #1156, #50610 ) ) ;
#47837 = FACE_OUTER_BOUND ( 'NONE', #40292, .T. ) ;
#47838 = CARTESIAN_POINT ( 'NONE',  ( 2.595923711085492247, -79.40708866698008705, 11.48131793224416697 ) ) ;
#47839 = CARTESIAN_POINT ( 'NONE',  ( 8.440830090958000298, -79.52906001420200255, -4.863879970414000553 ) ) ;
#47840 = EDGE_CURVE ( 'NONE', #10899, #29444, #18595, .T. ) ;
#47841 = CARTESIAN_POINT ( 'NONE',  ( 0.000000000000000000, -23.75000000000000000, -11.79999999999999893 ) ) ;
#47842 = CARTESIAN_POINT ( 'NONE',  ( -1.497546582071999977, -80.79352275519998727, 0.7298035716741000378 ) ) ;
#47843 = ORIENTED_EDGE ( 'NONE', *, *, #29990, .F. ) ;
#47844 = CARTESIAN_POINT ( 'NONE',  ( 0.1162510832417349149, -79.01752743935004730, 1.268882844012923838 ) ) ;
#47845 = FACE_OUTER_BOUND ( 'NONE', #14704, .T. ) ;
#47846 = DIRECTION ( 'NONE',  ( 0.000000000000000000, -1.000000000000000000, 0.000000000000000000 ) ) ;
#47847 = CIRCLE ( 'NONE', #5388, 10.20000000000000107 ) ;
#47848 = CARTESIAN_POINT ( 'NONE',  ( -12.71658889743999943, -60.11584477251999203, 1.931087888049999979 ) ) ;
#47849 = CARTESIAN_POINT ( 'NONE',  ( -2.813605875113437182, -78.49586331468553624, 10.46960120928732607 ) ) ;
#47850 = CARTESIAN_POINT ( 'NONE',  ( -0.5483576180056000116, -79.33007562064699414, -9.751923335751000010 ) ) ;
#47851 = VERTEX_POINT ( 'NONE', #25624 ) ;
#47852 = AXIS2_PLACEMENT_3D ( 'NONE', #18140, #40863, #26387 ) ;
#47853 = ORIENTED_EDGE ( 'NONE', *, *, #36765, .F. ) ;
#47854 = CARTESIAN_POINT ( 'NONE',  ( 11.90218195501999965, -77.10299069267900052, 4.100124956475999838 ) ) ;
#47855 = CARTESIAN_POINT ( 'NONE',  ( 5.166696889923573011, -78.76497110610900165, -9.426996544925714261 ) ) ;
#47856 = EDGE_LOOP ( 'NONE', ( #44168, #736, #32345 ) ) ;
#47857 = CARTESIAN_POINT ( 'NONE',  ( 8.292781013307999771, -16.94469293076999961, 9.770415148734000965 ) ) ;
#47858 = CARTESIAN_POINT ( 'NONE',  ( 1.882211411147126867, -78.70937264597593241, 9.520037184477153858 ) ) ;
#47859 = AXIS2_PLACEMENT_3D ( 'NONE', #9782, #31312, #17464 ) ;
#47860 = CARTESIAN_POINT ( 'NONE',  ( 1.003693376005942550, -53.83776007856020840, 12.70247752660074347 ) ) ;
#47861 = CARTESIAN_POINT ( 'NONE',  ( 9.024219425886000678, -76.86072037624001041, -8.086445476350000661 ) ) ;
#47862 = DIRECTION ( 'NONE',  ( 0.9999999999999998890, -1.433670265775999799E-08, 0.000000000000000000 ) ) ;
#47863 = FACE_BOUND ( 'NONE', #50256, .T. ) ;
#47864 = DIRECTION ( 'NONE',  ( 0.000000000000000000, 1.000000000000000000, 0.000000000000000000 ) ) ;
#47865 = CARTESIAN_POINT ( 'NONE',  ( 5.986115112277999195, -80.23188549357229249, 9.486000076385000312 ) ) ;
#47866 = CARTESIAN_POINT ( 'NONE',  ( -0.7330981857557979930, -79.98140777903502396, 9.220843587065861158 ) ) ;
#47867 = VERTEX_POINT ( 'NONE', #10914 ) ;
#47868 = CARTESIAN_POINT ( 'NONE',  ( -11.75000000000000000, -76.20000000000000284, -1.391479524197000231E-14 ) ) ;
#47869 = EDGE_LOOP ( 'NONE', ( #33304, #46949, #31741, #14751 ) ) ;
#47870 = CARTESIAN_POINT ( 'NONE',  ( 7.511900341590999730, -79.80389345209998453, -8.396444939682998765 ) ) ;
#47871 = CARTESIAN_POINT ( 'NONE',  ( 9.249996494687895421, -77.35002555369160859, 0.002770370553531230698 ) ) ;
#47872 = CARTESIAN_POINT ( 'NONE',  ( 0.9236342483431000394, -80.42865684227599843, -0.9420537984437000745 ) ) ;
#47873 = DIRECTION ( 'NONE',  ( -1.000000000000000000, 0.000000000000000000, 0.000000000000000000 ) ) ;
#47874 = CARTESIAN_POINT ( 'NONE',  ( 7.199925632633625838, -77.16944745444732234, 8.601318494760706201 ) ) ;
#47875 = UNCERTAINTY_MEASURE_WITH_UNIT (LENGTH_MEASURE( 1.000000000000000082E-05 ), #376, 'distance_accuracy_value', 'NONE');
#47876 = CARTESIAN_POINT ( 'NONE',  ( -1.488622005431999851, -78.06252216817030387, -0.2880046469693999800 ) ) ;
#47877 = FACE_OUTER_BOUND ( 'NONE', #28282, .T. ) ;
#47878 = CARTESIAN_POINT ( 'NONE',  ( -2.813789756862300262, -80.89583333333328596, 10.47020627418438465 ) ) ;
#47879 = CARTESIAN_POINT ( 'NONE',  ( 1.623578234368999951, -78.08511356898999622, 0.1125035222880000074 ) ) ;
#47880 = CARTESIAN_POINT ( 'NONE',  ( 0.000000000000000000, -80.69999999999998863, 0.000000000000000000 ) ) ;
#47881 = CARTESIAN_POINT ( 'NONE',  ( -7.626500777237000150, -18.68415268018999953, 10.35747145892000098 ) ) ;
#47882 = CARTESIAN_POINT ( 'NONE',  ( 2.567527713034000403, -78.63672486022498731, -10.74642708485000142 ) ) ;
#47883 = CARTESIAN_POINT ( 'NONE',  ( -9.837756816580965236, -24.31467795600408266, -7.850057934563161588 ) ) ;
#47884 =( LENGTH_UNIT ( ) NAMED_UNIT ( * ) SI_UNIT ( .MILLI., .METRE. ) );
#47885 = SURFACE_SIDE_STYLE ('',( #42861 ) ) ;
#47886 = DIRECTION ( 'NONE',  ( 0.000000000000000000, -0.7071067811866525998, -0.7071067811864425456 ) ) ;
#47887 = ORIENTED_EDGE ( 'NONE', *, *, #40304, .F. ) ;
#47888 = CARTESIAN_POINT ( 'NONE',  ( 0.5386432692752000095, -83.17941453081499503, 1.615427185862999826 ) ) ;
#47889 = CARTESIAN_POINT ( 'NONE',  ( -0.3737996561424999920, -80.35214000165998982, 1.420113360969999849 ) ) ;
#47890 = DIRECTION ( 'NONE',  ( -1.000000000000000000, 0.000000000000000000, -1.158063445485999906E-14 ) ) ;
#47891 = CARTESIAN_POINT ( 'NONE',  ( 1.634596122093999959, -78.86221076299099764, 11.63574645295999943 ) ) ;
#47892 = CARTESIAN_POINT ( 'NONE',  ( -12.71162569433759515, -17.76025712765776987, 1.720540999454742481 ) ) ;
#47893 = CARTESIAN_POINT ( 'NONE',  ( 1.271232804528975580, -79.00641992688407811, 0.09643353776494044405 ) ) ;
#47894 = CARTESIAN_POINT ( 'NONE',  ( 2.125686459585773846, -1.925872778455320455, -2.860343808299961488 ) ) ;
#47895 = CARTESIAN_POINT ( 'NONE',  ( -3.230363664242999810, -78.22810194988500143, -9.171071524558000121 ) ) ;
#47896 = CARTESIAN_POINT ( 'NONE',  ( -7.921993249237998747, -78.18986703093798951, -5.283218639336999978 ) ) ;
#47898 = ADVANCED_FACE ( 'NONE', ( #24769 ), #56931, .T. ) ;
#47897 = CARTESIAN_POINT ( 'NONE',  ( 1.250000000000000000, -81.34999999999999432, 0.000000000000000000 ) ) ;
#47899 = CARTESIAN_POINT ( 'NONE',  ( -4.410648470793000264, -77.61849323694099212, -9.986067597275999574 ) ) ;
#47900 = CARTESIAN_POINT ( 'NONE',  ( -1.250000000000000000, -78.00000000000000000, 2.658254822585999717E-14 ) ) ;
#47901 = DIRECTION ( 'NONE',  ( 0.000000000000000000, 1.000000000000000000, 0.000000000000000000 ) ) ;
#47902 = CARTESIAN_POINT ( 'NONE',  ( 7.601397897754999633, -60.04999999966999980, -9.369164850722000892 ) ) ;
#47903 = VERTEX_POINT ( 'NONE', #30038 ) ;
#47904 = CARTESIAN_POINT ( 'NONE',  ( -2.421167930323375295, -78.89583333333332860, 9.009247259181911716 ) ) ;
#47905 = CARTESIAN_POINT ( 'NONE',  ( 5.918638737202504885, -77.03089283734779258, 10.27313499612968251 ) ) ;
#47906 = CARTESIAN_POINT ( 'NONE',  ( -2.904336368201000163, -79.22060522871599630, 11.92263291878999887 ) ) ;
#47907 = VECTOR ( 'NONE', #17544, 1000.000000000000000 ) ;
#47908 = CARTESIAN_POINT ( 'NONE',  ( -0.03689308533088261205, -78.48547955770028750, -3.914326904521404860 ) ) ;
#47909 = CARTESIAN_POINT ( 'NONE',  ( -1.561527218546999940, -82.35792792946999441, -0.5804237711334999661 ) ) ;
#47910 = CARTESIAN_POINT ( 'NONE',  ( -10.90760146693999921, -78.87871187410598850, -1.219937219691999974 ) ) ;
#47911 = CARTESIAN_POINT ( 'NONE',  ( -1.493873713138741843, -79.33798222089950514, 0.2208649169497922671 ) ) ;
#47912 = CARTESIAN_POINT ( 'NONE',  ( -1.417398247622813079, -80.37838541666540948, 10.82161458338522841 ) ) ;
#47913 = LINE ( 'NONE', #33719, #49650 ) ;
#47914 = CARTESIAN_POINT ( 'NONE',  ( 11.21770439229572247, -78.47291413386186321, 3.494388818491212856 ) ) ;
#47915 = DIRECTION ( 'NONE',  ( 0.000000000000000000, 1.000000000000000000, 0.000000000000000000 ) ) ;
#47916 = ORIENTED_EDGE ( 'NONE', *, *, #56573, .F. ) ;
#47917 = CARTESIAN_POINT ( 'NONE',  ( -2.693529710394999999, -79.60328470783500165, 10.81663063389000001 ) ) ;
#47918 = CARTESIAN_POINT ( 'NONE',  ( -0.9999999970599000587, -81.20000000293998710, -7.000000017349999659 ) ) ;
#47919 = CARTESIAN_POINT ( 'NONE',  ( 6.760013919724038978, -78.02291666666666003, 8.796335266380001627 ) ) ;
#47920 = EDGE_CURVE ( 'NONE', #1043, #409, #38959, .T. ) ;
#47921 = CARTESIAN_POINT ( 'NONE',  ( 6.895942029498000281, -78.85660385176299769, -8.909260232556000858 ) ) ;
#47922 = CARTESIAN_POINT ( 'NONE',  ( -12.49168433582000226, -60.09849137195000424, -1.667916687244999974 ) ) ;
#47923 = CARTESIAN_POINT ( 'NONE',  ( 11.74999999999999289, -77.56041666666666856, 1.538071403320028452 ) ) ;
#47924 = CARTESIAN_POINT ( 'NONE',  ( 12.50000000000000000, -23.25000000000000000, -1.250000000000000000 ) ) ;
#47925 = CARTESIAN_POINT ( 'NONE',  ( 0.04925494599860675421, -82.72182841701953748, 1.510347986472535320 ) ) ;
#47926 = PRODUCT_DEFINITION_SHAPE ( 'NONE', 'NONE',  #4815 ) ;
#47927 = PLANE ( 'NONE',  #7046 ) ;
#47928 = ADVANCED_FACE ( 'NONE', ( #29467 ), #36786, .F. ) ;
#47929 = DIRECTION ( 'NONE',  ( 0.000000000000000000, 1.000000000000000000, 0.000000000000000000 ) ) ;
#47930 = DIRECTION ( 'NONE',  ( 1.000000000000000000, 0.000000000000000000, 0.000000000000000000 ) ) ;
#47931 = EDGE_CURVE ( 'NONE', #52567, #2048, #18657, .T. ) ;
#47932 = CARTESIAN_POINT ( 'NONE',  ( -12.83675988120999989, -23.22754371161000009, 2.062832873794000044 ) ) ;
#47933 = ORIENTED_EDGE ( 'NONE', *, *, #54218, .F. ) ;
#47934 = EDGE_LOOP ( 'NONE', ( #8158, #25422, #53628 ) ) ;
#47935 = CARTESIAN_POINT ( 'NONE',  ( -12.66001647282000064, -54.16746073337000666, -1.381678996660000047 ) ) ;
#47936 = VERTEX_POINT ( 'NONE', #22779 ) ;
#47937 = VERTEX_POINT ( 'NONE', #38032 ) ;
#47938 = CARTESIAN_POINT ( 'NONE',  ( -2.181032210905110791, -81.00000000000000000, -10.72093034226582553 ) ) ;
#47939 = CARTESIAN_POINT ( 'NONE',  ( -0.1861229965304324052, -77.82161458351710337, -1.428385417274072422 ) ) ;
#47940 = CIRCLE ( 'NONE', #46080, 12.57042253521000141 ) ;
#47941 = FACE_BOUND ( 'NONE', #56548, .T. ) ;
#47942 = VECTOR ( 'NONE', #18157, 999.9999999999998863 ) ;
#47943 = CARTESIAN_POINT ( 'NONE',  ( 2.029274658824999911, -78.33471332859899405, -9.586470329786999756 ) ) ;
#47944 = CARTESIAN_POINT ( 'NONE',  ( 8.696932689530999738, -76.29999999999999716, -6.318691462144000681 ) ) ;
#47945 = ORIENTED_EDGE ( 'NONE', *, *, #18621, .T. ) ;
#47946 = ORIENTED_EDGE ( 'NONE', *, *, #1100, .F. ) ;
#47947 = CARTESIAN_POINT ( 'NONE',  ( -2.925878650339476472, -77.50071622641024760, 8.775276054172831408 ) ) ;
#47948 = CARTESIAN_POINT ( 'NONE',  ( 8.680753609988000719, -77.61254516213799093, 6.821192461343000168 ) ) ;
#47949 = EDGE_CURVE ( 'NONE', #8361, #22144, #29137, .T. ) ;
#47950 = CARTESIAN_POINT ( 'NONE',  ( -12.66008999775999833, -61.42705329315000284, -1.387101471715999956 ) ) ;
#47951 = CARTESIAN_POINT ( 'NONE',  ( 8.898653440358000211, -78.54749933893899083, -3.871004561473999850 ) ) ;
#47952 = CARTESIAN_POINT ( 'NONE',  ( -3.684198380124665828, -86.09999999999978115, 1.557781209248828347 ) ) ;
#47953 = AXIS2_PLACEMENT_3D ( 'NONE', #43153, #29258, #20706 ) ;
#47954 = LINE ( 'NONE', #7485, #15303 ) ;
#47955 = CARTESIAN_POINT ( 'NONE',  ( -10.18491080493000212, -18.69283319134000010, 7.640030264154999529 ) ) ;
#47956 = CARTESIAN_POINT ( 'NONE',  ( -10.55592303174000079, -79.89804181175900055, -3.904632140253000205 ) ) ;
#47957 = CARTESIAN_POINT ( 'NONE',  ( -0.3011984493834000132, -79.59686628078000581, 1.556817658704999996 ) ) ;
#47958 = FACE_OUTER_BOUND ( 'NONE', #5298, .T. ) ;
#47959 = CARTESIAN_POINT ( 'NONE',  ( 6.635658238781000584, -78.32268667140098728, 7.210160158573999389 ) ) ;
#47960 = CARTESIAN_POINT ( 'NONE',  ( -5.687706977064000746, -78.11605038298799286, 10.54353137130999940 ) ) ;
#47961 = CARTESIAN_POINT ( 'NONE',  ( -10.36292447790000004, -18.79904187578000219, -7.633480004415999609 ) ) ;
#47962 = CARTESIAN_POINT ( 'NONE',  ( -2.062323307449999810, -18.77286846807999865, -12.83634826442999888 ) ) ;
#47963 = CARTESIAN_POINT ( 'NONE',  ( 12.00000000000000000, -23.25000000000000000, -1.250000000000000000 ) ) ;
#47964 = CARTESIAN_POINT ( 'NONE',  ( -10.55482845722999841, -80.40477481282198369, 3.343238611526999637 ) ) ;
#47965 = CARTESIAN_POINT ( 'NONE',  ( 10.33259770149999923, -77.60596644471499417, 4.480110411294999651 ) ) ;
#47966 = CARTESIAN_POINT ( 'NONE',  ( 12.50000000000000000, -24.68359816828999698, 1.003641515614000168 ) ) ;
#47967 = CARTESIAN_POINT ( 'NONE',  ( 12.50000000000000000, -18.75000000240999753, 1.750000000000000000 ) ) ;
#47968 = VERTEX_POINT ( 'NONE', #51050 ) ;
#47969 = CARTESIAN_POINT ( 'NONE',  ( 10.26995137457921636, -80.27463911791144824, 3.283750080291039986 ) ) ;
#47970 = CARTESIAN_POINT ( 'NONE',  ( -12.54238283049878788, -60.32853599783591392, 1.749799162368518513 ) ) ;
#47971 = CARTESIAN_POINT ( 'NONE',  ( 1.189217420461008423, -78.37516310198307679, 0.3845707844590672830 ) ) ;
#47972 = CARTESIAN_POINT ( 'NONE',  ( -2.445119831658000287, -3.656279784236000197, 2.430454651384000186 ) ) ;
#47973 = CARTESIAN_POINT ( 'NONE',  ( -12.61277494327999982, -55.60332099621999902, 1.798398135845999946 ) ) ;
#47974 = CARTESIAN_POINT ( 'NONE',  ( 0.3926218265389220807, -80.14583333333337123, -1.460959015002473382 ) ) ;
#47975 = CARTESIAN_POINT ( 'NONE',  ( 5.610847844242323745, -79.07500000000000284, -7.718163323371677542 ) ) ;
#47976 = VECTOR ( 'NONE', #17134, 999.9999999999998863 ) ;
#47977 = CARTESIAN_POINT ( 'NONE',  ( -11.00000000000000000, -77.21041666666667425, -1.439896632895322881 ) ) ;
#47978 = EDGE_CURVE ( 'NONE', #14764, #45494, #15355, .T. ) ;
#47979 = CARTESIAN_POINT ( 'NONE',  ( -14.00000000000000000, -5.899999999999999467, 0.000000000000000000 ) ) ;
#47980 = B_SPLINE_CURVE_WITH_KNOTS ( 'NONE', 3,
 ( #39103, #2812, #25236, #2524, #52686, #56539, #8099, #44120, #38813, #26095, #16100, #56830, #52116, #29936, #39675, #11676, #16386, #34371 ),
 .UNSPECIFIED., .F., .F.,
 ( 4, 2, 2, 2, 2, 2, 2, 2, 4 ),
 ( 0.000000000000000000, 0.1250000000000000833, 0.2500000000000001665, 0.3750000000000001665, 0.5000000000000002220, 0.6250000000000002220, 0.7500000000000001110, 0.8750000000000001110, 1.000000000000000000 ),
 .UNSPECIFIED. ) ;
#47981 = CARTESIAN_POINT ( 'NONE',  ( -10.15589153752000051, -77.33928062571699513, -4.371041081978999543 ) ) ;
#47982 = EDGE_CURVE ( 'NONE', #22708, #43698, #31955, .T. ) ;
#47983 = CARTESIAN_POINT ( 'NONE',  ( 7.575616321950742638, -76.38051645574682880, -8.984648930537860068 ) ) ;
#47984 = CARTESIAN_POINT ( 'NONE',  ( 6.163257195008000622, -78.38114111159998743, -9.114053931137998887 ) ) ;
#47985 = B_SPLINE_CURVE_WITH_KNOTS ( 'NONE', 3,
 ( #56521, #16080, #34061, #52099, #11656, #30786, #26074, #4232, #8658, #57958, #17512, #21933, #35503, #26644, #136, #53832, #53239, #13367 ),
 .UNSPECIFIED., .F., .F.,
 ( 4, 2, 2, 2, 2, 2, 2, 2, 4 ),
 ( 0.000000000000000000, 0.1250000000000000000, 0.2500000000000000000, 0.3750000000000000000, 0.5000000000000000000, 0.6250000000000000000, 0.7500000000000000000, 0.8750000000000000000, 1.000000000000000000 ),
 .UNSPECIFIED. ) ;
#47986 = CARTESIAN_POINT ( 'NONE',  ( 1.224722617583677176, -81.86616265547245064, 0.2496387431639754406 ) ) ;
#47987 = DIRECTION ( 'NONE',  ( -0.7071067811705844530, 1.925104039395958879E-07, -0.7071067812024844912 ) ) ;
#47988 = CARTESIAN_POINT ( 'NONE',  ( 5.491552160713999875, -77.03649626283258556, 7.961786551375001686 ) ) ;
#47989 = CARTESIAN_POINT ( 'NONE',  ( -5.684557159767977375, -78.42708333333332860, 7.396918292183154442 ) ) ;
#47990 = CARTESIAN_POINT ( 'NONE',  ( 1.439896632895286466, -77.46458333333332291, 11.00000000000000711 ) ) ;
#47991 = CARTESIAN_POINT ( 'NONE',  ( 5.974268513220012622, -80.27235878227935473, -8.936697743355807688 ) ) ;
#47992 = DIRECTION ( 'NONE',  ( 0.000000000000000000, 0.000000000000000000, 1.000000000000000000 ) ) ;
#47993 = CARTESIAN_POINT ( 'NONE',  ( -8.620934061270462578, -16.83470696675769673, -9.346030177896617275 ) ) ;
#47994 = ORIENTED_EDGE ( 'NONE', *, *, #1949, .F. ) ;
#47995 = CARTESIAN_POINT ( 'NONE',  ( 3.714552462503000196, -79.34833626489600533, 11.44155784250999908 ) ) ;
#47996 = DIRECTION ( 'NONE',  ( 1.000000000000000000, 0.000000000000000000, 0.000000000000000000 ) ) ;
#47997 = EDGE_CURVE ( 'NONE', #36547, #7212, #51338, .T. ) ;
#47998 = CARTESIAN_POINT ( 'NONE',  ( 10.09881335831000015, -79.03692200396399414, -4.984770136353999348 ) ) ;
#47999 = CARTESIAN_POINT ( 'NONE',  ( -1.072483829238511044, -81.25721727793691684, -0.9250620443464491194 ) ) ;
#48000 = ORIENTED_EDGE ( 'NONE', *, *, #54164, .F. ) ;
#48001 = CARTESIAN_POINT ( 'NONE',  ( 1.980584515756000030, -23.26485150094000076, 12.76303204340999997 ) ) ;
#48002 = ORIENTED_EDGE ( 'NONE', *, *, #33347, .F. ) ;
#48003 = ORIENTED_EDGE ( 'NONE', *, *, #31148, .F. ) ;
#48004 = DIRECTION ( 'NONE',  ( -1.000000000000000000, 0.000000000000000000, 0.000000000000000000 ) ) ;
#48005 = ORIENTED_EDGE ( 'NONE', *, *, #2953, .F. ) ;
#48006 = CARTESIAN_POINT ( 'NONE',  ( 3.342652169347999802, -81.08749251809699388, 1.179681212160999859 ) ) ;
#48007 = CARTESIAN_POINT ( 'NONE',  ( 4.262956496346735236, -79.23758755414554855, 8.489663765682541552 ) ) ;
#48008 = ORIENTED_EDGE ( 'NONE', *, *, #43881, .T. ) ;
#48009 = CARTESIAN_POINT ( 'NONE',  ( 0.2479148173105888420, -82.74134425127877535, -1.224891232295899801 ) ) ;
#48010 = ORIENTED_EDGE ( 'NONE', *, *, #5504, .T. ) ;
#48011 = CARTESIAN_POINT ( 'NONE',  ( -5.684557159767956058, -79.57291666666664298, -7.396918292183169541 ) ) ;
#48012 = VERTEX_POINT ( 'NONE', #16471 ) ;
#48013 = CARTESIAN_POINT ( 'NONE',  ( 0.8760958855005448465, -79.41347816698738882, 0.8914155223916401249 ) ) ;
#48014 = CARTESIAN_POINT ( 'NONE',  ( 0.000000000000000000, -23.94999999999946994, 12.00000000000000000 ) ) ;
#48015 = CARTESIAN_POINT ( 'NONE',  ( 4.976371158049889942, -79.80000000000001137, 10.82108306336006720 ) ) ;
#48016 = EDGE_CURVE ( 'NONE', #53695, #21736, #41778, .T. ) ;
#48017 = CARTESIAN_POINT ( 'NONE',  ( -10.20761871445822244, -80.07464919416229066, 3.371456631957987948 ) ) ;
#48018 = CARTESIAN_POINT ( 'NONE',  ( 9.250000000000000000, -77.74999999999998579, 0.000000000000000000 ) ) ;
#48019 = AXIS2_PLACEMENT_3D ( 'NONE', #25419, #26555, #44585 ) ;
#48020 = CARTESIAN_POINT ( 'NONE',  ( 3.308356911591940008, -86.39318692614399708, -1.472975398279134485 ) ) ;
#48021 = CARTESIAN_POINT ( 'NONE',  ( 7.778176538613999824, -76.52009807519600315, -8.035785801754000701 ) ) ;
#48022 = CARTESIAN_POINT ( 'NONE',  ( 11.91901974179999968, -77.28985072955998703, 5.468333046474000980 ) ) ;
#48023 = CARTESIAN_POINT ( 'NONE',  ( -11.00000000000000000, -78.69999999999998863, 0.000000000000000000 ) ) ;
#48024 = CARTESIAN_POINT ( 'NONE',  ( 9.963260314060999434, -76.67766803430798461, 4.924740193090999085 ) ) ;
#48025 = CARTESIAN_POINT ( 'NONE',  ( -9.134711892043656078, -78.61273296005398947, -1.455512071036835220 ) ) ;
#48026 = B_SPLINE_CURVE_WITH_KNOTS ( 'NONE', 3,
 ( #8346, #40223, #45254, #57647, #40522, #27216, #53513, #44360, #18093, #54105, #57941, #40815, #30766, #13349, #48799, #8060, #115, #31347 ),
 .UNSPECIFIED., .F., .F.,
 ( 4, 2, 2, 2, 2, 2, 2, 2, 4 ),
 ( 0.000000000000000000, 0.1250000000000000833, 0.2500000000000001110, 0.3750000000000000000, 0.4999999999999999445, 0.6249999999999998890, 0.7499999999999997780, 0.8749999999999998890, 1.000000000000000000 ),
 .UNSPECIFIED. ) ;
#48027 = CARTESIAN_POINT ( 'NONE',  ( 1.329937235669000017, -79.46596153841599630, -0.09921221311570001256 ) ) ;
#48028 = AXIS2_PLACEMENT_3D ( 'NONE', #28183, #5761, #1357 ) ;
#48029 = CARTESIAN_POINT ( 'NONE',  ( -10.99959862783280506, -80.10247156894594411, -0.2778054206351758815 ) ) ;
#48030 = CARTESIAN_POINT ( 'NONE',  ( -0.08333306579402115222, -2.977413547009986949, 3.248820096312940997 ) ) ;
#48031 = CARTESIAN_POINT ( 'NONE',  ( -3.453033859651000181, -78.47775883115959061, 0.4993677312671000457 ) ) ;
#48032 = ADVANCED_FACE ( 'NONE', ( #26183 ), #35024, .F. ) ;
#48033 = CARTESIAN_POINT ( 'NONE',  ( -2.524762559494834413, -77.99400743061801222, 10.44993185993495999 ) ) ;
#48034 = CIRCLE ( 'NONE', #9329, 11.75000000000000178 ) ;
#48035 = CARTESIAN_POINT ( 'NONE',  ( 0.6454797251240073086, -24.88806512139955984, -12.50471521368228167 ) ) ;
#48036 = CARTESIAN_POINT ( 'NONE',  ( -0.6682991597444000176, -84.35769503318799423, 3.483523875034000294 ) ) ;
#48037 = CARTESIAN_POINT ( 'NONE',  ( 3.542727183245000244, -3.002891436244000456, -1.391102635753999950 ) ) ;
#48038 = CARTESIAN_POINT ( 'NONE',  ( 10.18491068059999805, -18.69283065396999888, 7.640030139758000161 ) ) ;
#48039 = CARTESIAN_POINT ( 'NONE',  ( -9.636781270596999960, -61.24031362749000351, -7.948066289865000300 ) ) ;
#48040 = CARTESIAN_POINT ( 'NONE',  ( 9.500000000000000000, -78.14999999999999147, 0.000000000000000000 ) ) ;
#48041 = CARTESIAN_POINT ( 'NONE',  ( -0.05395919428434999693, -80.75611789099500015, -1.332567581519000122 ) ) ;
#48042 = DIRECTION ( 'NONE',  ( 0.000000000000000000, 1.000000000000000000, 0.000000000000000000 ) ) ;
#48043 = CARTESIAN_POINT ( 'NONE',  ( 7.287838312904000304, -78.22430371036000452, -10.78085041437000058 ) ) ;
#48044 = CARTESIAN_POINT ( 'NONE',  ( -2.169167664939000151, -78.20037715311599413, 10.75912301088999889 ) ) ;
#48045 = CARTESIAN_POINT ( 'NONE',  ( 0.6484536763440467144, -25.12402982711201105, -12.70397497891696226 ) ) ;
#48046 = CARTESIAN_POINT ( 'NONE',  ( -6.449220533167999925, -76.07628699674000927, -10.72226218736000014 ) ) ;
#48047 = ORIENTED_EDGE ( 'NONE', *, *, #7090, .T. ) ;
#48048 = EDGE_CURVE ( 'NONE', #50691, #38883, #41803, .T. ) ;
#48049 = FACE_OUTER_BOUND ( 'NONE', #30171, .T. ) ;
#48050 = CARTESIAN_POINT ( 'NONE',  ( 4.000000000000000000, -74.80000000000001137, 0.5999999999999999778 ) ) ;
#48051 = PRODUCT_DEFINITION_FORMATION_WITH_SPECIFIED_SOURCE ( 'ANY', '', #56856, .NOT_KNOWN. ) ;
#48052 = EDGE_CURVE ( 'NONE', #36787, #326, #25581, .T. ) ;
#48053 = CARTESIAN_POINT ( 'NONE',  ( 12.57434559700999976, -60.51110719467000365, 1.760800161976000089 ) ) ;
#48054 = CARTESIAN_POINT ( 'NONE',  ( -12.65371606323000009, -79.09322042626999405, -1.883862808345000195 ) ) ;
#48055 = CARTESIAN_POINT ( 'NONE',  ( 12.77301916222999800, -53.74808379519999590, -1.052060437763999934 ) ) ;
#48056 = CARTESIAN_POINT ( 'NONE',  ( -4.391285525405000278, -79.04379552517198704, -8.449082048777999177 ) ) ;
#48057 = CARTESIAN_POINT ( 'NONE',  ( 2.284771741974000125, -82.63025363959900460, 3.494189356575999827 ) ) ;
#48058 = CARTESIAN_POINT ( 'NONE',  ( 0.000000000000000000, -87.70000000000000284, 0.000000000000000000 ) ) ;
#48059 = CARTESIAN_POINT ( 'NONE',  ( -1.469401861277999988, -80.52594520594300320, -0.6692011555514000287 ) ) ;
#48060 = EDGE_LOOP ( 'NONE', ( #57913, #55454, #21116, #10009 ) ) ;
#48061 = CARTESIAN_POINT ( 'NONE',  ( 8.473210114131379811, -77.29736020677133013, -6.623708463630019416 ) ) ;
#48062 = CARTESIAN_POINT ( 'NONE',  ( 8.566298481405405951, -78.88243973942240927, 3.641100821265425669 ) ) ;
#48063 = AXIS2_PLACEMENT_3D ( 'NONE', #32025, #5180, #13144 ) ;
#48064 = CARTESIAN_POINT ( 'NONE',  ( -3.671083419894561217, -78.75032998289347574, -1.629121246791012778 ) ) ;
#48065 = ORIENTED_EDGE ( 'NONE', *, *, #18574, .F. ) ;
#48066 = CARTESIAN_POINT ( 'NONE',  ( 4.619608356761999879, -78.71112282211998945, 9.917007359391000421 ) ) ;
#48067 = CARTESIAN_POINT ( 'NONE',  ( 12.75763395696999858, -56.02204592290999585, 1.931043742978000077 ) ) ;
#48068 = ADVANCED_FACE ( 'NONE', ( #43052 ), #39756, .T. ) ;
#48069 = CARTESIAN_POINT ( 'NONE',  ( -7.171416948513999579, -80.31415055360498911, -8.914771748833000942 ) ) ;
#48070 = ORIENTED_EDGE ( 'NONE', *, *, #52887, .F. ) ;
#48071 = CARTESIAN_POINT ( 'NONE',  ( -3.600395895414000069, -77.65777409222799577, 11.61979689923000159 ) ) ;
#48072 = ORIENTED_EDGE ( 'NONE', *, *, #27832, .F. ) ;
#48073 = ORIENTED_EDGE ( 'NONE', *, *, #12623, .T. ) ;
#48074 = CIRCLE ( 'NONE', #51823, 10.40000000000000036 ) ;
#48075 = CARTESIAN_POINT ( 'NONE',  ( 0.6303254723250644176, -80.43299358135132593, 1.079794037324565581 ) ) ;
#48076 = CARTESIAN_POINT ( 'NONE',  ( 1.749722766153996911, -60.27588992799950063, 12.54673760685730954 ) ) ;
#48077 = CARTESIAN_POINT ( 'NONE',  ( -9.358268528169000788, -79.65327210978701089, -2.797054701638000296 ) ) ;
#48078 = ORIENTED_EDGE ( 'NONE', *, *, #27149, .F. ) ;
#48079 = ORIENTED_EDGE ( 'NONE', *, *, #19969, .T. ) ;
#48080 = CARTESIAN_POINT ( 'NONE',  ( -7.766269599678000013, -78.62042853322630265, -9.491266709826003733 ) ) ;
#48081 = CARTESIAN_POINT ( 'NONE',  ( 3.778552491320999795, -78.99318692756679638, -2.230001151765018008 ) ) ;
#48082 = CARTESIAN_POINT ( 'NONE',  ( 10.47840693000000023, -55.01310507149000273, 7.622759963108999948 ) ) ;
#48083 = FACE_OUTER_BOUND ( 'NONE', #5269, .T. ) ;
#48084 = CARTESIAN_POINT ( 'NONE',  ( 0.1963495408493571848, -78.26458333333334849, 1.500000000000000666 ) ) ;
#48085 = CARTESIAN_POINT ( 'NONE',  ( 9.392127196910033504, -77.39524328896870031, -7.218255399355257396 ) ) ;
#48086 = DIRECTION ( 'NONE',  ( -1.000000000000000000, 0.000000000000000000, 0.000000000000000000 ) ) ;
#48087 = CARTESIAN_POINT ( 'NONE',  ( 6.233047529871999615, -78.98050366622999263, 9.960502923565000444 ) ) ;
#48088 = CARTESIAN_POINT ( 'NONE',  ( 8.646211292720670016, -78.82120266248546159, -3.287401068500848567 ) ) ;
#48089 = CARTESIAN_POINT ( 'NONE',  ( -9.844172144369998989, -75.89675078460000179, 7.391061701651999272 ) ) ;
#48090 = CARTESIAN_POINT ( 'NONE',  ( -10.75000000000000000, -80.44999999999899387, 2.612557432076000154E-10 ) ) ;
#48091 = EDGE_CURVE ( 'NONE', #57578, #5899, #16328, .T. ) ;
#48092 = CARTESIAN_POINT ( 'NONE',  ( -7.396918292183192634, -77.94791666666667140, 5.684557159767932077 ) ) ;
#48093 = CARTESIAN_POINT ( 'NONE',  ( -12.54987159816999842, -16.94886760191999997, 0.1385534523823999942 ) ) ;
#48094 = CARTESIAN_POINT ( 'NONE',  ( -7.766269599678000013, -78.51842792576000818, -9.491266709826000181 ) ) ;
#48095 = CARTESIAN_POINT ( 'NONE',  ( 7.144724566336000393, -76.32390714479099358, 9.988770583665001368 ) ) ;
#48096 = CARTESIAN_POINT ( 'NONE',  ( -7.342331066867000544, -59.94999999967000548, -8.190859204290999784 ) ) ;
#48097 = DIRECTION ( 'NONE',  ( 0.000000000000000000, -1.000000000000000000, 0.000000000000000000 ) ) ;
#48098 = CARTESIAN_POINT ( 'NONE',  ( 1.504090402702771501, -80.99286779333345976, -0.1339503099265954567 ) ) ;
#48099 = CARTESIAN_POINT ( 'NONE',  ( -3.000000000000000000, -86.20000000000000284, 0.000000000000000000 ) ) ;
#48100 = DIRECTION ( 'NONE',  ( 0.000000000000000000, -1.000000000000000000, 0.000000000000000000 ) ) ;
#48101 = CARTESIAN_POINT ( 'NONE',  ( 6.365665562422999635, -78.73050366622999263, 10.17242851768000023 ) ) ;
#48102 = CARTESIAN_POINT ( 'NONE',  ( -3.161480484322999995, -3.525554798046000027, 1.254767625763999916 ) ) ;
#48103 = AXIS2_PLACEMENT_3D ( 'NONE', #45224, #18063, #57910 ) ;
#48104 = CARTESIAN_POINT ( 'NONE',  ( -5.292199200464000164, -77.59767930019499715, -10.82535908394999957 ) ) ;
#48105 = CARTESIAN_POINT ( 'NONE',  ( 0.1963495408493571015, -80.86458333333332860, 1.500000000000000444 ) ) ;
#48107 = FACE_OUTER_BOUND ( 'NONE', #20473, .T. ) ;
#48106 = CARTESIAN_POINT ( 'NONE',  ( -11.77140462957510714, -75.79999999999998295, 1.896298482247357198 ) ) ;
#48108 = CARTESIAN_POINT ( 'NONE',  ( -0.7208041749482999583, -83.11920712346199025, 1.412512638229999951 ) ) ;
#48109 = FACE_OUTER_BOUND ( 'NONE', #40493, .T. ) ;
#48110 = ORIENTED_EDGE ( 'NONE', *, *, #3751, .T. ) ;
#48111 = CARTESIAN_POINT ( 'NONE',  ( 0.1636246173744697330, -82.13541666666665719, -1.249999999999999778 ) ) ;
#48112 = CARTESIAN_POINT ( 'NONE',  ( 0.2390640603075999959, -79.56455645514600405, 12.03889950388999885 ) ) ;
#48113 = CARTESIAN_POINT ( 'NONE',  ( 2.925805176656314899, -79.39985491316186028, -9.059708552875285648 ) ) ;
#48114 = EDGE_CURVE ( 'NONE', #36712, #3531, #55930, .T. ) ;
#48115 = CARTESIAN_POINT ( 'NONE',  ( 1.491917775262641577, -79.99999999999997158, -9.368459166867951993 ) ) ;
#48116 = CARTESIAN_POINT ( 'NONE',  ( -5.449838856306469026, -76.22708333364460032, -9.457243427908759159 ) ) ;
#48117 = CARTESIAN_POINT ( 'NONE',  ( -3.055517426832999650, -0.5241180847798000420, 0.7952000566461999709 ) ) ;
#48118 = CARTESIAN_POINT ( 'NONE',  ( -1.318181353051000038, -80.15644912722899562, 9.802870741655000941 ) ) ;
#48119 = DIRECTION ( 'NONE',  ( 0.9957542233430587419, 0.04890176636653797981, 0.07798810127637677281 ) ) ;
#48120 = CARTESIAN_POINT ( 'NONE',  ( -11.59999999999999964, -87.70000000000000284, 0.000000000000000000 ) ) ;
#48121 = ORIENTED_EDGE ( 'NONE', *, *, #3071, .F. ) ;
#48122 = DIRECTION ( 'NONE',  ( 0.000000000000000000, 1.000000000000000000, 0.000000000000000000 ) ) ;
#48123 = CARTESIAN_POINT ( 'NONE',  ( 7.514114347650544978, -79.22981446509285774, -9.060189168767688983 ) ) ;
#48124 = CARTESIAN_POINT ( 'NONE',  ( 9.019414222045478269, -24.99291943955440942, -8.666941068747364696 ) ) ;
#48125 = CARTESIAN_POINT ( 'NONE',  ( -10.42272502865000128, -57.04546192861999998, -7.691893942748999180 ) ) ;
#48126 = CARTESIAN_POINT ( 'NONE',  ( -1.630114970985000022, -79.78691820467999207, -0.3434887894992000312 ) ) ;
#48127 = ADVANCED_FACE ( 'NONE', ( #12324 ), #30311, .F. ) ;
#48128 = ORIENTED_EDGE ( 'NONE', *, *, #2194, .T. ) ;
#48129 = AXIS2_PLACEMENT_3D ( 'NONE', #44714, #8691, #4268 ) ;
#48130 = CARTESIAN_POINT ( 'NONE',  ( -8.613561821356000792, -77.48351239614198960, -7.003728345069999861 ) ) ;
#48131 = CARTESIAN_POINT ( 'NONE',  ( -0.9994139296504542802, -82.15273062190185271, -0.7675533749920089299 ) ) ;
#48132 = CARTESIAN_POINT ( 'NONE',  ( 1.931043762602999925, -59.57819125629999490, -12.75761570869000039 ) ) ;
#48133 = EDGE_CURVE ( 'NONE', #55386, #10196, #8022, .T. ) ;
#48134 = CARTESIAN_POINT ( 'NONE',  ( -12.64500484464000074, -56.02847221959000024, 1.799490225533999732 ) ) ;
#48135 = CARTESIAN_POINT ( 'NONE',  ( -10.69999999999999929, -81.79999999999998295, 0.000000000000000000 ) ) ;
#48136 = CARTESIAN_POINT ( 'NONE',  ( 0.000000000000000000, -77.59999999938000315, -2.399999999383999771 ) ) ;
#48137 = ORIENTED_EDGE ( 'NONE', *, *, #51329, .F. ) ;
#48138 = ORIENTED_EDGE ( 'NONE', *, *, #45154, .F. ) ;
#48139 = CARTESIAN_POINT ( 'NONE',  ( -12.58344645258000050, -76.32431866488499850, 0.3593549516198999982 ) ) ;
#48140 = APPLICATION_CONTEXT ( 'automotive_design' ) ;
#48141 = CARTESIAN_POINT ( 'NONE',  ( 0.2431151423990842164, -78.72686878867834537, -10.74764302140133765 ) ) ;
#48142 = ORIENTED_EDGE ( 'NONE', *, *, #4950, .F. ) ;
#48143 = CARTESIAN_POINT ( 'NONE',  ( 10.36222501930000028, -18.77880030165999869, 7.631889976314999657 ) ) ;
#48144 = CIRCLE ( 'NONE', #52842, 10.50000000000000000 ) ;
#48145 = CARTESIAN_POINT ( 'NONE',  ( -1.439896632895359962, -77.58541666666667425, 10.99999999999999645 ) ) ;
#48146 = EDGE_CURVE ( 'NONE', #44548, #32213, #53999, .T. ) ;
#48147 = CARTESIAN_POINT ( 'NONE',  ( 1.501534314742096310, -54.24847048308878072, 12.70455943736382132 ) ) ;
#48148 = CARTESIAN_POINT ( 'NONE',  ( -12.76493461869000079, -78.17433021234000989, -0.9303755367166000045 ) ) ;
#48149 = DIRECTION ( 'NONE',  ( 0.000000000000000000, -1.000000000000000000, 0.000000000000000000 ) ) ;
#48150 = DIRECTION ( 'NONE',  ( 1.000000000000000000, 0.000000000000000000, 0.000000000000000000 ) ) ;
#48151 = CARTESIAN_POINT ( 'NONE',  ( -0.1963495408493673433, -79.88541666666667140, 1.499999999999999334 ) ) ;
#48152 = CARTESIAN_POINT ( 'NONE',  ( 8.733858618705999888, -78.59770491346299082, -7.038306768505999678 ) ) ;
#48153 = CARTESIAN_POINT ( 'NONE',  ( 1.225466286858300391, -79.96494772406065010, 9.168303427177114884 ) ) ;
#48154 = ORIENTED_EDGE ( 'NONE', *, *, #3416, .F. ) ;
#48155 = CARTESIAN_POINT ( 'NONE',  ( 1.129552310421328976, -78.16734973423666588, 11.73990984186074016 ) ) ;
#48156 = EDGE_LOOP ( 'NONE', ( #31833, #12970, #40277, #3119, #19929, #16843, #48531, #53198, #11694, #50478, #3617 ) ) ;
#48157 = CARTESIAN_POINT ( 'NONE',  ( 11.02792952375000013, -79.35441578277699648, -2.305147454016000186 ) ) ;
#48158 = CARTESIAN_POINT ( 'NONE',  ( 8.300692004267670399, -77.31357384288631351, -4.110348182662033167 ) ) ;
#48159 = CARTESIAN_POINT ( 'NONE',  ( 0.5499573741622000300, -79.64061393252499954, 1.306754138290999956 ) ) ;
#48160 = CARTESIAN_POINT ( 'NONE',  ( 7.342331066867000544, -55.64999999967000122, -8.190859204290999784 ) ) ;
#48162 = EDGE_CURVE ( 'NONE', #41200, #20196, #4472, .T. ) ;
#48161 = CARTESIAN_POINT ( 'NONE',  ( -0.2007418666109000160, -78.16174741493239253, -1.502878855747000086 ) ) ;
#48163 = CARTESIAN_POINT ( 'NONE',  ( -0.5999999998848000171, -18.85000000520999919, 11.79999999988000070 ) ) ;
#48164 = CYLINDRICAL_SURFACE ( 'NONE', #30402, 1.250000000000000000 ) ;
#48165 = CARTESIAN_POINT ( 'NONE',  ( -8.796335266380006956, -78.54791666666665151, 6.760013919724027431 ) ) ;
#48166 = DIRECTION ( 'NONE',  ( 0.000000000000000000, -1.000000000000000000, 0.000000000000000000 ) ) ;
#48167 = DIRECTION ( 'NONE',  ( 0.000000000000000000, -1.000000000000000000, 0.000000000000000000 ) ) ;
#48168 = EDGE_CURVE ( 'NONE', #57192, #12818, #53054, .T. ) ;
#48169 = CARTESIAN_POINT ( 'NONE',  ( 0.1312417595986999919, -79.43100181365798562, 11.15680847095000061 ) ) ;
#48170 = DIRECTION ( 'NONE',  ( -0.4045849535019032661, -0.8201353734596047440, 0.4045849535019032661 ) ) ;
#48171 = CARTESIAN_POINT ( 'NONE',  ( 8.485281374238999419, -55.54999999966999980, 8.485281374238999419 ) ) ;
#48172 = LINE ( 'NONE', #34553, #20619 ) ;
#48173 = CARTESIAN_POINT ( 'NONE',  ( 1.925977698187999909, -85.23083017214499080, -2.979122324201999739 ) ) ;
#48174 = ORIENTED_EDGE ( 'NONE', *, *, #53542, .T. ) ;
#48175 = CARTESIAN_POINT ( 'NONE',  ( -1.596184505169000012, -82.35834473437999748, -0.5933059756569000198 ) ) ;
#48176 = CARTESIAN_POINT ( 'NONE',  ( 0.8987165921316000450, -79.72039037689999930, 1.306408957324000086 ) ) ;
#48177 = CARTESIAN_POINT ( 'NONE',  ( 0.000000000000000000, -74.64999999999999147, 0.000000000000000000 ) ) ;
#48178 = CARTESIAN_POINT ( 'NONE',  ( 1.720939166139000109, -77.20276623428699736, -11.69973432676000158 ) ) ;
#48179 = CARTESIAN_POINT ( 'NONE',  ( 9.500000000000000000, -78.14999999999999147, 0.000000000000000000 ) ) ;
#48180 = CARTESIAN_POINT ( 'NONE',  ( -1.374853770045000090, -81.25000091166998573, -0.7192078502473999713 ) ) ;
#48181 = CARTESIAN_POINT ( 'NONE',  ( -3.256586129738097135, -1.781125447738561851, -1.344250386147469500 ) ) ;
#48182 = CARTESIAN_POINT ( 'NONE',  ( -7.603664017118000551, -78.57650194988499948, 6.060370778711000384 ) ) ;
#48183 = CARTESIAN_POINT ( 'NONE',  ( 8.875952806245999582, -78.91941197858199075, 3.056903470501999731 ) ) ;
#48184 = CARTESIAN_POINT ( 'NONE',  ( -5.871863728900494905, -86.10000000000019327, -4.829204525511367585 ) ) ;
#48185 = CARTESIAN_POINT ( 'NONE',  ( 8.485281374238999419, -55.54999999966999980, 8.485281374238999419 ) ) ;
#48186 = CARTESIAN_POINT ( 'NONE',  ( 9.850786281789762455, -75.99584267488174305, 6.405190026801080627 ) ) ;
#48187 = CARTESIAN_POINT ( 'NONE',  ( 1.157688070529184321, -81.43455268099248201, 0.5329657265460440163 ) ) ;
#48188 = ORIENTED_EDGE ( 'NONE', *, *, #36608, .F. ) ;
#48189 = DIRECTION ( 'NONE',  ( -1.000000000000000000, 0.000000000000000000, 0.000000000000000000 ) ) ;
#48190 = CARTESIAN_POINT ( 'NONE',  ( 1.199500263597268246, -79.20208333333333428, 0.9218200799623752495 ) ) ;
#48191 = CARTESIAN_POINT ( 'NONE',  ( 9.537121434155222843, -78.89952835878608539, -6.926593624396411464 ) ) ;
#48192 = CARTESIAN_POINT ( 'NONE',  ( 0.000000000000000000, -74.99999999999998579, -4.799999999999999822 ) ) ;
#48193 = CARTESIAN_POINT ( 'NONE',  ( 0.8286895765316001361, -81.66317656325999508, 1.445177540541999983 ) ) ;
#48194 = VECTOR ( 'NONE', #26884, 1000.000000000000000 ) ;
#48195 = CARTESIAN_POINT ( 'NONE',  ( 4.634563706678000550, -78.71015774810999233, 9.949112313689999709 ) ) ;
#48196 = CARTESIAN_POINT ( 'NONE',  ( 10.36292431357999888, -23.20096201633999655, -7.633479737313000335 ) ) ;
#48197 = CARTESIAN_POINT ( 'NONE',  ( -8.623051981844785274, -80.41744791666556580, 6.625779411460311685 ) ) ;
#48198 = CARTESIAN_POINT ( 'NONE',  ( 9.414259929411999295, -76.63483834893800406, -8.050387765842000221 ) ) ;
#48199 = CARTESIAN_POINT ( 'NONE',  ( 5.943163592195922718, -78.53230635707669194, 10.13577355096580668 ) ) ;
#48200 = CARTESIAN_POINT ( 'NONE',  ( -10.25201842922365358, -60.92180395180005092, 7.730408553586130438 ) ) ;
#48201 = ORIENTED_EDGE ( 'NONE', *, *, #14831, .F. ) ;
#48202 = VECTOR ( 'NONE', #13187, 1000.000000000000114 ) ;
#48203 = CARTESIAN_POINT ( 'NONE',  ( 7.861046360898000351, -79.52157567883000411, 7.903072230637000040 ) ) ;
#48204 = CARTESIAN_POINT ( 'NONE',  ( 6.026835113838189706, -77.31868998740377208, 7.054302318249272119 ) ) ;
#48205 = CARTESIAN_POINT ( 'NONE',  ( 8.082524092276869965, -78.20833333333330017, -4.658475568430838543 ) ) ;
#48206 = CARTESIAN_POINT ( 'NONE',  ( -11.07910306079999962, -79.19371210375499004, -2.045094064781999954 ) ) ;
#48207 = DIRECTION ( 'NONE',  ( -1.000000000000000000, 0.000000000000000000, -3.332495962870000189E-11 ) ) ;
#48208 = CARTESIAN_POINT ( 'NONE',  ( 8.909545442949999838, -57.79999999967000690, 7.919595949288999570 ) ) ;
#48209 = DIRECTION ( 'NONE',  ( -0.7071067811865474617, 0.000000000000000000, 0.7071067811865474617 ) ) ;
#48210 = CARTESIAN_POINT ( 'NONE',  ( 1.098001230595262445, -82.66109697007367174, 1.088914393985984885 ) ) ;
#48211 = CARTESIAN_POINT ( 'NONE',  ( -0.3740291581177058733, -79.70132840708080835, -1.192537797324159099 ) ) ;
#48212 = B_SPLINE_CURVE_WITH_KNOTS ( 'NONE', 3,
 ( #43574, #8713, #11993, #26704, #34976, #52721, #53006, #57144, #56860, #44735, #8133, #26134, #3137, #7556, #12557, #43870, #7841, #39428 ),
 .UNSPECIFIED., .F., .F.,
 ( 4, 2, 2, 2, 2, 2, 2, 2, 4 ),
 ( 0.000000000000000000, 0.1250000000000000833, 0.2500000000000001110, 0.3750000000000001110, 0.5000000000000001110, 0.6250000000000001110, 0.7500000000000000000, 0.8750000000000000000, 1.000000000000000000 ),
 .UNSPECIFIED. ) ;
#48213 = DIRECTION ( 'NONE',  ( 0.6489586447433830507, 0.04890182323489870864, -0.7592504784964801967 ) ) ;
#48214 = CARTESIAN_POINT ( 'NONE',  ( 1.667916687244999974, -18.70150862776000267, 12.49168433580000048 ) ) ;
#48215 = SHAPE_REPRESENTATION_RELATIONSHIP ( 'NONE' , 'NONE' ,  #52046, #44024 ) ;
#48216 = CARTESIAN_POINT ( 'NONE',  ( -12.46083365854999769, -23.68341615479999973, 1.628972628240999976 ) ) ;
#48217 = ORIENTED_EDGE ( 'NONE', *, *, #43394, .T. ) ;
#48218 = ORIENTED_EDGE ( 'NONE', *, *, #34951, .F. ) ;
#48219 = CIRCLE ( 'NONE', #22735, 12.50000000000000000 ) ;
#48220 = CARTESIAN_POINT ( 'NONE',  ( -7.648026766735999793, -23.25000000582000226, 10.12290050089000104 ) ) ;
#48221 = ORIENTED_EDGE ( 'NONE', *, *, #27046, .F. ) ;
#48222 = CARTESIAN_POINT ( 'NONE',  ( 9.494981342583157513, -79.50754469819568726, 0.9006174050536093212 ) ) ;
#48223 = ORIENTED_EDGE ( 'NONE', *, *, #9369, .F. ) ;
#48224 = CARTESIAN_POINT ( 'NONE',  ( -9.611543720960897375, -81.00000000000001421, -4.953819405574181545 ) ) ;
#48225 = CARTESIAN_POINT ( 'NONE',  ( -2.247674004742000076, -77.46491181672199389, 10.68285203299000052 ) ) ;
#48226 = CARTESIAN_POINT ( 'NONE',  ( 8.163677614451000153, -78.11386001420198966, 4.925422544966999716 ) ) ;
#48227 = EDGE_CURVE ( 'NONE', #53705, #12208, #20672, .T. ) ;
#48228 = DIRECTION ( 'NONE',  ( 0.7071067811865474617, 0.7071067811865474617, -9.196969555969614050E-11 ) ) ;
#48229 = VERTEX_POINT ( 'NONE', #17924 ) ;
#48230 = ORIENTED_EDGE ( 'NONE', *, *, #36282, .T. ) ;
#48231 = CARTESIAN_POINT ( 'NONE',  ( -6.574272315842624614, -77.53807528016541539, 6.506900208772002259 ) ) ;
#48232 = CARTESIAN_POINT ( 'NONE',  ( 9.507661145905998978, -77.51711603614198509, -5.611464101879999333 ) ) ;
#48233 = CARTESIAN_POINT ( 'NONE',  ( -12.54715528154999937, -61.33180535358000185, -1.292252957172000061 ) ) ;
#48234 = CARTESIAN_POINT ( 'NONE',  ( -7.456816947376000648, -78.77488997197099252, 6.210200510404999541 ) ) ;
#48235 = FACE_OUTER_BOUND ( 'NONE', #34427, .T. ) ;
#48236 = DIRECTION ( 'NONE',  ( 0.000000000000000000, 1.000000000000000000, 0.000000000000000000 ) ) ;
#48237 = CARTESIAN_POINT ( 'NONE',  ( 7.770365053994759741, -54.56417299442668423, -10.20675369723379156 ) ) ;
#48238 = CARTESIAN_POINT ( 'NONE',  ( -7.054457466615000172, -80.38063403548999020, -8.769379688592000122 ) ) ;
#48239 = EDGE_CURVE ( 'NONE', #13840, #21227, #49514, .T. ) ;
#48240 = CARTESIAN_POINT ( 'NONE',  ( 12.61277494329999982, -18.80332099654000189, -1.798398135845000079 ) ) ;
#48241 = CARTESIAN_POINT ( 'NONE',  ( -1.750000000000000000, -55.54999999966999980, 12.00000000000000000 ) ) ;
#48242 = CARTESIAN_POINT ( 'NONE',  ( -10.71456977360709928, -76.66589582642508560, 4.824031268171789399 ) ) ;
#48243 = ORIENTED_EDGE ( 'NONE', *, *, #39099, .F. ) ;
#48244 = CARTESIAN_POINT ( 'NONE',  ( -7.660411364605000273, -55.60826384781999820, 10.01752038681999935 ) ) ;
#48245 = CARTESIAN_POINT ( 'NONE',  ( 6.444980599754999595, -77.87188654417400357, -10.09843005143000028 ) ) ;
#48246 = CARTESIAN_POINT ( 'NONE',  ( -9.523369619462000557, -17.18054357685999989, -8.220347091616000412 ) ) ;
#48248 = DIRECTION ( 'NONE',  ( -1.000000000000000000, 0.000000000000000000, 0.000000000000000000 ) ) ;
#48247 = CARTESIAN_POINT ( 'NONE',  ( 2.980315163536433332, -78.44898908488615064, 8.777200079706965141 ) ) ;
#48249 = CARTESIAN_POINT ( 'NONE',  ( 2.841157093317593141, -1.309822438106574616, -1.639539360290898307 ) ) ;
#48250 = EDGE_CURVE ( 'NONE', #22264, #23504, #54232, .T. ) ;
#48251 = CARTESIAN_POINT ( 'NONE',  ( -3.491544874602000359, -78.49078379918199744, -10.58601217070000189 ) ) ;
#48252 = CARTESIAN_POINT ( 'NONE',  ( -4.659120039122103485, -79.68376931176990752, -8.083663002107071449 ) ) ;
#48253 = CARTESIAN_POINT ( 'NONE',  ( 8.796335266379964324, -80.00208333333898736, 6.760013919724087827 ) ) ;
#48254 = EDGE_LOOP ( 'NONE', ( #25025, #34025, #9234 ) ) ;
#48255 = LINE ( 'NONE', #15785, #37623 ) ;
#48256 = EDGE_CURVE ( 'NONE', #47291, #27444, #4033, .T. ) ;
#48257 = DIRECTION ( 'NONE',  ( -2.044813970925000100E-13, 0.000000000000000000, 1.000000000000000000 ) ) ;
#48258 = DIRECTION ( 'NONE',  ( -0.3090169943750105119, 0.000000000000000000, -0.9510565162951329921 ) ) ;
#48259 = B_SPLINE_CURVE_WITH_KNOTS ( 'NONE', 3,
 ( #7486, #42351, #20489, #47086, #52366, #11350, #6322, #52081, #51795, #42932, #29046, #43217, #20773, #51216, #42637, #2204, #46797, #47669 ),
 .UNSPECIFIED., .F., .F.,
 ( 4, 2, 2, 2, 2, 2, 2, 2, 4 ),
 ( 0.000000000000000000, 0.1249999999999999722, 0.2500000000000000000, 0.3750000000000000000, 0.5000000000000001110, 0.6250000000000001110, 0.7500000000000000000, 0.8750000000000000000, 1.000000000000000000 ),
 .UNSPECIFIED. ) ;
#48260 = CARTESIAN_POINT ( 'NONE',  ( -3.784563998892999770, -3.226994571379000032, -0.4035839726128000460 ) ) ;
#48261 = STYLED_ITEM ( 'NONE', ( #24010 ), #34903 ) ;
#48262 = CARTESIAN_POINT ( 'NONE',  ( 8.365650024713001898, -79.80890222813398793, 4.340751507912000484 ) ) ;
#48263 = CARTESIAN_POINT ( 'NONE',  ( -12.43647099676999979, -53.88193128055999637, -0.03491583288326999962 ) ) ;
#48264 = CARTESIAN_POINT ( 'NONE',  ( 5.766697267524079962, -77.26874999999996874, -9.406996941509154553 ) ) ;
#48265 = CARTESIAN_POINT ( 'NONE',  ( -2.598938867667634156, -2.049404340733311347, 1.996446441638521030 ) ) ;
#48266 = CARTESIAN_POINT ( 'NONE',  ( 9.500000000000000000, -79.14999999999999147, 0.000000000000000000 ) ) ;
#48267 = CARTESIAN_POINT ( 'NONE',  ( 3.270789807158999807, -85.87746544543099958, 1.847510159297000021 ) ) ;
#48268 = CARTESIAN_POINT ( 'NONE',  ( 6.760013919724077169, -77.37708333333333144, -8.796335266379971429 ) ) ;
#48269 = CARTESIAN_POINT ( 'NONE',  ( -2.946080165379000082, -77.91047479902398720, -10.65686345704000004 ) ) ;
#48270 = CARTESIAN_POINT ( 'NONE',  ( 10.83581499240337997, -76.41815442928682955, -4.543561087761390560 ) ) ;
#48271 = CARTESIAN_POINT ( 'NONE',  ( -4.457153411444000568, -77.23303910811499406, -10.09135857296999994 ) ) ;
#48272 = CARTESIAN_POINT ( 'NONE',  ( 0.8795903431313560894, -81.91347361793080495, 0.8876339888831865643 ) ) ;
#48273 = CARTESIAN_POINT ( 'NONE',  ( -3.251154051729839178, -1.100857096137070279, 2.995606203745920413E-05 ) ) ;
#48274 = CARTESIAN_POINT ( 'NONE',  ( -9.467475792354999697, -77.19315246464168467, 1.978357023055999919 ) ) ;
#48275 = CARTESIAN_POINT ( 'NONE',  ( 5.645287065787000458, -79.33454415034599094, 7.708789581145000014 ) ) ;
#48276 = CARTESIAN_POINT ( 'NONE',  ( -2.879226727952121756, -77.49583333333333712, 10.71369944335146407 ) ) ;
#48277 = CARTESIAN_POINT ( 'NONE',  ( 2.326191296373886885, -80.24266891153970960, -10.49546658612705841 ) ) ;
#48278 = CARTESIAN_POINT ( 'NONE',  ( 0.000000000000000000, -76.75499999999999545, 0.000000000000000000 ) ) ;
#48279 = CARTESIAN_POINT ( 'NONE',  ( -6.206331755963327090, -79.77156576277585032, 9.343610388852424009 ) ) ;
#48280 = CARTESIAN_POINT ( 'NONE',  ( -11.22206352833000054, -79.52763804998100738, -4.332716936452000844 ) ) ;
#48281 = CARTESIAN_POINT ( 'NONE',  ( -0.9995866622284782510, -78.15219033508832069, -0.7680681559914127599 ) ) ;
#48282 = CARTESIAN_POINT ( 'NONE',  ( -4.169330562119000660, -79.41823080598898343, -10.46186633551000078 ) ) ;
#48283 = CARTESIAN_POINT ( 'NONE',  ( -10.99999999999999467, -23.74999999999998934, -0.1603812274926581793 ) ) ;
#48284 = ORIENTED_EDGE ( 'NONE', *, *, #11379, .T. ) ;
#48285 = CARTESIAN_POINT ( 'NONE',  ( -1.931736162947090385, -23.76670395714575790, 12.72978979890153362 ) ) ;
#48286 = ORIENTED_EDGE ( 'NONE', *, *, #31298, .F. ) ;
#48287 = EDGE_LOOP ( 'NONE', ( #33864, #34221, #7037, #47144 ) ) ;
#48288 = PLANE ( 'NONE',  #39525 ) ;
#48289 = EDGE_LOOP ( 'NONE', ( #48230, #55765, #44062, #24737 ) ) ;
#48290 = CARTESIAN_POINT ( 'NONE',  ( -3.478405327321000051, -78.80273445295348722, -0.6821537367355999804 ) ) ;
#48291 = CARTESIAN_POINT ( 'NONE',  ( -6.738130626923404698, -79.33754562427129997, 6.696801847776262306 ) ) ;
#48292 = VERTEX_POINT ( 'NONE', #45385 ) ;
#48293 = CARTESIAN_POINT ( 'NONE',  ( -12.19527860736999969, -78.51856776420000017, -2.001746843535999965 ) ) ;
#48294 = CARTESIAN_POINT ( 'NONE',  ( -2.421167930323333106, -79.60416666666665719, -9.009247259181917045 ) ) ;
#48295 = ORIENTED_EDGE ( 'NONE', *, *, #23059, .T. ) ;
#48296 = DIRECTION ( 'NONE',  ( -1.000000000000000000, 0.000000000000000000, 0.000000000000000000 ) ) ;
#48297 = LINE ( 'NONE', #22791, #39688 ) ;
#48298 = CARTESIAN_POINT ( 'NONE',  ( -4.834103127707872538, -80.01221937575003551, 9.601684949764214494 ) ) ;
#48299 = LINE ( 'NONE', #43867, #44708 ) ;
#48300 = CARTESIAN_POINT ( 'NONE',  ( -3.929996950240798093, -86.12609999968209706, -0.3761983785355073051 ) ) ;
#48301 = CARTESIAN_POINT ( 'NONE',  ( 11.09875712452000052, -76.09370506138100154, 1.375294608629999971 ) ) ;
#48302 = CARTESIAN_POINT ( 'NONE',  ( -1.273906987915999878, -77.62287857533000590, -13.05154622979999957 ) ) ;
#48303 = EDGE_CURVE ( 'NONE', #28385, #22487, #40944, .T. ) ;
#48304 = CARTESIAN_POINT ( 'NONE',  ( 2.879226727952050258, -78.55416666666667425, 10.71369944335148361 ) ) ;
#48305 = B_SPLINE_CURVE_WITH_KNOTS ( 'NONE', 3,
 ( #8353, #44370, #16647, #8067, #16361, #3356, #8649, #21924, #2782, #53230, #34631, #11931, #48247, #26635, #39367, #52659, #57374, #52377, #29908, #25493 ),
 .UNSPECIFIED., .F., .F.,
 ( 4, 2, 2, 2, 2, 2, 2, 2, 2, 4 ),
 ( 0.000000000000000000, 0.1250000000000000555, 0.2500000000000000555, 0.3750000000000001665, 0.5000000000000002220, 0.5625000000000002220, 0.6250000000000002220, 0.7500000000000002220, 0.8750000000000001110, 1.000000000000000000 ),
 .UNSPECIFIED. ) ;
#48306 = CARTESIAN_POINT ( 'NONE',  ( 1.536913952029000052, -76.52717638237299980, -11.00715755867000034 ) ) ;
#48307 = CARTESIAN_POINT ( 'NONE',  ( -10.18496935385000057, -21.75064714707999869, 7.710095619702999947 ) ) ;
#48308 = CARTESIAN_POINT ( 'NONE',  ( 2.442089561480999649, -82.53821485768798993, -3.121279332836000009 ) ) ;
#48309 = AXIS2_PLACEMENT_3D ( 'NONE', #8711, #32006, #50048 ) ;
#48310 = CARTESIAN_POINT ( 'NONE',  ( -10.29238134969365959, -80.12908025125918243, -3.880928803044727982 ) ) ;
#48311 = CARTESIAN_POINT ( 'NONE',  ( 2.286833087265501163, -2.913422680531678743, 2.308828009290456951 ) ) ;
#48312 = CARTESIAN_POINT ( 'NONE',  ( 2.211827365938999979, -82.04517549782597996, -2.826962668278000024 ) ) ;
#48313 = CARTESIAN_POINT ( 'NONE',  ( -13.99609303101000002, -32.95862266598000190, -3.303296643088999776E-05 ) ) ;
#48314 = CARTESIAN_POINT ( 'NONE',  ( -3.514734140608999802, -83.15519503318799366, 0.4777095056862999400 ) ) ;
#48315 = CARTESIAN_POINT ( 'NONE',  ( -0.4587696627765999735, -3.398051649099999683, -3.778272981138000031 ) ) ;
#48316 = CARTESIAN_POINT ( 'NONE',  ( 1.251999141562743167, -80.48525731161612384, -0.2411094176575541426 ) ) ;
#48317 = CARTESIAN_POINT ( 'NONE',  ( 10.75000000000000000, -80.25000000000000000, -1.651583051307000043E-14 ) ) ;
#48318 = CONICAL_SURFACE ( 'NONE', #253, 10.29999999923999887, 0.7853981633972997312 ) ;
#48319 = ADVANCED_FACE ( 'NONE', ( #10825 ), #9939, .T. ) ;
#48320 = DIRECTION ( 'NONE',  ( 0.7071067811865474617, -0.7071067811865474617, 3.646357685208241723E-10 ) ) ;
#48321 = CARTESIAN_POINT ( 'NONE',  ( -1.321095329625999959, -82.14527134566500877, -0.1826337427822999904 ) ) ;
#48322 = CARTESIAN_POINT ( 'NONE',  ( -12.65989785480000229, -17.05665906540999899, -0.9744897697751000454 ) ) ;
#48323 = CARTESIAN_POINT ( 'NONE',  ( 12.49837680049000177, -23.20957148803000081, 1.667051419334999895 ) ) ;
#48324 = CARTESIAN_POINT ( 'NONE',  ( 6.760013919724077169, -79.87708333333333144, -8.796335266379971429 ) ) ;
#48325 = CARTESIAN_POINT ( 'NONE',  ( 1.423904377506817864, -24.30512805201019688, -12.50677628656594642 ) ) ;
#48326 = CARTESIAN_POINT ( 'NONE',  ( -8.784096368091999452, -76.01934928261999858, 8.698479859056998720 ) ) ;
#48327 = ORIENTED_EDGE ( 'NONE', *, *, #24901, .F. ) ;
#48328 = AXIS2_PLACEMENT_3D ( 'NONE', #20797, #16376, #3658 ) ;
#48329 = CARTESIAN_POINT ( 'NONE',  ( -9.497662397991334160, -77.28501590207432059, -0.2008463566140032963 ) ) ;
#48330 = CARTESIAN_POINT ( 'NONE',  ( 4.999999999872000167, -80.49999999987198862, -4.857398774947999725E-10 ) ) ;
#48331 = CARTESIAN_POINT ( 'NONE',  ( -0.8205178898083000938, -80.81311342771999762, -1.021985690358000243 ) ) ;
#48332 = CARTESIAN_POINT ( 'NONE',  ( 1.570796326794910547, -79.03541666666664867, -11.99999999999999822 ) ) ;
#48333 = CARTESIAN_POINT ( 'NONE',  ( 8.875952806245999582, -79.23328771936498072, 3.056903470501999731 ) ) ;
#48334 = CARTESIAN_POINT ( 'NONE',  ( 2.265335474502999880, -85.22456467766599530, -3.504044460248999737 ) ) ;
#48335 = CARTESIAN_POINT ( 'NONE',  ( 4.280065084278556142, -79.94253482840156266, 9.861166758580704794 ) ) ;
#48336 = CARTESIAN_POINT ( 'NONE',  ( -0.1931516691869999969, -80.43247902352800338, 1.503874604587000174 ) ) ;
#48337 = ADVANCED_FACE ( 'NONE', ( #19918 ), #21277, .F. ) ;
#48338 = VERTEX_POINT ( 'NONE', #51510 ) ;
#48339 = LINE ( 'NONE', #30591, #33371 ) ;
#48340 = CARTESIAN_POINT ( 'NONE',  ( -1.256510416662318663, -82.24348958333220594, 0.1636246174179673829 ) ) ;
#48341 = CARTESIAN_POINT ( 'NONE',  ( 3.699999999670000150, -79.00321104920828930, -4.531193156441073745E-16 ) ) ;
#48342 = ORIENTED_EDGE ( 'NONE', *, *, #39959, .T. ) ;
#48343 = CARTESIAN_POINT ( 'NONE',  ( 6.064331118019999245, -78.54256869612397907, -9.105586440592000841 ) ) ;
#48344 = CARTESIAN_POINT ( 'NONE',  ( 9.599999999999999645, -92.13603921945998820, 0.000000000000000000 ) ) ;
#48345 = CARTESIAN_POINT ( 'NONE',  ( -10.46536824075000105, -80.40014086983299535, -4.041474877054999304 ) ) ;
#48346 = VERTEX_POINT ( 'NONE', #30699 ) ;
#48347 = CARTESIAN_POINT ( 'NONE',  ( -11.03570087982000025, -77.79342066934700028, -5.118186854384000561 ) ) ;
#48348 = CIRCLE ( 'NONE', #3992, 13.86363636363999952 ) ;
#48349 = ORIENTED_EDGE ( 'NONE', *, *, #8799, .T. ) ;
#48350 = VERTEX_POINT ( 'NONE', #15185 ) ;
#48351 = LINE ( 'NONE', #31404, #6627 ) ;
#48352 = CARTESIAN_POINT ( 'NONE',  ( -3.308356910955999819, -86.39318692608898687, 1.472975399707999955 ) ) ;
#48353 = CARTESIAN_POINT ( 'NONE',  ( -3.862145970064539746, -0.8702854025945180316, -1.118418364751955218 ) ) ;
#48354 = ORIENTED_EDGE ( 'NONE', *, *, #1245, .F. ) ;
#48355 = DIRECTION ( 'NONE',  ( -1.000000000000000000, 0.000000000000000000, 0.000000000000000000 ) ) ;
#48356 = ORIENTED_EDGE ( 'NONE', *, *, #13370, .F. ) ;
#48357 = CARTESIAN_POINT ( 'NONE',  ( -9.042566447131001439, -79.10902074051685418, -8.284387575507999202 ) ) ;
#48358 = CARTESIAN_POINT ( 'NONE',  ( -3.587191200520567502, -78.96264282632948550, -2.026888227377177998 ) ) ;
#48359 = VECTOR ( 'NONE', #27747, 1000.000000000000000 ) ;
#48360 = CARTESIAN_POINT ( 'NONE',  ( 7.974020021219000220, -54.16898233660000272, 9.929669236765001017 ) ) ;
#48361 = CARTESIAN_POINT ( 'NONE',  ( 0.3926218265389159745, -78.25416666666667709, 1.460959015002474493 ) ) ;
#48362 = DIRECTION ( 'NONE',  ( 0.000000000000000000, 0.000000000000000000, -1.000000000000000000 ) ) ;
#48363 = CIRCLE ( 'NONE', #9715, 5.000000000000000000 ) ;
#48364 = EDGE_CURVE ( 'NONE', #47937, #54593, #31201, .T. ) ;
#48365 = CARTESIAN_POINT ( 'NONE',  ( -1.626826133776999786E-14, -74.80000000000001137, 0.000000000000000000 ) ) ;
#48366 = CARTESIAN_POINT ( 'NONE',  ( -1.297604665245808642, -77.89238241849264455, -0.7720361663834586219 ) ) ;
#48367 = CARTESIAN_POINT ( 'NONE',  ( 8.548480318118429011, -78.81895703212624937, -3.533306059048998637 ) ) ;
#48368 = ADVANCED_FACE ( 'NONE', ( #56220 ), #51800, .T. ) ;
#48369 = CARTESIAN_POINT ( 'NONE',  ( 12.21199139566000014, -76.20804719422000062, 1.550091862394999964 ) ) ;
#48370 = CARTESIAN_POINT ( 'NONE',  ( 3.837977402148000206, -82.36630496681199531, -1.636926709757999809 ) ) ;
#48371 = CARTESIAN_POINT ( 'NONE',  ( -7.810754875833999300, -77.80808667140099999, -5.856810041960000213 ) ) ;
#48372 = CARTESIAN_POINT ( 'NONE',  ( -1.333333333333332815, -83.45000000000000284, 0.000000000000000000 ) ) ;
#48373 = CARTESIAN_POINT ( 'NONE',  ( 2.879226727952049814, -77.95416666666666572, 10.71369944335148183 ) ) ;
#48374 = CARTESIAN_POINT ( 'NONE',  ( -12.17466003208999936, -76.48783809801099665, 1.612538369963999907 ) ) ;
#48375 = CARTESIAN_POINT ( 'NONE',  ( 8.018769647075153273, -79.91052682219850567, 7.624166446277077291 ) ) ;
#48376 = DIRECTION ( 'NONE',  ( -3.342748300494999961E-11, -1.000000000000000000, -3.127658994406000054E-09 ) ) ;
#48377 = CARTESIAN_POINT ( 'NONE',  ( -12.90000000000000036, 0.000000000000000000, 0.000000000000000000 ) ) ;
#48378 = EDGE_CURVE ( 'NONE', #23335, #8076, #39856, .T. ) ;
#48379 = CARTESIAN_POINT ( 'NONE',  ( -0.7266214904040529943, -81.16493616783630216, 1.326165027772164828 ) ) ;
#48380 = CARTESIAN_POINT ( 'NONE',  ( 5.326985168515999902, -77.34776426251399073, 7.723193303612999827 ) ) ;
#48381 = CARTESIAN_POINT ( 'NONE',  ( 1.592284932317999946, -78.67132866053199791, 0.2680347371437999948 ) ) ;
#48382 = CIRCLE ( 'NONE', #19138, 12.69999999999999929 ) ;
#48383 = DIRECTION ( 'NONE',  ( -0.6562721000522208081, -0.7545243075561237633, -7.874467463877248089E-10 ) ) ;
#48384 = CARTESIAN_POINT ( 'NONE',  ( -1.204158649194000175, -3.066063735461000306, -3.347755931201000124 ) ) ;
#48385 = CARTESIAN_POINT ( 'NONE',  ( 5.022587898441999599, -78.03194079526799953, -11.20577484976000093 ) ) ;
#48386 = DIRECTION ( 'NONE',  ( 0.000000000000000000, -1.000000000000000000, 0.000000000000000000 ) ) ;
#48388 = CARTESIAN_POINT ( 'NONE',  ( 0.1427930653877000078, -78.10831261029910877, 1.311554697429999861 ) ) ;
#48387 = CARTESIAN_POINT ( 'NONE',  ( -4.131565180156527184, -75.80000000000001137, 11.24552900431304892 ) ) ;
#48389 = CARTESIAN_POINT ( 'NONE',  ( 1.457613149566999944, -82.42445575724998719, -0.6243081169531999874 ) ) ;
#48390 = CARTESIAN_POINT ( 'NONE',  ( -8.951034867792523997, -79.55334570058815302, 5.953222655899479854 ) ) ;
#48391 = ORIENTED_EDGE ( 'NONE', *, *, #5281, .F. ) ;
#48392 = CARTESIAN_POINT ( 'NONE',  ( 0.000000000000000000, -39.30476017083000073, 0.000000000000000000 ) ) ;
#48393 = CIRCLE ( 'NONE', #54078, 13.86363636363999952 ) ;
#48394 = CARTESIAN_POINT ( 'NONE',  ( 5.174923306164999737, -79.35148740836599757, -10.87255359444000113 ) ) ;
#48395 = CARTESIAN_POINT ( 'NONE',  ( -7.645247686219181382, -79.19858867851458228, 5.772722378017828504 ) ) ;
#48396 = CARTESIAN_POINT ( 'NONE',  ( -0.001936697166661765362, -79.77500000000000568, 12.03695396042130561 ) ) ;
#48397 = CARTESIAN_POINT ( 'NONE',  ( -12.80088938724999892, -59.56256651724000051, -1.980532758767000301 ) ) ;
#48398 = CARTESIAN_POINT ( 'NONE',  ( -3.274849198131999817, -0.5460671121268000361, -0.04757157529786999739 ) ) ;
#48399 = CARTESIAN_POINT ( 'NONE',  ( -1.303463199981000020, -80.09257338644599145, 9.693416794543999515 ) ) ;
#48400 = CARTESIAN_POINT ( 'NONE',  ( 12.54705830248999909, -24.53699017355999956, -1.287129557046000183 ) ) ;
#48401 = CARTESIAN_POINT ( 'NONE',  ( -12.71107039379021586, -54.54871969218453387, -1.717622521768342292 ) ) ;
#48402 = EDGE_LOOP ( 'NONE', ( #30466, #51032, #21896, #45089, #53129 ) ) ;
#48403 = AXIS2_PLACEMENT_3D ( 'NONE', #20728, #52321, #3304 ) ;
#48404 = DIRECTION ( 'NONE',  ( 0.000000000000000000, 1.000000000000000000, 0.000000000000000000 ) ) ;
#48405 = CARTESIAN_POINT ( 'NONE',  ( -9.717796984206000133, -79.81506001420198970, 0.6849888841999000055 ) ) ;
#48406 = CARTESIAN_POINT ( 'NONE',  ( -1.750000000000000000, -23.25000000000000000, -12.00000000000000000 ) ) ;
#48407 = AXIS2_PLACEMENT_3D ( 'NONE', #48975, #3800, #35073 ) ;
#48408 = CARTESIAN_POINT ( 'NONE',  ( -0.3926218265389189721, -78.50416666666667709, -1.460959015002473604 ) ) ;
#48409 = CARTESIAN_POINT ( 'NONE',  ( 1.617840321509000034, -80.03955506511998408, 0.3973055507782000118 ) ) ;
#48410 = VERTEX_POINT ( 'NONE', #45479 ) ;
#48411 = CARTESIAN_POINT ( 'NONE',  ( 10.52161952788999955, -77.15335001815408589, -3.541364337751999880 ) ) ;
#48412 = CARTESIAN_POINT ( 'NONE',  ( 1.535712162480687759, -77.83339044027641762, -11.74751977916936418 ) ) ;
#48413 = CARTESIAN_POINT ( 'NONE',  ( -9.050966799188000067, -59.94999999969999749, 7.919595949288999570 ) ) ;
#48414 = ADVANCED_FACE ( 'NONE', ( #22141 ), #10644, .F. ) ;
#48415 = CARTESIAN_POINT ( 'NONE',  ( -12.71798280857999863, -60.09778595451999905, 1.931086388455000025 ) ) ;
#48416 = CARTESIAN_POINT ( 'NONE',  ( -8.596775676211999340, -53.66467110130999885, -9.310147894663000301 ) ) ;
#48417 = CARTESIAN_POINT ( 'NONE',  ( 1.841371367509999857, -79.84963815277498611, -9.592189096167999196 ) ) ;
#48418 = EDGE_LOOP ( 'NONE', ( #55313, #42179, #24171, #8111 ) ) ;
#48419 = VERTEX_POINT ( 'NONE', #36309 ) ;
#48420 = CARTESIAN_POINT ( 'NONE',  ( 7.255050800794000665, -76.58445350691199849, 10.14301354085000106 ) ) ;
#48421 = CARTESIAN_POINT ( 'NONE',  ( -10.36620373394242911, -78.62142715943907945, -2.852891701318189810 ) ) ;
#48422 = ORIENTED_EDGE ( 'NONE', *, *, #13697, .F. ) ;
#48423 = CARTESIAN_POINT ( 'NONE',  ( 12.50412681322812958, -17.48010473091090589, 1.235016000439091988 ) ) ;
#48424 = CARTESIAN_POINT ( 'NONE',  ( 0.000000000000000000, -75.00000000000000000, 0.000000000000000000 ) ) ;
#48425 = CARTESIAN_POINT ( 'NONE',  ( -0.6838172738181883537, -82.21924584448981932, -1.066457163286079979 ) ) ;
#48426 = CARTESIAN_POINT ( 'NONE',  ( -1.169957374810000061, -77.28625595695000072, -12.74520906849999946 ) ) ;
#48427 = CARTESIAN_POINT ( 'NONE',  ( 0.000000000000000000, -75.67500000000001137, 0.000000000000000000 ) ) ;
#48428 = CARTESIAN_POINT ( 'NONE',  ( -8.096452064242996016, -19.21421830981000056, 13.15643568217000769 ) ) ;
#48429 = CARTESIAN_POINT ( 'NONE',  ( -2.611770760766960464, -86.39318692756700102, 3.525481195052141192 ) ) ;
#48430 = CARTESIAN_POINT ( 'NONE',  ( -8.382198119002001846, -79.95952206355410397, -7.453647783897999979 ) ) ;
#48431 = CARTESIAN_POINT ( 'NONE',  ( 1.441608637993120112, -79.96304127600662071, 9.136664121622990464 ) ) ;
#48432 = DIRECTION ( 'NONE',  ( -0.7592504785509017751, -0.04890181650815008524, 0.6489586451866018457 ) ) ;
#48433 = ORIENTED_EDGE ( 'NONE', *, *, #23941, .F. ) ;
#48434 = EDGE_CURVE ( 'NONE', #53816, #22708, #27145, .T. ) ;
#48435 = CARTESIAN_POINT ( 'NONE',  ( 5.473581026676259675, -77.27553049482349934, -7.456605559097626568 ) ) ;
#48436 = CARTESIAN_POINT ( 'NONE',  ( -0.5179932711920000044, -79.39255081561999816, -1.319781611125000031 ) ) ;
#48437 = CARTESIAN_POINT ( 'NONE',  ( -0.3271848554490991434, -83.10416666666665719, -1.217465845835395299 ) ) ;
#48438 = AXIS2_PLACEMENT_3D ( 'NONE', #13110, #21686, #44717 ) ;
#48439 = CARTESIAN_POINT ( 'NONE',  ( -1.040416939902000237, -78.11213479155139794, -1.102939138596999991 ) ) ;
#48440 = AXIS2_PLACEMENT_3D ( 'NONE', #6187, #6479, #10336 ) ;
#48441 = CARTESIAN_POINT ( 'NONE',  ( -7.644093100862067836, -60.32380578946135330, -10.09634101415690566 ) ) ;
#48442 = CARTESIAN_POINT ( 'NONE',  ( -8.114915067892086498, -17.17115967855345104, 9.847905526149444810 ) ) ;
#48443 = DIRECTION ( 'NONE',  ( 0.000000000000000000, -1.000000000000000000, 0.000000000000000000 ) ) ;
#48444 = CARTESIAN_POINT ( 'NONE',  ( -1.259732397319124342, -79.12633733726526941, -0.4364906895173376600 ) ) ;
#48445 = CARTESIAN_POINT ( 'NONE',  ( 0.2656919276500000482, -79.68383300265197988, -11.15441650005999996 ) ) ;
#48446 = FACE_OUTER_BOUND ( 'NONE', #29960, .T. ) ;
#48447 = CARTESIAN_POINT ( 'NONE',  ( -0.8868929876605555762, -83.03844894029447232, 0.8802993065933630845 ) ) ;
#48448 = CARTESIAN_POINT ( 'NONE',  ( -3.126681305892000218, -81.85392767752199461, -2.762320878000999791 ) ) ;
#48449 = ADVANCED_FACE ( 'NONE', ( #23026 ), #47451, .F. ) ;
#48450 = ORIENTED_EDGE ( 'NONE', *, *, #39828, .T. ) ;
#48451 = CARTESIAN_POINT ( 'NONE',  ( 1.614964347157999747, -82.10570787394000547, 0.5400991692461000193 ) ) ;
#48452 = CARTESIAN_POINT ( 'NONE',  ( 0.4206423954835999401, -80.60477686209999604, -1.406949933701999944 ) ) ;
#48453 = CARTESIAN_POINT ( 'NONE',  ( -1.291666666665713281, -77.95833333333236226, 0.2617993877989879259 ) ) ;
#48454 = EDGE_CURVE ( 'NONE', #44413, #23208, #25704, .T. ) ;
#48455 = CARTESIAN_POINT ( 'NONE',  ( -4.085659785884999451, -78.40101240078699618, 11.26159174134999930 ) ) ;
#48456 = DIRECTION ( 'NONE',  ( 0.000000000000000000, 1.000000000000000000, 0.000000000000000000 ) ) ;
#48457 = CARTESIAN_POINT ( 'NONE',  ( -1.462746796095000024, -81.22894783996999024, -0.3322225316158000097 ) ) ;
#48458 = CARTESIAN_POINT ( 'NONE',  ( 3.008183132799063131, -2.043479984662694093, 1.827109633313784620 ) ) ;
#48459 = CARTESIAN_POINT ( 'NONE',  ( -7.401612602209000968, -79.18620194988500316, -6.305503003149000030 ) ) ;
#48460 = CARTESIAN_POINT ( 'NONE',  ( -1.582498447122000051, -54.64913877488999816, -12.55493832969000145 ) ) ;
#48461 = CARTESIAN_POINT ( 'NONE',  ( 11.09363377535068196, -75.97617094292559159, 3.874839546677522506 ) ) ;
#48462 = CARTESIAN_POINT ( 'NONE',  ( 4.443227334435270848, -85.83735716284300565, 0.5100107989082148796 ) ) ;
#48463 = VERTEX_POINT ( 'NONE', #27443 ) ;
#48464 = CARTESIAN_POINT ( 'NONE',  ( 0.000000000000000000, -51.86282895648000135, 0.000000000000000000 ) ) ;
#48465 = CARTESIAN_POINT ( 'NONE',  ( 0.4259464286568289682, -2.236800215964222627, -3.249988294983786830 ) ) ;
#48466 = CARTESIAN_POINT ( 'NONE',  ( -2.739513636030999955, -79.43367427549699755, -11.96158333944000063 ) ) ;
#48467 = CARTESIAN_POINT ( 'NONE',  ( 0.000000000000000000, -75.20000000000000284, -11.64999999999768043 ) ) ;
#48468 = CARTESIAN_POINT ( 'NONE',  ( 0.6304340365998000184, -82.67372400502100049, 1.542015542100000136 ) ) ;
#48469 = CARTESIAN_POINT ( 'NONE',  ( -4.399243655502999673, -79.77766721275199302, 10.05537673064999815 ) ) ;
#48470 = CARTESIAN_POINT ( 'NONE',  ( 0.9356112518261625599, -17.25892169760723860, -12.50329130247260601 ) ) ;
#48471 = CARTESIAN_POINT ( 'NONE',  ( -12.18147860638999980, -75.95564905944900147, -2.246276167021000081 ) ) ;
#48472 = CARTESIAN_POINT ( 'NONE',  ( 3.171384185490563112, -78.55103045045009935, 11.31254194630599486 ) ) ;
#48473 = CARTESIAN_POINT ( 'NONE',  ( 3.938458446976999205, -79.21000000000000796, -8.369650235310999165 ) ) ;
#48474 = ORIENTED_EDGE ( 'NONE', *, *, #26694, .F. ) ;
#48475 = CARTESIAN_POINT ( 'NONE',  ( 3.449307203194000415, -78.99083078338598796, 10.47874105986000082 ) ) ;
#48476 = CARTESIAN_POINT ( 'NONE',  ( -2.164532541486328565, -77.39366991027993947, 9.022216075546257485 ) ) ;
#48477 = PRODUCT_RELATED_PRODUCT_CATEGORY ( 'part', '', ( #8315 ) ) ;
#48478 = CARTESIAN_POINT ( 'NONE',  ( 11.40864393521657227, -75.79999999999999716, -3.704034794931656993 ) ) ;
#48479 = VECTOR ( 'NONE', #21738, 1000.000000000000000 ) ;
#48480 = CARTESIAN_POINT ( 'NONE',  ( -2.977158780993999887, -78.63955604921899578, 10.75305190397999944 ) ) ;
#48481 = B_SPLINE_CURVE_WITH_KNOTS ( 'NONE', 3,
 ( #14573, #46195, #41740, #19312, #42035, #50904, #1604, #37302, #14862, #32858, #52352, #6889, #57060, #7471, #12467, #3611, #43781, #3333 ),
 .UNSPECIFIED., .F., .F.,
 ( 4, 2, 2, 2, 2, 2, 2, 2, 4 ),
 ( 0.000000000000000000, 0.1250000000000000833, 0.2500000000000001665, 0.3750000000000001665, 0.5000000000000002220, 0.6250000000000002220, 0.7500000000000001110, 0.8750000000000001110, 1.000000000000000000 ),
 .UNSPECIFIED. ) ;
#48482 = CARTESIAN_POINT ( 'NONE',  ( 2.269106295766999856E-14, -92.56607767729998670, 0.000000000000000000 ) ) ;
#48483 = DIRECTION ( 'NONE',  ( 0.000000000000000000, -1.000000000000000000, 0.000000000000000000 ) ) ;
#48484 = DIRECTION ( 'NONE',  ( -1.000000000000000000, 0.000000000000000000, 0.000000000000000000 ) ) ;
#48485 = DIRECTION ( 'NONE',  ( 1.000000000000000000, 0.000000000000000000, 2.582621269619999448E-11 ) ) ;
#48486 = EDGE_CURVE ( 'NONE', #53713, #39513, #45376, .T. ) ;
#48487 = CARTESIAN_POINT ( 'NONE',  ( 10.75000000000000000, -77.19999999999998863, -6.141891925717000695E-13 ) ) ;
#48488 = EDGE_CURVE ( 'NONE', #9151, #30430, #53834, .T. ) ;
#48489 = PLANE ( 'NONE',  #3750 ) ;
#48490 =( LENGTH_UNIT ( ) NAMED_UNIT ( * ) SI_UNIT ( .MILLI., .METRE. ) );
#48491 = CARTESIAN_POINT ( 'NONE',  ( -1.538071403320043551, -76.18541666666665435, 11.74999999999999467 ) ) ;
#48492 = VERTEX_POINT ( 'NONE', #33329 ) ;
#48493 = ORIENTED_EDGE ( 'NONE', *, *, #3071, .T. ) ;
#48494 = CARTESIAN_POINT ( 'NONE',  ( -12.70926961117000076, -55.39159259587000150, -1.933875435151000133 ) ) ;
#48495 = ORIENTED_EDGE ( 'NONE', *, *, #1134, .F. ) ;
#48496 = CARTESIAN_POINT ( 'NONE',  ( -6.961488625003511288, -79.69021735228992043, 6.501630528635893747 ) ) ;
#48497 = ORIENTED_EDGE ( 'NONE', *, *, #21868, .T. ) ;
#48498 = CARTESIAN_POINT ( 'NONE',  ( -6.807885647488862269, -81.00000000000001421, -8.483415954689156990 ) ) ;
#48499 = CARTESIAN_POINT ( 'NONE',  ( -5.702669450565000631, -77.49214815972399606, 9.308862826782998923 ) ) ;
#48500 = CARTESIAN_POINT ( 'NONE',  ( -7.750101915720000179, -78.70333667140100431, 6.177086609340000756 ) ) ;
#48501 = CARTESIAN_POINT ( 'NONE',  ( -10.34326456654000026, -78.66670268365299989, 4.339929572939999147 ) ) ;
#48502 = VECTOR ( 'NONE', #24547, 1000.000000000000000 ) ;
#48503 = ORIENTED_EDGE ( 'NONE', *, *, #40726, .F. ) ;
#48504 = EDGE_LOOP ( 'NONE', ( #17917, #11524, #20605, #15076, #53802, #11022 ) ) ;
#48505 = CARTESIAN_POINT ( 'NONE',  ( -7.498854895474774906, -77.55022293857352622, 5.415685297931227993 ) ) ;
#48506 = CARTESIAN_POINT ( 'NONE',  ( 6.393001003723999709, -77.19570245782817608, 9.000752526674000720 ) ) ;
#48507 = CARTESIAN_POINT ( 'NONE',  ( 9.045658679128999680, -79.10650131180899791, 3.115350657311999782 ) ) ;
#48508 = CARTESIAN_POINT ( 'NONE',  ( -2.764837346328296253, -86.12610001270964233, 3.732097096069109554 ) ) ;
#48509 = CARTESIAN_POINT ( 'NONE',  ( -8.465407715419214441, -79.43746552134066974, -4.311206955701401000 ) ) ;
#48510 = CARTESIAN_POINT ( 'NONE',  ( -1.462188802161999979, -79.24735702617999777, -0.7147474581103999691 ) ) ;
#48511 = CARTESIAN_POINT ( 'NONE',  ( 11.10498291493000167, -80.10684763845199541, -1.830582403018000015 ) ) ;
#48512 = CARTESIAN_POINT ( 'NONE',  ( 12.66008925484999992, -17.37289997915000228, -1.387046028394999908 ) ) ;
#48513 = CIRCLE ( 'NONE', #56067, 14.00000000000000533 ) ;
#48514 = CARTESIAN_POINT ( 'NONE',  ( -9.830801209626999437, -24.09088558010999748, -7.765011064334000679 ) ) ;
#48515 = CARTESIAN_POINT ( 'NONE',  ( -11.46828826707757365, -76.68240725586073836, 2.559436963939517362 ) ) ;
#48516 = EDGE_CURVE ( 'NONE', #24529, #49672, #7804, .T. ) ;
#48517 = ORIENTED_EDGE ( 'NONE', *, *, #32159, .T. ) ;
#48518 = CARTESIAN_POINT ( 'NONE',  ( 10.79000226207000068, -79.78942873821000603, -5.440152796310999683 ) ) ;
#48519 = CARTESIAN_POINT ( 'NONE',  ( -1.199999999999999956, -75.00000000000000000, -7.200000000000000178 ) ) ;
#48520 = ADVANCED_FACE ( 'NONE', ( #10921 ), #30414, .T. ) ;
#48521 = CARTESIAN_POINT ( 'NONE',  ( -4.085659785884999451, -78.60437806061599986, 11.26159174134999930 ) ) ;
#48522 = CARTESIAN_POINT ( 'NONE',  ( -9.213130513696000889, -16.99475660687000200, -8.533779407534000327 ) ) ;
#48524 = CARTESIAN_POINT ( 'NONE',  ( -0.4450739772392999782, -17.12186785197999939, -12.43586747594999942 ) ) ;
#48523 = FACE_OUTER_BOUND ( 'NONE', #57649, .T. ) ;
#48525 = CARTESIAN_POINT ( 'NONE',  ( 1.634168180750863897, -1.268200832823612956, -2.838472589007412061 ) ) ;
#48526 = CARTESIAN_POINT ( 'NONE',  ( 10.18491068061999982, -60.10716934574000447, -7.640030139773000606 ) ) ;
#48527 = CARTESIAN_POINT ( 'NONE',  ( -5.838193839761688153, -78.37291666666668277, -7.596835002782716728 ) ) ;
#48528 = CARTESIAN_POINT ( 'NONE',  ( 11.23689443680000011, -77.57873010171299200, 0.7524413429202000403 ) ) ;
#48529 = CARTESIAN_POINT ( 'NONE',  ( 12.52134121557681468, -23.92745484923118937, 1.618935178668554631 ) ) ;
#48530 = CARTESIAN_POINT ( 'NONE',  ( -10.38445589244000011, -80.29189122021149672, 4.342440965381999973 ) ) ;
#48531 = ORIENTED_EDGE ( 'NONE', *, *, #18449, .F. ) ;
#48532 = CARTESIAN_POINT ( 'NONE',  ( 0.000000000000000000, 0.000000000000000000, -13.80000000000000071 ) ) ;
#48533 = CARTESIAN_POINT ( 'NONE',  ( -1.477284502223000118, -54.07368499670000261, 12.77254812464999922 ) ) ;
#48534 = CARTESIAN_POINT ( 'NONE',  ( 7.651160336694000641, -22.76232686216999923, -10.45205658994000153 ) ) ;
#48535 = CARTESIAN_POINT ( 'NONE',  ( -2.072817167316999942, -2.797709358522999956, -3.192057609956000075 ) ) ;
#48536 = CARTESIAN_POINT ( 'NONE',  ( 0.2539499232592060118, -78.07730306633010287, -10.83454063274043300 ) ) ;
#48537 = CARTESIAN_POINT ( 'NONE',  ( 9.350230382969998644, -79.19953686653599334, -0.8778377520234000864 ) ) ;
#48538 = CARTESIAN_POINT ( 'NONE',  ( -10.40651698430760419, -77.07932101869644725, 2.787361001673857253 ) ) ;
#48539 = CARTESIAN_POINT ( 'NONE',  ( 8.925548456419079457, -77.29999999999999716, -6.486984937931281614 ) ) ;
#48540 = CARTESIAN_POINT ( 'NONE',  ( -0.5154756746308999382, -61.93240599730000184, 12.66205448077000106 ) ) ;
#48541 = CARTESIAN_POINT ( 'NONE',  ( 0.000000000000000000, -74.64999999999999147, 0.000000000000000000 ) ) ;
#48542 = CARTESIAN_POINT ( 'NONE',  ( 3.685513155162999599, -82.55394503318800048, 1.956341549149999581 ) ) ;
#48543 = EDGE_CURVE ( 'NONE', #17562, #53718, #5928, .T. ) ;
#48544 = CARTESIAN_POINT ( 'NONE',  ( -5.539808784079887083, -77.28333333333333144, -9.611650271896841957 ) ) ;
#48545 = CYLINDRICAL_SURFACE ( 'NONE', #18276, 1.750000000000001332 ) ;
#48546 = VECTOR ( 'NONE', #21363, 1000.000000000000000 ) ;
#48547 = CARTESIAN_POINT ( 'NONE',  ( 9.566106889961746518, -76.40027222109127081, -6.823059203283996510 ) ) ;
#48548 = CARTESIAN_POINT ( 'NONE',  ( -7.755223252044999960, -78.14509280558399951, 8.006941543446998821 ) ) ;
#48549 = CARTESIAN_POINT ( 'NONE',  ( 1.118667866065873318, -81.88699651758111031, 0.5575489754530202902 ) ) ;
#48550 = CARTESIAN_POINT ( 'NONE',  ( -12.05000000000000071, -74.80000000000001137, 0.000000000000000000 ) ) ;
#48551 = VECTOR ( 'NONE', #17145, 1000.000000000000000 ) ;
#48552 = CARTESIAN_POINT ( 'NONE',  ( -6.294203684166999935, -77.20123665637598265, 7.343715272572999275 ) ) ;
#48553 = LINE ( 'NONE', #43256, #16152 ) ;
#48554 = DIRECTION ( 'NONE',  ( 0.7071067811865975328, 0.7071067811864976127, -1.603641050304993672E-09 ) ) ;
#48555 = CARTESIAN_POINT ( 'NONE',  ( 4.141311620441085140, -80.25655908808295180, -9.920226166596769701 ) ) ;
#48556 = DIRECTION ( 'NONE',  ( 0.000000000000000000, 1.000000000000000000, 0.000000000000000000 ) ) ;
#48557 = CARTESIAN_POINT ( 'NONE',  ( -10.27342224349341926, -17.93842478175206523, -7.712153330322490952 ) ) ;
#48558 = ORIENTED_EDGE ( 'NONE', *, *, #29345, .T. ) ;
#48559 = ADVANCED_FACE ( 'NONE', ( #41617 ), #55195, .F. ) ;
#48560 = CARTESIAN_POINT ( 'NONE',  ( 11.66950233118999947, -79.22880174150600396, -2.920592611544999606 ) ) ;
#48561 = VECTOR ( 'NONE', #23755, 1000.000000000000000 ) ;
#48562 = CARTESIAN_POINT ( 'NONE',  ( 7.596835002782697188, -78.60208333333333997, 5.838193839761710358 ) ) ;
#48563 = CARTESIAN_POINT ( 'NONE',  ( 6.010232441408999371, -80.15361206703849462, 9.524218016016000377 ) ) ;
#48564 = CARTESIAN_POINT ( 'NONE',  ( -6.557200067333805116, -77.52710381399123207, 8.547272894749051275 ) ) ;
#48565 = ORIENTED_EDGE ( 'NONE', *, *, #12691, .F. ) ;
#48566 = EDGE_LOOP ( 'NONE', ( #55976, #53879, #27332, #34167, #30251 ) ) ;
#48567 = CARTESIAN_POINT ( 'NONE',  ( -1.811016405462510859, -24.06173555372251371, 12.71771640064107523 ) ) ;
#48568 = ORIENTED_EDGE ( 'NONE', *, *, #45634, .T. ) ;
#48569 = PLANE ( 'NONE',  #15107 ) ;
#48570 = ORIENTED_EDGE ( 'NONE', *, *, #55153, .F. ) ;
#48571 = DIRECTION ( 'NONE',  ( 0.000000000000000000, -1.000000000000000000, 0.000000000000000000 ) ) ;
#48572 = CIRCLE ( 'NONE', #41949, 0.5000000000000004441 ) ;
#48573 = CARTESIAN_POINT ( 'NONE',  ( -1.500000000000000000, -78.50000000000000000, 0.000000000000000000 ) ) ;
#48574 = CARTESIAN_POINT ( 'NONE',  ( -10.11939726227999969, -79.60401229401898604, -4.095505467953000078 ) ) ;
#48575 = CARTESIAN_POINT ( 'NONE',  ( -2.751373484785000212, -79.05481202895639115, -2.305178922514000028 ) ) ;
#48576 = CARTESIAN_POINT ( 'NONE',  ( -1.436252226850364355, -79.28687123219287969, 9.390701153346968866 ) ) ;
#48577 = ORIENTED_EDGE ( 'NONE', *, *, #17980, .T. ) ;
#48578 = CARTESIAN_POINT ( 'NONE',  ( 9.838393222920561954, -78.31597548449377655, -4.482763737194812137 ) ) ;
#48579 = CARTESIAN_POINT ( 'NONE',  ( 4.729275446575999631, -78.57519050484999923, -11.25706921911999991 ) ) ;
#48580 = ORIENTED_EDGE ( 'NONE', *, *, #46706, .T. ) ;
#48581 = CARTESIAN_POINT ( 'NONE',  ( -0.7509728292934746419, -77.83402495159873524, -1.337060448512992439 ) ) ;
#48582 = CARTESIAN_POINT ( 'NONE',  ( 12.80000000000000071, -6.000000000000000000, 0.000000000000000000 ) ) ;
#48583 = CARTESIAN_POINT ( 'NONE',  ( -8.776032052582039000, -80.05126053055296609, 6.209312603182142176 ) ) ;
#48584 = CARTESIAN_POINT ( 'NONE',  ( 0.000000000000000000, -65.72928575305999743, 0.000000000000000000 ) ) ;
#48585 = CARTESIAN_POINT ( 'NONE',  ( -3.318865696948021693, -86.31452042059397911, -2.316308510770335172 ) ) ;
#48586 = CARTESIAN_POINT ( 'NONE',  ( 2.090460633792530221, -85.88583664465505763, 2.794791628714064391 ) ) ;
#48587 = CARTESIAN_POINT ( 'NONE',  ( 11.88773275212999891, -76.79030896091001068, 5.537155082298999886 ) ) ;
#48588 = CARTESIAN_POINT ( 'NONE',  ( -3.180509609271000127, -77.13961746229999505, 12.23476839664999893 ) ) ;
#48589 = AXIS2_PLACEMENT_3D ( 'NONE', #11240, #37497, #29506 ) ;
#48590 = CARTESIAN_POINT ( 'NONE',  ( 8.109890173097999977, -76.21951620272498928, -7.078589237139000012 ) ) ;
#48591 = CARTESIAN_POINT ( 'NONE',  ( -9.236754519813018760, -78.60432763383623467, -0.5006253770964849137 ) ) ;
#48592 = CARTESIAN_POINT ( 'NONE',  ( 0.5517604069303000403, -79.29531287791878924, -4.093176084825000061 ) ) ;
#48593 = CARTESIAN_POINT ( 'NONE',  ( -10.35747145894000099, -60.11584731951999316, 7.626500777253000685 ) ) ;
#48594 = CARTESIAN_POINT ( 'NONE',  ( -2.103158146349364710, -3.031636871358540208, 2.492261966649085281 ) ) ;
#48595 = CARTESIAN_POINT ( 'NONE',  ( -1.281543785372999844, -78.99930496681159298, -3.307439830080999510 ) ) ;
#48596 = B_SPLINE_CURVE_WITH_KNOTS ( 'NONE', 3,
 ( #16291, #47021, #29553, #56732, #47311, #28979 ),
 .UNSPECIFIED., .F., .F.,
 ( 4, 2, 4 ),
 ( 0.000000000000000000, 0.5000000000000000000, 1.000000000000000000 ),
 .UNSPECIFIED. ) ;
#48597 = CYLINDRICAL_SURFACE ( 'NONE', #51530, 1.500000000000000000 ) ;
#48598 = CARTESIAN_POINT ( 'NONE',  ( 0.8024039916437721853, -80.96950772143027564, 10.72170357542168340 ) ) ;
#48599 = CARTESIAN_POINT ( 'NONE',  ( 2.573795024414000210, -83.82549735065198604, -2.437322908517999931 ) ) ;
#48600 = CARTESIAN_POINT ( 'NONE',  ( -3.796701970596999764, -2.742418933659000135, 0.2667143827384000354 ) ) ;
#48601 = CARTESIAN_POINT ( 'NONE',  ( 0.5769587189189382403, -79.91279883384609661, -1.136438736130747529 ) ) ;
#48602 = EDGE_LOOP ( 'NONE', ( #1963, #33979, #39126, #55611, #27274 ) ) ;
#48603 = CARTESIAN_POINT ( 'NONE',  ( -2.813789756862274949, -80.10416666666667140, -10.47020627418438998 ) ) ;
#48604 = CARTESIAN_POINT ( 'NONE',  ( -7.596835002782739821, -78.34791666666669130, 5.838193839761659731 ) ) ;
#48605 = CARTESIAN_POINT ( 'NONE',  ( -0.8719406389885000497, -81.24640551900300522, -1.009106372638000071 ) ) ;
#48606 = CARTESIAN_POINT ( 'NONE',  ( -12.82202470520000048, -18.57373556878999921, -2.066041976111999467 ) ) ;
#48607 = DIRECTION ( 'NONE',  ( -0.5721800012450221073, 0.8201280669354309438, 0.000000000000000000 ) ) ;
#48608 = CARTESIAN_POINT ( 'NONE',  ( 10.31626776183999894, -78.03182302711998375, -3.746764721243999841 ) ) ;
#48609 = ADVANCED_FACE ( 'NONE', ( #1485 ), #55490, .F. ) ;
#48610 = CARTESIAN_POINT ( 'NONE',  ( 0.000000000000000000, -80.99999999999998579, -7.000000000000000000 ) ) ;
#48611 = CARTESIAN_POINT ( 'NONE',  ( -11.74660045421000021, -76.64649974677999467, 3.339300926223000232 ) ) ;
#48612 = ORIENTED_EDGE ( 'NONE', *, *, #34477, .F. ) ;
#48613 = CARTESIAN_POINT ( 'NONE',  ( 12.50000000000000000, -18.75000000000000000, 0.000000000000000000 ) ) ;
#48614 = CARTESIAN_POINT ( 'NONE',  ( -9.326075088887810338, -79.75741750814056275, 5.512176992475737336 ) ) ;
#48615 = CARTESIAN_POINT ( 'NONE',  ( -10.75000000000000000, -79.00000000000000000, 0.000000000000000000 ) ) ;
#48616 = CARTESIAN_POINT ( 'NONE',  ( 0.000000000000000000, -3.000000000000000000, 0.000000000000000000 ) ) ;
#48617 = CARTESIAN_POINT ( 'NONE',  ( 8.177883213696999221, -78.09878108138998698, -5.086790354254000057 ) ) ;
#48618 = CARTESIAN_POINT ( 'NONE',  ( 3.675289024537000238, -85.34481509293298984, -1.975429873306999928 ) ) ;
#48619 = CARTESIAN_POINT ( 'NONE',  ( -0.7814361956828775879, -79.98113340217017253, 10.72722109628113074 ) ) ;
#48620 = CARTESIAN_POINT ( 'NONE',  ( -1.227075629532000001, -79.64443611377700449, -0.7101723588523999320 ) ) ;
#48621 = EDGE_LOOP ( 'NONE', ( #56328, #4454, #10234, #50065 ) ) ;
#48622 = DIRECTION ( 'NONE',  ( 0.000000000000000000, 1.000000000000000000, 0.000000000000000000 ) ) ;
#48623 = CARTESIAN_POINT ( 'NONE',  ( 7.307999405654648228, -78.90319446237640477, 5.704134542545350683 ) ) ;
#48624 = FACE_OUTER_BOUND ( 'NONE', #17911, .T. ) ;
#48625 = VERTEX_POINT ( 'NONE', #38344 ) ;
#48627 = EDGE_CURVE ( 'NONE', #14640, #44478, #26310, .T. ) ;
#48626 = EDGE_LOOP ( 'NONE', ( #35901, #26752, #7188 ) ) ;
#48628 = CARTESIAN_POINT ( 'NONE',  ( -0.6558374186847000242, -79.68666419164598835, 11.02940581592999969 ) ) ;
#48629 = CARTESIAN_POINT ( 'NONE',  ( 12.53241208775000004, -56.03537109808000594, 1.667936697358999965 ) ) ;
#48630 = CARTESIAN_POINT ( 'NONE',  ( -8.889114177306000286, -80.18886705758899325, 7.203513103890000657 ) ) ;
#48631 = ORIENTED_EDGE ( 'NONE', *, *, #3886, .F. ) ;
#48632 = B_SPLINE_CURVE_WITH_KNOTS ( 'NONE', 3,
 ( #23715, #18133, #40855, #18426, #36128, #41726, #50018, #54144, #36416, #31682, #49728, #9271, #27549, #45592, #23136, #734, #18714, #33849, #19711, #37122, #19128, #33268, #46598, #6125, #42446, #1141, #55432, #55134, #14679, #24131, #29133, #42149, #37995, #20294, #28550, #1719, #10271, #15863, #9983, #38286, #15275, #2014, #6417, #2297, #37709, #55731, #56309, #56020, #32677, #15569, #33563, #51309, #28252, #10868, #27963, #28839, #46888, #1431, #11160, #24430, #47180, #20012, #46306, #51601, #37411 ),
 .UNSPECIFIED., .F., .F.,
 ( 4, 1, 1, 1, 1, 1, 1, 1, 1, 1, 1, 1, 1, 1, 1, 1, 1, 1, 1, 1, 1, 1, 1, 1, 1, 1, 1, 1, 1, 1, 1, 1, 1, 1, 1, 1, 1, 1, 1, 1, 1, 1, 1, 1, 1, 1, 1, 1, 1, 1, 1, 1, 1, 1, 1, 1, 1, 1, 1, 1, 1, 1, 4 ),
 ( 0.000000000000000000, 0.01249974716340015654, 0.02874975559081316412, 0.04499976401822616823, 0.06124977244563917234, 0.07749978087305219032, 0.09374978930046519443, 0.1099997977278781985, 0.1262498061552911888, 0.1424998145827041929, 0.1587498230101172247, 0.1749998314375302011, 0.1912498398649432330, 0.2074998482923562093, 0.2237498567197692412, 0.2399998651471822453, 0.2562498735745952216, 0.2724998820020082535, 0.2887498904294212854, 0.3049998988568342617, 0.3212499072842472381, 0.3374999157116603254, 0.3537499241390733018, 0.3699999325664862782, 0.3862499409938993100, 0.4024999494213123419, 0.4187499578487253182, 0.4349999662761383501, 0.4512499747035513264, 0.4674999831309643583, 0.4837499915583773902, 0.4999999999857903665, 0.5162500084132033429, 0.5325000168406163192, 0.5487500252680292956, 0.5650000336954423830, 0.5812500421228554703, 0.5975000505502684467, 0.6137500589776814230, 0.6300000674050943994, 0.6462500758325073758, 0.6625000842599203521, 0.6787500926873334395, 0.6950001011147464158, 0.7112501095421595032, 0.7275001179695724796, 0.7437501263969854559, 0.7600001348243984323, 0.7762501432518115196, 0.7925001516792244960, 0.8087501601066374723, 0.8250001685340504487, 0.8412501769614635361, 0.8575001853888765124, 0.8737501938162895998, 0.8900002022437025762, 0.9062502106711155525, 0.9225002190985285289, 0.9387502275259415052, 0.9550002359533544816, 0.9712502443807674579, 0.9875002528081806563, 1.000000000000000000 ),
 .UNSPECIFIED. ) ;
#48633 = CARTESIAN_POINT ( 'NONE',  ( -10.11841891201000010, -77.71203272307600685, 6.752786780719000070 ) ) ;
#48634 = VERTEX_POINT ( 'NONE', #52793 ) ;
#48635 = CIRCLE ( 'NONE', #3487, 10.34999999999999964 ) ;
#48636 = VERTEX_POINT ( 'NONE', #48377 ) ;
#48637 = ADVANCED_FACE ( 'NONE', ( #7058 ), #12517, .F. ) ;
#48638 = CARTESIAN_POINT ( 'NONE',  ( 8.485281374238999419, -59.94999999967000548, 8.485281374238999419 ) ) ;
#48639 = CARTESIAN_POINT ( 'NONE',  ( -3.567760415766010773, -1.844193969458715276, 0.1559241275462920073 ) ) ;
#48640 = ADVANCED_FACE ( 'NONE', ( #47237 ), #51235, .T. ) ;
#48641 = ORIENTED_EDGE ( 'NONE', *, *, #53545, .F. ) ;
#48642 = CARTESIAN_POINT ( 'NONE',  ( 10.98364301412005517, -18.76988149294329844, 0.5996551156055476284 ) ) ;
#48643 = ORIENTED_EDGE ( 'NONE', *, *, #47982, .T. ) ;
#48644 = CARTESIAN_POINT ( 'NONE',  ( -10.46898571549482249, -80.62085544309125851, -2.813567758576272393 ) ) ;
#48645 = CARTESIAN_POINT ( 'NONE',  ( -0.03204405817075896279, -78.72609999968184979, -3.399848993460421465 ) ) ;
#48646 = CARTESIAN_POINT ( 'NONE',  ( 8.878349648264999061, -53.73036913477000098, 8.870329531799001188 ) ) ;
#48647 = CARTESIAN_POINT ( 'NONE',  ( -7.613962827178999859, -18.69360374348000065, -10.53101998747000145 ) ) ;
#48648 = CARTESIAN_POINT ( 'NONE',  ( 5.208905169669622914, -77.35915899447975619, -10.56041358256653062 ) ) ;
#48649 = CARTESIAN_POINT ( 'NONE',  ( 9.779478297622604899, -80.64050622746258057, 5.481461471981479150 ) ) ;
#48650 = CARTESIAN_POINT ( 'NONE',  ( 9.450487096927000508, -77.84733340637855292, -7.362360902975001231 ) ) ;
#48651 = CARTESIAN_POINT ( 'NONE',  ( 9.238076819936575035, -78.84538428185697967, -0.5563267852515336731 ) ) ;
#48652 = DIRECTION ( 'NONE',  ( 1.000000000000000000, 0.000000000000000000, 0.000000000000000000 ) ) ;
#48653 = EDGE_CURVE ( 'NONE', #31908, #42463, #25629, .T. ) ;
#48654 = CARTESIAN_POINT ( 'NONE',  ( -4.007886309445000350, -81.57575264934799009, 1.168951343685000088 ) ) ;
#48655 = CARTESIAN_POINT ( 'NONE',  ( 5.073817278557999799, -78.08715333806699732, 8.075442521356999137 ) ) ;
#48656 = CARTESIAN_POINT ( 'NONE',  ( -1.250000000000001332, -83.48958333333335702, 0.1636246173744632659 ) ) ;
#48657 = CARTESIAN_POINT ( 'NONE',  ( 12.80088938719999803, -19.23743348210000192, -1.980532758767000301 ) ) ;
#48658 = DIRECTION ( 'NONE',  ( 1.000000000000000000, 0.000000000000000000, 0.000000000000000000 ) ) ;
#48659 = CARTESIAN_POINT ( 'NONE',  ( -9.469606800734000629, -80.05752053325198858, 5.597012331546999953 ) ) ;
#48660 = CARTESIAN_POINT ( 'NONE',  ( 12.52582323433381362, -23.80939730775251917, -1.680974276152543467 ) ) ;
#48661 = CARTESIAN_POINT ( 'NONE',  ( 7.624341766656999475, -60.06485146221000093, 10.42531125026000005 ) ) ;
#48662 = CARTESIAN_POINT ( 'NONE',  ( 0.2751614629225042630, -79.98895914179001920, -1.487999588816689700 ) ) ;
#48663 = CARTESIAN_POINT ( 'NONE',  ( -0.4913431507998999859, -77.39998299644997815, 9.369261706097999465 ) ) ;
#48664 = DIRECTION ( 'NONE',  ( 0.000000000000000000, -1.000000000000000000, 0.000000000000000000 ) ) ;
#48665 = CARTESIAN_POINT ( 'NONE',  ( 8.096452064242996016, -19.21421830981000056, -13.15643568217000769 ) ) ;
#48666 = VECTOR ( 'NONE', #38790, 999.9999999999998863 ) ;
#48667 = CARTESIAN_POINT ( 'NONE',  ( 10.63100742340999894, -77.23152976611999065, 5.913054471243999188 ) ) ;
#48668 = CARTESIAN_POINT ( 'NONE',  ( -1.199500263597274685, -80.94791666666668561, 0.9218200799623673669 ) ) ;
#48669 = CARTESIAN_POINT ( 'NONE',  ( -6.606377239730330864, -79.07291666666665719, -8.596418555780440229 ) ) ;
#48671 = CARTESIAN_POINT ( 'NONE',  ( -1.250000000000000000, -77.10000000000000853, 0.5000000000000000000 ) ) ;
#48670 = DIRECTION ( 'NONE',  ( -1.000000000000000000, 0.000000000000000000, 0.000000000000000000 ) ) ;
#48672 = CARTESIAN_POINT ( 'NONE',  ( -0.5511181765943999888, -82.80341104791099838, -1.486830790314999984 ) ) ;
#48673 = CARTESIAN_POINT ( 'NONE',  ( -4.297144572240187976, -79.50789134964543337, 9.855296198807199204 ) ) ;
#48674 = VECTOR ( 'NONE', #2674, 1000.000000000000000 ) ;
#48675 = ORIENTED_EDGE ( 'NONE', *, *, #37768, .F. ) ;
#48676 = CARTESIAN_POINT ( 'NONE',  ( 2.445294723173424334, -78.75875305519164726, 11.79638544041784876 ) ) ;
#48677 = CARTESIAN_POINT ( 'NONE',  ( 11.88364051439999969, -79.52574899616899984, 2.560115967181999963 ) ) ;
#48678 = CARTESIAN_POINT ( 'NONE',  ( 1.012474343122873544, -79.38347396807189682, -9.467961831871633649 ) ) ;
#48679 = CARTESIAN_POINT ( 'NONE',  ( 9.468749999988999022, -76.98125000001098783, 2.084568677130999610E-09 ) ) ;
#48680 = CARTESIAN_POINT ( 'NONE',  ( -2.879226727952121756, -78.99583333333333712, 10.71369944335146407 ) ) ;
#48681 = CARTESIAN_POINT ( 'NONE',  ( 2.965054089066000209, -1.248435987229999933, -1.931333211479999923 ) ) ;
#48682 = CARTESIAN_POINT ( 'NONE',  ( 4.335968019780999327, -79.86848743689799335, -8.767120549026998333 ) ) ;
#48683 = CARTESIAN_POINT ( 'NONE',  ( 12.43641409351999982, -24.91801033895000117, 0.03481937293212000045 ) ) ;
#48684 = CARTESIAN_POINT ( 'NONE',  ( -1.799501877793999949, -60.08917723397000543, 12.60552511012999943 ) ) ;
#48685 = EDGE_LOOP ( 'NONE', ( #1143, #33227, #27621, #51913, #46789, #30768 ) ) ;
#48686 = DIRECTION ( 'NONE',  ( 0.000000000000000000, -1.000000000000000000, 0.000000000000000000 ) ) ;
#48687 = CARTESIAN_POINT ( 'NONE',  ( -0.6048802941109999720, -79.63688667140100108, 9.614296959915000329 ) ) ;
#48688 = FACE_OUTER_BOUND ( 'NONE', #1313, .T. ) ;
#48689 = EDGE_CURVE ( 'NONE', #35908, #53225, #11781, .T. ) ;
#48690 = LINE ( 'NONE', #35670, #13855 ) ;
#48691 = CARTESIAN_POINT ( 'NONE',  ( -1.490242064849000014, -84.95267953870899191, -3.219274950222999809 ) ) ;
#48692 = ORIENTED_EDGE ( 'NONE', *, *, #19862, .F. ) ;
#48693 = EDGE_CURVE ( 'NONE', #12876, #21964, #40435, .T. ) ;
#48694 = CARTESIAN_POINT ( 'NONE',  ( -1.514723870011999818, -77.04329589215798535, -10.99769645839000098 ) ) ;
#48695 = CARTESIAN_POINT ( 'NONE',  ( 9.392095713130165890, -77.89521769223929937, -7.218153635797654566 ) ) ;
#48696 = CARTESIAN_POINT ( 'NONE',  ( -1.931087888240000217, -23.31584731985000047, 12.71658872084999992 ) ) ;
#48697 = VERTEX_POINT ( 'NONE', #34476 ) ;
#48698 = CARTESIAN_POINT ( 'NONE',  ( -12.87022657272000004, -56.01514526721999943, 2.062597299672999540 ) ) ;
#48699 = DIRECTION ( 'NONE',  ( -1.000000000000000000, 0.000000000000000000, 0.000000000000000000 ) ) ;
#48700 = SURFACE_STYLE_USAGE ( .BOTH. , #7955 ) ;
#48701 = CARTESIAN_POINT ( 'NONE',  ( 3.366547962069000199, -79.42285120457597714, -9.168809063548000182 ) ) ;
#48702 = ORIENTED_EDGE ( 'NONE', *, *, #10459, .T. ) ;
#48703 = ADVANCED_FACE ( 'NONE', ( #25342 ), #43357, .F. ) ;
#48704 = ORIENTED_EDGE ( 'NONE', *, *, #43376, .F. ) ;
#48705 = CARTESIAN_POINT ( 'NONE',  ( 6.700289941238000146, -77.29597596972099893, -9.806486244952001385 ) ) ;
#48706 = CARTESIAN_POINT ( 'NONE',  ( -10.68949850836979820, -78.61016907666331122, -1.353545228532917699 ) ) ;
#48707 = ORIENTED_EDGE ( 'NONE', *, *, #6635, .F. ) ;
#48708 = CARTESIAN_POINT ( 'NONE',  ( 7.092659876394000307, -77.99803084965400046, 6.312768414564000174 ) ) ;
#48709 = VECTOR ( 'NONE', #36263, 1000.000000000000000 ) ;
#48710 = CARTESIAN_POINT ( 'NONE',  ( 0.000000000000000000, -75.67500000000001137, 0.000000000000000000 ) ) ;
#48711 = CARTESIAN_POINT ( 'NONE',  ( 0.4901547383881838527, -80.25723238900481249, -1.149788170831134382 ) ) ;
#48712 = CARTESIAN_POINT ( 'NONE',  ( 11.77596950146999966, -77.36568903011000486, 5.402702954953999992 ) ) ;
#48713 = UNCERTAINTY_MEASURE_WITH_UNIT (LENGTH_MEASURE( 1.000000000000000082E-05 ), #24611, 'distance_accuracy_value', 'NONE');
#48714 = AXIS2_PLACEMENT_3D ( 'NONE', #25055, #47235, #6763 ) ;
#48715 = CARTESIAN_POINT ( 'NONE',  ( 10.75916580683999690, -78.02281159953585643, 3.171507801093999657 ) ) ;
#48716 = CARTESIAN_POINT ( 'NONE',  ( 3.451879464910831974, -86.39318692756698681, -1.536875756006378824 ) ) ;
#48717 = CARTESIAN_POINT ( 'NONE',  ( 1.250000000000000000, -82.84999999999999432, 0.000000000000000000 ) ) ;
#48718 = CARTESIAN_POINT ( 'NONE',  ( 4.044174147134872221, -79.93931354737067352, 8.336790591702616382 ) ) ;
#48719 = CIRCLE ( 'NONE', #23269, 1.750000000000001998 ) ;
#48720 = CARTESIAN_POINT ( 'NONE',  ( 8.803761571639995509, -16.78431590350725244, 9.164326402704537244 ) ) ;
#48721 = ORIENTED_EDGE ( 'NONE', *, *, #31004, .T. ) ;
#48722 = CARTESIAN_POINT ( 'NONE',  ( 2.863093780795163745, -77.25021378612967737, -8.795631279814358550 ) ) ;
#48723 = CARTESIAN_POINT ( 'NONE',  ( 1.299878529918000014, -80.47826946565700723, -0.2255693107841999778 ) ) ;
#48724 = VECTOR ( 'NONE', #51254, 1000.000000000000000 ) ;
#48725 = CARTESIAN_POINT ( 'NONE',  ( -12.60356226362999976, -19.24922971138999728, -1.750000000000000000 ) ) ;
#48726 = CARTESIAN_POINT ( 'NONE',  ( -0.1108284043172000077, -77.77636455657749082, -1.314634435239000032 ) ) ;
#48727 = CARTESIAN_POINT ( 'NONE',  ( 2.281100415086936284, -3.030341629373181078, -2.679643809356492490 ) ) ;
#48728 = CARTESIAN_POINT ( 'NONE',  ( 0.000000000000000000, -80.74999999986198418, 0.000000000000000000 ) ) ;
#48729 = CARTESIAN_POINT ( 'NONE',  ( 11.75000000000000000, -77.45000000000000284, 1.043320980279999928E-14 ) ) ;
#48730 = DIRECTION ( 'NONE',  ( 0.000000000000000000, 1.000000000000000000, 0.000000000000000000 ) ) ;
#48731 = CARTESIAN_POINT ( 'NONE',  ( -1.319038368507000181, -78.67250824667499387, -11.07933831235000177 ) ) ;
#48732 = CARTESIAN_POINT ( 'NONE',  ( 7.648026766715999791, -55.54999999381000464, 10.12290050087000104 ) ) ;
#48733 = CARTESIAN_POINT ( 'NONE',  ( -1.155223306477086931, -83.06892497275070752, 0.4772783199500317819 ) ) ;
#48734 = CARTESIAN_POINT ( 'NONE',  ( -1.405194841723999888, -81.98044359648298496, -3.928806027564999859 ) ) ;
#48735 = B_SPLINE_CURVE_WITH_KNOTS ( 'NONE', 3,
 ( #43677, #20373, #38367, #2941, #56389, #15939, #20658, #33927, #11523, #29500, #56676, #38942, #47835, #16520, #34501, #13827, #31825, #36266 ),
 .UNSPECIFIED., .F., .F.,
 ( 4, 2, 2, 2, 2, 2, 2, 2, 4 ),
 ( 0.000000000000000000, 0.1250000000000000000, 0.2500000000000000000, 0.3750000000000000000, 0.5000000000000000000, 0.6250000000000000000, 0.7500000000000000000, 0.8750000000000000000, 1.000000000000000000 ),
 .UNSPECIFIED. ) ;
#48736 = ORIENTED_EDGE ( 'NONE', *, *, #53504, .F. ) ;
#48737 = CARTESIAN_POINT ( 'NONE',  ( 0.6735630312197999903, -83.05325357425300581, -1.435516540950999786 ) ) ;
#48738 = CARTESIAN_POINT ( 'NONE',  ( -0.5136231202413000796, -81.42600413218998767, 1.249846006485000105 ) ) ;
#48739 = DIRECTION ( 'NONE',  ( 0.7071067811865975328, -0.7071067811864976127, 8.872297124978962287E-10 ) ) ;
#48740 = CARTESIAN_POINT ( 'NONE',  ( -9.964549960864999889, -77.45148636095500194, 6.650098383618000319 ) ) ;
#48741 = CARTESIAN_POINT ( 'NONE',  ( 4.511829301271795600, -77.00000000000001421, 8.104544903090385333 ) ) ;
#48742 = EDGE_CURVE ( 'NONE', #21248, #51275, #4078, .T. ) ;
#48743 = CARTESIAN_POINT ( 'NONE',  ( 0.5269479332349999989, -83.11978140203299859, 1.580352090963000000 ) ) ;
#48744 = CARTESIAN_POINT ( 'NONE',  ( 12.90000000000000036, -5.900000000000010125, 0.000000000000000000 ) ) ;
#48745 = CARTESIAN_POINT ( 'NONE',  ( 9.377128579935000374, -78.41885584965399403, -2.571625947824999869 ) ) ;
#48746 = CARTESIAN_POINT ( 'NONE',  ( -2.019183793707000074, -55.01279722724000010, -12.79944116701999768 ) ) ;
#48747 = CARTESIAN_POINT ( 'NONE',  ( 9.783314345684438251, -75.99666901279969977, 6.507558209343685895 ) ) ;
#48748 = CARTESIAN_POINT ( 'NONE',  ( -2.739132899391135911, -85.94828561723799965, 3.697400121254065919 ) ) ;
#48749 = ORIENTED_EDGE ( 'NONE', *, *, #35628, .F. ) ;
#48750 = CARTESIAN_POINT ( 'NONE',  ( -0.4767998270009902728, -79.59439922511664633, -1.192942613436671406 ) ) ;
#48751 = CARTESIAN_POINT ( 'NONE',  ( -1.250000000000000000, -76.50000000000000000, 0.000000000000000000 ) ) ;
#48752 = CARTESIAN_POINT ( 'NONE',  ( -9.675565990256998816, -79.27387249041099437, 7.547703503149000070 ) ) ;
#48753 = DIRECTION ( 'NONE',  ( 0.9999999929803531362, 0.000000000000000000, 0.0001184875252606944153 ) ) ;
#48754 = CARTESIAN_POINT ( 'NONE',  ( 2.550499813263000348, -78.57381419345199447, -10.67515654612000020 ) ) ;
#48755 = CARTESIAN_POINT ( 'NONE',  ( 1.980610890452897399, -18.47926110520256771, 12.74374574607350574 ) ) ;
#48756 = CARTESIAN_POINT ( 'NONE',  ( 11.93738031268999933, -76.74029815165599189, -2.836636764837000335 ) ) ;
#48757 = DIRECTION ( 'NONE',  ( 0.000000000000000000, 0.000000000000000000, -1.000000000000000000 ) ) ;
#48758 = CARTESIAN_POINT ( 'NONE',  ( 0.000000000000000000, -74.70999999999999375, 0.000000000000000000 ) ) ;
#48759 = ORIENTED_EDGE ( 'NONE', *, *, #6979, .T. ) ;
#48760 = VECTOR ( 'NONE', #27366, 1000.000000000000000 ) ;
#48761 = CARTESIAN_POINT ( 'NONE',  ( -7.180765598437999664, -79.07253981239199447, 8.374863569145000852 ) ) ;
#48762 = CARTESIAN_POINT ( 'NONE',  ( 0.8738424494231588069, -79.91383025740681489, 0.8934342867657290022 ) ) ;
#48763 = CARTESIAN_POINT ( 'NONE',  ( 12.00000000000000000, -75.80000000000001137, -2.990830162875999918E-13 ) ) ;
#48764 = VECTOR ( 'NONE', #127, 1000.000000000000000 ) ;
#48765 = CIRCLE ( 'NONE', #22331, 1.750000000000000000 ) ;
#48766 = CARTESIAN_POINT ( 'NONE',  ( 11.04877620194000087, -78.05730764035098446, 0.05135089858452999978 ) ) ;
#48767 = EDGE_CURVE ( 'NONE', #47851, #24723, #17649, .T. ) ;
#48768 = LINE ( 'NONE', #26590, #55244 ) ;
#48769 = VECTOR ( 'NONE', #6291, 1000.000000000000000 ) ;
#48770 = CARTESIAN_POINT ( 'NONE',  ( 10.99607952894010054, -23.68503250286068607, -0.3139933498775518417 ) ) ;
#48771 = CARTESIAN_POINT ( 'NONE',  ( -10.88187945745999841, -78.86493240443898856, -5.690384754473000406 ) ) ;
#48772 = CARTESIAN_POINT ( 'NONE',  ( 13.99999999961999819, -72.70000000038000110, -1.691901775850999968E-09 ) ) ;
#48773 = CARTESIAN_POINT ( 'NONE',  ( 7.137508353459040222, -79.51917351108399146, 8.454853940648140664 ) ) ;
#48774 =( NAMED_UNIT ( * ) PLANE_ANGLE_UNIT ( ) SI_UNIT ( $, .RADIAN. ) );
#48775 = CARTESIAN_POINT ( 'NONE',  ( 8.485281374238999419, 0.000000000000000000, 8.485281374238999419 ) ) ;
#48776 = ORIENTED_EDGE ( 'NONE', *, *, #22302, .F. ) ;
#48777 = EDGE_CURVE ( 'NONE', #35786, #470, #36873, .T. ) ;
#48778 = EDGE_LOOP ( 'NONE', ( #2311, #34447, #36785, #35465, #8392, #53457 ) ) ;
#48779 = CARTESIAN_POINT ( 'NONE',  ( -9.500000000000001776, -78.41041666666669130, -1.243547092045959923 ) ) ;
#48780 = ORIENTED_EDGE ( 'NONE', *, *, #12574, .T. ) ;
#48781 = CARTESIAN_POINT ( 'NONE',  ( 1.102440175093327257, -79.61576928092233629, 9.466448183039451791 ) ) ;
#48782 = ORIENTED_EDGE ( 'NONE', *, *, #45387, .T. ) ;
#48783 = CARTESIAN_POINT ( 'NONE',  ( 9.101516360816999551, -24.88066799059000189, 8.485522730740999720 ) ) ;
#48784 = CARTESIAN_POINT ( 'NONE',  ( 3.947457275559000500, -78.29525648518600178, -10.30140706531999939 ) ) ;
#48785 = CARTESIAN_POINT ( 'NONE',  ( -10.42531124905999995, -18.73514851523999880, 7.624341765453999997 ) ) ;
#48786 = CARTESIAN_POINT ( 'NONE',  ( -5.137220513087188856, -78.17816639323106642, -7.692279124526338663 ) ) ;
#48787 = CARTESIAN_POINT ( 'NONE',  ( 6.766402264611000028, -79.37484760169999731, -8.946167390840999545 ) ) ;
#48788 = ORIENTED_EDGE ( 'NONE', *, *, #39465, .F. ) ;
#48789 = ORIENTED_EDGE ( 'NONE', *, *, #35413, .F. ) ;
#48790 = CARTESIAN_POINT ( 'NONE',  ( -4.333990198683386197, -77.51391215394883716, 8.171957043909507945 ) ) ;
#48791 = CARTESIAN_POINT ( 'NONE',  ( -4.789974786805000662, -77.89883254012598002, -9.946872946892002076 ) ) ;
#48792 = CIRCLE ( 'NONE', #35581, 1.749999999999998890 ) ;
#48793 = CARTESIAN_POINT ( 'NONE',  ( 9.583411031200000707, -78.15302099854598339, 1.526087275887999972 ) ) ;
#48794 = CARTESIAN_POINT ( 'NONE',  ( 10.49984016500000017, -76.62494580621000750, -6.347025226577000190 ) ) ;
#48795 = CARTESIAN_POINT ( 'NONE',  ( 3.250000000000000000, -2.250000000000000000, 0.000000000000000000 ) ) ;
#48796 = DIRECTION ( 'NONE',  ( 0.7071067811865475727, 0.000000000000000000, -0.7071067811865475727 ) ) ;
#48797 = CARTESIAN_POINT ( 'NONE',  ( -1.870137171474999915, -80.10216999377799141, -11.09839649295000008 ) ) ;
#48798 = FACE_OUTER_BOUND ( 'NONE', #36500, .T. ) ;
#48799 = CARTESIAN_POINT ( 'NONE',  ( -1.092232985442822102, -78.04166666666664298, -0.6295237254636245616 ) ) ;
#48800 = CIRCLE ( 'NONE', #17696, 9.700000000000001066 ) ;
#48801 = CARTESIAN_POINT ( 'NONE',  ( 8.082524092276891281, -78.70833333333332860, -4.658475568430806568 ) ) ;
#48802 = ORIENTED_EDGE ( 'NONE', *, *, #10590, .T. ) ;
#48803 = CARTESIAN_POINT ( 'NONE',  ( -1.760068246105999989, -79.96322189244729373, 11.95491093743999933 ) ) ;
#48804 = CONICAL_SURFACE ( 'NONE', #26166, 3.899999999992999733, 0.7853981633972997312 ) ;
#48805 = CARTESIAN_POINT ( 'NONE',  ( -8.588893914397997875, -53.66760216274000328, 9.317954957978999531 ) ) ;
#48806 = CARTESIAN_POINT ( 'NONE',  ( -1.199999999999999956, -75.00000000000000000, 7.200000000000000178 ) ) ;
#48807 = CARTESIAN_POINT ( 'NONE',  ( -12.74331206683534390, -60.32649290773906614, 1.980611467281705229 ) ) ;
#48808 = EDGE_CURVE ( 'NONE', #3715, #31099, #12914, .T. ) ;
#48810 = CARTESIAN_POINT ( 'NONE',  ( -1.798954018882000128, -18.78469026612999926, -12.61117007302000026 ) ) ;
#48809 = CARTESIAN_POINT ( 'NONE',  ( 7.627487606591000002, -55.50221404479999876, 10.35845616725999996 ) ) ;
#48811 = AXIS2_PLACEMENT_3D ( 'NONE', #35668, #35075, #8822 ) ;
#48812 = DIRECTION ( 'NONE',  ( 1.000000000000000000, 0.000000000000000000, 1.147001872820999768E-14 ) ) ;
#48813 = CARTESIAN_POINT ( 'NONE',  ( -10.82681686033000013, -80.56778745972700051, -1.485342682486999966 ) ) ;
#48814 = CARTESIAN_POINT ( 'NONE',  ( 11.19999999861000006, -74.79999999860999083, 9.230036577774000073E-09 ) ) ;
#48815 = CARTESIAN_POINT ( 'NONE',  ( -3.647741209468000179, -77.22465764268899591, 10.65494948965999988 ) ) ;
#48816 = FACE_OUTER_BOUND ( 'NONE', #55164, .T. ) ;
#48817 = CARTESIAN_POINT ( 'NONE',  ( 7.443430083705999678, -80.64091113825868717, 8.443285209763999433 ) ) ;
#48818 = EDGE_CURVE ( 'NONE', #12545, #5875, #27040, .T. ) ;
#48819 = ORIENTED_EDGE ( 'NONE', *, *, #19355, .F. ) ;
#48820 = CARTESIAN_POINT ( 'NONE',  ( -11.79999999988000070, -23.14999999478999726, 0.5999999998848000171 ) ) ;
#48821 = CARTESIAN_POINT ( 'NONE',  ( -0.8445585116460000430, -54.08959556723999640, 12.43380736233000050 ) ) ;
#48822 = CARTESIAN_POINT ( 'NONE',  ( -12.75763395695999947, -22.77795407709999864, 1.931043742978000077 ) ) ;
#48823 = CARTESIAN_POINT ( 'NONE',  ( 3.208820596785000312, -1.826303692333000050, 1.361140077406000071 ) ) ;
#48824 = CARTESIAN_POINT ( 'NONE',  ( 0.2654799511899000319, -78.32520084447600084, -11.21373274707999990 ) ) ;
#48825 = CARTESIAN_POINT ( 'NONE',  ( 3.250000000000000000, -1.750000000000000000, 0.000000000000000000 ) ) ;
#48826 = CARTESIAN_POINT ( 'NONE',  ( 2.574080585026614187, -77.24375000000003411, -10.72942207085831079 ) ) ;
#48827 = CARTESIAN_POINT ( 'NONE',  ( 0.4701041210467000186, -61.80796934391000264, 12.54901038419999892 ) ) ;
#48828 = CARTESIAN_POINT ( 'NONE',  ( 12.66235371498999918, -16.86260492134000089, 0.4957155363045000485 ) ) ;
#48829 = CARTESIAN_POINT ( 'NONE',  ( -0.7865880339533001253, -84.42674735065199343, 4.100107199207999820 ) ) ;
#48830 = CARTESIAN_POINT ( 'NONE',  ( 12.90000000000000036, 0.000000000000000000, 0.000000000000000000 ) ) ;
#48831 = CARTESIAN_POINT ( 'NONE',  ( 9.499157866768639380, -79.10080562451891240, 0.1004279358040388037 ) ) ;
#48832 = B_SPLINE_SURFACE_WITH_KNOTS ( 'NONE', 3, 3, ( 
 ( #34498, #8511, #57815, #53386, #53104, #57524, #48681, #3512, #3795, #21513, #30066, #52814, #12932, #17674, #35660, #22084, #38939, #48398, #48117 ),
 ( #7649, #43674, #2938, #40098, #44243, #44531, #53691, #12653, #58111, #13229, #39802, #7363, #48970, #57241, #8225, #20937, #21223, #56956, #21797 ),
 ( #25648, #17374, #39228, #26505, #16805, #12369, #34790, #35361, #30357, #7935, #43962, #39519, #9408, #36556, #37133, #36843, #53989, #54855, #18850 ),
 ( #19139, #27398, #5546, #13527, #34769, #8813, #14402, #49568, #27976, #55144, #41572, #54578, #26805, #13824, #18565, #9115, #22982, #46025, #22389 ) ),
 .UNSPECIFIED., .F., .F., .F.,
 ( 4, 4 ),
 ( 4, 1, 1, 1, 1, 1, 1, 1, 1, 1, 1, 1, 1, 1, 1, 1, 4 ),
 ( -0.3708084972812999980, 1.370808497280999960 ),
 ( -0.01016343285802999950, 0.02286772393056000011, 0.05589888071915000145, 0.08893003750774999827, 0.1219611942962999934, 0.1549923510849000041, 0.1880235078735000009, 0.2210546646621000255, 0.2540858214506999668, 0.2871169782393000469, 0.3201481350279000160, 0.3531792918164999850, 0.3862104486051000096, 0.4192416053937000342, 0.4522727621821999722, 0.4853039189707999967, 0.5183350757593999658 ),
 .UNSPECIFIED. ) ;
#48833 = CARTESIAN_POINT ( 'NONE',  ( 6.355487164442999770, -78.10387449799000592, 9.297405415548999130 ) ) ;
#48834 = ADVANCED_FACE ( 'NONE', ( #30912 ), #19188, .F. ) ;
#48835 = CARTESIAN_POINT ( 'NONE',  ( -0.03524841727520977575, -81.97784558154000933, 1.249284716020608421 ) ) ;
#48836 = CARTESIAN_POINT ( 'NONE',  ( -0.8529715180118000450, -77.81475764398999218, 1.292944160158000066 ) ) ;
#48837 = CARTESIAN_POINT ( 'NONE',  ( 5.212684961665999595, -77.06074883803579212, -8.147089634514999901 ) ) ;
#48838 = CARTESIAN_POINT ( 'NONE',  ( -0.9512744292220589593, -83.17914831638273654, 1.173546308381462122 ) ) ;
#48839 = CARTESIAN_POINT ( 'NONE',  ( -12.83836863002999884, -60.00626272179999887, 2.062146390631000248 ) ) ;
#48840 = CARTESIAN_POINT ( 'NONE',  ( -5.888313336375618157, -80.17893371189863672, -8.993908195848307585 ) ) ;
#48841 = CARTESIAN_POINT ( 'NONE',  ( -2.500000000000000000, -80.69999999999998863, 0.000000000000000000 ) ) ;
#48842 = CARTESIAN_POINT ( 'NONE',  ( -7.610436392414960061, -18.47459049293312816, -10.41144384038885207 ) ) ;
#48843 = CARTESIAN_POINT ( 'NONE',  ( 0.5039928918671183755, -81.75818078180917325, -1.143829648980971836 ) ) ;
#48844 = CARTESIAN_POINT ( 'NONE',  ( 0.000000000000000000, -2.660000000000000142, 0.000000000000000000 ) ) ;
#48845 = DIRECTION ( 'NONE',  ( 0.000000000000000000, -1.000000000000000000, 0.000000000000000000 ) ) ;
#48846 = CARTESIAN_POINT ( 'NONE',  ( 10.56386067434198317, -78.73297245124483368, -2.300023321096129614 ) ) ;
#48847 = EDGE_LOOP ( 'NONE', ( #14425, #27558 ) ) ;
#48848 = EDGE_CURVE ( 'NONE', #16033, #45960, #23498, .T. ) ;
#48849 = ORIENTED_EDGE ( 'NONE', *, *, #44879, .T. ) ;
#48850 = CARTESIAN_POINT ( 'NONE',  ( -1.169332518864999892, -82.05248746382200409, -1.113388286646999958 ) ) ;
#48851 = EDGE_CURVE ( 'NONE', #3682, #15743, #34768, .T. ) ;
#48852 = EDGE_LOOP ( 'NONE', ( #24380, #52521, #13983, #47138, #23217, #17367 ) ) ;
#48853 = CARTESIAN_POINT ( 'NONE',  ( 0.000000000000000000, -32.70420297070000260, 0.000000000000000000 ) ) ;
#48854 = ORIENTED_EDGE ( 'NONE', *, *, #34778, .F. ) ;
#48855 = DIRECTION ( 'NONE',  ( 1.000000000000000000, 0.000000000000000000, 0.000000000000000000 ) ) ;
#48856 = CIRCLE ( 'NONE', #56400, 5.299999999999999822 ) ;
#48857 = CARTESIAN_POINT ( 'NONE',  ( 0.6938652518923514867, -79.12395832888063296, -3.339787257827266043 ) ) ;
#48858 = CARTESIAN_POINT ( 'NONE',  ( 9.789168614380999500, -78.78692200396399414, -4.831929617604999727 ) ) ;
#48859 = CARTESIAN_POINT ( 'NONE',  ( -11.99999999994999911, -76.29999999994899440, 3.078392110872999642E-09 ) ) ;
#48860 = CARTESIAN_POINT ( 'NONE',  ( -3.617892441770000023, -78.93070212325169166, 1.159015290449999958 ) ) ;
#48861 = CARTESIAN_POINT ( 'NONE',  ( -5.443693558267039379, -79.32340947642325091, 7.785673846661049780 ) ) ;
#48862 = ORIENTED_EDGE ( 'NONE', *, *, #51247, .F. ) ;
#48863 = DIRECTION ( 'NONE',  ( 0.7071067811865474617, 0.7071067811865474617, -1.168837077090079199E-09 ) ) ;
#48864 = CARTESIAN_POINT ( 'NONE',  ( 8.504094770722000263, -78.69101207264999687, -8.967282323152000245 ) ) ;
#48865 = ORIENTED_EDGE ( 'NONE', *, *, #56821, .T. ) ;
#48866 = VERTEX_POINT ( 'NONE', #9677 ) ;
#48867 = CARTESIAN_POINT ( 'NONE',  ( 4.765028101803320482, -79.46666666666665435, -8.256991974504542142 ) ) ;
#48868 = B_SPLINE_SURFACE_WITH_KNOTS ( 'NONE', 3, 3, ( 
 ( #6260, #47317, #19269, #24275, #42293, #41700, #1858, #14820, #19853, #37848, #47027, #6557, #24565, #20147, #38134, #39294, #44304, #43164, #7427, #52310, #26291, #3860, #29843, #48745, #11579, #8288, #57587, #53166, #25430, #16869, #7137, #52595, #21858, #30708, #29558 ),
 ( #43445, #21002, #16578, #39867, #48459, #57306, #47613, #57880, #39583, #30133, #34848, #17437, #17148, #16298, #35135, #12715, #52880, #35422, #48182, #25138, #34275, #20717, #2721, #38717, #11866, #56738, #47895, #3006, #25999, #39008, #57016, #34563, #12146, #7715, #25716 ),
 ( #12434, #43742, #30427, #3295, #21287, #8002, #44022, #3574, #21579, #31877, #49921, #10563, #9466, #49328, #27451, #22152, #31580, #42144, #54343, #6121, #348, #4448, #26868, #44599, #13883, #58173, #51013, #24126, #22449, #46595, #4153, #40464, #17739, #49626, #45489 ),
 ( #40160, #28546, #19706, #1713, #53452, #22744, #5032, #9173, #23034, #41050, #40754, #18327, #35727, #55426, #1426, #19415, #13291, #37405, #26567, #36320, #56, #14972, #53754, #27156, #12997, #32969, #30994, #49032, #18031, #44896, #31285, #8580, #8874, #36023, #54050 ) ),
 .UNSPECIFIED., .F., .F., .F.,
 ( 4, 4 ),
 ( 4, 1, 1, 1, 1, 1, 1, 1, 1, 1, 1, 1, 1, 1, 1, 1, 1, 1, 1, 1, 1, 1, 1, 1, 1, 1, 1, 1, 1, 1, 1, 1, 4 ),
 ( -0.4015584965371999937, 1.401558496537000043 ),
 ( -0.02000000000000000042, 0.01250000000000000069, 0.04499999999999999833, 0.07749999999999999944, 0.1100000000000000006, 0.1424999999999999878, 0.1749999999999999889, 0.2074999999999999900, 0.2399999999999999911, 0.2725000000000000200, 0.3049999999999999933, 0.3375000000000000222, 0.3699999999999999956, 0.4025000000000000244, 0.4349999999999999978, 0.4675000000000000266, 0.5000000000000000000, 0.5324999999999999734, 0.5649999999999999467, 0.5975000000000000311, 0.6300000000000000044, 0.6624999999999999778, 0.6949999999999999512, 0.7275000000000000355, 0.7600000000000000089, 0.7924999999999999822, 0.8249999999999999556, 0.8575000000000000400, 0.8900000000000000133, 0.9224999999999999867, 0.9549999999999999600, 0.9875000000000000444, 1.020000000000000018 ),
 .UNSPECIFIED. ) ;
#48869 = CARTESIAN_POINT ( 'NONE',  ( -0.6056189234361001317, -80.35315015347299550, -1.188192690176999911 ) ) ;
#48870 = DIRECTION ( 'NONE',  ( -0.7071067811865475727, 0.000000000000000000, 0.7071067811865475727 ) ) ;
#48871 = ADVANCED_FACE ( 'NONE', ( #845 ), #23250, .T. ) ;
#48872 = CARTESIAN_POINT ( 'NONE',  ( 2.544856321172368485, -86.39318692756700102, -3.574083091624765007 ) ) ;
#48873 = CARTESIAN_POINT ( 'NONE',  ( 0.000000000000000000, -81.99999999999998579, 0.000000000000000000 ) ) ;
#48874 = CARTESIAN_POINT ( 'NONE',  ( -9.412102823527000339, -78.06691570303000560, -9.131157420175998851 ) ) ;
#48875 = CARTESIAN_POINT ( 'NONE',  ( -7.818192365797999699, -78.17570409358999939, 9.061685001942999307 ) ) ;
#48876 = DIRECTION ( 'NONE',  ( 0.000000000000000000, 1.000000000000000000, 0.000000000000000000 ) ) ;
#48877 = CARTESIAN_POINT ( 'NONE',  ( -9.102064877486805372, -78.61442264338772645, -1.647833208901029689 ) ) ;
#48878 = CARTESIAN_POINT ( 'NONE',  ( 1.539486242883999934, -80.97495933943199020, -3.651845052344000031 ) ) ;
#48879 = CARTESIAN_POINT ( 'NONE',  ( 10.14999999998000035, -87.10000000002298748, -2.878934427392999978E-10 ) ) ;
#48880 = CARTESIAN_POINT ( 'NONE',  ( -1.389309474284118329, -3.011527199678093680, 2.937373092524380169 ) ) ;
#48881 = CARTESIAN_POINT ( 'NONE',  ( -0.3707676657765999750, -80.56255496681198736, -3.527618700040000110 ) ) ;
#48882 = EDGE_CURVE ( 'NONE', #29606, #22997, #6823, .T. ) ;
#48883 = CIRCLE ( 'NONE', #23427, 2.899999999999999911 ) ;
#48884 = DIRECTION ( 'NONE',  ( 0.000000000000000000, 0.000000000000000000, -1.000000000000000000 ) ) ;
#48885 = CARTESIAN_POINT ( 'NONE',  ( -1.002682972311154996, -80.98253985172503633, 10.70322111416496469 ) ) ;
#48886 = CARTESIAN_POINT ( 'NONE',  ( 11.14639666075000157, -81.14010679683600813, -1.632917082138999776 ) ) ;
#48887 = CARTESIAN_POINT ( 'NONE',  ( 2.534829140202000008, -2.065001425904999799, 2.839140403359000420 ) ) ;
#48888 = CARTESIAN_POINT ( 'NONE',  ( -0.01872084306268049364, -79.62656959496065667, 1.274104374990254973 ) ) ;
#48889 = ADVANCED_FACE ( 'NONE', ( #38984 ), #11558, .T. ) ;
#48890 = VERTEX_POINT ( 'NONE', #7691 ) ;
#48891 = DIRECTION ( 'NONE',  ( -1.000000000000000000, 0.000000000000000000, 0.000000000000000000 ) ) ;
#48892 = B_SPLINE_CURVE_WITH_KNOTS ( 'NONE', 3,
 ( #48473, #51756, #20737, #2448 ),
 .UNSPECIFIED., .F., .F.,
 ( 4, 4 ),
 ( 0.000000000000000000, 1.000000000000000000 ),
 .UNSPECIFIED. ) ;
#48893 = CARTESIAN_POINT ( 'NONE',  ( -11.00000000000000000, -79.19999999999998863, 0.000000000000000000 ) ) ;
#48894 = CARTESIAN_POINT ( 'NONE',  ( 0.2153359604882000011, -81.99643347552201078, 1.316133176457000120 ) ) ;
#48895 = CARTESIAN_POINT ( 'NONE',  ( -12.43410192431999839, -17.55868879885999689, -1.192687910177000044 ) ) ;
#48896 = CARTESIAN_POINT ( 'NONE',  ( -9.287618194362000423, -77.54441932644999724, -9.114789584104999065 ) ) ;
#48897 = VECTOR ( 'NONE', #50259, 1000.000000000000114 ) ;
#48898 = CARTESIAN_POINT ( 'NONE',  ( 8.119885838724000493, -79.78146001420199696, -4.358224697923000157 ) ) ;
#48899 = CARTESIAN_POINT ( 'NONE',  ( -5.893333102785000222, -76.58035197021000329, -11.03757542588999918 ) ) ;
#48900 = EDGE_LOOP ( 'NONE', ( #758, #30164, #3516, #2889 ) ) ;
#48901 = CARTESIAN_POINT ( 'NONE',  ( -10.12290050122000018, -55.54999999974999980, 7.648026767069000087 ) ) ;
#48902 = CARTESIAN_POINT ( 'NONE',  ( -9.397814129314344456, -79.70741671815727614, 5.554578354712478294 ) ) ;
#48903 = CARTESIAN_POINT ( 'NONE',  ( -1.271707153813000035, -81.76195542696700613, 0.6054370633115999656 ) ) ;
#48904 = CARTESIAN_POINT ( 'NONE',  ( -7.374560639698973574, -78.97291666666667709, -9.596002108778167283 ) ) ;
#48905 = CARTESIAN_POINT ( 'NONE',  ( 5.254748191175000471, -79.19294275334198119, -7.810174947890000219 ) ) ;
#48906 = CARTESIAN_POINT ( 'NONE',  ( 3.674917764513000229, -85.35108058741198533, -1.975230324880000277 ) ) ;
#48907 = CARTESIAN_POINT ( 'NONE',  ( 1.888467876749918561, -79.96132589731932683, 10.58272476696118147 ) ) ;
#48908 = CARTESIAN_POINT ( 'NONE',  ( 1.040651332726000078, -79.79327398392099724, -0.9628624948066000222 ) ) ;
#48909 = VERTEX_POINT ( 'NONE', #29536 ) ;
#48910 = CARTESIAN_POINT ( 'NONE',  ( 7.661146283331804696, -77.28829716686190920, -7.541047385534751513 ) ) ;
#48911 = CARTESIAN_POINT ( 'NONE',  ( -1.115313966523381550, -82.22395833333196435, 0.6418514623139731645 ) ) ;
#48912 = CARTESIAN_POINT ( 'NONE',  ( 0.8935345625127607549, -78.91502747134597939, -3.805630735094382988 ) ) ;
#48913 = ORIENTED_EDGE ( 'NONE', *, *, #50687, .T. ) ;
#48914 = ORIENTED_EDGE ( 'NONE', *, *, #45640, .F. ) ;
#48915 = CARTESIAN_POINT ( 'NONE',  ( 2.542269563431000190, -78.51447634179098145, -10.64070870773999822 ) ) ;
#48916 = CARTESIAN_POINT ( 'NONE',  ( -7.342331066867000544, -55.64999999967000122, -8.190859204290999784 ) ) ;
#48917 = B_SPLINE_CURVE_WITH_KNOTS ( 'NONE', 3,
 ( #54670, #5941, #9505, #55839, #5364, #23371, #19528, #680, #55539, #23946, #32788, #10682, #28663, #50836, #15389, #10381, #46124, #50249, #41962, #1535, #49964, #37521, #41382, #15090, #18663, #28075, #37818, #28366, #1830, #55247, #965, #18948, #41089, #46412, #14211, #46712, #19826, #36941, #42264, #36651, #54952, #51129, #33085, #6232, #45533, #14504, #5648, #27492, #32208, #5079, #24248, #37230, #14793, #23074, #9800, #19238, #27783, #32495, #50542, #10095, #23657, #41670, #1250, #2401, #33959 ),
 .UNSPECIFIED., .F., .F.,
 ( 4, 1, 1, 1, 1, 1, 1, 1, 1, 1, 1, 1, 1, 1, 1, 1, 1, 1, 1, 1, 1, 1, 1, 1, 1, 1, 1, 1, 1, 1, 1, 1, 1, 1, 1, 1, 1, 1, 1, 1, 1, 1, 1, 1, 1, 1, 1, 1, 1, 1, 1, 1, 1, 1, 1, 1, 1, 1, 1, 1, 1, 1, 4 ),
 ( 0.000000000000000000, 0.01249978245764908277, 0.02874978979738820883, 0.04499979713712733143, 0.06124980447686646096, 0.07749981181660559049, 0.09374981915634472696, 0.1099998264960838495, 0.1262498338358229721, 0.1424998411755621086, 0.1587498485153012451, 0.1749998558550403538, 0.1912498631947794903, 0.2074998705345185990, 0.2237498778742577632, 0.2399998852139968719, 0.2562498925537359806, 0.2724998998934751171, 0.2887499072332142536, 0.3049999145729533345, 0.3212499219126924710, 0.3374999292524316630, 0.3537499365921707439, 0.3699999439319098804, 0.3862499512716489614, 0.4024999586113881533, 0.4187499659511272898, 0.4349999732908663708, 0.4512499806306055072, 0.4674999879703446437, 0.4837499953100837802, 0.5000000026498229166, 0.5162500099895620531, 0.5325000173293011896, 0.5487500246690403261, 0.5650000320087793515, 0.5812500393485185990, 0.5975000466882577355, 0.6137500540279968719, 0.6300000613677360084, 0.6462500687074750338, 0.6625000760472141703, 0.6787500833869533068, 0.6950000907266924433, 0.7112500980664316907, 0.7275001054061708272, 0.7437501127459098527, 0.7600001200856489891, 0.7762501274253881256, 0.7925001347651272621, 0.8087501421048663985, 0.8250001494446054240, 0.8412501567843446715, 0.8575001641240838079, 0.8737501714638229444, 0.8900001788035620809, 0.9062501861433011063, 0.9225001934830402428, 0.9387502008227793793, 0.9550002081625185157, 0.9712502155022576522, 0.9875002228419967887, 1.000000000000000000 ),
 .UNSPECIFIED. ) ;
#48918 = CARTESIAN_POINT ( 'NONE',  ( -10.62639753186000036, -79.83513114498597929, -3.930700632546999529 ) ) ;
#48919 = VERTEX_POINT ( 'NONE', #20980 ) ;
#48920 = ORIENTED_EDGE ( 'NONE', *, *, #23668, .T. ) ;
#48921 = ORIENTED_EDGE ( 'NONE', *, *, #46836, .T. ) ;
#48922 = AXIS2_PLACEMENT_3D ( 'NONE', #38632, #11778, #47807 ) ;
#48923 = CARTESIAN_POINT ( 'NONE',  ( 6.043450171152322525, -76.56602488911100579, -10.48647902363864048 ) ) ;
#48924 = LINE ( 'NONE', #39478, #14785 ) ;
#48925 = VERTEX_POINT ( 'NONE', #24834 ) ;
#48926 = CARTESIAN_POINT ( 'NONE',  ( 1.412760417132294943, -82.08723958285546018, -0.1840777080652946651 ) ) ;
#48927 = ORIENTED_EDGE ( 'NONE', *, *, #16172, .F. ) ;
#48928 = CARTESIAN_POINT ( 'NONE',  ( -0.7578051741271042419, -80.57587266093590017, 1.024356917418570267 ) ) ;
#48929 = CARTESIAN_POINT ( 'NONE',  ( 3.548349909811000735, -78.96264282632948550, -1.307818870560639724E-15 ) ) ;
#48930 = PLANE ( 'NONE',  #57604 ) ;
#48931 = EDGE_CURVE ( 'NONE', #32213, #10018, #20410, .T. ) ;
#48932 = CARTESIAN_POINT ( 'NONE',  ( 0.5245219981312709834, -18.54839576652498323, 10.98753021428709253 ) ) ;
#48933 = CARTESIAN_POINT ( 'NONE',  ( 1.229229938689273993, -79.60286458332932114, 9.397135416583925149 ) ) ;
#48934 = EDGE_CURVE ( 'NONE', #21614, #54902, #28609, .T. ) ;
#48935 = CARTESIAN_POINT ( 'NONE',  ( -1.749722766161712073, -55.32411007028972705, 12.54673760671600213 ) ) ;
#48936 = CARTESIAN_POINT ( 'NONE',  ( 7.627487525399000212, -55.50221245779999890, -10.35845608624000036 ) ) ;
#48937 = CARTESIAN_POINT ( 'NONE',  ( 9.086237931134723667, -78.83508176315426397, -1.732778305792737283 ) ) ;
#48938 = LINE ( 'NONE', #26199, #54632 ) ;
#48939 = CARTESIAN_POINT ( 'NONE',  ( -4.168307155918999918, -80.20180496681199145, 0.1878237294363000187 ) ) ;
#48940 = CARTESIAN_POINT ( 'NONE',  ( 8.241485672608000357, -77.61706001420199641, 5.435909736561999495 ) ) ;
#48941 = CARTESIAN_POINT ( 'NONE',  ( -1.416666666666666519, -83.39999999999999147, 0.000000000000000000 ) ) ;
#48942 = CARTESIAN_POINT ( 'NONE',  ( -2.879226727952121756, -77.99583333333333712, 10.71369944335146407 ) ) ;
#48943 = CARTESIAN_POINT ( 'NONE',  ( -1.295048492660999973, -24.52893519126000044, 12.54716442236999896 ) ) ;
#48944 = CARTESIAN_POINT ( 'NONE',  ( 0.8762648495846868668, -81.43265505382323965, -0.9941098996437038871 ) ) ;
#48945 = EDGE_CURVE ( 'NONE', #15410, #56481, #16272, .T. ) ;
#48946 = CARTESIAN_POINT ( 'NONE',  ( -3.630949683904999947, -76.04999999999999716, 11.17491406647000041 ) ) ;
#48947 = CARTESIAN_POINT ( 'NONE',  ( 0.1636246173744642929, -80.86458333333331439, 1.250000000000000888 ) ) ;
#48948 = AXIS2_PLACEMENT_3D ( 'NONE', #37304, #56202, #55913 ) ;
#48949 = CARTESIAN_POINT ( 'NONE',  ( 1.466761443839349921, -80.08005631220875387, -0.3644506899237003328 ) ) ;
#48950 = CARTESIAN_POINT ( 'NONE',  ( -1.193943581762582529, -78.57580789766646490, 0.3796058497236899920 ) ) ;
#48951 = CARTESIAN_POINT ( 'NONE',  ( 1.412851607863000014, -79.11784227096099187, -0.7817060856327000540 ) ) ;
#48952 = CARTESIAN_POINT ( 'NONE',  ( -13.13047446164998711, -19.21421830981000767, 0.8260994316375004365 ) ) ;
#48953 = CARTESIAN_POINT ( 'NONE',  ( -7.506332976489000330, -77.59125689393900416, -7.926558599818001483 ) ) ;
#48954 = CARTESIAN_POINT ( 'NONE',  ( -6.947761447124999989, -77.95055284899699188, -10.12543283296999874 ) ) ;
#48955 = DIRECTION ( 'NONE',  ( -8.659560562353647261E-17, 0.7071067811866525998, 0.7071067811864425456 ) ) ;
#48956 = CONICAL_SURFACE ( 'NONE', #23506, 11.09999999881999955, 0.7853981633972997312 ) ;
#48957 = EDGE_CURVE ( 'NONE', #17800, #32925, #41688, .T. ) ;
#48959 = CARTESIAN_POINT ( 'NONE',  ( -1.146672249030999957, -77.71141162325049834, 0.4628715253012000153 ) ) ;
#48958 = DIRECTION ( 'NONE',  ( 0.000000000000000000, -0.7071067811864425456, -0.7071067811866525998 ) ) ;
#48960 = CARTESIAN_POINT ( 'NONE',  ( -1.586699731716999962, -82.74040930645999481, 0.6182239771991999699 ) ) ;
#48961 = ORIENTED_EDGE ( 'NONE', *, *, #21888, .T. ) ;
#48962 = CARTESIAN_POINT ( 'NONE',  ( -10.01234990228999955, -18.70150862776000267, -7.653559502277999194 ) ) ;
#48963 = CARTESIAN_POINT ( 'NONE',  ( 4.180271402314000184, -79.53792282429900240, 11.29236839158000016 ) ) ;
#48964 = ADVANCED_FACE ( 'NONE', ( #30401 ), #29529, .T. ) ;
#48965 = DIRECTION ( 'NONE',  ( 0.000000000000000000, 0.7071067811866525998, -0.7071067811864425456 ) ) ;
#48966 = LINE ( 'NONE', #8508, #25659 ) ;
#48967 = CARTESIAN_POINT ( 'NONE',  ( -11.12496554189999998, -77.34408788795398948, -1.432917402686000097 ) ) ;
#48968 = CARTESIAN_POINT ( 'NONE',  ( -9.641208724103000449, -61.23394297667999808, 7.943747389727000119 ) ) ;
#48969 = AXIS2_PLACEMENT_3D ( 'NONE', #48610, #47475, #25290 ) ;
#48970 = CARTESIAN_POINT ( 'NONE',  ( 2.730509227798000094, -0.9404343447128000744, 2.498711234688000271 ) ) ;
#48971 = CARTESIAN_POINT ( 'NONE',  ( -6.912870113367000080, -79.64440148735099001, 6.919194171953000350 ) ) ;
#48972 = CARTESIAN_POINT ( 'NONE',  ( 12.49830695668999958, -23.20970582274999927, -1.666977511086999986 ) ) ;
#48973 = DIRECTION ( 'NONE',  ( -1.000000000000000000, 0.000000000000000000, 0.000000000000000000 ) ) ;
#48974 = ORIENTED_EDGE ( 'NONE', *, *, #25374, .T. ) ;
#48975 = CARTESIAN_POINT ( 'NONE',  ( 0.000000000000000000, -79.99999999999998579, 0.000000000000000000 ) ) ;
#48976 = FACE_OUTER_BOUND ( 'NONE', #19962, .T. ) ;
#48977 = CARTESIAN_POINT ( 'NONE',  ( -12.50409217856559962, -17.47871355536218729, 1.233808107092820183 ) ) ;
#48978 = CARTESIAN_POINT ( 'NONE',  ( 3.399999999999999911, -78.69999999999998863, 0.000000000000000000 ) ) ;
#48979 = CARTESIAN_POINT ( 'NONE',  ( 1.078548557676999975, -83.62992953870899271, -3.379539263167000041 ) ) ;
#48980 = ORIENTED_EDGE ( 'NONE', *, *, #21040, .F. ) ;
#48981 = LINE ( 'NONE', #25661, #28495 ) ;
#48982 = CARTESIAN_POINT ( 'NONE',  ( 0.000000000000000000, -87.29999999999999716, -9.599999999999999645 ) ) ;
#48983 = DIRECTION ( 'NONE',  ( 1.000000000000000000, 0.000000000000000000, 0.000000000000000000 ) ) ;
#48984 = ADVANCED_FACE ( 'NONE', ( #34540 ), #43422, .F. ) ;
#48985 = EDGE_LOOP ( 'NONE', ( #37432, #23760, #21112, #52641, #6302, #17786 ) ) ;
#48986 = ORIENTED_EDGE ( 'NONE', *, *, #53195, .F. ) ;
#48987 = CARTESIAN_POINT ( 'NONE',  ( -8.194873807802000698, -54.08956116737999764, -9.389185139509999445 ) ) ;
#48988 = CARTESIAN_POINT ( 'NONE',  ( 8.249323304235000265, -80.03518932063198577, -5.229696851825000437 ) ) ;
#48989 = ORIENTED_EDGE ( 'NONE', *, *, #13188, .F. ) ;
#48990 = ORIENTED_EDGE ( 'NONE', *, *, #50786, .T. ) ;
#48991 = CARTESIAN_POINT ( 'NONE',  ( 8.143754814233000516, -77.30963688248900212, -8.408463387949000278 ) ) ;
#48992 = CARTESIAN_POINT ( 'NONE',  ( -10.45280047210375862, -78.61879557912125449, -2.510124479038314149 ) ) ;
#48993 = CARTESIAN_POINT ( 'NONE',  ( -1.140637725705999861, -79.20579340557999615, 1.189889555309999958 ) ) ;
#48994 = VERTEX_POINT ( 'NONE', #52004 ) ;
#48995 = CARTESIAN_POINT ( 'NONE',  ( 8.503129636637000388, -77.90345584965399439, -4.225430575863000193 ) ) ;
#48996 = CARTESIAN_POINT ( 'NONE',  ( -1.262801891034090351, -79.29605910888498954, -0.8245544024085487145 ) ) ;
#48997 = CARTESIAN_POINT ( 'NONE',  ( 0.4103876590417050441, -80.25167417027007843, -1.183805647784901494 ) ) ;
#48998 = CARTESIAN_POINT ( 'NONE',  ( 12.62753648294000008, -77.72264530807001393, -3.537092078510000182 ) ) ;
#48999 = CARTESIAN_POINT ( 'NONE',  ( -3.513443458491999571, -78.34964771555745244, -10.65240647004999808 ) ) ;
#49000 = CARTESIAN_POINT ( 'NONE',  ( -13.63885489310999510, -22.78578169018999944, 7.254376133916000668 ) ) ;
#49001 = CARTESIAN_POINT ( 'NONE',  ( 3.518657424384828758, -86.36264283715698298, -1.566607219110386140 ) ) ;
#49002 = CARTESIAN_POINT ( 'NONE',  ( 4.653115705712000505, -79.06072274449400084, -10.20620521156999949 ) ) ;
#49003 = DIRECTION ( 'NONE',  ( 0.000000000000000000, 0.000000000000000000, -1.000000000000000000 ) ) ;
#49004 = CARTESIAN_POINT ( 'NONE',  ( -8.128721809369904960, -80.39067905721536533, 7.570748975258281277 ) ) ;
#49005 = EDGE_LOOP ( 'NONE', ( #13240, #16038, #25544, #50356, #28371, #51525, #17926 ) ) ;
#49006 = CARTESIAN_POINT ( 'NONE',  ( 6.895942029498000281, -79.29823107411199601, -8.909260232556000858 ) ) ;
#49007 = CARTESIAN_POINT ( 'NONE',  ( 2.096143898794329274, -77.24324615902062874, -9.044846050601076826 ) ) ;
#49008 = CARTESIAN_POINT ( 'NONE',  ( 1.330388504836999886, -80.14249923068300063, 0.7273297589862000034 ) ) ;
#49009 = AXIS2_PLACEMENT_3D ( 'NONE', #56758, #2740, #52332 ) ;
#49010 = CARTESIAN_POINT ( 'NONE',  ( 0.2064441143900000164, -78.52055390729400131, 1.303052737963999785 ) ) ;
#49011 = CARTESIAN_POINT ( 'NONE',  ( -1.484444257814014012, -3.439588485883066316, -3.191343661318504665 ) ) ;
#49012 = AXIS2_PLACEMENT_3D ( 'NONE', #44776, #41217, #22630 ) ;
#49013 = CARTESIAN_POINT ( 'NONE',  ( -9.689263856525805352, -17.02111184948868328, 8.274777959192654464 ) ) ;
#49014 = CARTESIAN_POINT ( 'NONE',  ( 10.14999999999999858, -86.39999999999999147, 0.000000000000000000 ) ) ;
#49015 = DIRECTION ( 'NONE',  ( -1.000000000000000000, -3.446666965303000135E-11, 0.000000000000000000 ) ) ;
#49016 = CARTESIAN_POINT ( 'NONE',  ( 11.15746894976000014, -78.30730764035098446, 0.05185606496389000286 ) ) ;
#49017 = EDGE_CURVE ( 'NONE', #21891, #56481, #52573, .T. ) ;
#49018 = CARTESIAN_POINT ( 'NONE',  ( 8.914106061823998672, -77.72396332859899815, 3.639947156824000274 ) ) ;
#49019 = CARTESIAN_POINT ( 'NONE',  ( 10.01332844637000008, -23.28056692670000061, -7.654537085030000299 ) ) ;
#49020 = CARTESIAN_POINT ( 'NONE',  ( 3.949587968339014044, -78.99812697311170950, 11.21690579045210967 ) ) ;
#49021 = CARTESIAN_POINT ( 'NONE',  ( 10.35453599130000057, -76.65783510652001098, -6.064947188958000446 ) ) ;
#49022 = B_SPLINE_CURVE_WITH_KNOTS ( 'NONE', 3,
 ( #6038, #51516, #42361, #46807, #19923, #6916, #11075, #10779, #34051, #42648, #50933, #11648, #20216, #28465, #38205, #47679, #28757, #42941 ),
 .UNSPECIFIED., .F., .F.,
 ( 4, 2, 2, 2, 2, 2, 2, 2, 4 ),
 ( 0.000000000000000000, 0.1249999999999999722, 0.2499999999999999445, 0.3749999999999998890, 0.4999999999999998890, 0.6249999999999998890, 0.7499999999999997780, 0.8749999999999998890, 1.000000000000000000 ),
 .UNSPECIFIED. ) ;
#49023 = DIRECTION ( 'NONE',  ( 0.000000000000000000, -1.000000000000000000, 0.000000000000000000 ) ) ;
#49024 = ORIENTED_EDGE ( 'NONE', *, *, #40709, .T. ) ;
#49025 = CARTESIAN_POINT ( 'NONE',  ( -0.5793938177159999592, -82.86393340258099727, 1.349352049262000142 ) ) ;
#49026 = CARTESIAN_POINT ( 'NONE',  ( 1.288070761429999989, -80.79441198108999345, 0.4084665662698999666 ) ) ;
#49027 = CARTESIAN_POINT ( 'NONE',  ( 7.710095619848000403, -57.04935285743999884, -10.18496935399999970 ) ) ;
#49028 = DIRECTION ( 'NONE',  ( -1.000000000000000000, 0.000000000000000000, 0.000000000000000000 ) ) ;
#49029 = CARTESIAN_POINT ( 'NONE',  ( 1.750000000000000000, -77.50000000000000000, 0.000000000000000000 ) ) ;
#49030 = CARTESIAN_POINT ( 'NONE',  ( -1.181111693982000110, -79.27654225787900089, -0.4092372983238000139 ) ) ;
#49031 = CARTESIAN_POINT ( 'NONE',  ( -8.852102014390000662, -78.01808746511700576, 8.004735621704000437 ) ) ;
#49032 = CARTESIAN_POINT ( 'NONE',  ( -7.530775182571000315, -78.06434415034598828, -6.150709233331999037 ) ) ;
#49033 = CARTESIAN_POINT ( 'NONE',  ( 9.521438313890000060, -77.39399981532699258, 0.1121992162086000028 ) ) ;
#49034 = CARTESIAN_POINT ( 'NONE',  ( -1.801614160562000189, -55.41347738061999451, -12.59687422885999908 ) ) ;
#49035 = CARTESIAN_POINT ( 'NONE',  ( -9.722718241315000398, -60.04999999966999980, 7.954951288349001004 ) ) ;
#49036 = CARTESIAN_POINT ( 'NONE',  ( 1.592434616855321838, -86.07389998728979208, 3.669353075276816423 ) ) ;
#49037 = ORIENTED_EDGE ( 'NONE', *, *, #52839, .T. ) ;
#49038 = CARTESIAN_POINT ( 'NONE',  ( -5.610847844242281113, -78.22500000000000853, 7.718163323371710405 ) ) ;
#49039 = CARTESIAN_POINT ( 'NONE',  ( -0.7554284705563540925, -79.31666666666669130, 1.310679582531384391 ) ) ;
#49040 = CARTESIAN_POINT ( 'NONE',  ( 6.998236738571699256, -78.87457940415021085, -9.608823350299664057 ) ) ;
#49041 = EDGE_CURVE ( 'NONE', #51923, #25833, #35110, .T. ) ;
#49042 = CARTESIAN_POINT ( 'NONE',  ( -2.089807409446279074, -78.48547957940618858, -3.465957297018673611 ) ) ;
#49043 = AXIS2_PLACEMENT_3D ( 'NONE', #7911, #43649, #3208 ) ;
#49044 = CARTESIAN_POINT ( 'NONE',  ( -8.058638732054999920, -78.48953713045399638, -7.451332657186999775 ) ) ;
#49045 = CARTESIAN_POINT ( 'NONE',  ( 1.722320550008820339, -17.76336311177879779, 12.71171904436578615 ) ) ;
#49046 = CARTESIAN_POINT ( 'NONE',  ( 4.569396385344999700, -76.85349636657100802, 11.38719340697999982 ) ) ;
#49047 = CARTESIAN_POINT ( 'NONE',  ( 3.536460498928797769, -78.54893592801708735, 11.20448496730672794 ) ) ;
#49048 = CARTESIAN_POINT ( 'NONE',  ( 10.53559655343999957, -18.79430958026000198, -7.620036381602000475 ) ) ;
#49049 = ORIENTED_EDGE ( 'NONE', *, *, #31173, .T. ) ;
#49050 = CARTESIAN_POINT ( 'NONE',  ( 10.41480047653000085, -78.36439489434398808, -3.637813056042999982 ) ) ;
#49051 = CARTESIAN_POINT ( 'NONE',  ( 0.6919073629492709099, -79.92850570978326630, 1.042099490686354990 ) ) ;
#49052 = DIRECTION ( 'NONE',  ( -1.000000000000000000, 0.000000000000000000, 0.000000000000000000 ) ) ;
#49053 = CARTESIAN_POINT ( 'NONE',  ( -2.394032993764998452, -78.62148118236264338, 3.970517833774876326 ) ) ;
#49054 = CARTESIAN_POINT ( 'NONE',  ( 6.829411927397999627, -78.92047959254598766, -8.823306204757001225 ) ) ;
#49055 = CARTESIAN_POINT ( 'NONE',  ( 12.50240681836000078, -61.48234730679999416, -1.005418944265000114 ) ) ;
#49056 = DIRECTION ( 'NONE',  ( -1.000000000000000000, 0.000000000000000000, 0.000000000000000000 ) ) ;
#49057 = EDGE_CURVE ( 'NONE', #45906, #26455, #55819, .T. ) ;
#49058 = CARTESIAN_POINT ( 'NONE',  ( -9.108185712014998714, -78.26808746511700576, 8.236305738405000909 ) ) ;
#49059 = ORIENTED_EDGE ( 'NONE', *, *, #25817, .T. ) ;
#49060 = CIRCLE ( 'NONE', #51901, 13.86363636363999952 ) ;
#49061 = CARTESIAN_POINT ( 'NONE',  ( 8.130813118010999929, -17.31476110167000115, -9.546856411651999608 ) ) ;
#49062 = CARTESIAN_POINT ( 'NONE',  ( -12.70610460586324386, -61.25512899760538232, -1.580683094070863604 ) ) ;
#49063 = DIRECTION ( 'NONE',  ( 0.000000000000000000, -1.000000000000000000, 0.000000000000000000 ) ) ;
#49064 = EDGE_LOOP ( 'NONE', ( #23646, #21622, #13763, #3799 ) ) ;
#49065 = ORIENTED_EDGE ( 'NONE', *, *, #7631, .F. ) ;
#49066 = CARTESIAN_POINT ( 'NONE',  ( 5.838193839761703252, -78.57708333333333428, -7.596835002782702517 ) ) ;
#49067 = CARTESIAN_POINT ( 'NONE',  ( 9.254623623301998947, -77.89893998579799472, 2.326634063882999648 ) ) ;
#49068 = VERTEX_POINT ( 'NONE', #2409 ) ;
#49069 = CARTESIAN_POINT ( 'NONE',  ( -10.39285214024000048, -78.50746505344999093, 6.510605926401999533 ) ) ;
#49070 = VERTEX_POINT ( 'NONE', #22354 ) ;
#49071 = CARTESIAN_POINT ( 'NONE',  ( 9.929702205000999982, -24.63097880280000140, 7.973987073284000360 ) ) ;
#49072 = CARTESIAN_POINT ( 'NONE',  ( -10.42531125068999920, -23.26485145404000221, 7.624341767093000044 ) ) ;
#49073 = CARTESIAN_POINT ( 'NONE',  ( -12.50728321917715391, -24.99975184166999753, -0.1774118160393889920 ) ) ;
#49074 = CARTESIAN_POINT ( 'NONE',  ( 5.745747329289000227, -78.53052096864399800, 9.633509135241000720 ) ) ;
#49075 = CARTESIAN_POINT ( 'NONE',  ( -0.9956369009631184097, -79.54819107059427097, 0.7605103355424140954 ) ) ;
#49076 = ORIENTED_EDGE ( 'NONE', *, *, #2042, .F. ) ;
#49077 = CIRCLE ( 'NONE', #22700, 10.74999999999999467 ) ;
#49078 = EDGE_LOOP ( 'NONE', ( #21180, #25949, #25304, #43140 ) ) ;
#49079 = CARTESIAN_POINT ( 'NONE',  ( 2.855190675867043115, -77.45020626835986377, 8.798204014871961576 ) ) ;
#49080 = CARTESIAN_POINT ( 'NONE',  ( -10.84202097104999929, -77.29444807548399865, 2.082001701158999740 ) ) ;
#49081 = CARTESIAN_POINT ( 'NONE',  ( -9.702231720816998362, -78.89204055589898701, -0.1934140619087000024 ) ) ;
#49082 = CARTESIAN_POINT ( 'NONE',  ( 6.758991595627000137, -76.50069210185999680, -10.87838826503999989 ) ) ;
#49083 = CARTESIAN_POINT ( 'NONE',  ( -6.047833114999293436, -79.47011274197635089, -7.345927578306194583 ) ) ;
#49084 = CARTESIAN_POINT ( 'NONE',  ( 1.619712389308999967, -78.96894917727999541, 0.1587296492880999887 ) ) ;
#49085 = CARTESIAN_POINT ( 'NONE',  ( 0.9993909113990739890, -79.43417149341397021, -9.481187304795884785 ) ) ;
#49086 = CARTESIAN_POINT ( 'NONE',  ( 0.000000000000000000, -81.79999999999998295, 0.000000000000000000 ) ) ;
#49087 = EDGE_CURVE ( 'NONE', #10981, #19814, #27635, .T. ) ;
#49088 = CARTESIAN_POINT ( 'NONE',  ( 0.000000000000000000, -15.06282895647999887, 0.000000000000000000 ) ) ;
#49089 = DIRECTION ( 'NONE',  ( 0.000000000000000000, 1.000000000000000000, 0.000000000000000000 ) ) ;
#49090 = ORIENTED_EDGE ( 'NONE', *, *, #25505, .F. ) ;
#49091 = EDGE_CURVE ( 'NONE', #41589, #48697, #33290, .T. ) ;
#49092 = CARTESIAN_POINT ( 'NONE',  ( -11.42485267055999998, -79.41066419345099803, 4.602037622659000071 ) ) ;
#49093 = CIRCLE ( 'NONE', #53818, 11.65000000000000036 ) ;
#49094 = CARTESIAN_POINT ( 'NONE',  ( -7.758650587924000419, -54.64922688096000059, 9.996717134826001327 ) ) ;
#49095 = CARTESIAN_POINT ( 'NONE',  ( -2.114515350056125342, -77.99088766215147928, 10.53989743401121970 ) ) ;
#49096 = CARTESIAN_POINT ( 'NONE',  ( -9.690626710582000314, -78.18390840682999965, -7.043281791253000357 ) ) ;
#49097 = CARTESIAN_POINT ( 'NONE',  ( -12.70255466322978144, -61.54616562041045569, 1.306323829516669255 ) ) ;
#49098 = VECTOR ( 'NONE', #49820, 1000.000000000000114 ) ;
#49100 = CARTESIAN_POINT ( 'NONE',  ( -1.667269374596999976, -18.79060116514999734, -12.49858097730999873 ) ) ;
#49099 = CARTESIAN_POINT ( 'NONE',  ( 7.655555357438999842, -56.02204592290999585, 10.38646360829000059 ) ) ;
#49101 = DIRECTION ( 'NONE',  ( -1.000000000000000000, 0.000000000000000000, 0.000000000000000000 ) ) ;
#49102 = CARTESIAN_POINT ( 'NONE',  ( 10.53101990622000095, -60.10639784916000394, -7.613962745625999062 ) ) ;
#49103 = CARTESIAN_POINT ( 'NONE',  ( -0.3713770062794000126, -82.26979749068699732, -1.193557338046999927 ) ) ;
#49104 = CARTESIAN_POINT ( 'NONE',  ( 5.172078487859000262, -77.66043913071798954, 10.00417756108999967 ) ) ;
#49105 = CARTESIAN_POINT ( 'NONE',  ( 3.140974612311327796, -78.15416666666665435, 11.68767212001979594 ) ) ;
#49106 = CARTESIAN_POINT ( 'NONE',  ( -2.507084801459968038, -0.8133145018255537595, -2.558030464532227821 ) ) ;
#49107 = ORIENTED_EDGE ( 'NONE', *, *, #22266, .T. ) ;
#49108 = DIRECTION ( 'NONE',  ( 0.009503199022040095811, 0.000000000000000000, -0.9999548435846228323 ) ) ;
#49109 = CARTESIAN_POINT ( 'NONE',  ( -1.807051837523000026, -54.49921584723999501, 12.77977401831000037 ) ) ;
#49110 = DIRECTION ( 'NONE',  ( 0.9999999930530776293, 0.000000000000000000, 0.0001178721535674748841 ) ) ;
#49111 = ADVANCED_FACE ( 'NONE', ( #9665 ), #39896, .F. ) ;
#49112 = CARTESIAN_POINT ( 'NONE',  ( -3.266298089353000034, -1.668078706142999801, -1.618310284079999883 ) ) ;
#49113 = CARTESIAN_POINT ( 'NONE',  ( -8.960380918909999437, -79.54589830381199533, -2.921951021776999724 ) ) ;
#49114 = PLANE ( 'NONE',  #39437 ) ;
#49115 = CARTESIAN_POINT ( 'NONE',  ( -0.9887300587116000239, -61.73410057736000311, 12.65963207093999898 ) ) ;
#49116 = DIRECTION ( 'NONE',  ( 1.000000000000000000, 0.000000000000000000, 0.000000000000000000 ) ) ;
#49117 = CARTESIAN_POINT ( 'NONE',  ( 3.807751541924000005, -82.42258068398498949, -1.403160745109000018 ) ) ;
#49118 = CARTESIAN_POINT ( 'NONE',  ( 9.722718241315000398, -23.44678171330999916, -7.954951288349001004 ) ) ;
#49119 = CARTESIAN_POINT ( 'NONE',  ( 12.07139231284771164, -77.20343651399288376, 0.05712616762542849919 ) ) ;
#49120 = CARTESIAN_POINT ( 'NONE',  ( -6.190658199239000403, -78.41135615475999998, 10.70411142322000053 ) ) ;
#49121 = CIRCLE ( 'NONE', #39670, 1.749999999999999556 ) ;
#49122 = CARTESIAN_POINT ( 'NONE',  ( 1.639991984446999895, -77.91322009697699968, -11.14201017990999887 ) ) ;
#49123 = CARTESIAN_POINT ( 'NONE',  ( 0.7831030525921437446, -81.92154750067230395, 0.9747994925984700965 ) ) ;
#49124 = CARTESIAN_POINT ( 'NONE',  ( -1.601737029647000154, -78.30825665301999550, 0.4494192519392999907 ) ) ;
#49125 = CARTESIAN_POINT ( 'NONE',  ( -9.555818165766000405, -77.39146748629899264, -0.1257991660602000017 ) ) ;
#49126 = CARTESIAN_POINT ( 'NONE',  ( -1.505894968352336827, -82.74391654559087783, 0.1164684639126788851 ) ) ;
#49127 = DIRECTION ( 'NONE',  ( 1.000000000000000000, 0.000000000000000000, 0.000000000000000000 ) ) ;
#49128 = CARTESIAN_POINT ( 'NONE',  ( 4.127591228001228352, -80.25644506522834831, -9.925940447433527325 ) ) ;
#49129 = DIRECTION ( 'NONE',  ( 0.000000000000000000, -1.000000000000000000, 0.000000000000000000 ) ) ;
#49130 = CARTESIAN_POINT ( 'NONE',  ( 2.179326186851605396, -78.70934838570477154, 11.00327889010784332 ) ) ;
#49131 = DIRECTION ( 'NONE',  ( 0.000000000000000000, 1.000000000000000000, 7.697546304067999821E-14 ) ) ;
#49132 = CARTESIAN_POINT ( 'NONE',  ( 11.00000000000000000, -79.34999999999999432, -1.064824513673000067E-14 ) ) ;
#49133 = CARTESIAN_POINT ( 'NONE',  ( -0.2704138798119000153, -79.26806712638799013, 11.14367429999999892 ) ) ;
#49134 = CARTESIAN_POINT ( 'NONE',  ( 8.190836719257328369, -55.61035107871643390, 7.342356150419330874 ) ) ;
#49135 = ORIENTED_EDGE ( 'NONE', *, *, #35821, .T. ) ;
#49136 = ORIENTED_EDGE ( 'NONE', *, *, #50580, .T. ) ;
#49137 = CARTESIAN_POINT ( 'NONE',  ( 1.508679547070999938, -80.71294663253300428, -0.5754170318403001305 ) ) ;
#49138 = VECTOR ( 'NONE', #18371, 1000.000000000000000 ) ;
#49139 = ORIENTED_EDGE ( 'NONE', *, *, #47082, .F. ) ;
#49140 = CARTESIAN_POINT ( 'NONE',  ( -11.75000000000000000, -78.79999999999999716, 1.318041981624000073E-14 ) ) ;
#49142 = ADVANCED_FACE ( 'NONE', ( #9961 ), #25750, .T. ) ;
#49141 = ORIENTED_EDGE ( 'NONE', *, *, #27294, .T. ) ;
#49143 = CIRCLE ( 'NONE', #8597, 11.59999999999999964 ) ;
#49144 = CARTESIAN_POINT ( 'NONE',  ( 0.000000000000000000, -46.09579702914000165, 0.000000000000000000 ) ) ;
#49145 = CARTESIAN_POINT ( 'NONE',  ( 2.193927587745784891, -79.23958332842951791, -2.654379237460795071 ) ) ;
#49146 = CARTESIAN_POINT ( 'NONE',  ( 2.005614507304999794, -79.78068473043899189, -10.84800649278999884 ) ) ;
#49147 = CARTESIAN_POINT ( 'NONE',  ( 1.570796326794909881, -76.43541666664329171, -11.99999999999999822 ) ) ;
#49148 = CARTESIAN_POINT ( 'NONE',  ( 3.319279290813000216, -79.89270551910098561, 2.165265596042999618 ) ) ;
#49149 = CARTESIAN_POINT ( 'NONE',  ( -0.1688430469021683922, -79.27612716086017031, 9.502712028091975682 ) ) ;
#49150 = EDGE_LOOP ( 'NONE', ( #37443, #16474, #23507, #9644, #33804, #35314 ) ) ;
#49151 = CARTESIAN_POINT ( 'NONE',  ( 9.298505144763540287, -78.30746914334582698, -5.515131374144830012 ) ) ;
#49152 = CARTESIAN_POINT ( 'NONE',  ( -9.315216588649001039, -78.86259768561001238, 7.893946640039000151 ) ) ;
#49153 = ORIENTED_EDGE ( 'NONE', *, *, #42765, .T. ) ;
#49154 = EDGE_LOOP ( 'NONE', ( #40589, #21790, #3193, #30874, #40790, #10160 ) ) ;
#49155 = FACE_OUTER_BOUND ( 'NONE', #8461, .T. ) ;
#49156 = DIRECTION ( 'NONE',  ( -0.9999463328794432337, 0.000000000000000000, 0.01036008498777044214 ) ) ;
#49157 = CARTESIAN_POINT ( 'NONE',  ( -1.213636094208999872, -80.79966376390299843, -0.5527192377158001158 ) ) ;
#49158 = CARTESIAN_POINT ( 'NONE',  ( 8.240135455977000589, -77.91526456327599703, -5.125512367919999868 ) ) ;
#49159 = CARTESIAN_POINT ( 'NONE',  ( 3.576074390005934855, -86.31452044229999387, -1.592170899228145586 ) ) ;
#49160 = DIRECTION ( 'NONE',  ( -2.622163234167000180E-09, -1.000000000000000000, -6.038615341233999930E-09 ) ) ;
#49161 = CARTESIAN_POINT ( 'NONE',  ( -10.33814977949000102, -76.69558033460998558, 7.275158806450000348 ) ) ;
#49162 = CARTESIAN_POINT ( 'NONE',  ( 8.745915541949560890, -77.83069693750340434, 3.571268974134527152 ) ) ;
#49163 = CARTESIAN_POINT ( 'NONE',  ( -10.18499221077999906, -20.25022860214999909, 7.710118476625000383 ) ) ;
#49164 = EDGE_CURVE ( 'NONE', #14569, #52925, #48393, .T. ) ;
#49165 = CARTESIAN_POINT ( 'NONE',  ( -3.381175124639000273, -80.37370721702599496, 2.067279602469000110 ) ) ;
#49166 = B_SPLINE_CURVE_WITH_KNOTS ( 'NONE', 3,
 ( #23022, #10039, #33029, #45476 ),
 .UNSPECIFIED., .F., .F.,
 ( 4, 4 ),
 ( 0.000000000000000000, 1.000000000000000000 ),
 .UNSPECIFIED. ) ;
#49167 = CARTESIAN_POINT ( 'NONE',  ( 12.65372179303999900, -21.75064713777999970, 1.750000000000000000 ) ) ;
#49168 = DIRECTION ( 'NONE',  ( 0.000000000000000000, -1.000000000000000000, 0.000000000000000000 ) ) ;
#49169 = CARTESIAN_POINT ( 'NONE',  ( -2.656469456053000222, -81.81625264934800157, -2.346940931520999918 ) ) ;
#49170 = CARTESIAN_POINT ( 'NONE',  ( 0.7999999999999001243, -18.84999999997999964, 12.00000000000000000 ) ) ;
#49171 = CARTESIAN_POINT ( 'NONE',  ( 3.228614917279000185, -81.04981373882509388, -10.79283437469000084 ) ) ;
#49172 = CARTESIAN_POINT ( 'NONE',  ( -2.809159726167000048, -3.341600190120999958, -2.568020482856000264 ) ) ;
#49173 = CARTESIAN_POINT ( 'NONE',  ( 1.219634552038143083, -79.97640533137604280, -0.3722560451975370222 ) ) ;
#49174 = VERTEX_POINT ( 'NONE', #28232 ) ;
#49175 = CARTESIAN_POINT ( 'NONE',  ( 0.5999381870725726262, -23.23019609313229239, 10.98362755083784847 ) ) ;
#49176 = LINE ( 'NONE', #17891, #13810 ) ;
#49177 = ADVANCED_FACE ( 'NONE', ( #41538 ), #22950, .F. ) ;
#49178 = CARTESIAN_POINT ( 'NONE',  ( 0.08638142328466999476, -81.04795502547899844, 1.330832257483999914 ) ) ;
#49179 = VECTOR ( 'NONE', #17876, 1000.000000000000000 ) ;
#49181 = EDGE_CURVE ( 'NONE', #10450, #22499, #42753, .T. ) ;
#49180 = CARTESIAN_POINT ( 'NONE',  ( -12.77568125278999922, -16.73490786122999907, -0.5296379231476000538 ) ) ;
#49182 = CARTESIAN_POINT ( 'NONE',  ( 12.53073434187000146, -77.71093324932999735, -3.509976885708000260 ) ) ;
#49183 = CIRCLE ( 'NONE', #9619, 4.100000000000000533 ) ;
#49184 = CARTESIAN_POINT ( 'NONE',  ( -6.137787596906999710, -79.43688667140099824, 7.419310695580000115 ) ) ;
#49185 = CARTESIAN_POINT ( 'NONE',  ( 12.83044027761000017, -18.69360215052999763, -2.062670899361999766 ) ) ;
#49186 = ORIENTED_EDGE ( 'NONE', *, *, #18704, .F. ) ;
#49187 = DIRECTION ( 'NONE',  ( 1.000000000000000000, 0.000000000000000000, 0.000000000000000000 ) ) ;
#49188 = DIRECTION ( 'NONE',  ( 0.000000000000000000, 1.000000000000000000, 0.000000000000000000 ) ) ;
#49189 = CARTESIAN_POINT ( 'NONE',  ( -1.242342038214000022, -82.25520586034700443, -0.2121855787343999988 ) ) ;
#49190 = CARTESIAN_POINT ( 'NONE',  ( -1.799490225533999732, -19.22847221992000044, -12.64500484465999897 ) ) ;
#49191 = CARTESIAN_POINT ( 'NONE',  ( -8.968424590936999508, -77.43311187452998468, 2.773906523901999766 ) ) ;
#49193 = CARTESIAN_POINT ( 'NONE',  ( 2.627446458840999810, -1.600918092571000040, 3.037392460054000320 ) ) ;
#49192 = CARTESIAN_POINT ( 'NONE',  ( 3.614576214518000263, -82.06136777077499289, -1.331977498170999974 ) ) ;
#49194 = CARTESIAN_POINT ( 'NONE',  ( -0.3271848554491046945, -82.39583333333330017, 1.217465845835393301 ) ) ;
#49195 = CARTESIAN_POINT ( 'NONE',  ( -0.8999941789210000875, -80.66976366365300066, -1.015940422307999969 ) ) ;
#49196 = ORIENTED_EDGE ( 'NONE', *, *, #50332, .F. ) ;
#49197 = CARTESIAN_POINT ( 'NONE',  ( -4.804849618107155607, -77.18816215842083750, -9.616802285769223246 ) ) ;
#49198 = CARTESIAN_POINT ( 'NONE',  ( -3.251154051729839178, -1.100857096137070279, 2.995606203745920413E-05 ) ) ;
#49199 = ADVANCED_FACE ( 'NONE', ( #50708 ), #1696, .F. ) ;
#49200 = CARTESIAN_POINT ( 'NONE',  ( 1.792077181278651565, -78.94486059145259560, -3.438065020606960065 ) ) ;
#49201 = ORIENTED_EDGE ( 'NONE', *, *, #481, .T. ) ;
#49202 = ORIENTED_EDGE ( 'NONE', *, *, #10820, .F. ) ;
#49203 = CARTESIAN_POINT ( 'NONE',  ( -10.66249531825000041, -79.86290934975998823, 1.062579819291000094 ) ) ;
#49204 = CARTESIAN_POINT ( 'NONE',  ( 0.000000000000000000, -76.75499999999999545, 0.000000000000000000 ) ) ;
#49205 = CARTESIAN_POINT ( 'NONE',  ( 8.838834764832000701, -23.25000000000000000, -8.838834764832000701 ) ) ;
#49206 = EDGE_LOOP ( 'NONE', ( #22259, #56698, #9132, #57885 ) ) ;
#49207 =( GEOMETRIC_REPRESENTATION_CONTEXT ( 3 ) GLOBAL_UNCERTAINTY_ASSIGNED_CONTEXT ( ( #20127 ) ) GLOBAL_UNIT_ASSIGNED_CONTEXT ( ( #10015, #28284, #14710 ) ) REPRESENTATION_CONTEXT ( 'NONE', 'WORKASPACE' ) );
#49208 = CARTESIAN_POINT ( 'NONE',  ( 8.321246128606000880, -78.37679717510499700, -8.715080868295999039 ) ) ;
#49209 = ORIENTED_EDGE ( 'NONE', *, *, #39447, .T. ) ;
#49210 = B_SPLINE_CURVE_WITH_KNOTS ( 'NONE', 3,
 ( #38718, #25719, #39010, #42584, #57018, #16580, #16299, #20149, #34277, #37850, #29560, #30135, #55870 ),
 .UNSPECIFIED., .F., .F.,
 ( 4, 2, 2, 1, 2, 2, 4 ),
 ( 0.000000000000000000, 0.2499999999999995559, 0.3749999999999995559, 0.4374999999999995004, 0.4687499999999995004, 0.4999999999999994449, 1.000000000000000000 ),
 .UNSPECIFIED. ) ;
#49212 = ADVANCED_FACE ( 'NONE', ( #46284 ), #1009, .F. ) ;
#49211 = EDGE_LOOP ( 'NONE', ( #8957, #46495, #4530, #13566, #970 ) ) ;
#49213 = CARTESIAN_POINT ( 'NONE',  ( 7.364280830343314044, -60.14010097497207141, 8.171144579306906408 ) ) ;
#49214 = EDGE_CURVE ( 'NONE', #41145, #23631, #44495, .T. ) ;
#49215 = CARTESIAN_POINT ( 'NONE',  ( 3.141622339616611193, -76.54521521273609608, -11.68862050864443880 ) ) ;
#49216 = CARTESIAN_POINT ( 'NONE',  ( -1.081559480311999888, -0.7500000000000000000, 3.328697807033000000 ) ) ;
#49217 = ORIENTED_EDGE ( 'NONE', *, *, #37975, .T. ) ;
#49218 = VERTEX_POINT ( 'NONE', #1915 ) ;
#49219 = CARTESIAN_POINT ( 'NONE',  ( -1.260218936850459936, -79.63768523161391499, 0.1932868554924389581 ) ) ;
#49220 = VECTOR ( 'NONE', #8262, 1000.000000000000114 ) ;
#49221 = DIRECTION ( 'NONE',  ( -0.9859154929576978699, -0.1672442547472993701, -2.241743217924995723E-11 ) ) ;
#49222 = CIRCLE ( 'NONE', #18929, 9.199999999999999289 ) ;
#49223 = CARTESIAN_POINT ( 'NONE',  ( 10.53495272788000214, -55.57289072595000334, 7.618387390351999855 ) ) ;
#49224 = CARTESIAN_POINT ( 'NONE',  ( -7.682344222590000271, -19.23537109840999904, -10.04116292118000153 ) ) ;
#49225 = CARTESIAN_POINT ( 'NONE',  ( 2.460597061978947675, -79.59635416666264973, 9.159220229803393565 ) ) ;
#49226 = CARTESIAN_POINT ( 'NONE',  ( -9.396085398178650294, -78.74791666666668277, 7.220923959705211281 ) ) ;
#49227 = CARTESIAN_POINT ( 'NONE',  ( 7.627487606627999739, -60.09778595451999905, -10.35845616728999907 ) ) ;
#49228 = CARTESIAN_POINT ( 'NONE',  ( 8.768124086712999699, -59.94999999969000015, -7.919595949288999570 ) ) ;
#49229 = CARTESIAN_POINT ( 'NONE',  ( -9.778543098479998363, -25.04857981702999936, 8.284584910395000890 ) ) ;
#49230 = CARTESIAN_POINT ( 'NONE',  ( 9.249824806346651940, -77.84496366503705644, -0.6054522768334679172 ) ) ;
#49231 = CARTESIAN_POINT ( 'NONE',  ( 4.047000891220999819, -82.44647163347798369, -0.2667513232904999421 ) ) ;
#49232 = CARTESIAN_POINT ( 'NONE',  ( 0.7109233471628000345, -77.62608667140099783, 9.736770704497999418 ) ) ;
#49233 = AXIS2_PLACEMENT_3D ( 'NONE', #46248, #42094, #46545 ) ;
#49234 = CARTESIAN_POINT ( 'NONE',  ( -12.43645963092999907, -17.08248289540999920, -0.05235777564062000372 ) ) ;
#49235 = CARTESIAN_POINT ( 'NONE',  ( 9.250000000000000000, -79.84999999999999432, 0.000000000000000000 ) ) ;
#49236 = CARTESIAN_POINT ( 'NONE',  ( 1.194090705999000024, -24.44031658902999737, 12.43436538489999954 ) ) ;
#49237 = CARTESIAN_POINT ( 'NONE',  ( -8.090910852015257504, -60.34721902435955343, -7.452378523310254188 ) ) ;
#49238 = CARTESIAN_POINT ( 'NONE',  ( -0.6684780613089000845, -84.38907726527799014, 3.483919782562000300 ) ) ;
#49239 = CARTESIAN_POINT ( 'NONE',  ( 2.702298720593999892, -1.280362276481999961, 2.656632122398999485 ) ) ;
#49240 = CARTESIAN_POINT ( 'NONE',  ( 7.686941364987999847, -57.04527982297999955, 10.48774103564000093 ) ) ;
#49241 = CARTESIAN_POINT ( 'NONE',  ( 0.8080229617562444400, -80.01932486526288812, -1.277038703091432748 ) ) ;
#49242 = CARTESIAN_POINT ( 'NONE',  ( -1.054090230153319485, -78.55495177038956456, 0.6754526289925347760 ) ) ;
#49243 = CARTESIAN_POINT ( 'NONE',  ( 0.8292593438864999111, -78.07597717995859909, -1.385477418387000004 ) ) ;
#49244 = FACE_BOUND ( 'NONE', #11480, .T. ) ;
#49245 = EDGE_CURVE ( 'NONE', #50686, #15223, #36163, .T. ) ;
#49246 = CARTESIAN_POINT ( 'NONE',  ( 8.899710312955001257, -77.72743860894800605, -6.322224476856000308 ) ) ;
#49247 = CARTESIAN_POINT ( 'NONE',  ( 10.03503830778000072, -78.57452710374299443, -7.077696433220999950 ) ) ;
#49248 = CARTESIAN_POINT ( 'NONE',  ( -1.500000000000000000, -81.00000000000000000, 0.000000000000000000 ) ) ;
#49250 = CARTESIAN_POINT ( 'NONE',  ( -1.092853437769999880, -78.91363271308999572, -1.051005954092999906 ) ) ;
#49249 = CARTESIAN_POINT ( 'NONE',  ( 0.000000000000000000, -0.2000000000000000111, 0.000000000000000000 ) ) ;
#49251 = CARTESIAN_POINT ( 'NONE',  ( 1.529418508686999800, -83.05620538201100089, 0.7487957062819000642 ) ) ;
#49252 = ORIENTED_EDGE ( 'NONE', *, *, #12591, .F. ) ;
#49253 = CARTESIAN_POINT ( 'NONE',  ( 1.142103019466000013, -83.95346544543099299, -3.578681710149999695 ) ) ;
#49254 = CARTESIAN_POINT ( 'NONE',  ( 7.165667693159000429, -78.94640101988399294, 9.347813962385000508 ) ) ;
#49255 = CARTESIAN_POINT ( 'NONE',  ( 11.12875569142000032, -80.39817708664989482, 0.9871941560245000025 ) ) ;
#49256 = CARTESIAN_POINT ( 'NONE',  ( 7.919595949288999570, -57.79999999967000690, -8.909545442949999838 ) ) ;
#49257 = CARTESIAN_POINT ( 'NONE',  ( -0.07384301375007251700, -85.83020833989095877, 3.410305331954705643 ) ) ;
#49258 = CARTESIAN_POINT ( 'NONE',  ( -3.633103876188000125, -77.23514251594700397, 10.61219425078000000 ) ) ;
#49259 = DIRECTION ( 'NONE',  ( 1.000000000000000000, 0.000000000000000000, 0.000000000000000000 ) ) ;
#49260 = CARTESIAN_POINT ( 'NONE',  ( -9.737659524074000927, -78.83077255621898871, -0.1941203154314999901 ) ) ;
#49261 = CONICAL_SURFACE ( 'NONE', #31320, 8.899999998586000771, 0.7853981633972997312 ) ;
#49262 = DIRECTION ( 'NONE',  ( 0.000000000000000000, 1.000000000000000000, 0.000000000000000000 ) ) ;
#49263 = DIRECTION ( 'NONE',  ( -0.9999999999999992228, 4.158392525768991814E-08, -7.902844367246985944E-12 ) ) ;
#49264 = CARTESIAN_POINT ( 'NONE',  ( -3.250000000000000000, -3.100000000000000089, 0.000000000000000000 ) ) ;
#49265 = CARTESIAN_POINT ( 'NONE',  ( -1.930989144707000005, -57.04634220890999785, 12.80900240956999880 ) ) ;
#49266 = ORIENTED_EDGE ( 'NONE', *, *, #54501, .F. ) ;
#49267 = FACE_OUTER_BOUND ( 'NONE', #3466, .T. ) ;
#49268 = CARTESIAN_POINT ( 'NONE',  ( 9.505044359491998662, -79.49388667140100040, -1.566734738709000041 ) ) ;
#49269 = EDGE_CURVE ( 'NONE', #45083, #54465, #50334, .T. ) ;
#49270 = B_SPLINE_CURVE_WITH_KNOTS ( 'NONE', 3,
 ( #38094, #37508, #23931, #16247, #24231, #25093 ),
 .UNSPECIFIED., .F., .F.,
 ( 4, 2, 4 ),
 ( 0.000000000000000000, 0.5000000000000000000, 1.000000000000000000 ),
 .UNSPECIFIED. ) ;
#49271 = CARTESIAN_POINT ( 'NONE',  ( -1.249999993052000047, -76.30000000069199473, -0.6999999993075000093 ) ) ;
#49272 = CARTESIAN_POINT ( 'NONE',  ( -10.35845608624000036, -55.50221245779999890, -7.627487525399000212 ) ) ;
#49273 = EDGE_CURVE ( 'NONE', #31098, #31041, #7902, .T. ) ;
#49274 = CARTESIAN_POINT ( 'NONE',  ( 0.3704480504712000521, -80.03166928263999580, -1.624200486671999899 ) ) ;
#49275 = VERTEX_POINT ( 'NONE', #19032 ) ;
#49276 = CARTESIAN_POINT ( 'NONE',  ( -4.598873869541999504, -77.52019710480799120, -10.10425737566999871 ) ) ;
#49277 = DIRECTION ( 'NONE',  ( -2.678911359553000079E-11, -1.000000000000000000, 2.678929432950999965E-11 ) ) ;
#49278 = CARTESIAN_POINT ( 'NONE',  ( 12.50000000000000000, -61.48359816765000119, 1.003641516062000250 ) ) ;
#49279 = ORIENTED_EDGE ( 'NONE', *, *, #26108, .F. ) ;
#49280 = VECTOR ( 'NONE', #55209, 1000.000000000000000 ) ;
#49281 = CARTESIAN_POINT ( 'NONE',  ( -8.958657468006999025, -53.59887336276000269, -8.950049500613999953 ) ) ;
#49282 = ADVANCED_FACE ( 'NONE', ( #6024 ), #14452, .F. ) ;
#49283 = CIRCLE ( 'NONE', #52122, 0.5999999999999999778 ) ;
#49284 = CARTESIAN_POINT ( 'NONE',  ( -0.6514213267380000172, -79.65015981238198606, 9.745581310452999801 ) ) ;
#49285 = ORIENTED_EDGE ( 'NONE', *, *, #37333, .F. ) ;
#49286 = EDGE_LOOP ( 'NONE', ( #4114, #8039, #5145, #53053 ) ) ;
#49287 = CARTESIAN_POINT ( 'NONE',  ( -9.858444951501001086, -76.63967465741301055, 7.443044607738000806 ) ) ;
#49288 = CARTESIAN_POINT ( 'NONE',  ( -10.04959685401797032, -78.62904166612709389, -3.823887791762236699 ) ) ;
#49289 = CARTESIAN_POINT ( 'NONE',  ( -0.2341392558410000102, -78.09384532121998745, 1.516891056133000015 ) ) ;
#49290 = ORIENTED_EDGE ( 'NONE', *, *, #33717, .T. ) ;
#49291 = CARTESIAN_POINT ( 'NONE',  ( 8.256620083228000340, -77.39905584965399044, -4.688888258373000717 ) ) ;
#49292 = CARTESIAN_POINT ( 'NONE',  ( 7.406085232244485894, -77.54399565168795050, -6.270863524971103331 ) ) ;
#49293 = CARTESIAN_POINT ( 'NONE',  ( 1.181968933961157653, -80.32389716667498192, -0.4063731449358948256 ) ) ;
#49294 = CARTESIAN_POINT ( 'NONE',  ( -10.50899237707999845, -78.03174472164999997, 7.577845091584000770 ) ) ;
#49295 = CARTESIAN_POINT ( 'NONE',  ( 5.263131812197999970, -77.91386622752847302, -9.905430536777000583 ) ) ;
#49296 = DIRECTION ( 'NONE',  ( 0.6489586469986090567, 0.04890178910789071826, 0.7592504787669100974 ) ) ;
#49297 = CARTESIAN_POINT ( 'NONE',  ( 4.515731304085743858, -86.31452044230000809, 0.5183330846476985609 ) ) ;
#49298 = CARTESIAN_POINT ( 'NONE',  ( 1.099819419251000019, -79.76886766254099825, 11.16281809564999961 ) ) ;
#49299 = EDGE_CURVE ( 'NONE', #26517, #8180, #32573, .T. ) ;
#49300 = CARTESIAN_POINT ( 'NONE',  ( 8.864563766897090247, -79.87323291346528720, 2.649389835334180709 ) ) ;
#49301 = CARTESIAN_POINT ( 'NONE',  ( 8.121706841783367992, -17.16372996693625197, 9.841114038361700622 ) ) ;
#49302 = ORIENTED_EDGE ( 'NONE', *, *, #45383, .T. ) ;
#49303 = CARTESIAN_POINT ( 'NONE',  ( -10.98029981754000062, -80.11290934975998823, 1.094250890400999987 ) ) ;
#49304 = CARTESIAN_POINT ( 'NONE',  ( 1.379774402751460238, -77.23701117038012853, -9.169337788885616902 ) ) ;
#49305 = CARTESIAN_POINT ( 'NONE',  ( 1.161710437675000041, -79.54714775010999972, -0.9743588931339001169 ) ) ;
#49306 = AXIS2_PLACEMENT_3D ( 'NONE', #29478, #2074, #2921 ) ;
#49307 = CARTESIAN_POINT ( 'NONE',  ( -3.296692919738537064, -2.817192224941006629, 1.392370562533553180 ) ) ;
#49308 = CARTESIAN_POINT ( 'NONE',  ( -7.921329716887100858, -17.44906234264657741, 10.04564005581343267 ) ) ;
#49309 = CARTESIAN_POINT ( 'NONE',  ( 12.24159337356999977, -76.44530732801000283, -0.9828625608234000666 ) ) ;
#49310 = CARTESIAN_POINT ( 'NONE',  ( -9.358624512280380614, -80.44999999999998863, -5.407950800341189357 ) ) ;
#49311 = CARTESIAN_POINT ( 'NONE',  ( 9.791822688510999129, -79.34672475065998754, 5.349000663092000174 ) ) ;
#49312 = CARTESIAN_POINT ( 'NONE',  ( 7.497416719750999548, -77.63913832859898889, -6.041447127439999676 ) ) ;
#49313 = CARTESIAN_POINT ( 'NONE',  ( 9.098185902166729733, -77.24261121748705250, -8.011918831721102308 ) ) ;
#49314 = LINE ( 'NONE', #21566, #36537 ) ;
#49315 = CARTESIAN_POINT ( 'NONE',  ( -2.710423231297999891, -79.64442155979752158, 10.88447134676999895 ) ) ;
#49316 = AXIS2_PLACEMENT_3D ( 'NONE', #52008, #11562, #29540 ) ;
#49317 = B_SPLINE_SURFACE_WITH_KNOTS ( 'NONE', 3, 3, ( 
 ( #37870, #1585, #5411, #14844, #33436, #55297, #32838, #37282, #1297, #55890, #51472, #5131, #728, #19574, #18708, #50596, #32256, #41431, #18998, #36990, #55006, #32546, #33726, #52618, #43472, #29012, #52333, #11604, #43188, #47342, #3029, #21025, #11029, #42895, #20458, #6579, #47921, #34012, #39031, #6869, #24592, #47051, #38158, #57043, #52047, #24879, #21310, #16602, #48206, #16023, #29292, #34589, #12170, #38451, #29579, #42606, #2169, #20170, #56181, #7453, #34301, #15729, #30156, #25452, #2454, #7739, #56468 ),
 ( #25737, #57328, #39320, #47636, #2741, #7160, #25164, #11889, #20741, #38740, #43765, #3315, #16891, #34873, #51761, #11312, #56760, #16318, #29867, #4179, #40777, #53779, #4766, #58197, #36049, #22766, #48480, #27178, #39604, #12735, #22175, #26589, #44623, #53189, #17760, #31017, #49054, #26892, #44047, #39888, #3594, #21600, #8602, #13611, #26018, #369, #40184, #8312, #13018, #30730, #18350, #52903, #35747, #13313, #17169, #57609, #31308, #57904, #21881, #53477, #12452, #17458, #8899, #35446, #49351, #44916, #4473 ),
 ( #30447, #22473, #35154, #48766, #8023, #45217, #40484, #31606, #26311, #79, #18057, #44325, #3881, #54072, #49647, #9195, #2031, #11464, #32188, #33866, #51623, #55751, #23056, #20031, #50231, #15881, #19733, #6731, #45513, #41071, #38017, #54366, #15296, #56040, #9777, #36340, #15588, #51906, #7019, #658, #25021, #43042, #13905, #2603, #33289, #10886, #27767, #31900, #49942, #5059, #45809, #5343, #18644, #36634, #28861, #24154, #16461, #16173, #17316, #26452, #56905, #48628, #3178, #25596, #53332, #56614, #39749 ),
 ( #43909, #16751, #34731, #12598, #11746, #43616, #29725, #47776, #52759, #57759, #52190, #44475, #12314, #34442, #39172, #20881, #20600, #48915, #48343, #7881, #43327, #25308, #30302, #21168, #48066, #25883, #34151, #3455, #30596, #21461, #39468, #57472, #17033, #8175, #26177, #52475, #44195, #2885, #3742, #21745, #12880, #35303, #38885, #12033, #30011, #17614, #26745, #9640, #522, #50095, #13167, #49505, #31165, #32051, #58054, #45078, #36780, #23210, #40934, #58352, #235, #27626, #27337, #4025, #45668, #22030, #49203 ) ),
 .UNSPECIFIED., .F., .F., .F.,
 ( 4, 4 ),
 ( 4, 1, 1, 1, 1, 1, 1, 1, 1, 1, 1, 1, 1, 1, 1, 1, 1, 1, 1, 1, 1, 1, 1, 1, 1, 1, 1, 1, 1, 1, 1, 1, 1, 1, 1, 1, 1, 1, 1, 1, 1, 1, 1, 1, 1, 1, 1, 1, 1, 1, 1, 1, 1, 1, 1, 1, 1, 1, 1, 1, 1, 1, 1, 1, 4 ),
 ( -0.1387574078320999993, 1.138757407831999968 ),
 ( -0.02000000000000000042, -0.003749999999999999861, 0.01250000000000000069, 0.02875000000000000125, 0.04499999999999999833, 0.06124999999999999889, 0.07749999999999999944, 0.09375000000000000000, 0.1100000000000000006, 0.1262500000000000011, 0.1424999999999999878, 0.1587500000000000022, 0.1749999999999999889, 0.1912500000000000033, 0.2074999999999999900, 0.2237500000000000044, 0.2399999999999999911, 0.2562499999999999778, 0.2725000000000000200, 0.2887500000000000067, 0.3049999999999999933, 0.3212499999999999800, 0.3375000000000000222, 0.3537500000000000089, 0.3699999999999999956, 0.3862499999999999822, 0.4025000000000000244, 0.4187500000000000111, 0.4349999999999999978, 0.4512499999999999845, 0.4675000000000000266, 0.4837500000000000133, 0.5000000000000000000, 0.5162499999999999867, 0.5324999999999999734, 0.5487499999999999600, 0.5649999999999999467, 0.5812500000000000444, 0.5975000000000000311, 0.6137500000000000178, 0.6300000000000000044, 0.6462499999999999911, 0.6624999999999999778, 0.6787499999999999645, 0.6949999999999999512, 0.7112500000000000488, 0.7275000000000000355, 0.7437500000000000222, 0.7600000000000000089, 0.7762499999999999956, 0.7924999999999999822, 0.8087499999999999689, 0.8249999999999999556, 0.8412500000000000533, 0.8575000000000000400, 0.8737500000000000266, 0.8900000000000000133, 0.9062500000000000000, 0.9224999999999999867, 0.9387499999999999734, 0.9549999999999999600, 0.9712499999999999467, 0.9875000000000000444, 1.003749999999999920, 1.020000000000000018 ),
 .UNSPECIFIED. ) ;
#49318 = CARTESIAN_POINT ( 'NONE',  ( -8.343860018000999190, -59.94999999967000548, -8.343860018000999190 ) ) ;
#49319 = ORIENTED_EDGE ( 'NONE', *, *, #34513, .T. ) ;
#49320 = CARTESIAN_POINT ( 'NONE',  ( -1.308644393797000038, -81.43216705308998371, -0.6845726736234999388 ) ) ;
#49321 = CARTESIAN_POINT ( 'NONE',  ( 1.218119833583123146, -78.82945698446253857, -0.3274011781227666451 ) ) ;
#49322 = FACE_OUTER_BOUND ( 'NONE', #17976, .T. ) ;
#49323 = CARTESIAN_POINT ( 'NONE',  ( 10.46934363224000109, -77.28871046841200609, 5.823135730235999397 ) ) ;
#49324 = CARTESIAN_POINT ( 'NONE',  ( 0.000000000000000000, -75.15999999999999659, 0.000000000000000000 ) ) ;
#49325 = B_SPLINE_CURVE_WITH_KNOTS ( 'NONE', 3,
 ( #35334, #48656, #8785, #3207, #12627, #25625, #57499, #52502, #8200, #25912, #44220, #26481, #12060, #3769, #58083, #22059, #30623, #21772 ),
 .UNSPECIFIED., .F., .F.,
 ( 4, 2, 2, 2, 2, 2, 2, 2, 4 ),
 ( 0.000000000000000000, 0.1249999999999999722, 0.2500000000000000000, 0.3750000000000000000, 0.5000000000000001110, 0.6250000000000001110, 0.7500000000000000000, 0.8750000000000000000, 1.000000000000000000 ),
 .UNSPECIFIED. ) ;
#49326 = CIRCLE ( 'NONE', #16295, 3.000000000000000000 ) ;
#49327 = CARTESIAN_POINT ( 'NONE',  ( 0.9591162783412999771, -78.20799267308299818, -11.89603288543000126 ) ) ;
#49328 = CARTESIAN_POINT ( 'NONE',  ( 4.598371993787000456, -78.73414805011499595, -8.567308531191999421 ) ) ;
#49329 = CARTESIAN_POINT ( 'NONE',  ( 7.120006596302999924, -77.45084747358500010, 6.322648361264000094 ) ) ;
#49330 = CARTESIAN_POINT ( 'NONE',  ( -1.389926494652000022, -54.17618663712000426, -12.65988803918999928 ) ) ;
#49331 = CARTESIAN_POINT ( 'NONE',  ( 8.326851758844648899, -76.01173316031734828, 8.289602951553833421 ) ) ;
#49332 = B_SPLINE_CURVE_WITH_KNOTS ( 'NONE', 3,
 ( #18914, #54919, #14472, #28921, #30065, #20085, #48116, #43673, #56955, #20369 ),
 .UNSPECIFIED., .F., .F.,
 ( 4, 2, 2, 2, 4 ),
 ( 0.000000000000000000, 0.1562500009478632601, 0.3125000018957265202, 0.4687500028435898081, 0.6250000037914531514 ),
 .UNSPECIFIED. ) ;
#49333 = CARTESIAN_POINT ( 'NONE',  ( 1.070392484793000198, -79.89377542924650299, 10.86414404906000009 ) ) ;
#49334 = DIRECTION ( 'NONE',  ( -0.7071067811865475727, 0.000000000000000000, 0.7071067811865475727 ) ) ;
#49335 = EDGE_LOOP ( 'NONE', ( #42184, #16109, #13337 ) ) ;
#49336 = AXIS2_PLACEMENT_3D ( 'NONE', #47482, #56319, #33277 ) ;
#49337 = CARTESIAN_POINT ( 'NONE',  ( 4.594620150137029846, -78.13500000000000512, 8.363081028749705936 ) ) ;
#49338 = CARTESIAN_POINT ( 'NONE',  ( -0.1963495408493673156, -79.28541666666667709, 1.499999999999999556 ) ) ;
#49339 = CARTESIAN_POINT ( 'NONE',  ( -3.661088936265289195, -78.40681307385639798, -2.068643027229794651 ) ) ;
#49340 = CARTESIAN_POINT ( 'NONE',  ( 10.87588596538000019, -79.66941601242598381, -1.476184626237000197 ) ) ;
#49341 = CARTESIAN_POINT ( 'NONE',  ( -8.796335266379985640, -79.15208333333333712, -6.760013919724054965 ) ) ;
#49342 = CARTESIAN_POINT ( 'NONE',  ( -7.844390712406000610, -76.37070918080398485, 9.586582683531000626 ) ) ;
#49343 = CARTESIAN_POINT ( 'NONE',  ( 0.5189408976694140918, -79.25928653513095412, -1.150586733911741932 ) ) ;
#49344 = CARTESIAN_POINT ( 'NONE',  ( -9.006387858036243088, -76.95327272276941244, 6.000451096308640153 ) ) ;
#49345 = ORIENTED_EDGE ( 'NONE', *, *, #36983, .T. ) ;
#49346 = CARTESIAN_POINT ( 'NONE',  ( 2.047466772651000078, -79.91613885926460625, -11.07437783411999987 ) ) ;
#49347 = CARTESIAN_POINT ( 'NONE',  ( 9.021848782386655330, -77.26870337215281381, 2.167559314716497987 ) ) ;
#49348 = CARTESIAN_POINT ( 'NONE',  ( 11.98956178826566799, -75.80000000000001137, -0.9444271482678882057 ) ) ;
#49349 = FACE_BOUND ( 'NONE', #30248, .T. ) ;
#49350 = EDGE_CURVE ( 'NONE', #37882, #7601, #43669, .T. ) ;
#49351 = CARTESIAN_POINT ( 'NONE',  ( -10.03539896543000154, -79.70706551386098226, 4.876675511606999969 ) ) ;
#49352 = CARTESIAN_POINT ( 'NONE',  ( 8.696932689530999738, -76.29999999999999716, 6.318691462144000681 ) ) ;
#49353 = CARTESIAN_POINT ( 'NONE',  ( -10.98362417419999915, -23.15000000000000213, 0.5999999999999999778 ) ) ;
#49354 = CARTESIAN_POINT ( 'NONE',  ( 9.549999999999998934, -79.99999999999998579, 0.000000000000000000 ) ) ;
#49355 = CARTESIAN_POINT ( 'NONE',  ( 0.9218200799623742503, -81.17708333333334281, -1.199500263597268912 ) ) ;
#49356 = LINE ( 'NONE', #57335, #14151 ) ;
#49357 = CARTESIAN_POINT ( 'NONE',  ( 9.369164850722000892, -55.54999999966999980, -7.601397897754999633 ) ) ;
#49358 = EDGE_CURVE ( 'NONE', #24745, #9508, #762, .T. ) ;
#49359 = AXIS2_PLACEMENT_3D ( 'NONE', #54543, #40960, #33248 ) ;
#49360 = CARTESIAN_POINT ( 'NONE',  ( -12.65989858207000118, -24.94344101132999825, 0.9743214026256000748 ) ) ;
#49361 = VERTEX_POINT ( 'NONE', #54749 ) ;
#49362 = ORIENTED_EDGE ( 'NONE', *, *, #39826, .T. ) ;
#49363 = CARTESIAN_POINT ( 'NONE',  ( -7.596835002782708735, -78.45208333333333428, -5.838193839761694370 ) ) ;
#49364 = ORIENTED_EDGE ( 'NONE', *, *, #25335, .F. ) ;
#49365 = CARTESIAN_POINT ( 'NONE',  ( 9.499549289235639904, -79.50042064254546403, 0.05021470316550929319 ) ) ;
#49366 = ORIENTED_EDGE ( 'NONE', *, *, #51188, .T. ) ;
#49367 = CARTESIAN_POINT ( 'NONE',  ( 8.790688707546999936, -24.93813493249999880, 8.797962936834998970 ) ) ;
#49368 = CARTESIAN_POINT ( 'NONE',  ( -9.053955183288000086, -76.62058518366599458, -6.099285168125999412 ) ) ;
#49369 = EDGE_CURVE ( 'NONE', #37143, #11113, #32349, .T. ) ;
#49370 = VECTOR ( 'NONE', #31383, 1000.000000000000000 ) ;
#49371 = CARTESIAN_POINT ( 'NONE',  ( -7.612971540294999784, -60.12452273675999947, 10.53003236235000095 ) ) ;
#49372 = CARTESIAN_POINT ( 'NONE',  ( -1.250000000000000000, -82.99999999999998579, 0.000000000000000000 ) ) ;
#49373 = CARTESIAN_POINT ( 'NONE',  ( -6.539788562102244462, -78.16268306815329936, -6.541533809854823467 ) ) ;
#49374 = CARTESIAN_POINT ( 'NONE',  ( -11.19989528650999944, -78.69393902665500207, 0.6168112860373000661 ) ) ;
#49375 = CARTESIAN_POINT ( 'NONE',  ( 3.250000000000000000, -1.850000000000000089, 0.000000000000000000 ) ) ;
#49376 = ADVANCED_FACE ( 'NONE', ( #11915 ), #32541, .F. ) ;
#49377 = EDGE_LOOP ( 'NONE', ( #58357, #20255, #24887, #12602 ) ) ;
#49378 = ORIENTED_EDGE ( 'NONE', *, *, #51033, .F. ) ;
#49379 = CARTESIAN_POINT ( 'NONE',  ( 1.180810718627301803, -77.46484884203415788, 9.175185427096824498 ) ) ;
#49380 = CARTESIAN_POINT ( 'NONE',  ( 10.74764839381999870, -78.17848693479398037, -0.2248421733643000131 ) ) ;
#49381 = DIRECTION ( 'NONE',  ( 0.000000000000000000, -1.000000000000000000, 0.000000000000000000 ) ) ;
#49382 = CARTESIAN_POINT ( 'NONE',  ( -9.626984307556000431, -78.38041163157799929, 1.221426423741999834 ) ) ;
#49383 = CARTESIAN_POINT ( 'NONE',  ( 10.37229188467999919, -76.53786495648000709, -6.269923847882999723 ) ) ;
#49384 = CARTESIAN_POINT ( 'NONE',  ( -8.466964544433025708, -79.43743728541620897, -4.308145801908138672 ) ) ;
#49385 = CARTESIAN_POINT ( 'NONE',  ( 10.21026245498356033, -54.54392421755085962, -7.764236519575772100 ) ) ;
#49386 = B_SPLINE_CURVE_WITH_KNOTS ( 'NONE', 3,
 ( #51908, #33867, #55753, #46325 ),
 .UNSPECIFIED., .F., .F.,
 ( 4, 4 ),
 ( 0.000000000000000000, 1.000000000000000000 ),
 .UNSPECIFIED. ) ;
#49387 = DIRECTION ( 'NONE',  ( 0.000000000000000000, -1.000000000000000000, 0.000000000000000000 ) ) ;
#49388 = CARTESIAN_POINT ( 'NONE',  ( 12.59682398758999966, -18.61262488659000169, -1.801644812721000077 ) ) ;
#49389 = CARTESIAN_POINT ( 'NONE',  ( -10.13402523425000012, -23.72303809441999789, -7.647751776486000352 ) ) ;
#49390 = CARTESIAN_POINT ( 'NONE',  ( -11.37990774082085466, -76.67987294336911930, 2.931073317825884317 ) ) ;
#49391 = CARTESIAN_POINT ( 'NONE',  ( 3.756302695449999618, -85.14779509595699380, 0.03950336994162999965 ) ) ;
#49392 = ORIENTED_EDGE ( 'NONE', *, *, #39337, .T. ) ;
#49393 = CARTESIAN_POINT ( 'NONE',  ( 6.535144700214000402, -79.27162967006100303, 10.44020558090000073 ) ) ;
#49394 = CARTESIAN_POINT ( 'NONE',  ( -10.15588082254999946, -76.17008402689499746, 5.382090387917999763 ) ) ;
#49395 = CARTESIAN_POINT ( 'NONE',  ( -7.030156735645810784, -78.03177828160880836, 8.132844556063748342 ) ) ;
#49396 = CARTESIAN_POINT ( 'NONE',  ( -10.86788298907000083, -77.73623996705498485, -5.040355520269000245 ) ) ;
#49397 = EDGE_CURVE ( 'NONE', #23446, #16168, #25193, .T. ) ;
#49398 = DIRECTION ( 'NONE',  ( 9.558576152644999723E-12, 1.000000000000000000, 3.007563087384999928E-10 ) ) ;
#49400 = FACE_OUTER_BOUND ( 'NONE', #12464, .T. ) ;
#49399 = CARTESIAN_POINT ( 'NONE',  ( -3.075537641221531615, -78.40416666666666856, -11.44417895085270942 ) ) ;
#49401 = DIRECTION ( 'NONE',  ( 0.000000000000000000, 1.000000000000000000, 0.000000000000000000 ) ) ;
#49402 = CARTESIAN_POINT ( 'NONE',  ( 1.677588531244923464, -80.96289356016140459, 10.61806853404734419 ) ) ;
#49403 = CARTESIAN_POINT ( 'NONE',  ( 10.18491080491000034, -55.49283319101999723, -7.640030264136999705 ) ) ;
#49404 = CARTESIAN_POINT ( 'NONE',  ( -4.000000000000000000, -75.00000000000001421, -0.5999999999999999778 ) ) ;
#49405 = CARTESIAN_POINT ( 'NONE',  ( -9.992683672509999226, -78.35460208417299555, 4.939724043997999914 ) ) ;
#49406 = CARTESIAN_POINT ( 'NONE',  ( 12.00000000000000000, -78.04999999999999716, 0.000000000000000000 ) ) ;
#49407 = CARTESIAN_POINT ( 'NONE',  ( 1.439896632895284911, -80.06458333334573751, 11.00000000000000355 ) ) ;
#49408 = ORIENTED_EDGE ( 'NONE', *, *, #52709, .T. ) ;
#49409 = CARTESIAN_POINT ( 'NONE',  ( 3.042547531669000271, -78.24783470746899638, -10.31045122763999977 ) ) ;
#49410 = AXIS2_PLACEMENT_3D ( 'NONE', #25732, #29575, #20450 ) ;
#49411 = CARTESIAN_POINT ( 'NONE',  ( 1.930638663168000146, -55.57877936677999742, 12.72375916870000090 ) ) ;
#49412 = CARTESIAN_POINT ( 'NONE',  ( -12.83044027761000017, -18.69360215052999763, 2.062670899361999766 ) ) ;
#49413 = CARTESIAN_POINT ( 'NONE',  ( -2.548053818379999669, -3.743360633963999984, 2.532771267353999711 ) ) ;
#49414 = CARTESIAN_POINT ( 'NONE',  ( 8.282307197233999219, -77.88941935644699299, -7.564489280985000619 ) ) ;
#49415 = CARTESIAN_POINT ( 'NONE',  ( 2.598917237794088564, -1.697916666666666519, -1.997276839918468605 ) ) ;
#49416 = DIRECTION ( 'NONE',  ( 0.000000000000000000, 0.000000000000000000, -1.000000000000000000 ) ) ;
#49417 = DIRECTION ( 'NONE',  ( 0.000000000000000000, 1.000000000000000000, 0.000000000000000000 ) ) ;
#49418 = CARTESIAN_POINT ( 'NONE',  ( 12.66001647286000065, -17.36746073369999621, 1.381678996660999914 ) ) ;
#49419 = CARTESIAN_POINT ( 'NONE',  ( -4.095422038743000925, -84.91932450217399264, -0.5348100902707000337 ) ) ;
#49420 = DIRECTION ( 'NONE',  ( 1.000000000000000000, 0.000000000000000000, 0.000000000000000000 ) ) ;
#49421 = CARTESIAN_POINT ( 'NONE',  ( 0.000000000000000000, -81.99999999999998579, -7.000000000000000000 ) ) ;
#49422 = CARTESIAN_POINT ( 'NONE',  ( 4.636146969708000221, -78.82343122293001159, -11.75666478071000043 ) ) ;
#49423 = CARTESIAN_POINT ( 'NONE',  ( 4.249074618647000534, -76.86498468449899235, -10.30533674824999935 ) ) ;
#49424 = CARTESIAN_POINT ( 'NONE',  ( 0.9441861370063999725, -79.53822423548000131, 1.372505234203999835 ) ) ;
#49425 = CARTESIAN_POINT ( 'NONE',  ( 0.3963282436660999775, -77.97416723434000119, -1.615693196437999912 ) ) ;
#49426 = CARTESIAN_POINT ( 'NONE',  ( -0.6484536763444428420, -61.92402982674907719, 12.70397497896646932 ) ) ;
#49427 = CARTESIAN_POINT ( 'NONE',  ( 1.545316077588782866, -82.50099648747466574, 0.02805363615183451356 ) ) ;
#49428 = CARTESIAN_POINT ( 'NONE',  ( -12.46083365857999858, -60.48341615446999953, 1.628972628240000109 ) ) ;
#49429 = CARTESIAN_POINT ( 'NONE',  ( -2.849102345952564619, -80.20408735378460108, -10.37120360196352209 ) ) ;
#49430 = CARTESIAN_POINT ( 'NONE',  ( 12.60356226360999798, -22.75077028889999653, -1.750000000000000000 ) ) ;
#49431 = CARTESIAN_POINT ( 'NONE',  ( 6.879672600168782459, -79.17236621673578156, 8.859554948090913484 ) ) ;
#49432 = VERTEX_POINT ( 'NONE', #38481 ) ;
#49433 = CARTESIAN_POINT ( 'NONE',  ( 1.094998213286220823, -81.80994750764530465, -0.6032700728990865180 ) ) ;
#49434 = ADVANCED_FACE ( 'NONE', ( #16054 ), #52076, .T. ) ;
#49435 = CARTESIAN_POINT ( 'NONE',  ( 1.439896632895317552, -79.46458333333332291, 11.00000000000000000 ) ) ;
#49436 = CARTESIAN_POINT ( 'NONE',  ( 7.861046360898000351, -79.70384861441699798, 7.903072230637000040 ) ) ;
#49437 = VECTOR ( 'NONE', #20687, 1000.000000000000000 ) ;
#49438 = CARTESIAN_POINT ( 'NONE',  ( -10.75000000000000000, -79.59999999999999432, 0.000000000000000000 ) ) ;
#49439 = ORIENTED_EDGE ( 'NONE', *, *, #43576, .T. ) ;
#49440 = VERTEX_POINT ( 'NONE', #43211 ) ;
#49441 = EDGE_CURVE ( 'NONE', #41447, #24970, #30459, .T. ) ;
#49442 = DIRECTION ( 'NONE',  ( 0.000000000000000000, 1.000000000000000000, 0.000000000000000000 ) ) ;
#49443 = ORIENTED_EDGE ( 'NONE', *, *, #16396, .F. ) ;
#49444 = FACE_OUTER_BOUND ( 'NONE', #46496, .T. ) ;
#49445 = VERTEX_POINT ( 'NONE', #38769 ) ;
#49446 = CARTESIAN_POINT ( 'NONE',  ( 9.722718241315000398, -60.04999999966999980, 7.247844507162001015 ) ) ;
#49447 = CARTESIAN_POINT ( 'NONE',  ( 0.000000000000000000, -81.19999999999998863, 6.000000000000000000 ) ) ;
#49448 = DIRECTION ( 'NONE',  ( 0.000000000000000000, -0.7071067811866525998, -0.7071067811864425456 ) ) ;
#49449 = B_SPLINE_CURVE_WITH_KNOTS ( 'NONE', 3,
 ( #30289, #48329, #8160, #7868 ),
 .UNSPECIFIED., .F., .F.,
 ( 4, 4 ),
 ( 0.000000000000000000, 1.000000000000000000 ),
 .UNSPECIFIED. ) ;
#49450 = CARTESIAN_POINT ( 'NONE',  ( 10.46019799182000121, -79.91686644544779483, 3.505129431450999977 ) ) ;
#49451 = CARTESIAN_POINT ( 'NONE',  ( 1.389926494651000155, -24.62381336254999908, -12.65988803923000106 ) ) ;
#49452 = CIRCLE ( 'NONE', #38096, 0.5000000000000006661 ) ;
#49453 = CARTESIAN_POINT ( 'NONE',  ( -0.05492852729254000393, -80.13320636806399477, 3.756108806030999947 ) ) ;
#49454 = CARTESIAN_POINT ( 'NONE',  ( -4.760392715106998907, -79.31640648056026066, 8.226848814529617471 ) ) ;
#49455 = CARTESIAN_POINT ( 'NONE',  ( -9.177034484502000211, -77.30309342897207614, 6.137278520473000043 ) ) ;
#49457 = EDGE_CURVE ( 'NONE', #36425, #5025, #33936, .T. ) ;
#49456 = CARTESIAN_POINT ( 'NONE',  ( 10.77676250696000082, -79.20748630253001465, 5.740077567832999605 ) ) ;
#49458 = ORIENTED_EDGE ( 'NONE', *, *, #19753, .T. ) ;
#49459 = ORIENTED_EDGE ( 'NONE', *, *, #48133, .T. ) ;
#49460 = DIRECTION ( 'NONE',  ( 1.000000000000000000, 0.000000000000000000, 0.000000000000000000 ) ) ;
#49461 = DIRECTION ( 'NONE',  ( 0.000000000000000000, 1.000000000000000000, 0.000000000000000000 ) ) ;
#49462 = CARTESIAN_POINT ( 'NONE',  ( -1.185397549814999785, -80.25976351251399876, -0.6110718436566999756 ) ) ;
#49463 = CARTESIAN_POINT ( 'NONE',  ( 9.662203867310999783, -78.96694624104797811, 0.9012207007054000574 ) ) ;
#49464 = DIRECTION ( 'NONE',  ( 0.000000000000000000, 0.000000000000000000, -1.000000000000000000 ) ) ;
#49465 = CARTESIAN_POINT ( 'NONE',  ( 5.380788203752000065, -76.23673944062498720, 9.804131929786001010 ) ) ;
#49466 = CARTESIAN_POINT ( 'NONE',  ( -1.184344363998000027, -77.03625595695000072, -12.90193715879000003 ) ) ;
#49467 = CARTESIAN_POINT ( 'NONE',  ( -0.5717664302369001028, -80.67025799034000499, -1.224358761826999986 ) ) ;
#49468 = CARTESIAN_POINT ( 'NONE',  ( -1.394094229632999893, -76.41181109130799598, 10.79476414467999845 ) ) ;
#49469 = LINE ( 'NONE', #22879, #31235 ) ;
#49470 = CARTESIAN_POINT ( 'NONE',  ( 11.14639666075000157, -81.07231824355980621, -1.632917082138999776 ) ) ;
#49471 = CARTESIAN_POINT ( 'NONE',  ( -7.954951288349001004, -18.55321828668999729, 9.722718241315000398 ) ) ;
#49472 = CARTESIAN_POINT ( 'NONE',  ( 2.970834971129885815, -2.884370106164003467, 1.316369104713672966 ) ) ;
#49473 = CARTESIAN_POINT ( 'NONE',  ( -1.194669669092999875, -82.01182046129099490, -3.340258828557999493 ) ) ;
#49474 = CARTESIAN_POINT ( 'NONE',  ( 4.000000000000000000, -75.00000000000001421, -0.5999999999999999778 ) ) ;
#49475 = CARTESIAN_POINT ( 'NONE',  ( 10.70339364929999881, -81.17020448283959411, 2.537196166659999808 ) ) ;
#49476 = CARTESIAN_POINT ( 'NONE',  ( -0.6934022908089999548, -3.241579146514999898, 3.742362521638999961 ) ) ;
#49477 = CARTESIAN_POINT ( 'NONE',  ( 1.164955675041443817, -80.04001182890594635, 0.6368716809728905970 ) ) ;
#49478 = ORIENTED_EDGE ( 'NONE', *, *, #53613, .F. ) ;
#49479 = CARTESIAN_POINT ( 'NONE',  ( 0.5200379331771535218, -23.45155696396579970, 10.98772212209804700 ) ) ;
#49480 = DIRECTION ( 'NONE',  ( 0.000000000000000000, 1.000000000000000000, 0.000000000000000000 ) ) ;
#49481 = AXIS2_PLACEMENT_3D ( 'NONE', #5669, #5385, #41403 ) ;
#49482 = CARTESIAN_POINT ( 'NONE',  ( 0.6224761083686999319, -81.92930503473399995, -1.179448874982999884 ) ) ;
#49483 = CIRCLE ( 'NONE', #52303, 0.5000000000000004441 ) ;
#49484 = CARTESIAN_POINT ( 'NONE',  ( -12.54902617719999824, -16.99030198144999915, -0.4617931494615999943 ) ) ;
#49485 = CARTESIAN_POINT ( 'NONE',  ( 11.88928085110999966, -78.26597965894998765, 5.289737169833999886 ) ) ;
#49486 = EDGE_CURVE ( 'NONE', #57807, #28437, #56787, .T. ) ;
#49487 = CARTESIAN_POINT ( 'NONE',  ( -9.073558136300860610, -62.02808769461389460, -8.894842552386064582 ) ) ;
#49488 = CARTESIAN_POINT ( 'NONE',  ( 12.71798280855999863, -23.29778595484999926, -1.931086388455000025 ) ) ;
#49489 = ORIENTED_EDGE ( 'NONE', *, *, #41967, .F. ) ;
#49490 = TOROIDAL_SURFACE ( 'NONE', #34378, 8.500000000000000000, 2.000000000000000000 ) ;
#49491 = CARTESIAN_POINT ( 'NONE',  ( 9.502921958894958721, -54.05907999833515021, -8.179400290810697527 ) ) ;
#49492 = CARTESIAN_POINT ( 'NONE',  ( 1.339915889275999916, -81.06493106288900208, -0.6881352248621999124 ) ) ;
#49493 = CARTESIAN_POINT ( 'NONE',  ( 7.613962745610000304, -18.69360215052999763, -10.53101990620000095 ) ) ;
#49494 = CARTESIAN_POINT ( 'NONE',  ( -2.523869816676000077, -78.56059042997900121, -9.181528052588999955 ) ) ;
#49496 = CARTESIAN_POINT ( 'NONE',  ( 2.301364338783000285, -1.525557261822999999, -3.291430154679999998 ) ) ;
#49495 = CARTESIAN_POINT ( 'NONE',  ( 3.637992502009999463, -85.14393562394799631, -1.955383377840000048 ) ) ;
#49497 = CARTESIAN_POINT ( 'NONE',  ( -1.799501877759999813, -60.08917565288000162, -12.60552522438000089 ) ) ;
#49498 = CARTESIAN_POINT ( 'NONE',  ( 0.9925657212695000453, -80.28940021773100000, -1.012359935335999994 ) ) ;
#49499 = ORIENTED_EDGE ( 'NONE', *, *, #8298, .F. ) ;
#49500 = CARTESIAN_POINT ( 'NONE',  ( -2.343696616972932745, -77.20767214764329367, -10.49131370137163621 ) ) ;
#49501 = CYLINDRICAL_SURFACE ( 'NONE', #10609, 14.00000000000000000 ) ;
#49502 = CYLINDRICAL_SURFACE ( 'NONE', #46983, 1.250000000000000000 ) ;
#49503 = EDGE_LOOP ( 'NONE', ( #38358, #10099, #15459, #9938, #27269 ) ) ;
#49504 = ORIENTED_EDGE ( 'NONE', *, *, #32734, .F. ) ;
#49505 = CARTESIAN_POINT ( 'NONE',  ( -3.536853559812999759, -79.46961638910198644, -10.35270415072999839 ) ) ;
#49506 = CARTESIAN_POINT ( 'NONE',  ( 9.050966798898000931, -59.94999999040999938, 7.919595949288999570 ) ) ;
#49507 = CARTESIAN_POINT ( 'NONE',  ( 0.000000000000000000, -75.10000000019110189, 0.000000000000000000 ) ) ;
#49508 = ORIENTED_EDGE ( 'NONE', *, *, #45300, .F. ) ;
#49509 = EDGE_CURVE ( 'NONE', #16536, #30070, #12763, .T. ) ;
#49510 = CARTESIAN_POINT ( 'NONE',  ( 6.891697027498000061, -78.79739778831900310, -9.743716654505998775 ) ) ;
#49511 = ORIENTED_EDGE ( 'NONE', *, *, #31790, .T. ) ;
#49512 = ORIENTED_EDGE ( 'NONE', *, *, #23501, .F. ) ;
#49513 = CARTESIAN_POINT ( 'NONE',  ( -1.872510430921729752, -2.676471623700526159, -2.659056711493340774 ) ) ;
#49514 = LINE ( 'NONE', #4639, #27601 ) ;
#49515 = CARTESIAN_POINT ( 'NONE',  ( -3.758731266216853939, -1.376714976881707297, -1.426415079042028689 ) ) ;
#49516 = ORIENTED_EDGE ( 'NONE', *, *, #13867, .F. ) ;
#49518 = ADVANCED_FACE ( 'NONE', ( #23313 ), #34242, .T. ) ;
#49517 = LINE ( 'NONE', #13183, #31787 ) ;
#49519 = VERTEX_POINT ( 'NONE', #37402 ) ;
#49520 = CARTESIAN_POINT ( 'NONE',  ( -1.257915819032439098, -80.16243413275964258, -0.2016166298787092637 ) ) ;
#49521 = VECTOR ( 'NONE', #13779, 1000.000000000000000 ) ;
#49522 = CYLINDRICAL_SURFACE ( 'NONE', #170, 10.69999999999999929 ) ;
#49523 = FACE_OUTER_BOUND ( 'NONE', #47547, .T. ) ;
#49524 = VECTOR ( 'NONE', #30637, 1000.000000000000000 ) ;
#49525 = CARTESIAN_POINT ( 'NONE',  ( -9.939389728518001732, -76.66042233052399979, 5.126617716248000001 ) ) ;
#49526 = DIRECTION ( 'NONE',  ( -1.000000000000000000, 0.000000000000000000, 0.000000000000000000 ) ) ;
#49527 = AXIS2_PLACEMENT_3D ( 'NONE', #11361, #15775, #33767 ) ;
#49528 = CARTESIAN_POINT ( 'NONE',  ( 10.26699006316251683, -78.59166666666666856, 5.917523019358090330 ) ) ;
#49529 = CARTESIAN_POINT ( 'NONE',  ( 7.919842512017161162, -77.46752299044597123, 8.988445846368001924 ) ) ;
#49530 = CARTESIAN_POINT ( 'NONE',  ( 0.06586989957135422347, -78.72571929582086625, -9.249708549591806772 ) ) ;
#49531 = CARTESIAN_POINT ( 'NONE',  ( -8.485538010655998775, -24.88067982437999959, 9.101501073481999882 ) ) ;
#49532 = DIRECTION ( 'NONE',  ( 0.000000000000000000, 1.000000000000000000, 0.000000000000000000 ) ) ;
#49533 = CARTESIAN_POINT ( 'NONE',  ( 6.760013919724039866, -78.42291666666669414, 8.796335266379998075 ) ) ;
#49534 = CARTESIAN_POINT ( 'NONE',  ( 9.137847679653942734, -78.14631709695343886, -7.887011953151875865 ) ) ;
#49535 = CARTESIAN_POINT ( 'NONE',  ( 2.572610278691000119, -82.17700264934799748, -3.288083568311999993 ) ) ;
#49536 = CARTESIAN_POINT ( 'NONE',  ( -9.851679666438998950, -77.32586001420199295, -0.6446771120444999559 ) ) ;
#49537 = PRODUCT_DEFINITION ( 'UNKNOWN', '', #6519, #53417 ) ;
#49538 = CARTESIAN_POINT ( 'NONE',  ( 1.210984793496805656, -79.72721317835664934, -0.3578339234309608208 ) ) ;
#49539 = DIRECTION ( 'NONE',  ( 9.217554796542082011E-07, 2.920569602132825499E-20, -0.9999999999995752287 ) ) ;
#49540 = CARTESIAN_POINT ( 'NONE',  ( -2.062323307449999810, -23.22713153192000135, 12.83634826442999888 ) ) ;
#49541 = DIRECTION ( 'NONE',  ( 1.000000000000000000, 0.000000000000000000, 0.000000000000000000 ) ) ;
#49542 = CARTESIAN_POINT ( 'NONE',  ( 1.096138950756000208, -84.26882685001099560, 3.373876015865000078 ) ) ;
#49543 = CARTESIAN_POINT ( 'NONE',  ( -1.466295893230999958, -0.9762401806307999808, -3.674175840820999905 ) ) ;
#49544 = CARTESIAN_POINT ( 'NONE',  ( -0.7022187824378000043, -82.19906693409399168, -1.095132696781000003 ) ) ;
#49545 = CARTESIAN_POINT ( 'NONE',  ( 1.750000000001000089, -55.54999998977000075, -12.56594317853999954 ) ) ;
#49546 = CARTESIAN_POINT ( 'NONE',  ( 1.292974957763964872, -81.14285663376836055, 0.7849688150825027133 ) ) ;
#49547 = CARTESIAN_POINT ( 'NONE',  ( -1.085375040598030250, -78.55880290454010151, 0.6235288048130009919 ) ) ;
#49548 = CARTESIAN_POINT ( 'NONE',  ( 0.000000000000000000, -74.64999999999999147, 0.000000000000000000 ) ) ;
#49549 = CARTESIAN_POINT ( 'NONE',  ( 0.000000000000000000, -72.39999999999999147, 0.000000000000000000 ) ) ;
#49550 = CARTESIAN_POINT ( 'NONE',  ( -5.702669450565000631, -77.94532935296300025, 9.308862826782998923 ) ) ;
#49551 = ADVANCED_FACE ( 'NONE', ( #19412 ), #34008, .T. ) ;
#49552 = CARTESIAN_POINT ( 'NONE',  ( 4.023394881099000564, -78.22184600323399195, 11.60207191892000012 ) ) ;
#49553 = CARTESIAN_POINT ( 'NONE',  ( -9.146956334765604879, -78.14765838888041571, -6.250533269645468515 ) ) ;
#49555 = CARTESIAN_POINT ( 'NONE',  ( -1.428376501803000131, -77.83869253983340286, 0.2580938706625000023 ) ) ;
#49554 = DIRECTION ( 'NONE',  ( 0.000000000000000000, 0.000000000000000000, -1.000000000000000000 ) ) ;
#49556 = LINE ( 'NONE', #45129, #23769 ) ;
#49557 = ORIENTED_EDGE ( 'NONE', *, *, #2244, .T. ) ;
#49558 = EDGE_CURVE ( 'NONE', #55909, #50392, #10016, .T. ) ;
#49559 = CARTESIAN_POINT ( 'NONE',  ( 3.426173589824000221, -82.67079877876498983, -1.262548838661999850 ) ) ;
#49560 = CARTESIAN_POINT ( 'NONE',  ( 17.50000000000000000, -15.06282895647999887, 3.979097884520999899E-10 ) ) ;
#49561 = CIRCLE ( 'NONE', #33526, 0.5999999999999999778 ) ;
#49562 = CARTESIAN_POINT ( 'NONE',  ( 7.508137979765999503, -79.88746266619089909, 7.790962400017000355 ) ) ;
#49563 = CARTESIAN_POINT ( 'NONE',  ( -9.185039845617701815, -80.00000000000001421, -1.456806635703324915 ) ) ;
#49564 = CARTESIAN_POINT ( 'NONE',  ( 2.052407343088218816, -84.17291667838408387, 2.765357313056269639 ) ) ;
#49565 = CARTESIAN_POINT ( 'NONE',  ( 6.433795189870999742, -77.50750594596499354, -9.188274595716000803 ) ) ;
#49566 = CARTESIAN_POINT ( 'NONE',  ( 13.79999999999999893, 0.000000000000000000, 0.000000000000000000 ) ) ;
#49567 = CARTESIAN_POINT ( 'NONE',  ( 9.725848778082999857, -78.57495809405799037, -0.5172632330995999839 ) ) ;
#49568 = CARTESIAN_POINT ( 'NONE',  ( 0.6653596569558999363, -1.443831454374000067, -3.971211220357999672 ) ) ;
#49569 = CARTESIAN_POINT ( 'NONE',  ( 1.998841639285485527, -76.43855673768001679, -11.64912468341469776 ) ) ;
#49570 = CARTESIAN_POINT ( 'NONE',  ( -3.399186938124999724, -77.19999999999998863, -10.46162167925000119 ) ) ;
#49571 = CARTESIAN_POINT ( 'NONE',  ( -2.062503053667999797, -58.55736537918999574, 12.92177931905999877 ) ) ;
#49572 = VERTEX_POINT ( 'NONE', #10560 ) ;
#49573 = CARTESIAN_POINT ( 'NONE',  ( 1.500000000000000000, -80.75000000000000000, 0.000000000000000000 ) ) ;
#49574 = CARTESIAN_POINT ( 'NONE',  ( -1.884618100832999854, -79.80191332859899944, -9.129359532056000148 ) ) ;
#49575 = CARTESIAN_POINT ( 'NONE',  ( -7.958763982144999360, -54.32301960774000094, -9.723170657514000226 ) ) ;
#49576 = CARTESIAN_POINT ( 'NONE',  ( 1.199500263597271577, -81.59791666666669130, -0.9218200799623702535 ) ) ;
#49577 = CARTESIAN_POINT ( 'NONE',  ( 1.417725061834000044, -80.09482849775000091, -0.8748226493128999914 ) ) ;
#49578 = CARTESIAN_POINT ( 'NONE',  ( -12.87022657274000004, -59.58485473249000108, -2.062597299672999540 ) ) ;
#49579 = CARTESIAN_POINT ( 'NONE',  ( -3.250000000000000000, -2.600000000000000089, 0.000000000000000000 ) ) ;
#49580 = ORIENTED_EDGE ( 'NONE', *, *, #54291, .T. ) ;
#49581 = ADVANCED_FACE ( 'NONE', ( #14969 ), #9388, .F. ) ;
#49582 = CARTESIAN_POINT ( 'NONE',  ( 11.07931224411999871, -77.73081168025198906, -1.719192531530000068 ) ) ;
#49583 = CARTESIAN_POINT ( 'NONE',  ( 2.598917237794088564, -1.197916666666666963, -1.997276839918468605 ) ) ;
#49584 = EDGE_LOOP ( 'NONE', ( #50733, #50623, #25177, #17179, #14795 ) ) ;
#49585 = ORIENTED_EDGE ( 'NONE', *, *, #51695, .F. ) ;
#49586 = CARTESIAN_POINT ( 'NONE',  ( -7.948094694382998426, -54.35965255578000210, -9.636752590464999102 ) ) ;
#49587 = CARTESIAN_POINT ( 'NONE',  ( 9.202039358297998461, -80.03983171147699238, 2.360608321670000453 ) ) ;
#49588 = ORIENTED_EDGE ( 'NONE', *, *, #33929, .T. ) ;
#49590 = EDGE_CURVE ( 'NONE', #1742, #42116, #11400, .T. ) ;
#49589 = CARTESIAN_POINT ( 'NONE',  ( 10.13128904261999885, -76.32605116317100169, -6.858865348462000355 ) ) ;
#49591 = CARTESIAN_POINT ( 'NONE',  ( -8.547755989943867760, -78.65230355551688035, -6.557738066417508449 ) ) ;
#49592 = CARTESIAN_POINT ( 'NONE',  ( 0.7985095004294999743, -78.10473044020999112, 1.441967081790000105 ) ) ;
#49593 = EDGE_CURVE ( 'NONE', #57120, #51909, #50721, .T. ) ;
#49594 = VERTEX_POINT ( 'NONE', #9975 ) ;
#49595 = CARTESIAN_POINT ( 'NONE',  ( 9.426477049435000310, -77.31037305011500393, -1.139727483088999849 ) ) ;
#49596 = DIRECTION ( 'NONE',  ( 0.000000000000000000, 0.000000000000000000, -1.000000000000000000 ) ) ;
#49597 = CARTESIAN_POINT ( 'NONE',  ( -9.412102823527000339, -78.05567315384000437, -9.131157420175998851 ) ) ;
#49598 = CARTESIAN_POINT ( 'NONE',  ( 9.144378690012999300, -77.45084839649746300, -6.496033325431000094 ) ) ;
#49599 = CARTESIAN_POINT ( 'NONE',  ( 1.441729589605054818, -86.39318692614399708, 3.322092378136251689 ) ) ;
#49600 = CARTESIAN_POINT ( 'NONE',  ( -9.669247687117000112, -77.75675262319563785, -0.8224101967608998809 ) ) ;
#49601 = CIRCLE ( 'NONE', #11888, 1.750000000000000000 ) ;
#49602 = CARTESIAN_POINT ( 'NONE',  ( 8.989019320876588282, -79.86904670615129476, 2.181506882885325904 ) ) ;
#49603 = CARTESIAN_POINT ( 'NONE',  ( 3.403319483155256009, -79.31666665249466064, -2.125768741672802609 ) ) ;
#49604 = VERTEX_POINT ( 'NONE', #564 ) ;
#49605 = CARTESIAN_POINT ( 'NONE',  ( -9.512853590378179902, -77.34556464508717966, 0.5183098463306959891 ) ) ;
#49606 = CARTESIAN_POINT ( 'NONE',  ( 5.894077591580000330, -76.71673252672998444, -10.80721126921000064 ) ) ;
#49607 = CARTESIAN_POINT ( 'NONE',  ( 1.590911073979999868, -80.64438452883999275, -0.2760724992506000119 ) ) ;
#49608 = VECTOR ( 'NONE', #2220, 1000.000000000000000 ) ;
#49609 = CARTESIAN_POINT ( 'NONE',  ( -2.677348439713063133, -3.405484581173921388, -2.283878904445620694 ) ) ;
#49610 = ADVANCED_FACE ( 'NONE', ( #5821 ), #22130, .F. ) ;
#49611 = CARTESIAN_POINT ( 'NONE',  ( -7.712209501881797102, -17.93822238229371635, 10.27335463211299960 ) ) ;
#49612 = CARTESIAN_POINT ( 'NONE',  ( 10.16964605767000052, -76.40432458970499852, -6.884832982024000181 ) ) ;
#49613 = AXIS2_PLACEMENT_3D ( 'NONE', #12946, #44546, #30944 ) ;
#49614 = CARTESIAN_POINT ( 'NONE',  ( -9.621717088248901817, -61.42064477338403350, -8.060172376582604770 ) ) ;
#49615 = CARTESIAN_POINT ( 'NONE',  ( -7.080509631177999808, -76.88513832859899821, 6.324808343700000002 ) ) ;
#49616 = CARTESIAN_POINT ( 'NONE',  ( -10.34293954422016348, -77.00689439288741767, 6.233549652297469379 ) ) ;
#49617 = CARTESIAN_POINT ( 'NONE',  ( 5.976685521875192642, -76.61603491465773175, -11.25172029877191093 ) ) ;
#49618 = DIRECTION ( 'NONE',  ( -0.7071067811865474617, 0.000000000000000000, 0.7071067811865474617 ) ) ;
#49619 = EDGE_LOOP ( 'NONE', ( #47588, #43331, #10817 ) ) ;
#49620 = CARTESIAN_POINT ( 'NONE',  ( 0.6000739755967000599, -82.73745749870199973, 1.467756090344000119 ) ) ;
#49621 = CARTESIAN_POINT ( 'NONE',  ( -0.3439666625990999704, -80.41545669043000544, 1.306773950318999900 ) ) ;
#49622 = DIRECTION ( 'NONE',  ( -1.000000000000000000, 0.000000000000000000, 0.000000000000000000 ) ) ;
#49623 = CARTESIAN_POINT ( 'NONE',  ( -11.06076315227999984, -77.96694335400700027, 4.601693484369000053 ) ) ;
#49624 = CARTESIAN_POINT ( 'NONE',  ( -8.000000000000000000, -81.99999999999998579, 0.000000000000000000 ) ) ;
#49625 = DIRECTION ( 'NONE',  ( 0.8090169943750002979, 0.000000000000000000, -0.5877852522924001955 ) ) ;
#49626 = CARTESIAN_POINT ( 'NONE',  ( 7.048436826466999428, -77.87766471678199309, 6.223291978577000449 ) ) ;
#49627 = CARTESIAN_POINT ( 'NONE',  ( 4.498217319268383640, -76.04320575685785855, 10.85453619212339227 ) ) ;
#49628 = CARTESIAN_POINT ( 'NONE',  ( 6.585359383873000461, -79.70312102823399414, -8.706802385234000852 ) ) ;
#49629 = DIRECTION ( 'NONE',  ( -0.7071067811865475727, 0.000000000000000000, -0.7071067811865475727 ) ) ;
#49630 = ORIENTED_EDGE ( 'NONE', *, *, #52987, .T. ) ;
#49631 = ADVANCED_FACE ( 'NONE', ( #11725 ), #52899, .F. ) ;
#49632 = CARTESIAN_POINT ( 'NONE',  ( 0.000000000000000000, -74.64999999999999147, 0.000000000000000000 ) ) ;
#49633 = CARTESIAN_POINT ( 'NONE',  ( -2.038544480927684255, -78.67390000031812747, -3.380937442862520292 ) ) ;
#49634 = CARTESIAN_POINT ( 'NONE',  ( -8.596418555780466875, -77.44791666666667140, 6.606377239730298001 ) ) ;
#49635 = CARTESIAN_POINT ( 'NONE',  ( 0.2613587267741000475, -79.55704659509599708, -10.97249781033000104 ) ) ;
#49636 = DIRECTION ( 'NONE',  ( 0.7071067811865475727, 0.000000000000000000, 0.7071067811865475727 ) ) ;
#49637 = CARTESIAN_POINT ( 'NONE',  ( -2.533887857834999924, -76.98217140587999552, -12.24478563693999966 ) ) ;
#49638 = DIRECTION ( 'NONE',  ( -1.000000000000000000, 0.000000000000000000, 0.000000000000000000 ) ) ;
#49639 = CARTESIAN_POINT ( 'NONE',  ( -0.3862712429687000237, -78.00000000000000000, 1.188820645369000006 ) ) ;
#49640 = B_SPLINE_CURVE_WITH_KNOTS ( 'NONE', 3,
 ( #4645, #35618, #22646, #53644, #13185, #18230, #13775, #19977, #6384, #24098, #41525, #41818, #33233, #10533, #45683, #15241, #5223, #14356, #51278, #28515, #23802 ),
 .UNSPECIFIED., .F., .F.,
 ( 4, 2, 2, 2, 1, 2, 2, 2, 2, 2, 4 ),
 ( 0.000000000000000000, 0.1249999999999999167, 0.2499999999999998890, 0.3124999999999998335, 0.3749999999999998335, 0.4374999999999998890, 0.4999999999999998890, 0.6249999999999998890, 0.7499999999999998890, 0.8750000000000000000, 1.000000000000000000 ),
 .UNSPECIFIED. ) ;
#49641 = VERTEX_POINT ( 'NONE', #29703 ) ;
#49642 = CARTESIAN_POINT ( 'NONE',  ( -4.126717922116999837, -79.30368493481499570, -10.35494083817999922 ) ) ;
#49643 = CARTESIAN_POINT ( 'NONE',  ( 12.00000000000000000, -77.14999999999999147, 0.000000000000000000 ) ) ;
#49644 = CARTESIAN_POINT ( 'NONE',  ( 10.61050599188999932, -77.92876026662598576, -2.901234667509999809 ) ) ;
#49645 = CARTESIAN_POINT ( 'NONE',  ( 2.103056013418682646, -78.40681307385641219, 3.641429823450980763 ) ) ;
#49646 = CARTESIAN_POINT ( 'NONE',  ( -0.9860104425937412653, -81.54762977175269612, 0.7687338358433186691 ) ) ;
#49647 = CARTESIAN_POINT ( 'NONE',  ( -8.112440615085001028, -78.36632353800997919, -7.501079983178001065 ) ) ;
#49648 = CARTESIAN_POINT ( 'NONE',  ( 12.49999991316347270, -39.30476017083000073, 0.001473401919610936930 ) ) ;
#49649 = CYLINDRICAL_SURFACE ( 'NONE', #29902, 10.75000000000000000 ) ;
#49650 = VECTOR ( 'NONE', #11597, 1000.000000000000000 ) ;
#49651 = VECTOR ( 'NONE', #17292, 1000.000000000000000 ) ;
#49652 = CARTESIAN_POINT ( 'NONE',  ( -5.684557159767995138, -79.92708333333332860, 7.396918292183145560 ) ) ;
#49653 = AXIS2_PLACEMENT_3D ( 'NONE', #58157, #48730, #40145 ) ;
#49654 = DIRECTION ( 'NONE',  ( -0.9999999999995751176, 0.000000000000000000, -9.217554798440770948E-07 ) ) ;
#49655 = CARTESIAN_POINT ( 'NONE',  ( -12.54983138327999903, -25.05098386350000084, 0.1356331847737999863 ) ) ;
#49656 = VERTEX_POINT ( 'NONE', #56588 ) ;
#49657 = CIRCLE ( 'NONE', #45919, 0.8000000000000011546 ) ;
#49658 = VERTEX_POINT ( 'NONE', #7283 ) ;
#49659 = CARTESIAN_POINT ( 'NONE',  ( 9.500000000000001776, -78.63958333333336270, -1.243547092045940827 ) ) ;
#49660 = CARTESIAN_POINT ( 'NONE',  ( 5.722682530001000245, -76.87071332859899542, -7.358525362622999388 ) ) ;
#49661 = VECTOR ( 'NONE', #57481, 1000.000000000000114 ) ;
#49662 = ORIENTED_EDGE ( 'NONE', *, *, #19862, .T. ) ;
#49663 = CARTESIAN_POINT ( 'NONE',  ( -8.075725583014000009, -76.31079378115468614, -7.736700848914001227 ) ) ;
#49664 = EDGE_LOOP ( 'NONE', ( #29029, #3618, #54745, #35679, #37865 ) ) ;
#49665 = CARTESIAN_POINT ( 'NONE',  ( 7.619712170649999727, -23.40404510063000032, 10.35409959310000083 ) ) ;
#49666 = CARTESIAN_POINT ( 'NONE',  ( -11.03167625133000129, -77.64158425314199974, -0.06207630174703999970 ) ) ;
#49667 = DIRECTION ( 'NONE',  ( 0.000000000000000000, -1.000000000000000000, -1.853433557485999982E-14 ) ) ;
#49668 = CARTESIAN_POINT ( 'NONE',  ( -10.48774103546000092, -20.24527981753999839, 7.686941364807000632 ) ) ;
#49669 = CARTESIAN_POINT ( 'NONE',  ( -5.126676588143355140, -78.17827689695096183, -7.699309493463673881 ) ) ;
#49670 = CARTESIAN_POINT ( 'NONE',  ( -9.805641529082999241, -79.30645443996699839, -5.446788484474000214 ) ) ;
#49671 = CARTESIAN_POINT ( 'NONE',  ( 3.295987162183630748, -81.00000000000000000, 10.32795288958829616 ) ) ;
#49672 = VERTEX_POINT ( 'NONE', #16148 ) ;
#49673 = CARTESIAN_POINT ( 'NONE',  ( 11.44999999995999929, -74.99999999996168754, 1.667679908953999909E-09 ) ) ;
#49674 = ORIENTED_EDGE ( 'NONE', *, *, #17635, .T. ) ;
#49675 = CARTESIAN_POINT ( 'NONE',  ( 1.444433356061864737, -77.46253582747604582, 9.136518341544702437 ) ) ;
#49676 = CARTESIAN_POINT ( 'NONE',  ( 6.393001003723999709, -77.31630830916999741, 9.000752526674000720 ) ) ;
#49677 = DIRECTION ( 'NONE',  ( 0.7071067811865475727, 0.000000000000000000, 0.7071067811865475727 ) ) ;
#49678 = CARTESIAN_POINT ( 'NONE',  ( 2.260091721765999928, -79.03415970154399872, -9.437303113984999214 ) ) ;
#49679 = CARTESIAN_POINT ( 'NONE',  ( 6.925222504723999251, -76.67485380131999761, -11.14593178024999887 ) ) ;
#49680 = EDGE_CURVE ( 'NONE', #22393, #900, #8640, .T. ) ;
#49681 = CARTESIAN_POINT ( 'NONE',  ( -8.499390037608824500, -79.43684124743761288, -4.243882634569263068 ) ) ;
#49682 = CARTESIAN_POINT ( 'NONE',  ( -0.7213013439201000354, -77.85885253578000231, -1.458901041394999876 ) ) ;
#49683 = CARTESIAN_POINT ( 'NONE',  ( 0.000000000000000000, -23.25000000000000000, -12.50000000000000000 ) ) ;
#49684 = CARTESIAN_POINT ( 'NONE',  ( 10.52250585264000016, -78.65712618243998122, -2.994108701640999737 ) ) ;
#49685 = FACE_OUTER_BOUND ( 'NONE', #39991, .T. ) ;
#49686 = CARTESIAN_POINT ( 'NONE',  ( -11.33353239526517520, -76.67864579003945380, 3.106984491474204191 ) ) ;
#49687 = CARTESIAN_POINT ( 'NONE',  ( 1.939901737288000083, -82.63025363959900460, 2.966766385765999825 ) ) ;
#49688 = ORIENTED_EDGE ( 'NONE', *, *, #33087, .F. ) ;
#49689 = CARTESIAN_POINT ( 'NONE',  ( 2.837288914631000303, -79.51673028327599013, -12.10536388325999901 ) ) ;
#49690 = CARTESIAN_POINT ( 'NONE',  ( 9.595281647244998879, -75.85997436215698997, 4.747863145975999899 ) ) ;
#49691 = CARTESIAN_POINT ( 'NONE',  ( -6.826764225854004664, -78.02984463538199122, 8.304009225933823402 ) ) ;
#49692 = CARTESIAN_POINT ( 'NONE',  ( -8.557169117579000783, -77.76336928247899039, -8.383968101560000719 ) ) ;
#49693 = CARTESIAN_POINT ( 'NONE',  ( -10.30457855492000085, -18.23665569414000132, 7.636266481018999741 ) ) ;
#49694 = VECTOR ( 'NONE', #38849, 1000.000000000000114 ) ;
#49695 = CARTESIAN_POINT ( 'NONE',  ( 10.50000000000000000, -7.000000000000000000, 5.990617821004000856E-12 ) ) ;
#49696 = DIRECTION ( 'NONE',  ( -1.000000000000000000, 0.000000000000000000, 0.000000000000000000 ) ) ;
#49697 = CARTESIAN_POINT ( 'NONE',  ( 2.199922411859213778, -80.95883067551849877, 10.53541604723973180 ) ) ;
#49698 = CARTESIAN_POINT ( 'NONE',  ( 8.646554484075000602, -80.31431271246199799, -7.432130245983000094 ) ) ;
#49699 = CARTESIAN_POINT ( 'NONE',  ( 0.000000000000000000, -87.09999999999999432, -10.15000000000498659 ) ) ;
#49700 = CARTESIAN_POINT ( 'NONE',  ( 1.623230447552999944, -78.02776596815100163, -11.02813327291000078 ) ) ;
#49701 = DIRECTION ( 'NONE',  ( -1.000000000000000000, 0.000000000000000000, 0.000000000000000000 ) ) ;
#49702 = CARTESIAN_POINT ( 'NONE',  ( 0.6325562992502999915, -80.58843146505920174, -11.00758983218999987 ) ) ;
#49703 = VECTOR ( 'NONE', #20066, 1000.000000000000000 ) ;
#49704 = ORIENTED_EDGE ( 'NONE', *, *, #51363, .T. ) ;
#49705 = ADVANCED_FACE ( 'NONE', ( #34126 ), #35309, .F. ) ;
#49706 = CARTESIAN_POINT ( 'NONE',  ( 1.056237665594999875, -53.75133986268999564, 12.77256098193999989 ) ) ;
#49707 = FACE_BOUND ( 'NONE', #29099, .T. ) ;
#49708 = AXIS2_PLACEMENT_3D ( 'NONE', #21062, #47378, #20207 ) ;
#49709 = CARTESIAN_POINT ( 'NONE',  ( 0.3040822296088999677, -3.436728339067000260, -3.954576031983000117 ) ) ;
#49710 = CARTESIAN_POINT ( 'NONE',  ( -6.884807209879999057, -78.33851671174899423, -8.855368954042999619 ) ) ;
#49711 = CARTESIAN_POINT ( 'NONE',  ( -2.879226727952071574, -79.80416666666666003, -10.71369944335147473 ) ) ;
#49712 = AXIS2_PLACEMENT_3D ( 'NONE', #11080, #34057, #46518 ) ;
#49713 = CARTESIAN_POINT ( 'NONE',  ( 5.896171905175000560, -77.86999999999999034, 7.127247495676000355 ) ) ;
#49714 = DIRECTION ( 'NONE',  ( -1.000000000000000000, 0.000000000000000000, 0.000000000000000000 ) ) ;
#49715 = CARTESIAN_POINT ( 'NONE',  ( -5.769945183727626770, -78.58007713321237020, -9.108383413252392202 ) ) ;
#49716 = CARTESIAN_POINT ( 'NONE',  ( 12.77568125278999922, -16.73490786122999907, 0.5296379231475000227 ) ) ;
#49717 = CARTESIAN_POINT ( 'NONE',  ( -3.935749424346000058, -86.36232450217399048, 0.4303395207149999790 ) ) ;
#49718 = DIRECTION ( 'NONE',  ( 0.000000000000000000, -1.000000000000000000, 0.000000000000000000 ) ) ;
#49719 = EDGE_CURVE ( 'NONE', #54081, #28385, #14194, .T. ) ;
#49721 = ADVANCED_FACE ( 'NONE', ( #18476 ), #36183, .F. ) ;
#49720 = CARTESIAN_POINT ( 'NONE',  ( 9.636775127257999785, -54.35967715709000458, -7.948072248856999700 ) ) ;
#49722 = CARTESIAN_POINT ( 'NONE',  ( -11.05562587724999979, -77.21905714352298844, -1.423986317748999975 ) ) ;
#49723 = CARTESIAN_POINT ( 'NONE',  ( -1.497546582071999977, -80.73430643132999762, 0.7298035716741000378 ) ) ;
#49724 = CARTESIAN_POINT ( 'NONE',  ( 0.4117780953839000335, -79.03975217913999529, -1.493365003632999954 ) ) ;
#49725 = CARTESIAN_POINT ( 'NONE',  ( 9.208615812369000508, -77.10488338023777999, 2.957800710608999850 ) ) ;
#49726 = CARTESIAN_POINT ( 'NONE',  ( -17.49999986748943925, -49.87071424677999687, -0.002153571276212541078 ) ) ;
#49727 = CARTESIAN_POINT ( 'NONE',  ( -12.78015149461000100, -61.10330660662999946, 1.806228889759999845 ) ) ;
#49728 = CARTESIAN_POINT ( 'NONE',  ( -10.44304457033000055, -78.32510815631960099, 3.377400876517000050 ) ) ;
#49729 = CARTESIAN_POINT ( 'NONE',  ( 10.74987430283537471, -79.85617428146984764, 0.8320502212467579817 ) ) ;
#49730 = CARTESIAN_POINT ( 'NONE',  ( 1.200757745776334318, -77.87262074594069361, -0.4270230002123092117 ) ) ;
#49731 = ORIENTED_EDGE ( 'NONE', *, *, #37001, .F. ) ;
#49732 = CARTESIAN_POINT ( 'NONE',  ( 9.431004454403453252, -53.99940410528930101, 8.251853356943772866 ) ) ;
#49733 = CARTESIAN_POINT ( 'NONE',  ( 6.365665562422999635, -79.13050366622999832, 10.17242851768000023 ) ) ;
#49734 = CARTESIAN_POINT ( 'NONE',  ( 3.609690327934000020, -80.23949669345269342, 10.39335624559999971 ) ) ;
#49735 = CARTESIAN_POINT ( 'NONE',  ( 3.250000000000000000, -1.850000000000000089, 0.000000000000000000 ) ) ;
#49736 = ORIENTED_EDGE ( 'NONE', *, *, #46462, .T. ) ;
#49737 = ORIENTED_EDGE ( 'NONE', *, *, #46673, .F. ) ;
#49738 = B_SPLINE_CURVE_WITH_KNOTS ( 'NONE', 3,
 ( #48317, #6990, #21434, #39442, #34991, #47468, #20573, #52168, #47748, #30570, #48603, #43301, #26149, #57732, #53603, #27313, #44749, #493 ),
 .UNSPECIFIED., .F., .F.,
 ( 4, 2, 2, 2, 2, 2, 2, 2, 4 ),
 ( 0.000000000000000000, 0.1250000000000000000, 0.2499999999999999445, 0.3750000000000000000, 0.5000000000000000000, 0.6250000000000000000, 0.7500000000000000000, 0.8750000000000000000, 1.000000000000000000 ),
 .UNSPECIFIED. ) ;
#49739 = CARTESIAN_POINT ( 'NONE',  ( -10.24999999991999999, -82.10000000007899246, 6.817355505960000646E-10 ) ) ;
#49740 = VERTEX_POINT ( 'NONE', #22896 ) ;
#49741 = CARTESIAN_POINT ( 'NONE',  ( 9.837773999883454579, -54.48535604146630362, -7.850041801328902835 ) ) ;
#49742 = CIRCLE ( 'NONE', #2620, 10.20000000000000107 ) ;
#49743 = ORIENTED_EDGE ( 'NONE', *, *, #14112, .F. ) ;
#49744 = CARTESIAN_POINT ( 'NONE',  ( 1.122609662881488113, -80.38645885631675014, 0.5495315797171209660 ) ) ;
#49745 = CARTESIAN_POINT ( 'NONE',  ( -9.914363537814757876, -79.81715790035769942, 4.347490629219784353 ) ) ;
#49746 = CARTESIAN_POINT ( 'NONE',  ( -4.000000000000000000, -5.200000000000000178, -0.5999999999999999778 ) ) ;
#49747 = CARTESIAN_POINT ( 'NONE',  ( -0.5390150933986999071, -25.26260891652000140, -12.77520261005000002 ) ) ;
#49748 = CARTESIAN_POINT ( 'NONE',  ( -1.036641179982999983, -81.69646188631999451, 3.610643376931000237 ) ) ;
#49749 = CARTESIAN_POINT ( 'NONE',  ( -7.699832853999788895, -79.34979350599515158, 5.563995025944507233 ) ) ;
#49750 = CARTESIAN_POINT ( 'NONE',  ( 11.44999999999999929, -75.00000000000000000, 0.000000000000000000 ) ) ;
#49751 = CARTESIAN_POINT ( 'NONE',  ( -11.36395519648000096, -78.80425755395999943, 4.043272157487999507 ) ) ;
#49752 = CIRCLE ( 'NONE', #24284, 0.6000000000000008660 ) ;
#49753 = ORIENTED_EDGE ( 'NONE', *, *, #20905, .T. ) ;
#49754 = ORIENTED_EDGE ( 'NONE', *, *, #58236, .T. ) ;
#49755 = CARTESIAN_POINT ( 'NONE',  ( -10.12290050255000118, -55.55000002206000431, -7.648026768392999664 ) ) ;
#49756 = DIRECTION ( 'NONE',  ( 0.000000000000000000, -1.000000000000000000, 0.000000000000000000 ) ) ;
#49757 = AXIS2_PLACEMENT_3D ( 'NONE', #50524, #51113, #948 ) ;
#49758 = CARTESIAN_POINT ( 'NONE',  ( -0.5470841013496000604, -79.81324990208399583, -1.216254552179000026 ) ) ;
#49759 = CARTESIAN_POINT ( 'NONE',  ( 1.487026788147999934, -77.34678798069599281, -9.589549613196998834 ) ) ;
#49760 = CIRCLE ( 'NONE', #21458, 1.250000000000000000 ) ;
#49761 = CYLINDRICAL_SURFACE ( 'NONE', #55846, 1.750000000000000000 ) ;
#49762 = CARTESIAN_POINT ( 'NONE',  ( 1.826169837773488069, -85.89642030789714511, 2.963197235734413848 ) ) ;
#49763 = CARTESIAN_POINT ( 'NONE',  ( 7.289493654314999738, -77.00467974817999561, -10.52009694070999934 ) ) ;
#49764 = CARTESIAN_POINT ( 'NONE',  ( 5.486311112560000147, -77.58365458999999476, 11.38883617360999878 ) ) ;
#49765 = CARTESIAN_POINT ( 'NONE',  ( -1.408793263084000102, -76.34408402689498985, 10.90858184500000050 ) ) ;
#49766 = CARTESIAN_POINT ( 'NONE',  ( 2.854661674668000058E-14, -82.00000000000000000, 0.000000000000000000 ) ) ;
#49767 = CARTESIAN_POINT ( 'NONE',  ( -1.507728061743999870, -78.97418298445228402, -3.890598935239999889 ) ) ;
#49768 = CARTESIAN_POINT ( 'NONE',  ( 10.70339364929999881, -81.03462737628719026, 2.537196166659999808 ) ) ;
#49769 = CARTESIAN_POINT ( 'NONE',  ( -10.59548767697000038, -58.55736537918999574, 7.678667886039000301 ) ) ;
#49770 = CARTESIAN_POINT ( 'NONE',  ( 11.90625000002000000, -76.20625000001498961, 3.701036097655999965E-09 ) ) ;
#49771 = CARTESIAN_POINT ( 'NONE',  ( -1.309352690804000074, -78.28086903840210198, -0.2533212985548999874 ) ) ;
#49772 = LINE ( 'NONE', #49170, #18513 ) ;
#49773 = CARTESIAN_POINT ( 'NONE',  ( -11.09105850093000001, -80.38766464674519341, 1.974238845993000258 ) ) ;
#49774 = CARTESIAN_POINT ( 'NONE',  ( -3.399186938124999724, -77.19999999999998863, -10.46162167925000119 ) ) ;
#49775 = EDGE_LOOP ( 'NONE', ( #43040, #41004, #4870, #55608 ) ) ;
#49776 = CARTESIAN_POINT ( 'NONE',  ( 11.00000000000000711, -78.43958333333333144, -1.439896632895300010 ) ) ;
#49777 = ADVANCED_FACE ( 'NONE', ( #498 ), #14031, .F. ) ;
#49778 = CARTESIAN_POINT ( 'NONE',  ( 11.75000000000000000, -78.45000000000000284, 0.000000000000000000 ) ) ;
#49779 = CARTESIAN_POINT ( 'NONE',  ( 0.6791306551168999617, -81.43317880092300243, -1.147762040996999966 ) ) ;
#49780 = CARTESIAN_POINT ( 'NONE',  ( -8.739412744344001283, -79.79261095533199466, 4.325800834547999685 ) ) ;
#49781 = CARTESIAN_POINT ( 'NONE',  ( -8.048032176077001054, -78.44865870152001719, 9.328081102756000220 ) ) ;
#49782 = CARTESIAN_POINT ( 'NONE',  ( -3.637215472919097969, -79.50258317002523256, 10.11602608574209761 ) ) ;
#49783 = CARTESIAN_POINT ( 'NONE',  ( 2.759513673833999814, -79.21986001420199841, -8.792710209907999896 ) ) ;
#49784 = CARTESIAN_POINT ( 'NONE',  ( 12.60552511010000032, -18.71082276572999703, -1.799501877793999949 ) ) ;
#49785 = EDGE_LOOP ( 'NONE', ( #3042, #6678, #29951, #47078 ) ) ;
#49786 = CARTESIAN_POINT ( 'NONE',  ( 0.000000000000000000, -55.54999999966999980, 12.00000000000000000 ) ) ;
#49787 = DIRECTION ( 'NONE',  ( 0.000000000000000000, -1.000000000000000000, 0.000000000000000000 ) ) ;
#49788 = ADVANCED_FACE ( 'NONE', ( #42000 ), #1568, .F. ) ;
#49789 = AXIS2_PLACEMENT_3D ( 'NONE', #15663, #12388, #38672 ) ;
#49790 = CARTESIAN_POINT ( 'NONE',  ( -1.393363954175000030, -81.80898018020499762, -0.2057425908966999950 ) ) ;
#49791 = DIRECTION ( 'NONE',  ( -1.776356839400000238E-14, -1.000000000000000000, -4.588921835116999839E-14 ) ) ;
#49792 = CARTESIAN_POINT ( 'NONE',  ( -1.518219907972000016, -78.90870446205198618, 9.290113175764000530 ) ) ;
#49794 = CARTESIAN_POINT ( 'NONE',  ( -0.4617212151683000032, -1.166835600325000000, 3.989551193614000013 ) ) ;
#49793 = CARTESIAN_POINT ( 'NONE',  ( -2.639441014136000074, -84.30218271708000088, 3.176769522894000275 ) ) ;
#49795 = CARTESIAN_POINT ( 'NONE',  ( -2.062673488738000049, -55.47547470607999998, -12.82904091336000008 ) ) ;
#49796 = CARTESIAN_POINT ( 'NONE',  ( 0.5117640625906000329, -79.50135730798099587, 1.216002981391000048 ) ) ;
#49797 = EDGE_LOOP ( 'NONE', ( #22914, #46257, #29917, #29452 ) ) ;
#49798 = CARTESIAN_POINT ( 'NONE',  ( 0.002952034968893703631, -77.22510189820128801, -10.74995197471566222 ) ) ;
#49799 = CARTESIAN_POINT ( 'NONE',  ( -1.471932811527529195, -79.41769483858601575, -0.3335056313496183034 ) ) ;
#49800 = AXIS2_PLACEMENT_3D ( 'NONE', #17790, #49381, #43794 ) ;
#49801 = ORIENTED_EDGE ( 'NONE', *, *, #20391, .T. ) ;
#49802 = ORIENTED_EDGE ( 'NONE', *, *, #30681, .F. ) ;
#49803 = CARTESIAN_POINT ( 'NONE',  ( 3.552363299575000077, -79.85053823319960031, -11.49294985030999960 ) ) ;
#49804 = CARTESIAN_POINT ( 'NONE',  ( -1.342463812738999916E-14, -80.79999999999999716, -13.90000000000000036 ) ) ;
#49805 = ORIENTED_EDGE ( 'NONE', *, *, #29182, .F. ) ;
#49806 = CARTESIAN_POINT ( 'NONE',  ( -6.817533650000999756, -78.26827991340999802, -9.935643240620999350 ) ) ;
#49807 = EDGE_CURVE ( 'NONE', #47711, #3338, #21584, .T. ) ;
#49808 = VERTEX_POINT ( 'NONE', #39014 ) ;
#49809 = VERTEX_POINT ( 'NONE', #39589 ) ;
#49810 = CARTESIAN_POINT ( 'NONE',  ( 0.8446295986270583311, -2.746170833900309027, -3.145970808612796876 ) ) ;
#49811 = DIRECTION ( 'NONE',  ( 0.7071067811864970576, 3.544461081833985722E-08, -0.7071067811865970887 ) ) ;
#49812 = CARTESIAN_POINT ( 'NONE',  ( 8.500000000000000000, -3.500000000000000000, 0.000000000000000000 ) ) ;
#49813 = B_SPLINE_SURFACE_WITH_KNOTS ( 'NONE', 3, 3, ( 
 ( #44852, #12671, #3529, #54304 ),
 ( #18289, #31240, #40718, #35682 ),
 ( #310, #25954, #4706, #17102 ),
 ( #40116, #4105, #22106, #30662 ),
 ( #8532, #26525, #4404, #21531 ),
 ( #39536, #57542, #44552, #49586 ),
 ( #36281, #17691, #44261, #48987 ),
 ( #30376, #48416, #53711, #13247 ),
 ( #35088, #49281, #35377, #57835 ),
 ( #7952, #17391, #22406, #12950 ),
 ( #30948, #8833, #26822, #3815 ),
 ( #8243, #26245, #53122, #22704 ),
 ( #9133, #21818, #40418, #12 ),
 ( #39819, #17991, #54007, #13548 ),
 ( #31540, #27117, #45157, #28283 ),
 ( #600, #37151, #9714, #19450 ),
 ( #5859, #45450, #18582, #41591 ) ),
 .UNSPECIFIED., .F., .F., .F.,
 ( 4, 1, 1, 1, 1, 1, 1, 1, 1, 1, 1, 1, 1, 1, 4 ),
 ( 4, 4 ),
 ( -0.01011837001259000002, 0.000000000000000000, 0.08333333333333001192, 0.1666666666667000196, 0.2500000000000000000, 0.3333333333333000081, 0.4166666666666999919, 0.5000000000000000000, 0.5833333333333000637, 0.6666666666667000474, 0.7500000000000000000, 0.8333333333333000637, 0.9166666666667000474, 1.000000000000000000, 1.010372850415000023 ),
 ( -0.3559705548695000221, 1.357613361088000126 ),
 .UNSPECIFIED. ) ;
#49814 = VERTEX_POINT ( 'NONE', #56452 ) ;
#49815 = CARTESIAN_POINT ( 'NONE',  ( 0.8873640354812792896, -82.78847969525013184, -0.8798066330654785716 ) ) ;
#49816 = ORIENTED_EDGE ( 'NONE', *, *, #46109, .F. ) ;
#49817 = CARTESIAN_POINT ( 'NONE',  ( 1.041288859402153877, -80.44866080611242865, 0.7340484819354226032 ) ) ;
#49818 = CARTESIAN_POINT ( 'NONE',  ( -11.76761288928574345, -79.80000000000001137, -2.220697818543512003 ) ) ;
#49819 = EDGE_CURVE ( 'NONE', #30968, #39067, #37500, .T. ) ;
#49820 = DIRECTION ( 'NONE',  ( -0.7071067811704841999, -1.939413340559955448E-07, 0.7071067812025843002 ) ) ;
#49821 = TOROIDAL_SURFACE ( 'NONE', #11185, 1.250000000000000000, 0.5000000000000000000 ) ;
#49822 = CARTESIAN_POINT ( 'NONE',  ( -0.5847500590559130407, -18.69344856180045156, 10.98448857562230252 ) ) ;
#49823 = CARTESIAN_POINT ( 'NONE',  ( -1.538071403320043551, -77.18541666666666856, 11.74999999999999467 ) ) ;
#49824 = CARTESIAN_POINT ( 'NONE',  ( 10.05000000000000071, -87.20000000000000284, 0.000000000000000000 ) ) ;
#49825 = CARTESIAN_POINT ( 'NONE',  ( 11.79843486695000188, -77.38613504417455147, -2.076781258317999868 ) ) ;
#49826 = CARTESIAN_POINT ( 'NONE',  ( 8.209582066784916421, -78.81200429033071941, -4.264407347131307091 ) ) ;
#49827 = CARTESIAN_POINT ( 'NONE',  ( -12.65372179303999900, -21.75064713777999970, -1.750000000000000000 ) ) ;
#49828 = CARTESIAN_POINT ( 'NONE',  ( -10.30767511322000018, -23.74763733895999707, 7.634418707049000830 ) ) ;
#49829 = CARTESIAN_POINT ( 'NONE',  ( -1.210856240595359790, -77.71471340245162196, -9.250524551649785820 ) ) ;
#49830 = CARTESIAN_POINT ( 'NONE',  ( -11.75000000000000000, -76.79999999999999716, -1.435311119447000145E-14 ) ) ;
#49831 = CARTESIAN_POINT ( 'NONE',  ( 1.940281527255000027, -79.51992549782627862, 3.646067899498000031 ) ) ;
#49832 = DIRECTION ( 'NONE',  ( 0.000000000000000000, 0.000000000000000000, -1.000000000000000000 ) ) ;
#49833 = CARTESIAN_POINT ( 'NONE',  ( 5.445437576845045591, -76.26093750000428884, 10.69085136092807709 ) ) ;
#49834 = AXIS2_PLACEMENT_3D ( 'NONE', #5087, #27792, #50842 ) ;
#49835 = CARTESIAN_POINT ( 'NONE',  ( -2.935661446561999899, -77.00000000000000000, -9.035036904803998681 ) ) ;
#49836 = CARTESIAN_POINT ( 'NONE',  ( 1.629367637659999923, -23.68263643397999729, 12.46114270826000059 ) ) ;
#49837 = DIRECTION ( 'NONE',  ( -1.000000000000000000, 0.000000000000000000, 0.000000000000000000 ) ) ;
#49838 = CARTESIAN_POINT ( 'NONE',  ( -3.262415774573999894, -2.066798252606000474, -0.4905674017874000481 ) ) ;
#49839 = ADVANCED_FACE ( 'NONE', ( #16007 ), #29565, .F. ) ;
#49840 = CARTESIAN_POINT ( 'NONE',  ( 7.651147547619999933, -59.56256650291999222, 10.45204383579000051 ) ) ;
#49841 = DIRECTION ( 'NONE',  ( 0.000000000000000000, -1.000000000000000000, 0.000000000000000000 ) ) ;
#49843 = EDGE_CURVE ( 'NONE', #22190, #6045, #32140, .T. ) ;
#49842 = CARTESIAN_POINT ( 'NONE',  ( 1.491372860315189230, -81.11249091029543479, 0.2478840690545696945 ) ) ;
#49844 = CARTESIAN_POINT ( 'NONE',  ( -0.3473130761334148331, -78.49761955947900560, 1.203549973938182527 ) ) ;
#49845 = CARTESIAN_POINT ( 'NONE',  ( 0.000000000000000000, -45.91785611817000046, 0.000000000000000000 ) ) ;
#49846 = CARTESIAN_POINT ( 'NONE',  ( 9.546815223802999739, -54.11472046612000497, 8.130854305859999798 ) ) ;
#49847 = PRODUCT ( 'Push Button', 'Push Button', '', ( #42916 ) ) ;
#49848 = B_SPLINE_CURVE_WITH_KNOTS ( 'NONE', 3,
 ( #36050, #3882, #35155, #45515, #31309, #9488, #22474, #31901, #26893, #4767, #49943, #17170, #54367, #40485, #30732, #22768, #40185, #49352 ),
 .UNSPECIFIED., .F., .F.,
 ( 4, 2, 2, 2, 2, 2, 2, 2, 4 ),
 ( 0.000000000000000000, 0.1250000000000000000, 0.2500000000000000000, 0.3750000000000000000, 0.5000000000000000000, 0.6250000000000000000, 0.7500000000000000000, 0.8750000000000000000, 1.000000000000000000 ),
 .UNSPECIFIED. ) ;
#49849 = CARTESIAN_POINT ( 'NONE',  ( 10.42062934545543840, -77.22079869211786729, 2.728807196244066535 ) ) ;
#49850 = CARTESIAN_POINT ( 'NONE',  ( 2.600000000000000089, -77.49999999999998579, 0.000000000000000000 ) ) ;
#49852 = CARTESIAN_POINT ( 'NONE',  ( -1.391953914337000109, -78.31252216817028966, -0.2693022098514999962 ) ) ;
#49851 = CARTESIAN_POINT ( 'NONE',  ( 0.3926218265389159745, -79.75416666666667709, 1.460959015002474493 ) ) ;
#49853 = CARTESIAN_POINT ( 'NONE',  ( 0.4046438523804999909, -81.41406578915000125, -1.654233492563000008 ) ) ;
#49854 = ORIENTED_EDGE ( 'NONE', *, *, #55651, .F. ) ;
#49855 = CARTESIAN_POINT ( 'NONE',  ( -1.575735042988000156, -86.12182450217399321, 3.225051518789999960 ) ) ;
#49856 = CARTESIAN_POINT ( 'NONE',  ( 4.976417922892999890, -78.96415677378300302, 10.83839387946000166 ) ) ;
#49857 = CARTESIAN_POINT ( 'NONE',  ( -11.05289869489000054, -80.57525882426229202, -0.2569212408223999766 ) ) ;
#49858 = EDGE_CURVE ( 'NONE', #41874, #11038, #39692, .T. ) ;
#49859 = LINE ( 'NONE', #44526, #23811 ) ;
#49860 = CARTESIAN_POINT ( 'NONE',  ( 1.500000000000000000, -81.75000000000000000, 0.000000000000000000 ) ) ;
#49861 = CARTESIAN_POINT ( 'NONE',  ( 6.201912463541000342, -78.57396040930800041, -9.171216270948999494 ) ) ;
#49862 = DIRECTION ( 'NONE',  ( 1.205798305761979436E-11, -1.868137355152963707E-07, 0.9999999999999824585 ) ) ;
#49863 = FACE_BOUND ( 'NONE', #31260, .T. ) ;
#49864 = LINE ( 'NONE', #45731, #48709 ) ;
#49865 = CARTESIAN_POINT ( 'NONE',  ( 6.732849078471510929, -76.47319592210000394, -9.714227559369218667 ) ) ;
#49866 = CARTESIAN_POINT ( 'NONE',  ( -8.583677311523363329, -61.77185920727036716, 9.102132575252269930 ) ) ;
#49867 = DIRECTION ( 'NONE',  ( 0.000000000000000000, -1.000000000000000000, 0.000000000000000000 ) ) ;
#49868 = ORIENTED_EDGE ( 'NONE', *, *, #54939, .T. ) ;
#49869 = CARTESIAN_POINT ( 'NONE',  ( -1.980584515752000119, -55.53514853344000102, -12.76303204600000107 ) ) ;
#49870 = CARTESIAN_POINT ( 'NONE',  ( -5.025355631522999467, -79.70953998579798849, -7.962943362895000377 ) ) ;
#49871 = AXIS2_PLACEMENT_3D ( 'NONE', #54899, #36599, #54623 ) ;
#49872 = CARTESIAN_POINT ( 'NONE',  ( -1.842306058376209643, -75.81200536713309646, -11.64247462211659290 ) ) ;
#49873 = CARTESIAN_POINT ( 'NONE',  ( 14.00000000000000000, -9.295797029142999435, 0.000000000000000000 ) ) ;
#49874 = CARTESIAN_POINT ( 'NONE',  ( -12.69616050744000013, -58.55171076491000548, -1.799475304559999822 ) ) ;
#49875 = CARTESIAN_POINT ( 'NONE',  ( 10.99608688423679403, -23.68532521788496581, 0.3139246511496328607 ) ) ;
#49876 = EDGE_LOOP ( 'NONE', ( #36063, #39539, #28720, #12036, #44060 ) ) ;
#49877 = CARTESIAN_POINT ( 'NONE',  ( 6.923622142245000610, -78.17102818423599331, -8.818797536904998680 ) ) ;
#49878 = CARTESIAN_POINT ( 'NONE',  ( 10.04567131166087179, -61.35088387338642946, -7.921299640537584175 ) ) ;
#49879 = ORIENTED_EDGE ( 'NONE', *, *, #48934, .T. ) ;
#49880 = ORIENTED_EDGE ( 'NONE', *, *, #981, .F. ) ;
#49881 = CONICAL_SURFACE ( 'NONE', #51782, 4.899999999795999983, 0.7853981633972997312 ) ;
#49882 = CYLINDRICAL_SURFACE ( 'NONE', #21699, 1.750000000000001332 ) ;
#49883 = CARTESIAN_POINT ( 'NONE',  ( 1.739862777674999972, -79.13059728025397987, 9.611119481339999382 ) ) ;
#49884 = ORIENTED_EDGE ( 'NONE', *, *, #37066, .F. ) ;
#49885 = CARTESIAN_POINT ( 'NONE',  ( -12.24569868602999989, -76.68065739571800066, 1.621947466804000149 ) ) ;
#49886 = DIRECTION ( 'NONE',  ( -0.9999999924279686647, 0.000000000000000000, -0.0001230612157847738313 ) ) ;
#49887 = CARTESIAN_POINT ( 'NONE',  ( 1.645994068133999955, -78.52418299843999705, 0.08711949123553000551 ) ) ;
#49888 = ORIENTED_EDGE ( 'NONE', *, *, #20004, .F. ) ;
#49889 = CARTESIAN_POINT ( 'NONE',  ( -6.013262726775999489, -77.49952305011500187, 7.348341287529000176 ) ) ;
#49890 = EDGE_CURVE ( 'NONE', #21051, #28446, #14237, .T. ) ;
#49891 = CARTESIAN_POINT ( 'NONE',  ( 1.131496422793114576, -80.31479908467704831, -0.5381041634472353286 ) ) ;
#49892 = CARTESIAN_POINT ( 'NONE',  ( -1.273906987915999878, -77.61163602614999490, -13.05154622979999957 ) ) ;
#49893 = CARTESIAN_POINT ( 'NONE',  ( 12.00000000000000000, -79.04999999999999716, 0.000000000000000000 ) ) ;
#49894 = CARTESIAN_POINT ( 'NONE',  ( 4.186942200393000135, -78.41050069316224835, -8.754440266352000677 ) ) ;
#49895 = CARTESIAN_POINT ( 'NONE',  ( 8.197317322123611305, -79.88882380982184372, 4.285112605895506022 ) ) ;
#49896 = CARTESIAN_POINT ( 'NONE',  ( -1.668607604570423009, -23.79381631241137995, 12.52787843850897964 ) ) ;
#49897 = VERTEX_POINT ( 'NONE', #43173 ) ;
#49898 = DIRECTION ( 'NONE',  ( 1.000000000000000000, 0.000000000000000000, 0.000000000000000000 ) ) ;
#49899 = CARTESIAN_POINT ( 'NONE',  ( 1.328206530128999807, -76.68560288576000517, -12.23810562210000086 ) ) ;
#49900 = CARTESIAN_POINT ( 'NONE',  ( -1.347695613438000040, -80.39056234758800201, -0.6947364142266000409 ) ) ;
#49901 = CARTESIAN_POINT ( 'NONE',  ( 0.2696047275149000555, -79.01668014110398985, 1.291465103089999955 ) ) ;
#49902 = CARTESIAN_POINT ( 'NONE',  ( 0.6527094116100424781, -3.209387129096291424, 3.460698173749425344 ) ) ;
#49903 = AXIS2_PLACEMENT_3D ( 'NONE', #21251, #43131, #21541 ) ;
#49904 = CARTESIAN_POINT ( 'NONE',  ( 13.86363636363000218, -46.43897132165000130, 1.277887489249999988E-05 ) ) ;
#49905 = CARTESIAN_POINT ( 'NONE',  ( 7.081057523560999378, -79.22598300536000693, -10.01287680343000019 ) ) ;
#49906 = CARTESIAN_POINT ( 'NONE',  ( -8.598496321198998871, -77.26496209410798599, -8.768570137950998600 ) ) ;
#49907 = CARTESIAN_POINT ( 'NONE',  ( 12.71758670598766017, -17.93493368773965813, -1.809547514117120448 ) ) ;
#49908 = CARTESIAN_POINT ( 'NONE',  ( 2.191831765174000246, -77.29983832859899451, 9.375831637944999741 ) ) ;
#49909 = CARTESIAN_POINT ( 'NONE',  ( 6.160028937834207241, -76.88236474970555889, 10.38583856661684379 ) ) ;
#49910 = CARTESIAN_POINT ( 'NONE',  ( -3.009867212368674494, -75.84684136573420687, 12.37993388414874119 ) ) ;
#49911 = ORIENTED_EDGE ( 'NONE', *, *, #3630, .F. ) ;
#49913 = EDGE_CURVE ( 'NONE', #13828, #31238, #39648, .T. ) ;
#49912 = CARTESIAN_POINT ( 'NONE',  ( -1.329983713389000011, -82.42181889680900042, 0.6225684403671000178 ) ) ;
#49914 = CARTESIAN_POINT ( 'NONE',  ( -10.42531124905999995, -18.73514851523999880, 7.624341765453999997 ) ) ;
#49915 = CARTESIAN_POINT ( 'NONE',  ( 9.164385193226218362, -25.21567483134532139, 8.803702036953628962 ) ) ;
#49916 = AXIS2_PLACEMENT_3D ( 'NONE', #40913, #23193, #13740 ) ;
#49917 = DIRECTION ( 'NONE',  ( -0.07798810159164812350, -0.04890177460086881506, -0.9957542229139761947 ) ) ;
#49918 = CARTESIAN_POINT ( 'NONE',  ( 9.267587667790845529, -76.99999999999998579, 1.705438069304222370 ) ) ;
#49919 = CIRCLE ( 'NONE', #47115, 9.500000000000000000 ) ;
#49920 = CARTESIAN_POINT ( 'NONE',  ( -11.81636186152999990, -78.58780308901600620, -1.676035442350999993 ) ) ;
#49921 = CARTESIAN_POINT ( 'NONE',  ( 8.219513559211000242, -78.86479805011499877, 5.194554602171000290 ) ) ;
#49922 = CARTESIAN_POINT ( 'NONE',  ( 9.440269692223999698, -77.94108065130299678, -1.906441214165000009 ) ) ;
#49923 = CARTESIAN_POINT ( 'NONE',  ( 2.392485446417093264, -76.05844639573089694, 11.50375119131274992 ) ) ;
#49924 = CARTESIAN_POINT ( 'NONE',  ( -10.42930648941000094, -80.00272080125370167, 3.225667704544000092 ) ) ;
#49925 = CARTESIAN_POINT ( 'NONE',  ( 3.140027144888980271, -85.94828564506399005, -1.398030157552043740 ) ) ;
#49926 = EDGE_LOOP ( 'NONE', ( #10585, #5787, #18049 ) ) ;
#49927 = CARTESIAN_POINT ( 'NONE',  ( -6.282410744257000523, -75.96762204925410344, 10.58616248715999930 ) ) ;
#49928 = CARTESIAN_POINT ( 'NONE',  ( -3.740501297249256396, -78.39678895079168797, -2.113513782812399544 ) ) ;
#49929 = EDGE_CURVE ( 'NONE', #3043, #16917, #40326, .T. ) ;
#49930 = CARTESIAN_POINT ( 'NONE',  ( 0.2613587267741000475, -79.61734952076598404, -10.97249781033000104 ) ) ;
#49931 = ADVANCED_FACE ( 'NONE', ( #34856 ), #50092, .F. ) ;
#49932 = FACE_OUTER_BOUND ( 'NONE', #56560, .T. ) ;
#49933 = CARTESIAN_POINT ( 'NONE',  ( -10.99980394231345926, -80.10023817985064909, 1.711188753626703361E-06 ) ) ;
#49934 = CARTESIAN_POINT ( 'NONE',  ( 1.250000000000000000, -79.34999999999999432, 0.000000000000000000 ) ) ;
#49935 = CARTESIAN_POINT ( 'NONE',  ( -0.5999999998848000171, -23.14999999478999726, -11.79999999988000070 ) ) ;
#49936 = ORIENTED_EDGE ( 'NONE', *, *, #356, .T. ) ;
#49937 = CARTESIAN_POINT ( 'NONE',  ( 1.104250457816000175, -79.64377542924600561, 11.20779173096999948 ) ) ;
#49938 = CARTESIAN_POINT ( 'NONE',  ( -8.571485855526580266, -77.46864983315596476, 3.552044476763973613 ) ) ;
#49939 = CARTESIAN_POINT ( 'NONE',  ( -6.606377239730371720, -79.92708333333332860, 8.596418555780411808 ) ) ;
#49940 = CARTESIAN_POINT ( 'NONE',  ( 3.778552491321000240, -78.40681307243319509, -4.627392213906519702E-16 ) ) ;
#49941 = CARTESIAN_POINT ( 'NONE',  ( -0.4845542736245379567, -81.50687699870314873, 1.152130999872969852 ) ) ;
#49942 = CARTESIAN_POINT ( 'NONE',  ( -10.86532694299999946, -79.32146358532099839, -2.005633084294999868 ) ) ;
#49943 = CARTESIAN_POINT ( 'NONE',  ( -1.125737367536218558, -76.38333333333332575, 10.75000000000001066 ) ) ;
#49944 = CARTESIAN_POINT ( 'NONE',  ( -0.8385792221450999451, -2.855321851618000117, -3.712528424878000166 ) ) ;
#49946 = EDGE_CURVE ( 'NONE', #39734, #44850, #2438, .T. ) ;
#49945 = VECTOR ( 'NONE', #10126, 999.9999999999998863 ) ;
#49947 = CARTESIAN_POINT ( 'NONE',  ( -12.52582254643367499, -54.99059700767246284, -1.680974932891768914 ) ) ;
#49948 = CARTESIAN_POINT ( 'NONE',  ( 6.606377239730313988, -78.32291666666665719, 8.596418555780454440 ) ) ;
#49949 = SURFACE_STYLE_USAGE ( .BOTH. , #45520 ) ;
#49950 = CARTESIAN_POINT ( 'NONE',  ( -12.77568181202000019, -25.26511628633999962, 0.5294980821347999855 ) ) ;
#49951 = ORIENTED_EDGE ( 'NONE', *, *, #45098, .F. ) ;
#49952 = ORIENTED_EDGE ( 'NONE', *, *, #55708, .T. ) ;
#49953 = CARTESIAN_POINT ( 'NONE',  ( 10.56375213976313532, -78.83523569680077969, -1.992565471537876887 ) ) ;
#49954 = CARTESIAN_POINT ( 'NONE',  ( -9.596002108778193929, -79.74791666666662593, 7.374560639698935383 ) ) ;
#49955 = CIRCLE ( 'NONE', #43362, 0.5000000000000006661 ) ;
#49956 = ORIENTED_EDGE ( 'NONE', *, *, #18189, .F. ) ;
#49957 = CARTESIAN_POINT ( 'NONE',  ( -1.432420283025999996, -76.13522018723111273, 11.09153081809999897 ) ) ;
#49958 = CARTESIAN_POINT ( 'NONE',  ( 9.783241737786999792, -24.53564621530999901, 7.961026681561000018 ) ) ;
#49959 = CARTESIAN_POINT ( 'NONE',  ( -10.87089293717000160, -76.56611249766200444, 0.9996073426339999735 ) ) ;
#49960 = AXIS2_PLACEMENT_3D ( 'NONE', #56201, #1605, #55912 ) ;
#49961 = EDGE_CURVE ( 'NONE', #21244, #5115, #51648, .T. ) ;
#49962 = CARTESIAN_POINT ( 'NONE',  ( 10.47513974136000137, -60.60361494148999384, 7.624776006180999488 ) ) ;
#49963 = CARTESIAN_POINT ( 'NONE',  ( 1.250000000000000000, -82.34999999999999432, 0.000000000000000000 ) ) ;
#49964 = CARTESIAN_POINT ( 'NONE',  ( 7.483664081376597998, -78.37121083338536209, 9.354932563365712994 ) ) ;
#49965 = CARTESIAN_POINT ( 'NONE',  ( 10.63562707217000103, -80.10962425429239886, 3.563914325689000240 ) ) ;
#49966 = CARTESIAN_POINT ( 'NONE',  ( 6.715248240283044900, -81.00000000000001421, 8.571091062759663259 ) ) ;
#49967 = ORIENTED_EDGE ( 'NONE', *, *, #30439, .F. ) ;
#49968 = CARTESIAN_POINT ( 'NONE',  ( -9.355938762748150950, -25.17483711029779414, 8.610912454445188047 ) ) ;
#49969 = ORIENTED_EDGE ( 'NONE', *, *, #6348, .F. ) ;
#49970 = CARTESIAN_POINT ( 'NONE',  ( 2.734482912475208582, -77.45129537202082304, 8.836507949619202051 ) ) ;
#49971 = CARTESIAN_POINT ( 'NONE',  ( -10.47078769031000078, -77.89551604846599275, -3.499536356729999742 ) ) ;
#49972 = FACE_OUTER_BOUND ( 'NONE', #40938, .T. ) ;
#49973 = CARTESIAN_POINT ( 'NONE',  ( -8.592320330817999618, -78.35198780244898842, 4.510292750937000328 ) ) ;
#49974 = CARTESIAN_POINT ( 'NONE',  ( -9.924175329023000813, -75.86290228657999535, 8.344828977268999637 ) ) ;
#49975 = CARTESIAN_POINT ( 'NONE',  ( -2.588288305445375137, -2.052526692832498334, -2.006457613103411752 ) ) ;
#49976 = CARTESIAN_POINT ( 'NONE',  ( 0.08338359222296000406, -79.45859229021999681, -1.538001148114999994 ) ) ;
#49977 = DIRECTION ( 'NONE',  ( 1.000000000000000000, 0.000000000000000000, 0.000000000000000000 ) ) ;
#49978 = CARTESIAN_POINT ( 'NONE',  ( -10.10513987668000091, -78.46047970211098743, -4.192131248929999998 ) ) ;
#49979 = CARTESIAN_POINT ( 'NONE',  ( -7.956422463014998669, -24.52889896183999596, -9.787948076355000637 ) ) ;
#49980 = CARTESIAN_POINT ( 'NONE',  ( -8.140250184790149390, -60.25160423311102420, 7.398464061237165268 ) ) ;
#49981 = CARTESIAN_POINT ( 'NONE',  ( 3.478467325896999807, -83.82118105601298907, 0.8854434467574999745 ) ) ;
#49982 = AXIS2_PLACEMENT_3D ( 'NONE', #9671, #4663, #9382 ) ;
#49983 = EDGE_LOOP ( 'NONE', ( #48154, #53772 ) ) ;
#49984 = CARTESIAN_POINT ( 'NONE',  ( -2.526159795857000123, -79.54969871684099303, -12.05506223905000063 ) ) ;
#49985 = CARTESIAN_POINT ( 'NONE',  ( 8.325915139015000577, -76.51939509872099165, 7.923884736887000457 ) ) ;
#49986 = CARTESIAN_POINT ( 'NONE',  ( -7.655266710338128000, -78.03807782818779515, 7.547193342383588188 ) ) ;
#49987 = CARTESIAN_POINT ( 'NONE',  ( 11.79843486695000010, -77.43781749739399345, -2.076781258317999868 ) ) ;
#49988 = CARTESIAN_POINT ( 'NONE',  ( 3.165411199172024848, -3.270833333333332593, 0.8506806241676669877 ) ) ;
#49990 = DIRECTION ( 'NONE',  ( 0.000000000000000000, -1.000000000000000000, 0.000000000000000000 ) ) ;
#49989 = CARTESIAN_POINT ( 'NONE',  ( -11.75000000000000000, -78.29999999999999716, 0.000000000000000000 ) ) ;
#49991 = DIRECTION ( 'NONE',  ( -0.7071067811865475727, 0.000000000000000000, 0.7071067811865475727 ) ) ;
#49992 = CARTESIAN_POINT ( 'NONE',  ( 4.887195288127127668, -80.93790857794486726, 9.583764635476553551 ) ) ;
#49993 = CARTESIAN_POINT ( 'NONE',  ( -7.233356275331999541, -78.52392489796099539, 6.024097567370000128 ) ) ;
#49994 = CARTESIAN_POINT ( 'NONE',  ( 3.241578942234978111, -85.83735717367099483, -1.443243930775048645 ) ) ;
#49995 = CARTESIAN_POINT ( 'NONE',  ( -3.224264963920000504, -76.99278493408199608, -10.67046002915000003 ) ) ;
#49996 = CARTESIAN_POINT ( 'NONE',  ( -3.140974612311405512, -78.19583333333332575, 11.68767212001977640 ) ) ;
#49997 = CARTESIAN_POINT ( 'NONE',  ( -8.204091511170000572, -80.95026737670430350, -7.537247813386999340 ) ) ;
#49998 = ORIENTED_EDGE ( 'NONE', *, *, #44849, .F. ) ;
#49999 = CARTESIAN_POINT ( 'NONE',  ( 10.35453599130000057, -76.75783510652000530, -6.064947188958000446 ) ) ;
#50000 = CARTESIAN_POINT ( 'NONE',  ( 8.503129636637000388, -77.86329903538302233, -4.225430575863000193 ) ) ;
#50001 = CARTESIAN_POINT ( 'NONE',  ( 0.000000000000000000, -46.43897132165000130, 0.000000000000000000 ) ) ;
#50002 = CARTESIAN_POINT ( 'NONE',  ( 5.263131812197999970, -77.86218301344499082, -9.905430536777000583 ) ) ;
#50003 = DIRECTION ( 'NONE',  ( 0.000000000000000000, 0.000000000000000000, 1.000000000000000000 ) ) ;
#50004 = CARTESIAN_POINT ( 'NONE',  ( 0.4254240051736215000, -1.635416666666666519, -3.250000000000000000 ) ) ;
#50005 = CARTESIAN_POINT ( 'NONE',  ( -2.651434666701682374, -82.99739581956490042, 3.011249467861417450 ) ) ;
#50006 = CARTESIAN_POINT ( 'NONE',  ( 1.452949461559788435, -79.75000000000001421, -9.164018243494927773 ) ) ;
#50007 = CARTESIAN_POINT ( 'NONE',  ( 12.65989785480000229, -17.05665906540999899, 0.9744897697750000143 ) ) ;
#50008 = VECTOR ( 'NONE', #16761, 1000.000000000000000 ) ;
#50009 = CARTESIAN_POINT ( 'NONE',  ( 0.3142732060366000280, -82.78817953870900226, 4.160263707816999279 ) ) ;
#50010 = CARTESIAN_POINT ( 'NONE',  ( -11.00000000000000000, -23.75000000000000000, 0.000000000000000000 ) ) ;
#50011 = CARTESIAN_POINT ( 'NONE',  ( 9.310166272052999403, -53.66468533943000097, -8.596757084861000209 ) ) ;
#50012 = CARTESIAN_POINT ( 'NONE',  ( 11.01685767354999967, -76.94669371350400411, -1.698071721886999841 ) ) ;
#50013 = CARTESIAN_POINT ( 'NONE',  ( 12.50000000000000000, -18.75000000310999937, -1.750000000000000000 ) ) ;
#50014 = CARTESIAN_POINT ( 'NONE',  ( 1.097836406584000057, -78.70566276047000542, 1.092911459613999936 ) ) ;
#50015 = CARTESIAN_POINT ( 'NONE',  ( -6.294203684166999935, -77.32184250771798872, 7.343715272572999275 ) ) ;
#50016 = CARTESIAN_POINT ( 'NONE',  ( 1.423276841203632515, -83.02732328005990325, 0.5108568199358340944 ) ) ;
#50017 = CARTESIAN_POINT ( 'NONE',  ( -12.48375848566000101, -60.17270426026000507, 1.669543623995999981 ) ) ;
#50018 = CARTESIAN_POINT ( 'NONE',  ( 1.684372618195999927, -78.21273873898907425, 10.84559388857000073 ) ) ;
#50019 = CARTESIAN_POINT ( 'NONE',  ( 0.000000000000000000, -32.70420297070000260, 0.000000000000000000 ) ) ;
#50020 = EDGE_CURVE ( 'NONE', #24677, #31756, #14287, .T. ) ;
#50021 = ORIENTED_EDGE ( 'NONE', *, *, #35084, .T. ) ;
#50022 = CARTESIAN_POINT ( 'NONE',  ( 0.8955375890287041729, -81.78914646445058168, -0.8716670893819381538 ) ) ;
#50023 = EDGE_CURVE ( 'NONE', #2755, #12936, #16393, .T. ) ;
#50024 = DIRECTION ( 'NONE',  ( 1.000000000000000000, 0.000000000000000000, 0.000000000000000000 ) ) ;
#50025 = CARTESIAN_POINT ( 'NONE',  ( 10.83083824887000013, -79.62213958541198622, -2.635819302916999618 ) ) ;
#50026 = CARTESIAN_POINT ( 'NONE',  ( -17.49999999998999911, -28.92928575306000383, -1.613072089525000228E-05 ) ) ;
#50027 = ORIENTED_EDGE ( 'NONE', *, *, #49509, .F. ) ;
#50028 = ORIENTED_EDGE ( 'NONE', *, *, #35628, .T. ) ;
#50029 = CARTESIAN_POINT ( 'NONE',  ( -12.50000000000000000, -23.24999999688999708, -1.750000000000000000 ) ) ;
#50030 = ORIENTED_EDGE ( 'NONE', *, *, #20733, .T. ) ;
#50031 = ORIENTED_EDGE ( 'NONE', *, *, #24578, .F. ) ;
#50032 = FACE_OUTER_BOUND ( 'NONE', #33707, .T. ) ;
#50033 = CARTESIAN_POINT ( 'NONE',  ( -1.870137171474999915, -79.96171613058454852, -11.09839649295000008 ) ) ;
#50034 = DIRECTION ( 'NONE',  ( -1.000000000000000000, 0.000000000000000000, 0.000000000000000000 ) ) ;
#50035 = EDGE_CURVE ( 'NONE', #37958, #54663, #946, .T. ) ;
#50036 = CARTESIAN_POINT ( 'NONE',  ( 1.200170490671999879, -24.43405701997999913, -12.43444080551000042 ) ) ;
#50037 = CARTESIAN_POINT ( 'NONE',  ( 2.211821066349999754, -82.42182391443098766, -2.826968957741000210 ) ) ;
#50038 = CARTESIAN_POINT ( 'NONE',  ( 0.000000000000000000, -76.29999999999999716, -2.000000000000000000 ) ) ;
#50039 = CARTESIAN_POINT ( 'NONE',  ( -4.723620464148000408, -78.23902343179999264, 10.90888302421999789 ) ) ;
#50040 = VERTEX_POINT ( 'NONE', #20618 ) ;
#50041 = ORIENTED_EDGE ( 'NONE', *, *, #52437, .T. ) ;
#50042 = DIRECTION ( 'NONE',  ( 0.000000000000000000, 1.000000000000000000, 0.000000000000000000 ) ) ;
#50043 = DIRECTION ( 'NONE',  ( 1.000000000000000000, 0.000000000000000000, 0.000000000000000000 ) ) ;
#50044 = CARTESIAN_POINT ( 'NONE',  ( 0.1636246173744642929, -81.36458333333332860, 1.250000000000000888 ) ) ;
#50045 = CARTESIAN_POINT ( 'NONE',  ( 1.323534079420999987, -80.00586178980599072, -0.1638099207045999872 ) ) ;
#50046 = CIRCLE ( 'NONE', #11359, 1.750000000000000000 ) ;
#50047 = CARTESIAN_POINT ( 'NONE',  ( 9.259046916275000427, -78.48374114585499228, 2.905298533503999803 ) ) ;
#50048 = DIRECTION ( 'NONE',  ( 0.000000000000000000, 0.000000000000000000, -1.000000000000000000 ) ) ;
#50049 = CARTESIAN_POINT ( 'NONE',  ( -10.53003223722999948, -23.32452529362999982, 7.612971414713999962 ) ) ;
#50050 = CARTESIAN_POINT ( 'NONE',  ( -1.243328516745999979, -77.44871687587999531, -12.73826093197000020 ) ) ;
#50051 = CARTESIAN_POINT ( 'NONE',  ( 1.312293141192999890, -79.84918819389999101, 0.3222699683723999620 ) ) ;
#50052 = ADVANCED_FACE ( 'NONE', ( #3472 ), #50482, .F. ) ;
#50053 = DIRECTION ( 'NONE',  ( 0.000000000000000000, -1.000000000000000000, 0.000000000000000000 ) ) ;
#50054 = CARTESIAN_POINT ( 'NONE',  ( 7.919595949288999570, -59.94999999969999749, 9.050966799188000067 ) ) ;
#50055 = CARTESIAN_POINT ( 'NONE',  ( 4.049271546212999340, -82.49041413704399872, -0.2668988840931000306 ) ) ;
#50056 = CARTESIAN_POINT ( 'NONE',  ( 5.365883907697000410, -80.03381055689840196, 9.905345355165000143 ) ) ;
#50057 = CARTESIAN_POINT ( 'NONE',  ( -4.000000000000000000, -74.80000000000001137, -0.5999999999999999778 ) ) ;
#50058 = CARTESIAN_POINT ( 'NONE',  ( -11.75000000000000000, -78.29999999999999716, 0.000000000000000000 ) ) ;
#50059 = CARTESIAN_POINT ( 'NONE',  ( -2.719119925748999744, -78.88532046129088826, -2.278397777311000016 ) ) ;
#50061 = CARTESIAN_POINT ( 'NONE',  ( -0.9612450871864000046, -78.78283387801499771, -0.9244371432244999909 ) ) ;
#50060 = LINE ( 'NONE', #9606, #5192 ) ;
#50062 = CARTESIAN_POINT ( 'NONE',  ( 1.249999996278000181, -76.50000000037098857, 0.4999999996289999915 ) ) ;
#50063 = CARTESIAN_POINT ( 'NONE',  ( -0.3187246912203000049, -80.77893456479243639, 11.26088853021000169 ) ) ;
#50064 = CARTESIAN_POINT ( 'NONE',  ( 3.521688171515000132, -3.617922206379000194, 0.7298424208991000084 ) ) ;
#50065 = ORIENTED_EDGE ( 'NONE', *, *, #14581, .F. ) ;
#50066 = CARTESIAN_POINT ( 'NONE',  ( 0.1577469407148825997, -23.75042584457689898, 11.00002392222777203 ) ) ;
#50067 = CARTESIAN_POINT ( 'NONE',  ( -0.5962167095188589672, -18.77158755790547318, -10.98383273456533438 ) ) ;
#50068 = B_SPLINE_CURVE_WITH_KNOTS ( 'NONE', 3,
 ( #22902, #40020, #32033, #44457, #4008, #54205, #17299, #5190 ),
 .UNSPECIFIED., .F., .F.,
 ( 4, 2, 2, 4 ),
 ( 0.000000000000000000, 0.4999999999999977796, 0.7499999999999988898, 1.000000000000000000 ),
 .UNSPECIFIED. ) ;
#50069 = CARTESIAN_POINT ( 'NONE',  ( -11.75000000000000000, -77.70000000000000284, 0.000000000000000000 ) ) ;
#50070 = DIRECTION ( 'NONE',  ( 0.000000000000000000, -1.000000000000000000, 0.000000000000000000 ) ) ;
#50071 = AXIS2_PLACEMENT_3D ( 'NONE', #56259, #55089, #32920 ) ;
#50072 = B_SPLINE_CURVE_WITH_KNOTS ( 'NONE', 3,
 ( #32286, #37313, #32578, #28153, #5730, #31707, #13417, #31417, #36156, #54175, #10464, #55328, #28449, #14873, #51792, #20198, #46498, #24908 ),
 .UNSPECIFIED., .F., .F.,
 ( 4, 2, 2, 2, 2, 2, 2, 2, 4 ),
 ( 0.000000000000000000, 0.1250000000000000000, 0.2500000000000000000, 0.3750000000000000000, 0.5000000000000000000, 0.6250000000000000000, 0.7500000000000000000, 0.8750000000000000000, 1.000000000000000000 ),
 .UNSPECIFIED. ) ;
#50073 = CARTESIAN_POINT ( 'NONE',  ( 9.690945690674999113, -79.58805234752598778, 1.084186244826999879 ) ) ;
#50074 = CARTESIAN_POINT ( 'NONE',  ( -3.129814719915999799, -78.41165560753999841, 12.62985940900000159 ) ) ;
#50075 = CARTESIAN_POINT ( 'NONE',  ( -8.944662455087330599, -79.55325894290034228, 5.962789625861153020 ) ) ;
#50076 = CARTESIAN_POINT ( 'NONE',  ( -2.382925498960999811, -79.40178667140099833, 9.329537718716998995 ) ) ;
#50077 = CARTESIAN_POINT ( 'NONE',  ( -4.744667937345999675, -76.40032876540000473, 11.57788746584999906 ) ) ;
#50078 = ORIENTED_EDGE ( 'NONE', *, *, #8781, .F. ) ;
#50079 = CYLINDRICAL_SURFACE ( 'NONE', #4248, 1.750000000000000000 ) ;
#50080 = CARTESIAN_POINT ( 'NONE',  ( 7.408857453855000053, -77.49712623080398544, 8.497927402505000671 ) ) ;
#50081 = CARTESIAN_POINT ( 'NONE',  ( -1.042454788111000008, -81.85600493344199435, -0.9471436726904000070 ) ) ;
#50082 = CARTESIAN_POINT ( 'NONE',  ( 7.691893942754999713, -20.24546192895000019, -10.42272502865000128 ) ) ;
#50083 = VECTOR ( 'NONE', #23069, 1000.000000000000000 ) ;
#50084 = CARTESIAN_POINT ( 'NONE',  ( -6.351606481687999128, -78.39004745520499284, 7.094185741421999758 ) ) ;
#50086 = CARTESIAN_POINT ( 'NONE',  ( -1.488596180559999871, -0.8427806054948999703, -3.730054860412999940 ) ) ;
#50085 = CARTESIAN_POINT ( 'NONE',  ( 3.962535311936000060, -82.14153471428599573, -0.06234140039890999352 ) ) ;
#50087 = CARTESIAN_POINT ( 'NONE',  ( -0.1636246173744726473, -82.38541666666665719, 1.249999999999999112 ) ) ;
#50088 = DIRECTION ( 'NONE',  ( -0.9999433559010179051, 0.000000000000000000, -0.01064354214585019887 ) ) ;
#50089 = EDGE_LOOP ( 'NONE', ( #31772, #46844, #11502, #48284 ) ) ;
#50090 = CARTESIAN_POINT ( 'NONE',  ( 7.705636733279908057, -77.28876659844397068, -7.495763092362167868 ) ) ;
#50091 = CARTESIAN_POINT ( 'NONE',  ( -0.3926218265389189721, -79.00416666666667709, -1.460959015002473604 ) ) ;
#50092 = CONICAL_SURFACE ( 'NONE', #8542, 11.09999999881999955, 0.7853981633972997312 ) ;
#50093 = VERTEX_POINT ( 'NONE', #31478 ) ;
#50094 = ORIENTED_EDGE ( 'NONE', *, *, #35376, .F. ) ;
#50095 = CARTESIAN_POINT ( 'NONE',  ( -9.408410525920000822, -79.41343168043698597, -5.582976599613999724 ) ) ;
#50096 = CARTESIAN_POINT ( 'NONE',  ( 0.000000000000000000, -13.07071424677999971, 0.000000000000000000 ) ) ;
#50097 = DIRECTION ( 'NONE',  ( 0.000000000000000000, 1.000000000000000000, 0.000000000000000000 ) ) ;
#50098 = ORIENTED_EDGE ( 'NONE', *, *, #46865, .T. ) ;
#50099 = CARTESIAN_POINT ( 'NONE',  ( 2.945718361321999712, -78.97825989114500089, 11.40680644849000025 ) ) ;
#50100 = EDGE_LOOP ( 'NONE', ( #55679, #15893, #19726, #46036 ) ) ;
#50101 = ORIENTED_EDGE ( 'NONE', *, *, #43060, .F. ) ;
#50102 = CARTESIAN_POINT ( 'NONE',  ( -3.128637044992019334, -2.622704922558018126, -0.9068569082304414053 ) ) ;
#50103 = EDGE_CURVE ( 'NONE', #10301, #43339, #28349, .T. ) ;
#50104 = DIRECTION ( 'NONE',  ( 0.000000000000000000, 0.000000000000000000, -1.000000000000000000 ) ) ;
#50105 = CARTESIAN_POINT ( 'NONE',  ( 9.383705654690636777, -79.16227050890121575, 1.484107674336303972 ) ) ;
#50106 = ORIENTED_EDGE ( 'NONE', *, *, #56872, .F. ) ;
#50107 = CARTESIAN_POINT ( 'NONE',  ( 0.8928342013463602678, -82.78896698447270808, -0.8742295960309274250 ) ) ;
#50108 = B_SPLINE_CURVE_WITH_KNOTS ( 'NONE', 3,
 ( #5843, #45733, #6137, #18852, #27401, #50446, #22985, #5268, #23277, #41282, #866, #32402, #10880 ),
 .UNSPECIFIED., .F., .F.,
 ( 4, 1, 2, 2, 2, 2, 4 ),
 ( 0.000000000000000000, 0.1250000000000001110, 0.1875000000000000833, 0.2500000000000000555, 0.5000000000000000000, 0.7500000000000000000, 1.000000000000000000 ),
 .UNSPECIFIED. ) ;
#50109 = ORIENTED_EDGE ( 'NONE', *, *, #12669, .T. ) ;
#50110 = CARTESIAN_POINT ( 'NONE',  ( -0.4077636671461413176, -80.05112375978934836, 1.207988005846317270 ) ) ;
#50111 = CARTESIAN_POINT ( 'NONE',  ( -4.036611966185642331, -78.77851881763733388, -2.280826645528176488 ) ) ;
#50112 = LINE ( 'NONE', #22648, #31161 ) ;
#50113 = CARTESIAN_POINT ( 'NONE',  ( 7.995633008690000487, -76.57771923186500374, 7.819446035993999899 ) ) ;
#50114 = CARTESIAN_POINT ( 'NONE',  ( 0.000000000000000000, -81.79999999999998295, 0.000000000000000000 ) ) ;
#50115 = DIRECTION ( 'NONE',  ( 0.7071067811865975328, -3.445410891335986341E-11, 0.7071067811864976127 ) ) ;
#50116 = EDGE_CURVE ( 'NONE', #56774, #27498, #36221, .T. ) ;
#50117 = CARTESIAN_POINT ( 'NONE',  ( -10.11684109197000048, -76.35912155000400503, -4.871678881582000464 ) ) ;
#50118 = CARTESIAN_POINT ( 'NONE',  ( -1.686463579793599399, -78.71046731272916475, -9.094966459575084983 ) ) ;
#50119 = CARTESIAN_POINT ( 'NONE',  ( 9.869603865684988264, -77.06050208244033684, -5.330340373397550735 ) ) ;
#50120 = FACE_OUTER_BOUND ( 'NONE', #57841, .T. ) ;
#50121 = DIRECTION ( 'NONE',  ( 0.000000000000000000, 1.000000000000000000, 0.000000000000000000 ) ) ;
#50122 = VECTOR ( 'NONE', #1833, 1000.000000000000114 ) ;
#50123 = DIRECTION ( 'NONE',  ( 0.000000000000000000, 1.000000000000000000, 0.000000000000000000 ) ) ;
#50124 = DIRECTION ( 'NONE',  ( -1.000000000000000000, 0.000000000000000000, 0.000000000000000000 ) ) ;
#50125 = CARTESIAN_POINT ( 'NONE',  ( -1.093701836234999947, -81.08703455456799247, 3.809172760610000097 ) ) ;
#50126 = AXIS2_PLACEMENT_3D ( 'NONE', #7589, #2876, #44187 ) ;
#50127 = CARTESIAN_POINT ( 'NONE',  ( -5.375314035255999379, -77.27111332859900017, -8.017434526278000462 ) ) ;
#50128 = CARTESIAN_POINT ( 'NONE',  ( -1.750000000001000089, -59.55100836327999758, 12.60354432391999957 ) ) ;
#50129 = FACE_OUTER_BOUND ( 'NONE', #11009, .T. ) ;
#50130 = CARTESIAN_POINT ( 'NONE',  ( 0.5390150933987999382, -25.26260891652000140, 12.77520261005000002 ) ) ;
#50131 = CARTESIAN_POINT ( 'NONE',  ( 11.02435598943671380, -79.24999999999995737, -4.903336795166640449 ) ) ;
#50132 = DIRECTION ( 'NONE',  ( 1.000000000000000000, 0.000000000000000000, 0.000000000000000000 ) ) ;
#50133 = CARTESIAN_POINT ( 'NONE',  ( -3.542934954918000034, -1.497403522604999981, -1.344521724440000066 ) ) ;
#50134 = CARTESIAN_POINT ( 'NONE',  ( 1.217465845835393967, -80.77083333333331439, 0.3271848554491025851 ) ) ;
#50135 = CARTESIAN_POINT ( 'NONE',  ( 12.70228545255524111, -24.82820680357308518, -1.205254117560517146 ) ) ;
#50136 = CARTESIAN_POINT ( 'NONE',  ( -0.2201363562291999698, -79.46327907014000402, -1.483758735329000045 ) ) ;
#50137 = CARTESIAN_POINT ( 'NONE',  ( 7.624341764943999955, -60.06485149430999826, -10.42531124854999902 ) ) ;
#50138 = FACE_OUTER_BOUND ( 'NONE', #50321, .T. ) ;
#50139 = ADVANCED_FACE ( 'NONE', ( #49523 ), #22345, .F. ) ;
#50140 = CARTESIAN_POINT ( 'NONE',  ( 1.250000000000000222, -80.73958333333331439, -0.1636246173744659582 ) ) ;
#50141 = DIRECTION ( 'NONE',  ( 0.000000000000000000, 1.000000000000000000, -4.736951571734000187E-14 ) ) ;
#50142 = DIRECTION ( 'NONE',  ( -0.7071067811865474617, 0.000000000000000000, 0.7071067811865474617 ) ) ;
#50144 = CARTESIAN_POINT ( 'NONE',  ( -0.1273708076881999995, -77.97099286884960634, -1.510858618444999912 ) ) ;
#50143 = DIRECTION ( 'NONE',  ( 0.7071067811865470176, -0.7071067811865470176, 3.680441518142245308E-08 ) ) ;
#50145 = CARTESIAN_POINT ( 'NONE',  ( 0.4779442704572000045, -81.85602282125999807, -1.511941137165000004 ) ) ;
#50146 =( BOUNDED_SURFACE ( )  B_SPLINE_SURFACE ( 3, 3, ( 
 ( #8291, #26002, #40468, #21582, #53169, #44604, #8583 ),
 ( #44027, #3864, #39587, #49036, #60, #3578, #21864 ),
 ( #4157, #57592, #40758, #26571, #58178, #39871, #352 ),
 ( #44308, #48748, #18035, #22157, #17743, #17152, #35138 ),
 ( #57884, #17440, #35426, #36028, #35731, #12718, #34854 ),
 ( #12437, #31584, #8005, #53456, #26295, #48462, #54054 ),
 ( #54348, #51091, #18624, #50798, #928, #14750, #15052 ),
 ( #55504, #36615, #28038, #27455, #13887, #6194, #14173 ),
 ( #32750, #36901, #5898, #46374, #19488, #32170, #27744 ),
 ( #10640, #55207, #5608, #36324, #37481, #23908, #54914 ),
 ( #24207, #41926, #23038, #1498, #33044, #1210, #46667 ),
 ( #14466, #28622, #50502, #42225, #18331, #31882, #49925 ),
 ( #54637, #28322, #9470, #10343, #45493, #5036, #41054 ),
 ( #23334, #46083, #641, #50209, #9759, #45791, #5327 ),
 ( #41344, #18908, #32457, #10056, #23617, #41630, #19202 ) ),
 .UNSPECIFIED., .F., .F., .T. ) 
 B_SPLINE_SURFACE_WITH_KNOTS ( ( 4, 1, 1, 1, 1, 1, 1, 1, 1, 1, 1, 1, 4 ),
 ( 4, 3, 4 ),
 ( 0.009836358966825000175, 0.09153389967814999639, 0.1732269073519000224, 0.2549246240467999969, 0.3366128957582000258, 0.4183102327763000283, 0.5000049915180999616, 0.5816997512343000665, 0.6633971206824998967, 0.7450853986059999823, 0.8267830947368000061, 0.9084761241232000017, 0.9901736480482069558 ),
 ( 0.000000000000000000, 0.5000000000000000000, 1.000000000000000000 ),
 .UNSPECIFIED. ) 
 GEOMETRIC_REPRESENTATION_ITEM ( )  RATIONAL_B_SPLINE_SURFACE ( (
 ( 1.000000000000000000, 0.8025111637939374987, 0.8025111637939374987, 1.000000000000000000, 0.8025111637939374987, 0.8025111637939374987, 1.000000000000000000),
 ( 1.000000000000000000, 0.8025111637939374987, 0.8025111637939374987, 1.000000000000000000, 0.8025111637939374987, 0.8025111637939374987, 1.000000000000000000),
 ( 1.000000000000000000, 0.8025111637939374987, 0.8025111637939374987, 1.000000000000000000, 0.8025111637939374987, 0.8025111637939374987, 1.000000000000000000),
 ( 1.000000000000000000, 0.8025111637939374987, 0.8025111637939374987, 1.000000000000000000, 0.8025111637939374987, 0.8025111637939374987, 1.000000000000000000),
 ( 1.000000000000000000, 0.8025111637939374987, 0.8025111637939374987, 1.000000000000000000, 0.8025111637939374987, 0.8025111637939374987, 1.000000000000000000),
 ( 1.000000000000000000, 0.8025111637939374987, 0.8025111637939374987, 1.000000000000000000, 0.8025111637939374987, 0.8025111637939374987, 1.000000000000000000),
 ( 1.000000000000000000, 0.8025111637939374987, 0.8025111637939374987, 1.000000000000000000, 0.8025111637939374987, 0.8025111637939374987, 1.000000000000000000),
 ( 1.000000000000000000, 0.8025111637939374987, 0.8025111637939374987, 1.000000000000000000, 0.8025111637939374987, 0.8025111637939374987, 1.000000000000000000),
 ( 1.000000000000000000, 0.8025111637939374987, 0.8025111637939374987, 1.000000000000000000, 0.8025111637939374987, 0.8025111637939374987, 1.000000000000000000),
 ( 1.000000000000000000, 0.8025111637939374987, 0.8025111637939374987, 1.000000000000000000, 0.8025111637939374987, 0.8025111637939374987, 1.000000000000000000),
 ( 1.000000000000000000, 0.8025111637939374987, 0.8025111637939374987, 1.000000000000000000, 0.8025111637939374987, 0.8025111637939374987, 1.000000000000000000),
 ( 1.000000000000000000, 0.8025111637939374987, 0.8025111637939374987, 1.000000000000000000, 0.8025111637939374987, 0.8025111637939374987, 1.000000000000000000),
 ( 1.000000000000000000, 0.8025111637939374987, 0.8025111637939374987, 1.000000000000000000, 0.8025111637939374987, 0.8025111637939374987, 1.000000000000000000),
 ( 1.000000000000000000, 0.8025111637939374987, 0.8025111637939374987, 1.000000000000000000, 0.8025111637939374987, 0.8025111637939374987, 1.000000000000000000),
 ( 1.000000000000000000, 0.8025111637939374987, 0.8025111637939374987, 1.000000000000000000, 0.8025111637939374987, 0.8025111637939374987, 1.000000000000000000) ) ) 
 REPRESENTATION_ITEM ( '' )  SURFACE ( )  );
#50147 = ORIENTED_EDGE ( 'NONE', *, *, #4244, .T. ) ;
#50148 = CARTESIAN_POINT ( 'NONE',  ( -3.420407972780000083, -86.36232450217399048, 0.3739914737839999948 ) ) ;
#50149 = CARTESIAN_POINT ( 'NONE',  ( -4.367055522304000625, -79.98072316220059008, 10.15682858329000027 ) ) ;
#50150 = LINE ( 'NONE', #9692, #26609 ) ;
#50151 = CARTESIAN_POINT ( 'NONE',  ( -2.535599314688579575, -86.02291667262494457, 2.329467182686746352 ) ) ;
#50152 = CARTESIAN_POINT ( 'NONE',  ( 4.275724345439000373, -76.99001542893100236, -10.36997068233999997 ) ) ;
#50153 = CARTESIAN_POINT ( 'NONE',  ( 10.09635298636608880, -23.52373519997163953, -7.644087781972076279 ) ) ;
#50154 = DIRECTION ( 'NONE',  ( 0.000000000000000000, 0.000000000000000000, 1.000000000000000000 ) ) ;
#50155 = CARTESIAN_POINT ( 'NONE',  ( -10.29607860738999925, -77.70636465244999158, 7.334573225905999472 ) ) ;
#50156 = CARTESIAN_POINT ( 'NONE',  ( 8.775844806878042803, -79.80000000000001137, -7.911246177938791035 ) ) ;
#50157 = CARTESIAN_POINT ( 'NONE',  ( 9.075965193531663644, -80.99999999999998579, -6.216670379854907225 ) ) ;
#50158 = VERTEX_POINT ( 'NONE', #248 ) ;
#50159 = CARTESIAN_POINT ( 'NONE',  ( 10.98362417419999915, -18.84999999999999787, 0.5999999999999999778 ) ) ;
#50160 = CARTESIAN_POINT ( 'NONE',  ( 5.983750641729000286, -79.30913998579799795, -7.270309104952999313 ) ) ;
#50161 = FACE_OUTER_BOUND ( 'NONE', #8766, .T. ) ;
#50162 = DIRECTION ( 'NONE',  ( 0.000000000000000000, -1.000000000000000000, 0.000000000000000000 ) ) ;
#50163 = DIRECTION ( 'NONE',  ( 0.000000000000000000, 1.000000000000000000, 0.000000000000000000 ) ) ;
#50164 = ORIENTED_EDGE ( 'NONE', *, *, #30455, .F. ) ;
#50165 = CARTESIAN_POINT ( 'NONE',  ( -6.086064908458999945, -77.85035948279599438, 9.284690194605000002 ) ) ;
#50166 = CARTESIAN_POINT ( 'NONE',  ( -2.062670899148999926, -18.69360374348000065, 12.83044039274999903 ) ) ;
#50167 = ORIENTED_EDGE ( 'NONE', *, *, #53837, .F. ) ;
#50168 = CIRCLE ( 'NONE', #53914, 14.00000000000000000 ) ;
#50169 = VERTEX_POINT ( 'NONE', #40360 ) ;
#50170 = DIRECTION ( 'NONE',  ( 0.7071067811865474617, 0.000000000000000000, -0.7071067811865474617 ) ) ;
#50171 = ADVANCED_FACE ( 'NONE', ( #26764 ), #26469, .F. ) ;
#50172 = CARTESIAN_POINT ( 'NONE',  ( -0.6514213267380000172, -79.89061850717349955, 9.745581310452999801 ) ) ;
#50173 = ORIENTED_EDGE ( 'NONE', *, *, #28325, .F. ) ;
#50174 = DIRECTION ( 'NONE',  ( 1.000000000000000000, 0.000000000000000000, 0.000000000000000000 ) ) ;
#50175 = CARTESIAN_POINT ( 'NONE',  ( 10.27340958483875077, -24.06161210422248331, -7.712164009431025313 ) ) ;
#50176 = ADVANCED_FACE ( 'NONE', ( #18518 ), #27646, .F. ) ;
#50177 = CARTESIAN_POINT ( 'NONE',  ( -1.518142601816999893, -79.19490828658999249, 0.2258102331908000138 ) ) ;
#50178 = ORIENTED_EDGE ( 'NONE', *, *, #41362, .T. ) ;
#50179 = CARTESIAN_POINT ( 'NONE',  ( -5.597970637881999778, -76.99512305011499791, 7.669424558767000022 ) ) ;
#50180 = CARTESIAN_POINT ( 'NONE',  ( -0.8807074628163545915, -80.16329956998615103, -0.8865880600332928241 ) ) ;
#50181 = DIRECTION ( 'NONE',  ( 0.000000000000000000, 0.000000000000000000, 1.000000000000000000 ) ) ;
#50182 = CARTESIAN_POINT ( 'NONE',  ( -6.659967121051000305, -76.82441250745586103, -9.025682433062998555 ) ) ;
#50183 = CARTESIAN_POINT ( 'NONE',  ( 7.032282396509031308, -79.90637039191506119, 6.009017827964323821 ) ) ;
#50184 = EDGE_CURVE ( 'NONE', #35775, #19870, #44793, .T. ) ;
#50185 = CARTESIAN_POINT ( 'NONE',  ( 3.716963287104071867, -79.54791665507261200, 1.610115688683979585 ) ) ;
#50186 = ORIENTED_EDGE ( 'NONE', *, *, #30115, .T. ) ;
#50187 = CARTESIAN_POINT ( 'NONE',  ( 4.784380313523521444, -77.63333333333332575, 8.300970689365463784 ) ) ;
#50188 = CARTESIAN_POINT ( 'NONE',  ( 11.05577208806000122, -76.69928192833000935, -4.921212746988999243 ) ) ;
#50189 = CARTESIAN_POINT ( 'NONE',  ( 1.610212697858000030, -79.65213206121900669, -0.1201205297940999978 ) ) ;
#50190 = CARTESIAN_POINT ( 'NONE',  ( -3.494184512671483667, -2.339737559012720070, 0.4184823038404273388 ) ) ;
#50191 = DIRECTION ( 'NONE',  ( 0.000000000000000000, -1.000000000000000000, 0.000000000000000000 ) ) ;
#50192 = CARTESIAN_POINT ( 'NONE',  ( -3.417863094299999904, -78.38065028396999878, 11.50296535110000029 ) ) ;
#50193 = DIRECTION ( 'NONE',  ( 0.9999999999999998890, 1.433670265775999799E-08, 0.000000000000000000 ) ) ;
#50194 = DIRECTION ( 'NONE',  ( -1.000000000000000000, 0.000000000000000000, 0.000000000000000000 ) ) ;
#50195 = CARTESIAN_POINT ( 'NONE',  ( -2.745946062086999984, -76.98158998579799572, -9.341962526838999636 ) ) ;
#50196 = CARTESIAN_POINT ( 'NONE',  ( -10.97112726228940360, -77.01578936740024517, 5.028334835961087990 ) ) ;
#50197 = CARTESIAN_POINT ( 'NONE',  ( -5.394429334091999984, -79.83507596080985991, -9.834543342166998769 ) ) ;
#50198 = ORIENTED_EDGE ( 'NONE', *, *, #9869, .T. ) ;
#50199 = CARTESIAN_POINT ( 'NONE',  ( 0.4917238316050000502, -82.67461323090898873, -1.258641686703000140 ) ) ;
#50200 = DIRECTION ( 'NONE',  ( 0.7071067811865475727, 0.000000000000000000, 0.7071067811865475727 ) ) ;
#50201 = CARTESIAN_POINT ( 'NONE',  ( -1.250000000000001332, -79.48958333333334281, 0.1636246173744632659 ) ) ;
#50202 = VECTOR ( 'NONE', #42930, 1000.000000000000227 ) ;
#50203 = DIRECTION ( 'NONE',  ( 1.000000000000000000, 0.000000000000000000, 0.000000000000000000 ) ) ;
#50204 = CARTESIAN_POINT ( 'NONE',  ( 1.492218263521933874, -76.94999999999998863, -9.411694429295081932 ) ) ;
#50205 = CARTESIAN_POINT ( 'NONE',  ( -3.103176923767000162, -78.11313629324600072, -11.64328410086999988 ) ) ;
#50206 = CARTESIAN_POINT ( 'NONE',  ( 9.630178197611998669, -77.45787555610998254, 0.1134805908625000082 ) ) ;
#50207 = CARTESIAN_POINT ( 'NONE',  ( 9.107554314083696312, -76.00402216969793301, 7.423553679711462294 ) ) ;
#50208 = CARTESIAN_POINT ( 'NONE',  ( 7.679819846117000637, -79.14513978978800424, -7.919728626202000576 ) ) ;
#50209 = CARTESIAN_POINT ( 'NONE',  ( 1.353569424326575898, -86.07390000031791999, 3.118950113984900518 ) ) ;
#50210 = ORIENTED_EDGE ( 'NONE', *, *, #6837, .F. ) ;
#50211 = CARTESIAN_POINT ( 'NONE',  ( 7.709154088328855181, -18.07253195914803356, -9.998702477107977771 ) ) ;
#50212 = CIRCLE ( 'NONE', #6834, 4.000000000000000000 ) ;
#50213 = CARTESIAN_POINT ( 'NONE',  ( -3.819913647775994292, -78.40681307243319509, -2.158384532486305574 ) ) ;
#50215 = CARTESIAN_POINT ( 'NONE',  ( -5.036310450962679042, -76.28943874799483638, -10.61677181351809374 ) ) ;
#50214 = CARTESIAN_POINT ( 'NONE',  ( -13.98934701867000108, -46.22186981632000169, -1.420930502821999868E-05 ) ) ;
#50216 = CARTESIAN_POINT ( 'NONE',  ( 9.233664981878000333, -79.78590364676199442, 5.933249305785000871 ) ) ;
#50217 = CARTESIAN_POINT ( 'NONE',  ( -11.00000000000000000, -79.09999999999999432, 0.000000000000000000 ) ) ;
#50218 = CARTESIAN_POINT ( 'NONE',  ( 10.40130232906999908, -76.07658568656098907, -6.940236885917999032 ) ) ;
#50219 = CARTESIAN_POINT ( 'NONE',  ( 0.000000000000000000, -75.00000000000000000, -11.45000000000000107 ) ) ;
#50220 = CARTESIAN_POINT ( 'NONE',  ( 9.101506735347001609, -17.11932813898000205, -8.485532457246998561 ) ) ;
#50221 = CARTESIAN_POINT ( 'NONE',  ( 9.250000000000000000, -77.74999999999998579, 0.000000000000000000 ) ) ;
#50222 = ORIENTED_EDGE ( 'NONE', *, *, #37091, .T. ) ;
#50223 = EDGE_CURVE ( 'NONE', #11513, #6154, #23641, .T. ) ;
#50224 = CARTESIAN_POINT ( 'NONE',  ( -5.236138783747000147, -78.62277635977000045, 9.840602177168999987 ) ) ;
#50225 = CARTESIAN_POINT ( 'NONE',  ( -8.824831950807848102, -77.47489816006239494, 2.865719031100893321 ) ) ;
#50226 = CARTESIAN_POINT ( 'NONE',  ( -10.41906440735603390, -79.58915406351319177, -5.613747789635666230 ) ) ;
#50227 = CARTESIAN_POINT ( 'NONE',  ( 2.060606600077061756, -78.43735717367052018, 3.567928899679150057 ) ) ;
#50228 = AXIS2_PLACEMENT_3D ( 'NONE', #47825, #24788, #37780 ) ;
#50229 = CARTESIAN_POINT ( 'NONE',  ( -1.154931660856736153, -81.56894284788815241, 0.4778881009946403524 ) ) ;
#50230 = B_SPLINE_CURVE_WITH_KNOTS ( 'NONE', 3,
 ( #7711, #44019, #3571, #35131, #53163, #2717, #30705, #57013, #48741, #8285, #17434, #20714, #27153, #23329, #13289, #17736, #26564, #32165, #8872, #45786, #36895, #44894, #18618, #41336, #8577, #4445, #4742, #32452, #9464, #49918, #636, #27449, #18325, #41047, #44595, #346, #9171, #14167, #5321 ),
 .UNSPECIFIED., .F., .F.,
 ( 4, 1, 1, 1, 1, 1, 2, 2, 1, 1, 1, 1, 2, 2, 1, 1, 2, 2, 2, 2, 2, 2, 2, 2, 4 ),
 ( 0.000000000000000000, 0.06249999999999412970, 0.09374999999999117373, 0.1093749999999896888, 0.1171874999999888700, 0.1210937499999883704, 0.1230468749999882871, 0.1249999999999882039, 0.1874999999999883149, 0.2187499999999883982, 0.2343749999999884259, 0.2421874999999883704, 0.2460937499999883427, 0.2499999999999883427, 0.3124999999999890643, 0.3437499999999893419, 0.3593749999999896194, 0.3749999999999898415, 0.4374999999999908407, 0.4999999999999918954, 0.6249999999999938938, 0.7499999999999958922, 0.8124999999999970024, 0.8749999999999980016, 1.000000000000000000 ),
 .UNSPECIFIED. ) ;
#50231 = CARTESIAN_POINT ( 'NONE',  ( 4.665505440478000310, -78.64724708133699949, 10.01553556391000122 ) ) ;
#50232 = DIRECTION ( 'NONE',  ( 0.000000000000000000, 1.000000000000000000, 0.000000000000000000 ) ) ;
#50233 = CARTESIAN_POINT ( 'NONE',  ( -2.809159726167000048, -3.306933523454000046, -2.568020482856000264 ) ) ;
#50234 = CARTESIAN_POINT ( 'NONE',  ( -0.3926218265389190276, -81.10416666666667140, -1.460959015002473826 ) ) ;
#50235 = DIRECTION ( 'NONE',  ( 0.000000000000000000, -1.000000000000000000, 0.000000000000000000 ) ) ;
#50236 = CARTESIAN_POINT ( 'NONE',  ( 9.304647597727065289, -79.15561160917410177, -5.821627946328172598 ) ) ;
#50237 = CARTESIAN_POINT ( 'NONE',  ( -12.50659871789747513, -61.77347219457126215, 0.3508073943569843256 ) ) ;
#50238 = ORIENTED_EDGE ( 'NONE', *, *, #1131, .F. ) ;
#50239 = ORIENTED_EDGE ( 'NONE', *, *, #44488, .F. ) ;
#50240 = CARTESIAN_POINT ( 'NONE',  ( -3.329695900066999670, -77.97738998579799841, -9.453077866293002174 ) ) ;
#50241 = CARTESIAN_POINT ( 'NONE',  ( 7.628372981931305752, -78.78778873427579299, -7.574329845077384604 ) ) ;
#50242 = EDGE_CURVE ( 'NONE', #32054, #5068, #4044, .T. ) ;
#50243 = AXIS2_PLACEMENT_3D ( 'NONE', #6540, #38699, #42563 ) ;
#50244 = ORIENTED_EDGE ( 'NONE', *, *, #50242, .T. ) ;
#50245 = CARTESIAN_POINT ( 'NONE',  ( 4.903943924252999409, -76.41112154911152743, -10.05113017056000047 ) ) ;
#50246 = CARTESIAN_POINT ( 'NONE',  ( 0.5623895165579090305, -82.78541668270349874, 3.364310149638601199 ) ) ;
#50247 = CARTESIAN_POINT ( 'NONE',  ( 7.606021324617000090, -60.22158946241999899, 10.52692925329000140 ) ) ;
#50248 = CARTESIAN_POINT ( 'NONE',  ( -5.197406821774317009, -76.13935780419708976, -11.03714881444417806 ) ) ;
#50249 = CARTESIAN_POINT ( 'NONE',  ( -4.085715681792862597, -78.45259877965739292, 11.26174581117867390 ) ) ;
#50250 = AXIS2_PLACEMENT_3D ( 'NONE', #4736, #54334, #40150 ) ;
#50251 = CARTESIAN_POINT ( 'NONE',  ( 11.14115696400000033, -79.00685466694699244, -1.301050381412999890 ) ) ;
#50252 = CARTESIAN_POINT ( 'NONE',  ( 7.919595949288999570, -59.94999999969999749, 9.050966799188000067 ) ) ;
#50253 = EDGE_CURVE ( 'NONE', #49445, #46028, #9366, .T. ) ;
#50254 = VERTEX_POINT ( 'NONE', #4648 ) ;
#50255 = CARTESIAN_POINT ( 'NONE',  ( 7.624341764943999955, -60.06485149430999826, -10.42531124854999902 ) ) ;
#50256 = EDGE_LOOP ( 'NONE', ( #45366, #58255, #49153, #38536 ) ) ;
#50257 = CARTESIAN_POINT ( 'NONE',  ( 2.837648390166478407, -77.45036520058170026, 8.803880890672857618 ) ) ;
#50258 = CARTESIAN_POINT ( 'NONE',  ( 8.680753609988000719, -77.73315101347900224, 6.821192461343000168 ) ) ;
#50259 = DIRECTION ( 'NONE',  ( -0.7071067811865474617, -0.7071067811865474617, 4.786452749996315941E-09 ) ) ;
#50260 = CARTESIAN_POINT ( 'NONE',  ( -8.680270256945998852, -77.35715378293498645, 3.860428508128000313 ) ) ;
#50261 = VECTOR ( 'NONE', #39785, 1000.000000000000000 ) ;
#50262 = CYLINDRICAL_SURFACE ( 'NONE', #46430, 9.599999999999999645 ) ;
#50263 = CARTESIAN_POINT ( 'NONE',  ( -9.393203674808288994, -80.95833333333331439, 5.413904038987134015 ) ) ;
#50264 = CARTESIAN_POINT ( 'NONE',  ( 0.08338359222296000406, -79.39937596634999295, -1.538001148114999994 ) ) ;
#50265 = CARTESIAN_POINT ( 'NONE',  ( 7.117135278674999732, -80.31097582047098626, 8.718833803912000135 ) ) ;
#50266 = VECTOR ( 'NONE', #32325, 999.9999999999998863 ) ;
#50267 = CARTESIAN_POINT ( 'NONE',  ( -2.162167942093999873, -78.32001793044798887, 10.72440421974000024 ) ) ;
#50268 = CARTESIAN_POINT ( 'NONE',  ( 12.70451647738967793, -61.35458569080387292, 1.498866843944270943 ) ) ;
#50269 = CARTESIAN_POINT ( 'NONE',  ( -8.171144579303600608, -60.14010097497902052, 7.364280830346968010 ) ) ;
#50270 = CARTESIAN_POINT ( 'NONE',  ( 3.273752094640999921, -82.17775871403298993, -1.206383228866000135 ) ) ;
#50271 = ORIENTED_EDGE ( 'NONE', *, *, #36765, .T. ) ;
#50272 = CARTESIAN_POINT ( 'NONE',  ( 12.42775431196000113, -79.62100617581799611, -0.3754309351819000162 ) ) ;
#50273 = CARTESIAN_POINT ( 'NONE',  ( 7.200008815102000526, -76.32067638237299434, -8.806490984069000660 ) ) ;
#50274 = CARTESIAN_POINT ( 'NONE',  ( 9.600846333656411602, -77.88729592899156273, 4.835758510686050116 ) ) ;
#50275 = CARTESIAN_POINT ( 'NONE',  ( 11.95248949435000085, -78.88927060784799039, 0.8087524912306001124 ) ) ;
#50276 = CARTESIAN_POINT ( 'NONE',  ( -10.13402152809999990, -18.27694524397999842, 7.647754144029000223 ) ) ;
#50278 = DIRECTION ( 'NONE',  ( 0.000000000000000000, -1.000000000000000000, 4.107825191113000313E-14 ) ) ;
#50277 = CARTESIAN_POINT ( 'NONE',  ( -5.917523019358058356, -78.38333333333331154, -10.26699006316253282 ) ) ;
#50279 = CARTESIAN_POINT ( 'NONE',  ( -0.7620112687051859846, -2.857683719944371425, -3.439605056318825405 ) ) ;
#50280 = CARTESIAN_POINT ( 'NONE',  ( -5.190928442694000111, -77.50066704931698780, 7.852735600434000318 ) ) ;
#50281 = CARTESIAN_POINT ( 'NONE',  ( -5.936087459992990922, -85.94828564506399005, -4.882024132225906143 ) ) ;
#50282 = CARTESIAN_POINT ( 'NONE',  ( -3.610459473067000324, -77.29238470710198783, 10.54605058607999979 ) ) ;
#50283 = CARTESIAN_POINT ( 'NONE',  ( 8.135116633385999663, -76.96737925144761050, 9.200136113044999675 ) ) ;
#50284 = CARTESIAN_POINT ( 'NONE',  ( -10.71095089696999914, -80.41331365663170061, -3.064757027600999884 ) ) ;
#50285 = VERTEX_POINT ( 'NONE', #18232 ) ;
#50286 = PLANE ( 'NONE',  #53251 ) ;
#50287 = CARTESIAN_POINT ( 'NONE',  ( 8.838834764832000701, -23.25000000000000000, 8.838834764832000701 ) ) ;
#50288 = CARTESIAN_POINT ( 'NONE',  ( 11.08595418830999968, -76.93614735138400818, -1.708721840212999998 ) ) ;
#50289 = CARTESIAN_POINT ( 'NONE',  ( 7.788493169598000421, -78.62176246810599878, 7.733265204867000087 ) ) ;
#50290 = AXIS2_PLACEMENT_3D ( 'NONE', #40156, #49622, #22739 ) ;
#50291 = CARTESIAN_POINT ( 'NONE',  ( 8.958641849965999882, -25.20112647804999995, -8.950065109822000764 ) ) ;
#50292 = CARTESIAN_POINT ( 'NONE',  ( -7.648026766753000416, -60.05000000550000294, 10.12290050090999927 ) ) ;
#50293 = LINE ( 'NONE', #9846, #58138 ) ;
#50294 = CARTESIAN_POINT ( 'NONE',  ( -7.861037107713870320, -54.33338873116260004, -10.10708465676067114 ) ) ;
#50295 = EDGE_CURVE ( 'NONE', #45504, #52567, #50112, .T. ) ;
#50296 = CARTESIAN_POINT ( 'NONE',  ( 4.171543465321999378, -82.42742953870899214, -0.06563245401257999934 ) ) ;
#50297 = DIRECTION ( 'NONE',  ( -1.000000000000000000, 0.000000000000000000, 0.000000000000000000 ) ) ;
#50298 = EDGE_CURVE ( 'NONE', #22076, #12876, #4935, .T. ) ;
#50299 = VECTOR ( 'NONE', #27724, 1000.000000000000114 ) ;
#50300 = DIRECTION ( 'NONE',  ( 0.000000000000000000, 0.000000000000000000, 1.000000000000000000 ) ) ;
#50301 = B_SPLINE_SURFACE_WITH_KNOTS ( 'NONE', 3, 3, ( 
 ( #3804, #21808, #40106, #39810 ),
 ( #38951, #49272, #39529, #30075 ),
 ( #30939, #53701, #13237, #22092 ),
 ( #7944, #48125, #25372, #7658 ),
 ( #2946, #58119, #57825, #4095 ),
 ( #53114, #17681, #31231, #17382 ),
 ( #12941, #16815, #12661, #43387 ),
 ( #20946, #35369, #43970, #12094 ) ),
 .UNSPECIFIED., .F., .F., .F.,
 ( 4, 1, 1, 1, 1, 4 ),
 ( 4, 4 ),
 ( -0.01200407345746999990, 0.000000000000000000, 0.3333333333333000081, 0.6666666666667000474, 1.000000000000000000, 1.011997855551999947 ),
 ( -0.3559705542741999906, 1.355970554273999928 ),
 .UNSPECIFIED. ) ;
#50302 = CARTESIAN_POINT ( 'NONE',  ( -4.550163292746999488, -77.36849323694099212, -10.30194052436999996 ) ) ;
#50303 = CARTESIAN_POINT ( 'NONE',  ( -1.445929428138999828, -80.22903271044999940, 0.8273736140038000508 ) ) ;
#50304 = CARTESIAN_POINT ( 'NONE',  ( 1.316947385243999902, -78.27548044020998930, 0.09125597792054998547 ) ) ;
#50305 = CARTESIAN_POINT ( 'NONE',  ( -7.655984445823650120, -23.70337239445911237, 10.06694410249481031 ) ) ;
#50306 = CARTESIAN_POINT ( 'NONE',  ( 1.364940739897916533, -81.96454802580129240, -0.6510407284856819521 ) ) ;
#50307 = CARTESIAN_POINT ( 'NONE',  ( 1.424284261262790618, -83.12670472999310789, 0.5112557424970984865 ) ) ;
#50308 = CARTESIAN_POINT ( 'NONE',  ( -7.202660771834071163, -80.16699785840980041, -7.981660149312156172 ) ) ;
#50309 = CARTESIAN_POINT ( 'NONE',  ( -1.980532758766000212, -19.23743349341999931, -12.80088938805999987 ) ) ;
#50310 = VECTOR ( 'NONE', #55508, 1000.000000000000114 ) ;
#50311 = ORIENTED_EDGE ( 'NONE', *, *, #53886, .F. ) ;
#50312 = CIRCLE ( 'NONE', #36967, 9.700000000000001066 ) ;
#50313 = CARTESIAN_POINT ( 'NONE',  ( -1.184527705118542107, -81.62653070104380504, -0.4082925468394342783 ) ) ;
#50314 = CARTESIAN_POINT ( 'NONE',  ( 0.000000000000000000, 0.000000000000000000, 0.000000000000000000 ) ) ;
#50315 = CARTESIAN_POINT ( 'NONE',  ( -8.926133614190998600, -79.84003032942598566, 6.676731181684000482 ) ) ;
#50316 = CARTESIAN_POINT ( 'NONE',  ( -1.250000000000000000, -80.00000000000000000, 0.000000000000000000 ) ) ;
#50317 = EDGE_LOOP ( 'NONE', ( #6530, #50650, #15229, #22300 ) ) ;
#50318 = ORIENTED_EDGE ( 'NONE', *, *, #16182, .F. ) ;
#50319 = CARTESIAN_POINT ( 'NONE',  ( -0.05736323927548000329, -80.72446476122699721, -1.416633329004000075 ) ) ;
#50320 = ORIENTED_EDGE ( 'NONE', *, *, #18845, .F. ) ;
#50321 = EDGE_LOOP ( 'NONE', ( #54523, #3533, #38735 ) ) ;
#50322 = DIRECTION ( 'NONE',  ( 0.000000000000000000, 0.000000000000000000, 1.000000000000000000 ) ) ;
#50323 = FACE_OUTER_BOUND ( 'NONE', #16410, .T. ) ;
#50324 = CARTESIAN_POINT ( 'NONE',  ( 0.05530789208431366455, -81.32083332030849476, 3.442645786192767510 ) ) ;
#50325 = CARTESIAN_POINT ( 'NONE',  ( 4.312078000770541486, -78.26364788450446497, -8.189147600941369731 ) ) ;
#50326 = CARTESIAN_POINT ( 'NONE',  ( -9.393203674808267678, -78.04166666666665719, -5.413904038987171319 ) ) ;
#50327 = ADVANCED_FACE ( 'NONE', ( #17631, #22047 ), #48930, .T. ) ;
#50328 = EDGE_LOOP ( 'NONE', ( #57475, #20738, #2888, #5367 ) ) ;
#50329 = EDGE_LOOP ( 'NONE', ( #56080, #9347, #33873, #2672 ) ) ;
#50330 = CARTESIAN_POINT ( 'NONE',  ( -12.54238271617935041, -18.47146427654275413, -1.749799002659384817 ) ) ;
#50331 = DIRECTION ( 'NONE',  ( -1.000000000000000000, 0.000000000000000000, 0.000000000000000000 ) ) ;
#50332 = EDGE_CURVE ( 'NONE', #48890, #21042, #5734, .T. ) ;
#50333 = PRODUCT_DEFINITION_SHAPE ( 'NONE', 'NONE',  #58413 ) ;
#50334 = LINE ( 'NONE', #18740, #17275 ) ;
#50335 = CARTESIAN_POINT ( 'NONE',  ( 8.444976262095000408, -78.00053605066298701, 4.780490068936999570 ) ) ;
#50336 = DIRECTION ( 'NONE',  ( 0.000000000000000000, 1.000000000000000000, 0.000000000000000000 ) ) ;
#50337 = CARTESIAN_POINT ( 'NONE',  ( 3.513385375869528371, -85.82276001101435270, 1.485411387532208582 ) ) ;
#50338 = CARTESIAN_POINT ( 'NONE',  ( -9.082935096011000908, -76.89367046626000501, -9.017176053435999705 ) ) ;
#50339 = CARTESIAN_POINT ( 'NONE',  ( -0.2566745418018999692, -79.47023290324000300, 1.326684981396999863 ) ) ;
#50340 = CARTESIAN_POINT ( 'NONE',  ( -12.87022657272000004, -22.78485473281999774, -2.062597299672999540 ) ) ;
#50341 = CARTESIAN_POINT ( 'NONE',  ( -9.369164850722000892, -60.04999999966999980, -7.601397897754999633 ) ) ;
#50342 = CARTESIAN_POINT ( 'NONE',  ( -8.187117628376695322, -76.63618780861736468, 8.428237639695421279 ) ) ;
#50343 = CARTESIAN_POINT ( 'NONE',  ( -0.06104599752768998661, -79.88498827328399443, 4.174432124594999571 ) ) ;
#50344 = CARTESIAN_POINT ( 'NONE',  ( -6.474781754604000739, -80.34238059820370381, -9.218806710208998112 ) ) ;
#50345 = CARTESIAN_POINT ( 'NONE',  ( 8.283364115789000337, -78.80173667140100235, 5.234906771447999319 ) ) ;
#50346 = CLOSED_SHELL ( 'NONE', ( #37665, #5883, #42105, #23762, #15256, #14075, #43788, #1914, #13204, #38228, #43812 ) ) ;
#50347 = CARTESIAN_POINT ( 'NONE',  ( 3.250000000000000000, -2.850000000000000089, 0.000000000000000000 ) ) ;
#50348 = CARTESIAN_POINT ( 'NONE',  ( -1.250000000000000000, -23.25000000000000000, 12.00000000000000000 ) ) ;
#50349 = VECTOR ( 'NONE', #19195, 1000.000000000000000 ) ;
#50350 = CARTESIAN_POINT ( 'NONE',  ( -0.6568659331174000471, -78.18164379163989963, 1.160647793301999853 ) ) ;
#50351 = EDGE_CURVE ( 'NONE', #16006, #41301, #13258, .T. ) ;
#50352 = DIRECTION ( 'NONE',  ( 1.000000000000000000, 0.000000000000000000, 0.000000000000000000 ) ) ;
#50353 = CARTESIAN_POINT ( 'NONE',  ( 8.275552136666096459, -79.99999999999998579, -4.772006449322993227 ) ) ;
#50354 = CARTESIAN_POINT ( 'NONE',  ( 3.702420020526000055, -2.585946431073999907, 0.8821385418971999792 ) ) ;
#50355 = CARTESIAN_POINT ( 'NONE',  ( 10.65482429239385098, -77.19999999999998863, -1.623674524292790133 ) ) ;
#50356 = ORIENTED_EDGE ( 'NONE', *, *, #48364, .F. ) ;
#50357 = CARTESIAN_POINT ( 'NONE',  ( 2.879226727952094222, -78.34583333333331723, -10.71369944335146940 ) ) ;
#50358 = CARTESIAN_POINT ( 'NONE',  ( 0.000000000000000000, -86.29999999996098836, 0.000000000000000000 ) ) ;
#50359 = PLANE ( 'NONE',  #45662 ) ;
#50360 = CARTESIAN_POINT ( 'NONE',  ( 2.064412114960999745, -79.47116171449498268, -9.530377264972001328 ) ) ;
#50361 = CARTESIAN_POINT ( 'NONE',  ( 12.56884868898000107, -76.67718304534999163, -3.366471670097000324 ) ) ;
#50362 = CARTESIAN_POINT ( 'NONE',  ( -6.382001649558278089, -79.52561732951967599, 8.650654035762535443 ) ) ;
#50363 = DIRECTION ( 'NONE',  ( 0.000000000000000000, 1.000000000000000000, -4.137348672605999941E-14 ) ) ;
#50364 = CARTESIAN_POINT ( 'NONE',  ( 9.728739490418719882, -78.49536251359755568, 6.586777397229446329 ) ) ;
#50365 = ORIENTED_EDGE ( 'NONE', *, *, #27540, .F. ) ;
#50366 = EDGE_CURVE ( 'NONE', #17800, #55505, #32646, .T. ) ;
#50367 = DIRECTION ( 'NONE',  ( 0.000000000000000000, 0.000000000000000000, -1.000000000000000000 ) ) ;
#50368 = CARTESIAN_POINT ( 'NONE',  ( 5.517529752410999855, -77.13936266505909600, 9.309542203537999328 ) ) ;
#50369 = AXIS2_PLACEMENT_3D ( 'NONE', #29811, #2693, #48150 ) ;
#50370 = CARTESIAN_POINT ( 'NONE',  ( -4.514525519966182010, -76.29316198124988091, -10.84781437541200155 ) ) ;
#50371 = CARTESIAN_POINT ( 'NONE',  ( 0.6269351409810999254, -82.19352514059698933, 1.369619292736000027 ) ) ;
#50372 = CARTESIAN_POINT ( 'NONE',  ( -1.704789469148189296, -18.29653838474041549, 12.53199752960649072 ) ) ;
#50373 = CARTESIAN_POINT ( 'NONE',  ( 7.184025905720999639, -77.71490363863499340, -6.082841960620999799 ) ) ;
#50375 = CARTESIAN_POINT ( 'NONE',  ( -0.1204595238885999980, -0.6604060260386999115, 3.497926457646999943 ) ) ;
#50374 = CARTESIAN_POINT ( 'NONE',  ( 2.998969658540000083, -83.58068022547898579, -2.839840568714000035 ) ) ;
#50376 = CARTESIAN_POINT ( 'NONE',  ( 9.539544502573999551, -79.38455194988500807, 0.5400218831817999998 ) ) ;
#50377 = DIRECTION ( 'NONE',  ( 0.000000000000000000, 0.000000000000000000, -1.000000000000000000 ) ) ;
#50378 = CARTESIAN_POINT ( 'NONE',  ( -0.2944660333051000167, -79.55096993136200467, 1.286023070983999927 ) ) ;
#50379 = EDGE_LOOP ( 'NONE', ( #38212, #12689, #31351, #56119 ) ) ;
#50380 = CARTESIAN_POINT ( 'NONE',  ( -5.993167237703258543, -77.17810086631732247, -8.925825369205432125 ) ) ;
#50381 = CARTESIAN_POINT ( 'NONE',  ( 1.500000000000001110, -79.13958333333334849, -0.1963495408493590721 ) ) ;
#50382 = CARTESIAN_POINT ( 'NONE',  ( -3.778552491321000240, -78.99318692756679638, -1.585466545969598184E-14 ) ) ;
#50383 = VERTEX_POINT ( 'NONE', #54818 ) ;
#50384 = EDGE_LOOP ( 'NONE', ( #746, #56332, #45764 ) ) ;
#50385 = CARTESIAN_POINT ( 'NONE',  ( 11.43764105185000091, -79.97007275658970116, 2.691257544168000226 ) ) ;
#50386 = VECTOR ( 'NONE', #55374, 1000.000000000000114 ) ;
#50387 =( NAMED_UNIT ( * ) PLANE_ANGLE_UNIT ( ) SI_UNIT ( $, .RADIAN. ) );
#50388 = DIRECTION ( 'NONE',  ( -1.000000000000000000, 0.000000000000000000, 0.000000000000000000 ) ) ;
#50389 = ORIENTED_EDGE ( 'NONE', *, *, #25804, .T. ) ;
#50390 = CARTESIAN_POINT ( 'NONE',  ( -8.607099856842999941, -77.75282292035799969, -8.432888219828999610 ) ) ;
#50391 = EDGE_LOOP ( 'NONE', ( #50837, #11794, #19456, #4466, #27759, #54195 ) ) ;
#50392 = VERTEX_POINT ( 'NONE', #19980 ) ;
#50393 = CARTESIAN_POINT ( 'NONE',  ( -2.089133851730829328, -2.669960546984883276, -2.490096624221278088 ) ) ;
#50394 = VERTEX_POINT ( 'NONE', #24101 ) ;
#50395 = CARTESIAN_POINT ( 'NONE',  ( -0.05187192650483000295, -79.80967046134098553, 3.547093095958999687 ) ) ;
#50396 = CARTESIAN_POINT ( 'NONE',  ( 0.000000000000000000, -2.949999999935999817, -12.84999999993999964 ) ) ;
#50397 = VERTEX_POINT ( 'NONE', #15539 ) ;
#50398 = DIRECTION ( 'NONE',  ( 0.000000000000000000, 1.000000000000000000, 0.000000000000000000 ) ) ;
#50399 = EDGE_LOOP ( 'NONE', ( #18220, #40703, #11902, #25827, #14995 ) ) ;
#50400 = DIRECTION ( 'NONE',  ( -0.9957542233426791567, 0.04890176637352901257, -0.07798810127683841742 ) ) ;
#50401 = CARTESIAN_POINT ( 'NONE',  ( 7.658986946679876340, -78.65252498771793910, 5.959341133100068966 ) ) ;
#50402 = CARTESIAN_POINT ( 'NONE',  ( -11.78092668186225644, -79.79999999999998295, -2.153435279904234889 ) ) ;
#50403 = DIRECTION ( 'NONE',  ( 0.000000000000000000, -1.000000000000000000, 0.000000000000000000 ) ) ;
#50404 = CARTESIAN_POINT ( 'NONE',  ( -10.07624512687999996, -76.30181786998500115, -4.852130239470000106 ) ) ;
#50405 = DIRECTION ( 'NONE',  ( 0.000000000000000000, 0.000000000000000000, -1.000000000000000000 ) ) ;
#50406 = CARTESIAN_POINT ( 'NONE',  ( 12.50000000000000000, -23.24999999688999708, 1.750000000000000000 ) ) ;
#50407 = VECTOR ( 'NONE', #34771, 1000.000000000000000 ) ;
#50408 = CARTESIAN_POINT ( 'NONE',  ( 11.11267589788999999, -76.58485902790600619, 1.610019623660999821 ) ) ;
#50409 = CARTESIAN_POINT ( 'NONE',  ( -1.793454718549643445, -78.70954372627176099, -9.074418929172219705 ) ) ;
#50410 = CARTESIAN_POINT ( 'NONE',  ( 7.011029437969999556, -77.81601167140100017, 6.440258933668999930 ) ) ;
#50411 = DIRECTION ( 'NONE',  ( -0.7071067811865475727, 0.000000000000000000, 0.7071067811865475727 ) ) ;
#50412 = CARTESIAN_POINT ( 'NONE',  ( -9.331000443659689836, -80.14465528251990634, -5.825445497097998526 ) ) ;
#50413 = CARTESIAN_POINT ( 'NONE',  ( -3.100723057438616426, -78.05736609856147368, -11.66987326451405416 ) ) ;
#50414 = CARTESIAN_POINT ( 'NONE',  ( 3.894733971054000321, -80.84267549782599360, 1.374609327336000053 ) ) ;
#50415 = CARTESIAN_POINT ( 'NONE',  ( -12.59682398758999966, -18.61262488659000169, 1.801644812721000077 ) ) ;
#50416 = EDGE_CURVE ( 'NONE', #54024, #11618, #35900, .T. ) ;
#50417 = CARTESIAN_POINT ( 'NONE',  ( 1.407171709420440342, -79.63541666666665719, -10.74999999999999822 ) ) ;
#50418 = LINE ( 'NONE', #41254, #28289 ) ;
#50419 = CARTESIAN_POINT ( 'NONE',  ( 11.05000000000000071, -76.00000000000000000, 0.000000000000000000 ) ) ;
#50420 = CARTESIAN_POINT ( 'NONE',  ( 0.4526505179569237369, -81.90290258620123609, -1.245472627785131126 ) ) ;
#50421 = CARTESIAN_POINT ( 'NONE',  ( 0.000000000000000000, -76.00000000000000000, 0.000000000000000000 ) ) ;
#50422 = CARTESIAN_POINT ( 'NONE',  ( -17.50000000000000000, -13.07071424677999971, -2.007265881287999855E-13 ) ) ;
#50423 = AXIS2_PLACEMENT_3D ( 'NONE', #43542, #48556, #3107 ) ;
#50424 = CARTESIAN_POINT ( 'NONE',  ( 5.683913069336140822, -79.77753931263904974, -7.396130091655648719 ) ) ;
#50425 = CARTESIAN_POINT ( 'NONE',  ( -2.099388381696000023E-14, -0.04999999937963000435, 0.000000000000000000 ) ) ;
#50426 = CARTESIAN_POINT ( 'NONE',  ( -1.044910384896000188, -25.05526494194999643, -12.77260826199000121 ) ) ;
#50427 = DIRECTION ( 'NONE',  ( 0.000000000000000000, -1.000000000000000000, 0.000000000000000000 ) ) ;
#50428 = LINE ( 'NONE', #15269, #41821 ) ;
#50429 = CARTESIAN_POINT ( 'NONE',  ( 0.9781264271459000348, -53.85968856090000401, -12.65967462873999949 ) ) ;
#50430 = CARTESIAN_POINT ( 'NONE',  ( -7.722615280105806335, -77.38904062276650109, 7.510299681650742798 ) ) ;
#50431 = DIRECTION ( 'NONE',  ( 0.000000000000000000, -1.000000000000000000, 0.000000000000000000 ) ) ;
#50433 = CARTESIAN_POINT ( 'NONE',  ( -1.500872881732000064, -78.86402008970900113, -0.2152271930174000092 ) ) ;
#50432 = CARTESIAN_POINT ( 'NONE',  ( 1.460959015002472494, -79.67083333333336270, 0.3926218265389232465 ) ) ;
#50434 = CARTESIAN_POINT ( 'NONE',  ( 9.195259559916998171, -76.94960844227999530, -7.805988517003000560 ) ) ;
#50435 = ORIENTED_EDGE ( 'NONE', *, *, #50023, .F. ) ;
#50436 = EDGE_CURVE ( 'NONE', #49641, #4635, #42325, .T. ) ;
#50437 = CARTESIAN_POINT ( 'NONE',  ( -0.6762769136191999486, -84.55857450217399673, 3.525108090257000004 ) ) ;
#50438 = CARTESIAN_POINT ( 'NONE',  ( 10.51638713295000116, -81.05822150553019867, 4.415123262547999694 ) ) ;
#50439 = CARTESIAN_POINT ( 'NONE',  ( 8.847929224218546551, -78.32657344890409945, -2.698424406155022659 ) ) ;
#50440 = CARTESIAN_POINT ( 'NONE',  ( 3.242204976606303912, -85.36770834133103847, -1.159067530704637194 ) ) ;
#50441 = CARTESIAN_POINT ( 'NONE',  ( -10.96060824219999930, -77.38464009822899925, 2.383941600041999731 ) ) ;
#50442 = CARTESIAN_POINT ( 'NONE',  ( 12.54901566175999861, -53.79264670667999582, -0.4731578885121000555 ) ) ;
#50443 = DIRECTION ( 'NONE',  ( 1.000000000000000000, 0.000000000000000000, 0.000000000000000000 ) ) ;
#50444 = FACE_OUTER_BOUND ( 'NONE', #37592, .T. ) ;
#50445 = CARTESIAN_POINT ( 'NONE',  ( -0.5536397579754658294, -76.42123714547000191, -11.80639474213326601 ) ) ;
#50446 = CARTESIAN_POINT ( 'NONE',  ( -5.624774363530229415, -76.99999999999998579, 7.347433795508993448 ) ) ;
#50447 = ORIENTED_EDGE ( 'NONE', *, *, #56786, .T. ) ;
#50448 = DIRECTION ( 'NONE',  ( 1.000000000000000000, 0.000000000000000000, 0.000000000000000000 ) ) ;
#50449 = PLANE ( 'NONE',  #44504 ) ;
#50450 = CARTESIAN_POINT ( 'NONE',  ( 9.290732676231000298, -79.36633998579799254, -1.531409331864000078 ) ) ;
#50451 = DIRECTION ( 'NONE',  ( 0.000000000000000000, 0.000000000000000000, -1.000000000000000000 ) ) ;
#50452 = EDGE_CURVE ( 'NONE', #393, #28471, #55728, .T. ) ;
#50453 = ORIENTED_EDGE ( 'NONE', *, *, #18945, .F. ) ;
#50454 = CARTESIAN_POINT ( 'NONE',  ( -1.750000000000000000, -67.52659999995799467, 0.000000000000000000 ) ) ;
#50455 = CONICAL_SURFACE ( 'NONE', #43834, 9.334374999970000530, 0.7853981633972997312 ) ;
#50456 = DIRECTION ( 'NONE',  ( 1.000000000000000000, 0.000000000000000000, 0.000000000000000000 ) ) ;
#50457 = VERTEX_POINT ( 'NONE', #24401 ) ;
#50458 = CARTESIAN_POINT ( 'NONE',  ( 3.330893700617000075, -78.97344966613400175, -11.81951464247000061 ) ) ;
#50459 = CARTESIAN_POINT ( 'NONE',  ( 9.361729212764000607, -77.35447091705098899, 6.367909160671999302 ) ) ;
#50460 = AXIS2_PLACEMENT_3D ( 'NONE', #48427, #30391, #35388 ) ;
#50461 = CARTESIAN_POINT ( 'NONE',  ( 8.803747447747934274, -62.01568152305735993, -9.164340453748428317 ) ) ;
#50462 = ORIENTED_EDGE ( 'NONE', *, *, #4364, .F. ) ;
#50463 = DIRECTION ( 'NONE',  ( 0.000000000000000000, -1.000000000000000000, 0.000000000000000000 ) ) ;
#50464 = CIRCLE ( 'NONE', #1460, 12.50000000000000000 ) ;
#50465 = CARTESIAN_POINT ( 'NONE',  ( 8.193575559979001000, -79.12595488940898747, 5.316613930189999948 ) ) ;
#50466 = ORIENTED_EDGE ( 'NONE', *, *, #53848, .T. ) ;
#50467 = CARTESIAN_POINT ( 'NONE',  ( 12.82202470518000048, -55.37373556845999900, 2.066041976111999467 ) ) ;
#50468 = DIRECTION ( 'NONE',  ( 0.000000000000000000, -1.000000000000000000, -1.327216516273000122E-14 ) ) ;
#50469 = CARTESIAN_POINT ( 'NONE',  ( -12.54901606605999831, -25.00731603500000233, -0.4733145588205000531 ) ) ;
#50470 = EDGE_CURVE ( 'NONE', #53803, #46485, #37967, .T. ) ;
#50471 = CARTESIAN_POINT ( 'NONE',  ( -7.264520526674999701, -77.68572694988499450, -6.114261184555999762 ) ) ;
#50472 = CARTESIAN_POINT ( 'NONE',  ( -1.249805685293928548, -80.10851784185619806, -0.1286959038651522835 ) ) ;
#50473 = CARTESIAN_POINT ( 'NONE',  ( -1.003693375988829573, -17.03776007889603861, -12.70247752664623242 ) ) ;
#50474 = CARTESIAN_POINT ( 'NONE',  ( 10.48543666025110710, -79.00833333333332575, -6.043427764450776785 ) ) ;
#50475 = FACE_OUTER_BOUND ( 'NONE', #27283, .T. ) ;
#50476 = CARTESIAN_POINT ( 'NONE',  ( -0.2142199289669327877, -78.96319708694683470, -1.521292673437905529 ) ) ;
#50477 = CARTESIAN_POINT ( 'NONE',  ( -1.685420276471391254, -80.47291666538409061, -3.684289950626761012 ) ) ;
#50478 = ORIENTED_EDGE ( 'NONE', *, *, #58241, .F. ) ;
#50479 = DIRECTION ( 'NONE',  ( -1.000000000000000000, 0.000000000000000000, 0.000000000000000000 ) ) ;
#50480 = CARTESIAN_POINT ( 'NONE',  ( -7.450482419345999752, -76.05593601512001101, -9.799277032148999922 ) ) ;
#50481 = CARTESIAN_POINT ( 'NONE',  ( -0.6747260877994001316, -82.22962677363800310, -1.052256958371999840 ) ) ;
#50482 = B_SPLINE_SURFACE_WITH_KNOTS ( 'NONE', 3, 3, ( 
 ( #57487, #39485, #25325, #25040 ),
 ( #56635, #8190, #21759, #35032 ),
 ( #43062, #16480, #38618, #39765 ),
 ( #44209, #52778, #30612, #25901 ),
 ( #2621, #43343, #25613, #57778 ),
 ( #3759, #48360, #57202, #34750 ),
 ( #43925, #39187, #16770, #16194 ),
 ( #21478, #17051, #29740, #53066 ),
 ( #12332, #56922, #48646, #34171 ),
 ( #17333, #35321, #11485, #29456 ),
 ( #30320, #47513, #2899, #52207 ),
 ( #11763, #47792, #20900, #38903 ),
 ( #34460, #52491, #12048, #30029 ),
 ( #48082, #7613, #43634, #3196 ),
 ( #21186, #13488, #40950, #22939 ),
 ( #49223, #4345, #58368, #45686 ),
 ( #40658, #12897, #31778, #8772 ) ),
 .UNSPECIFIED., .F., .F., .F.,
 ( 4, 1, 1, 1, 1, 1, 1, 1, 1, 1, 1, 1, 1, 1, 4 ),
 ( 4, 4 ),
 ( -0.01011837001259000002, 0.000000000000000000, 0.08333333333333001192, 0.1666666666667000196, 0.2500000000000000000, 0.3333333333333000081, 0.4166666666666999919, 0.5000000000000000000, 0.5833333333333000637, 0.6666666666667000474, 0.7500000000000000000, 0.8333333333333000637, 0.9166666666667000474, 1.000000000000000000, 1.010372850415000023 ),
 ( -0.3559705548695000221, 1.357613361088000126 ),
 .UNSPECIFIED. ) ;
#50483 = CARTESIAN_POINT ( 'NONE',  ( -0.2035211792613734194, -2.228899868708034582, 3.513002120467708433 ) ) ;
#50484 = DIRECTION ( 'NONE',  ( 0.000000000000000000, 0.000000000000000000, -1.000000000000000000 ) ) ;
#50485 = CARTESIAN_POINT ( 'NONE',  ( -3.911342194028000208, -78.61650197717000310, -11.62327352135999980 ) ) ;
#50486 = CARTESIAN_POINT ( 'NONE',  ( -10.85634995915000012, -76.17260508320899248, -5.741293403527000017 ) ) ;
#50487 = CARTESIAN_POINT ( 'NONE',  ( -3.647699722740957995, -86.02148118236289065, 1.624060551956000520 ) ) ;
#50488 = CARTESIAN_POINT ( 'NONE',  ( 3.064790515199006471, -2.824239762174677537, -1.081059584728839562 ) ) ;
#50489 = CARTESIAN_POINT ( 'NONE',  ( -3.836625960323930773, -77.14921398509360984, -11.44188731050598129 ) ) ;
#50490 = CIRCLE ( 'NONE', #46714, 13.86363636363999952 ) ;
#50491 = ORIENTED_EDGE ( 'NONE', *, *, #30847, .T. ) ;
#50492 = CARTESIAN_POINT ( 'NONE',  ( 1.281517705925000028, -82.29565794024999548, 0.4285832374949000156 ) ) ;
#50493 = AXIS2_PLACEMENT_3D ( 'NONE', #34622, #8059, #44079 ) ;
#50494 = CARTESIAN_POINT ( 'NONE',  ( 9.705842814688999454, -77.07780893925938415, -0.1680204891633000075 ) ) ;
#50495 = CARTESIAN_POINT ( 'NONE',  ( -9.372147444698367025, -77.17635552105011243, -0.1981913680696959501 ) ) ;
#50496 = LINE ( 'NONE', #28032, #9797 ) ;
#50497 = CARTESIAN_POINT ( 'NONE',  ( 3.145445771509000288, -2.093880151312000226, 2.255325989060000147 ) ) ;
#50498 = CARTESIAN_POINT ( 'NONE',  ( 11.77424395174999994, -78.27591218578899657, 2.561825723684000078 ) ) ;
#50499 = CARTESIAN_POINT ( 'NONE',  ( -5.120069445942999842, -77.28733258133598838, -8.157089945504001349 ) ) ;
#50500 = CARTESIAN_POINT ( 'NONE',  ( 4.500613759774078737, -76.04318847295724026, 10.85354368999166574 ) ) ;
#50501 = CARTESIAN_POINT ( 'NONE',  ( 5.768362037549999322, -78.62764927275399884, -9.403610972502001175 ) ) ;
#50502 = CARTESIAN_POINT ( 'NONE',  ( -0.4924802140958408625, -85.94828564506400426, 3.960641768741219870 ) ) ;
#50503 = ORIENTED_EDGE ( 'NONE', *, *, #54978, .F. ) ;
#50504 = ADVANCED_FACE ( 'NONE', ( #55993 ), #33535, .T. ) ;
#50505 = CARTESIAN_POINT ( 'NONE',  ( 10.75000000000000000, -79.25000000000000000, 0.000000000000000000 ) ) ;
#50506 = CARTESIAN_POINT ( 'NONE',  ( 2.241317775079999741, -79.89861982803429896, -11.94785552921999994 ) ) ;
#50507 = DIRECTION ( 'NONE',  ( 0.000000000000000000, -1.000000000000000000, 0.000000000000000000 ) ) ;
#50508 = EDGE_CURVE ( 'NONE', #17378, #48346, #23806, .T. ) ;
#50509 = CARTESIAN_POINT ( 'NONE',  ( -10.13785388426000011, -78.52174770179199470, -4.205702700205000255 ) ) ;
#50510 = DIRECTION ( 'NONE',  ( 0.000000000000000000, -1.000000000000000000, 0.000000000000000000 ) ) ;
#50511 = CARTESIAN_POINT ( 'NONE',  ( 12.50657384761460378, -17.02752583206956416, -0.3552644805215970925 ) ) ;
#50512 = CARTESIAN_POINT ( 'NONE',  ( -11.99999999979999821, -18.85000000927000130, -0.7999999997951999786 ) ) ;
#50513 = CARTESIAN_POINT ( 'NONE',  ( 7.646091287767998956, -18.29149945126999910, -10.13691902392999999 ) ) ;
#50514 = CARTESIAN_POINT ( 'NONE',  ( -9.369164850722000892, -55.54999999966999980, 7.601397897754999633 ) ) ;
#50515 = ORIENTED_EDGE ( 'NONE', *, *, #3561, .T. ) ;
#50516 = CARTESIAN_POINT ( 'NONE',  ( -9.744524944696001612, -79.24921224881200033, -5.412839751281999234 ) ) ;
#50517 = CARTESIAN_POINT ( 'NONE',  ( 12.70253230845987957, -53.82944272757063686, 0.9891673677798649145 ) ) ;
#50518 = CARTESIAN_POINT ( 'NONE',  ( 12.50745077485999879, -53.80005551680000053, -2.012158279073999839E-09 ) ) ;
#50519 = CARTESIAN_POINT ( 'NONE',  ( -7.396362990145566307, -77.02553451721301769, -9.545941378553289169 ) ) ;
#50521 = CARTESIAN_POINT ( 'NONE',  ( -1.200102204978513942, -81.57785406893258084, 0.3492695309771673418 ) ) ;
#50520 = CARTESIAN_POINT ( 'NONE',  ( -0.1174688447357000037, -81.27596268276600711, -1.314064945473999879 ) ) ;
#50522 = EDGE_CURVE ( 'NONE', #21905, #37950, #29107, .T. ) ;
#50523 = CARTESIAN_POINT ( 'NONE',  ( -9.330562018306766348, -76.99999999999997158, -0.3894759657577204215 ) ) ;
#50524 = CARTESIAN_POINT ( 'NONE',  ( 0.000000000000000000, -72.89999999999999147, 0.000000000000000000 ) ) ;
#50525 = CARTESIAN_POINT ( 'NONE',  ( -0.1375932915944000079, -78.96341176948999419, 1.300711684584999972 ) ) ;
#50526 = CARTESIAN_POINT ( 'NONE',  ( 8.082524092276875294, -79.79166666666665719, 4.658475568430836766 ) ) ;
#50527 = CARTESIAN_POINT ( 'NONE',  ( 10.85747675193891304, -79.21179631784005437, 1.607176855388187331 ) ) ;
#50528 = AXIS2_PLACEMENT_3D ( 'NONE', #20945, #8517, #3801 ) ;
#50529 = CARTESIAN_POINT ( 'NONE',  ( -12.50485692592790166, -61.66593462659078995, 0.6924071803398014202 ) ) ;
#50530 = ORIENTED_EDGE ( 'NONE', *, *, #6764, .F. ) ;
#50531 = ORIENTED_EDGE ( 'NONE', *, *, #48818, .F. ) ;
#50532 = CARTESIAN_POINT ( 'NONE',  ( -5.941820572504999731, -78.80483998579799731, 8.071079272148001138 ) ) ;
#50533 = CARTESIAN_POINT ( 'NONE',  ( 6.286256452161005370, -78.77486376296185711, -8.720713732654903794 ) ) ;
#50534 = VERTEX_POINT ( 'NONE', #33237 ) ;
#50535 = EDGE_CURVE ( 'NONE', #56968, #24330, #21770, .T. ) ;
#50536 = LINE ( 'NONE', #13622, #21767 ) ;
#50537 = CARTESIAN_POINT ( 'NONE',  ( -3.418851969608866170, -83.17083334817002083, 0.4151850122235886120 ) ) ;
#50538 = AXIS2_PLACEMENT_3D ( 'NONE', #13243, #44256, #26819 ) ;
#50539 = CARTESIAN_POINT ( 'NONE',  ( 10.01676216528999852, -60.00941514989000325, 7.658899892539000831 ) ) ;
#50540 = CARTESIAN_POINT ( 'NONE',  ( -7.725782153457552148, -76.47895244894142763, 9.441631877404960349 ) ) ;
#50541 = AXIS2_PLACEMENT_3D ( 'NONE', #44424, #3975, #58002 ) ;
#50542 = CARTESIAN_POINT ( 'NONE',  ( 10.46948686332650169, -77.34029684728238863, 5.823215396550667222 ) ) ;
#50543 = CARTESIAN_POINT ( 'NONE',  ( -10.39759693597000023, -79.86449716727609882, -4.208097972746998927 ) ) ;
#50544 = ORIENTED_EDGE ( 'NONE', *, *, #40012, .T. ) ;
#50545 = FACE_OUTER_BOUND ( 'NONE', #52898, .T. ) ;
#50546 = ORIENTED_EDGE ( 'NONE', *, *, #4068, .T. ) ;
#50547 = CARTESIAN_POINT ( 'NONE',  ( 9.249208706614014730, -77.35106389758399814, 0.1238019141922536842 ) ) ;
#50548 = CARTESIAN_POINT ( 'NONE',  ( 1.160587285869999929, -77.73646750513898951, 10.97894289003999901 ) ) ;
#50549 = CARTESIAN_POINT ( 'NONE',  ( 1.500000000000000000, -77.76041666666668561, 0.1963495408493652339 ) ) ;
#50550 = ADVANCED_FACE ( 'NONE', ( #10536, #9952 ), #10835, .T. ) ;
#50551 = CARTESIAN_POINT ( 'NONE',  ( 1.487026788147999934, -77.52769675770798585, -9.589549613196998834 ) ) ;
#50552 = CARTESIAN_POINT ( 'NONE',  ( 12.00000000000000000, -77.64999999999999147, 0.000000000000000000 ) ) ;
#50553 = CARTESIAN_POINT ( 'NONE',  ( 0.000000000000000000, -75.67500000000001137, 0.000000000000000000 ) ) ;
#50554 = CARTESIAN_POINT ( 'NONE',  ( -1.578837173282999995, -79.31010810413999934, 0.3948290484592000271 ) ) ;
#50555 = CARTESIAN_POINT ( 'NONE',  ( 3.837589708125999977, -82.37257046129099081, -1.636761355292999820 ) ) ;
#50556 = CARTESIAN_POINT ( 'NONE',  ( -0.6493855936264999462, -79.80891271007898524, 10.92090362500000111 ) ) ;
#50557 = CARTESIAN_POINT ( 'NONE',  ( -7.618386461942000309, -23.22712559346000205, -10.53495196323000016 ) ) ;
#50558 = CARTESIAN_POINT ( 'NONE',  ( 12.58335110165999993, -57.05111654290000445, -1.667961430005999945 ) ) ;
#50559 = CARTESIAN_POINT ( 'NONE',  ( 0.2634948857500000186, -84.78704385015599598, -3.747257769858999943 ) ) ;
#50560 = ORIENTED_EDGE ( 'NONE', *, *, #32747, .F. ) ;
#50561 = CARTESIAN_POINT ( 'NONE',  ( -10.80510142227721282, -77.19999999999998863, 1.932663460688196500 ) ) ;
#50562 = CARTESIAN_POINT ( 'NONE',  ( 11.35264079262999992, -76.54345827915599898, 2.443064948458000263 ) ) ;
#50563 = CARTESIAN_POINT ( 'NONE',  ( 4.601699413956535700, -77.93997073655324925, 9.715216775470373989 ) ) ;
#50564 = CARTESIAN_POINT ( 'NONE',  ( 10.42503750987000011, -77.34289962869399915, -5.902083371034000159 ) ) ;
#50565 = CARTESIAN_POINT ( 'NONE',  ( -2.598917237794094337, -3.447916666666665630, 1.997276839918461722 ) ) ;
#50567 = CARTESIAN_POINT ( 'NONE',  ( 3.250000000000000000, -1.250000000000000000, 0.000000000000000000 ) ) ;
#50566 = CARTESIAN_POINT ( 'NONE',  ( -7.220923959705244144, -78.37291666666665435, -9.396085398178621872 ) ) ;
#50568 = CARTESIAN_POINT ( 'NONE',  ( 2.928645267525979090, -2.450581852303367558, -2.077595690244096627 ) ) ;
#50569 = CARTESIAN_POINT ( 'NONE',  ( 4.107670404649118368, -80.94402357793687486, 9.934114837241841300 ) ) ;
#50570 = CARTESIAN_POINT ( 'NONE',  ( 8.774584709929998283, -78.85553623779898658, 3.021992008916999595 ) ) ;
#50571 = CARTESIAN_POINT ( 'NONE',  ( 0.3439668297849150513, -85.94828564506399005, -7.678084447329936779 ) ) ;
#50572 = CARTESIAN_POINT ( 'NONE',  ( -5.822924921437000023, -77.80987522413700219, 9.505164171658000427 ) ) ;
#50573 = CARTESIAN_POINT ( 'NONE',  ( -4.368496844144680757, -76.05524822590969336, 10.93374668194784860 ) ) ;
#50574 = CARTESIAN_POINT ( 'NONE',  ( -3.181350147293000141, -80.78918126068253969, 10.67690104642000115 ) ) ;
#50575 = EDGE_LOOP ( 'NONE', ( #54080, #49302, #52425, #51189 ) ) ;
#50576 = EDGE_CURVE ( 'NONE', #36474, #27203, #1113, .T. ) ;
#50577 = CARTESIAN_POINT ( 'NONE',  ( 0.000000000000000000, -76.00000000000000000, -2.299999999999952749 ) ) ;
#50578 = CARTESIAN_POINT ( 'NONE',  ( -7.995796640818024770, -55.11315380192719005, 7.555116226634187804 ) ) ;
#50580 = EDGE_CURVE ( 'NONE', #15223, #23344, #37845, .T. ) ;
#50579 = B_SPLINE_CURVE_WITH_KNOTS ( 'NONE', 3,
 ( #16563, #41034, #4433, #8859, #36884, #54618 ),
 .UNSPECIFIED., .F., .F.,
 ( 4, 1, 1, 4 ),
 ( 0.000000000000000000, 0.3333333333333000081, 0.6666666666667000474, 1.000000000000000000 ),
 .UNSPECIFIED. ) ;
#50581 = CARTESIAN_POINT ( 'NONE',  ( -5.751434148371999733, -77.78047398443999327, -9.630115047516998317 ) ) ;
#50582 = CARTESIAN_POINT ( 'NONE',  ( 3.303001513109999898, -78.95887072009900010, -10.46681410869999951 ) ) ;
#50583 = DIRECTION ( 'NONE',  ( -1.000000000000000000, 0.000000000000000000, 0.000000000000000000 ) ) ;
#50584 = CARTESIAN_POINT ( 'NONE',  ( -1.250000000000000000, -60.04999999966999980, 12.50000000000000000 ) ) ;
#50585 = CARTESIAN_POINT ( 'NONE',  ( 0.000000000000000000, -76.39999999999999147, -0.5999999999999999778 ) ) ;
#50586 = CARTESIAN_POINT ( 'NONE',  ( -9.355955347527174837, -53.62516908766477997, -8.610895743755770937 ) ) ;
#50587 = B_SPLINE_CURVE_WITH_KNOTS ( 'NONE', 3,
 ( #28314, #32163, #37473, #55494, #5319, #46366 ),
 .UNSPECIFIED., .F., .F.,
 ( 4, 1, 1, 4 ),
 ( 0.000000000000000000, 0.3333333333333000081, 0.6666666666667000474, 1.000000000000000000 ),
 .UNSPECIFIED. ) ;
#50588 = AXIS2_PLACEMENT_3D ( 'NONE', #16218, #44232, #17363 ) ;
#50589 = CARTESIAN_POINT ( 'NONE',  ( -4.134104809361999422, -83.14892953870898396, 0.5618920481403999467 ) ) ;
#50590 = CARTESIAN_POINT ( 'NONE',  ( -10.42531124905999995, -23.26485148473999942, -7.624341765453999997 ) ) ;
#50591 = VECTOR ( 'NONE', #14030, 1000.000000000000000 ) ;
#50592 = AXIS2_PLACEMENT_3D ( 'NONE', #45797, #49636, #13304 ) ;
#50593 = CARTESIAN_POINT ( 'NONE',  ( 9.676723759786998613, -78.80221383193000406, 8.603871787294998796 ) ) ;
#50594 = EDGE_CURVE ( 'NONE', #21904, #19797, #6445, .T. ) ;
#50595 = CIRCLE ( 'NONE', #21450, 30.49999999999998934 ) ;
#50596 = CARTESIAN_POINT ( 'NONE',  ( -5.117553686986000550, -78.26666441077600211, -10.03691081092000026 ) ) ;
#50597 = CARTESIAN_POINT ( 'NONE',  ( -0.3164372427141999844, -79.60138345058999221, 1.635583079321000000 ) ) ;
#50598 = CARTESIAN_POINT ( 'NONE',  ( 0.3615948191998999972, -78.60193473990000257, -1.388282749240000058 ) ) ;
#50599 = CARTESIAN_POINT ( 'NONE',  ( 6.043427764450761686, -77.63333333333329733, 10.48543666025110888 ) ) ;
#50600 = CARTESIAN_POINT ( 'NONE',  ( 0.1760362647577854434, -82.11637306212345777, 1.535881408346201127 ) ) ;
#50601 = DIRECTION ( 'NONE',  ( 0.000000000000000000, -1.000000000000000000, -1.718649962392999796E-13 ) ) ;
#50602 = DIRECTION ( 'NONE',  ( -1.000000000000000000, 0.000000000000000000, 0.000000000000000000 ) ) ;
#50603 = DIRECTION ( 'NONE',  ( 0.000000000000000000, -1.000000000000000000, 0.000000000000000000 ) ) ;
#50604 = CARTESIAN_POINT ( 'NONE',  ( 1.310679582531388387, -78.10833333333333428, -0.7554284705563470981 ) ) ;
#50605 = ORIENTED_EDGE ( 'NONE', *, *, #23281, .F. ) ;
#50606 = CARTESIAN_POINT ( 'NONE',  ( 14.00000000000000000, -45.89236309322999574, 1.352041732613999901E-05 ) ) ;
#50607 = SURFACE_SIDE_STYLE ('',( #14272 ) ) ;
#50608 = CARTESIAN_POINT ( 'NONE',  ( 8.413030999918001740, -80.15288448085529183, -7.136010437995999212 ) ) ;
#50609 = CARTESIAN_POINT ( 'NONE',  ( -1.009333286406026264, -81.50605136130415929, -0.8706792349393618347 ) ) ;
#50610 = ORIENTED_EDGE ( 'NONE', *, *, #40953, .T. ) ;
#50611 = ORIENTED_EDGE ( 'NONE', *, *, #44033, .F. ) ;
#50612 = CARTESIAN_POINT ( 'NONE',  ( 1.496442341964999923, -81.81018341126400628, 0.2441364298766999785 ) ) ;
#50613 = VERTEX_POINT ( 'NONE', #43320 ) ;
#50614 = EDGE_LOOP ( 'NONE', ( #23728, #6589, #26112, #53490 ) ) ;
#50615 = CARTESIAN_POINT ( 'NONE',  ( 1.933504092460000212, -18.59593152724999854, 12.70940235707999832 ) ) ;
#50616 = CARTESIAN_POINT ( 'NONE',  ( 12.00000000000000000, -60.04999999966999980, -1.250000000000000000 ) ) ;
#50617 = DIRECTION ( 'NONE',  ( 0.000000000000000000, 0.000000000000000000, 1.000000000000000000 ) ) ;
#50618 = CARTESIAN_POINT ( 'NONE',  ( 3.433336739787663294, -79.43229166101083649, -0.2598626512273453648 ) ) ;
#50619 = CARTESIAN_POINT ( 'NONE',  ( 6.682297893293000612, -79.50746001420199605, -6.800905403285999462 ) ) ;
#50620 = CARTESIAN_POINT ( 'NONE',  ( 5.314949332417438832, -78.27388777455939817, -7.570571360755021573 ) ) ;
#50621 = CARTESIAN_POINT ( 'NONE',  ( 0.000000000000000000, 4.040000000000000036, 0.000000000000000000 ) ) ;
#50622 = EDGE_LOOP ( 'NONE', ( #14632, #10963, #15363, #22790 ) ) ;
#50623 = ORIENTED_EDGE ( 'NONE', *, *, #31148, .T. ) ;
#50624 = CARTESIAN_POINT ( 'NONE',  ( -8.697226998145453081, -77.57235979624698530, 3.151704567404991053 ) ) ;
#50625 = CARTESIAN_POINT ( 'NONE',  ( 6.536064251314178897, -80.02434017810877265, 8.743451022905414760 ) ) ;
#50626 = CARTESIAN_POINT ( 'NONE',  ( -1.500000000000000888, -79.48958333333334281, 0.1963495408493559080 ) ) ;
#50627 = EDGE_CURVE ( 'NONE', #49672, #43122, #29324, .T. ) ;
#50628 = CARTESIAN_POINT ( 'NONE',  ( 0.1380878923674745407, -62.02734402291400784, -12.70555840937129943 ) ) ;
#50629 = CARTESIAN_POINT ( 'NONE',  ( -8.592320330817999618, -78.23138195110698234, 4.510292750937000328 ) ) ;
#50630 = CARTESIAN_POINT ( 'NONE',  ( 0.000000000000000000, -78.00000000000000000, 0.000000000000000000 ) ) ;
#50631 = CARTESIAN_POINT ( 'NONE',  ( 0.1290952183515442220, -85.95735607754586738, 3.973009594863323279 ) ) ;
#50632 = CIRCLE ( 'NONE', #51560, 4.100000000000000533 ) ;
#50633 = CARTESIAN_POINT ( 'NONE',  ( -3.187445619818999987, -77.81332093041999087, 12.55797944092000051 ) ) ;
#50634 = EDGE_CURVE ( 'NONE', #41515, #22103, #41599, .T. ) ;
#50635 = CARTESIAN_POINT ( 'NONE',  ( -0.6027184710183000060, -81.11268744342000048, 1.466649853462000053 ) ) ;
#50636 = DIRECTION ( 'NONE',  ( 0.7071067811865475727, 0.000000000000000000, 0.7071067811865475727 ) ) ;
#50637 = VECTOR ( 'NONE', #57586, 1000.000000000000000 ) ;
#50638 = CARTESIAN_POINT ( 'NONE',  ( -6.829991769570769478, -76.62375042572244865, 9.568360097740603365 ) ) ;
#50639 = CARTESIAN_POINT ( 'NONE',  ( 2.572602951542000138, -82.28999676290898435, -3.288090883683000065 ) ) ;
#50640 = CONICAL_SURFACE ( 'NONE', #1629, 10.29999999923999887, 0.7853981633972997312 ) ;
#50641 = CARTESIAN_POINT ( 'NONE',  ( -11.26045488449999965, -80.76374820225451856, 0.3336940576009999604 ) ) ;
#50642 = FACE_OUTER_BOUND ( 'NONE', #18866, .T. ) ;
#50643 = CARTESIAN_POINT ( 'NONE',  ( -4.399010402408173093, -80.42916666666943115, -9.895799249887454963 ) ) ;
#50644 = CARTESIAN_POINT ( 'NONE',  ( 3.499633968373000226, -80.92957046129099297, -0.5806158015779000481 ) ) ;
#50645 = CARTESIAN_POINT ( 'NONE',  ( 1.315129997485000146, -78.48515813772890226, 0.2213803045116000123 ) ) ;
#50646 = CYLINDRICAL_SURFACE ( 'NONE', #5353, 12.50000000000000000 ) ;
#50647 = CARTESIAN_POINT ( 'NONE',  ( 0.000000000000000000, -62.90094976977999863, 0.000000000000000000 ) ) ;
#50648 = CARTESIAN_POINT ( 'NONE',  ( 1.911540947291000103, -3.185127687536000174, 3.291214574437999918 ) ) ;
#50649 = CARTESIAN_POINT ( 'NONE',  ( 10.59040229099152874, -77.20000000000000284, -2.027287110957618932 ) ) ;
#50650 = ORIENTED_EDGE ( 'NONE', *, *, #12879, .T. ) ;
#50651 = CARTESIAN_POINT ( 'NONE',  ( -0.7664558997027911547, -3.499999999999999556, -3.353144190923705192 ) ) ;
#50652 = CARTESIAN_POINT ( 'NONE',  ( -11.40562379108000002, -78.11535612247598692, 0.7834358085291999174 ) ) ;
#50653 = CARTESIAN_POINT ( 'NONE',  ( 8.485281374238999419, -60.04999999966999980, 8.485281374238999419 ) ) ;
#50654 = EDGE_CURVE ( 'NONE', #22997, #9420, #10645, .T. ) ;
#50655 = CARTESIAN_POINT ( 'NONE',  ( 1.799501877759999813, -60.08917565288000162, 12.60552522438000089 ) ) ;
#50656 = CARTESIAN_POINT ( 'NONE',  ( 12.52133763471539396, -18.07246868479867885, -1.618901767041418083 ) ) ;
#50657 = CARTESIAN_POINT ( 'NONE',  ( -2.439418945719407983, -79.49321589760896245, 10.46964760755776247 ) ) ;
#50658 = CARTESIAN_POINT ( 'NONE',  ( 5.754008857420999767, -79.26781332859900431, 7.857252078236999004 ) ) ;
#50659 = B_SPLINE_CURVE_WITH_KNOTS ( 'NONE', 3,
 ( #6332, #55936, #10777, #29335, #42062, #14599 ),
 .UNSPECIFIED., .F., .F.,
 ( 4, 1, 1, 4 ),
 ( 0.000000000000000000, 0.3333333333333000081, 0.6666666666667000474, 1.000000000000000000 ),
 .UNSPECIFIED. ) ;
#50660 = CARTESIAN_POINT ( 'NONE',  ( 13.86363636363000218, -69.16102867818000277, 1.277888278513000037E-05 ) ) ;
#50661 = CARTESIAN_POINT ( 'NONE',  ( -11.15274311834000009, -77.24684517626799618, -0.5305918353390000064 ) ) ;
#50662 = EDGE_CURVE ( 'NONE', #40049, #8187, #13459, .T. ) ;
#50663 = CARTESIAN_POINT ( 'NONE',  ( -3.075839145942573793, -76.30340551261170390, -11.34163394545276837 ) ) ;
#50664 = CARTESIAN_POINT ( 'NONE',  ( -1.586895984600000142, -81.91972355565999919, -0.2343193179190000142 ) ) ;
#50665 = CARTESIAN_POINT ( 'NONE',  ( 8.768124086549999419, -55.65000000488999632, -7.919595949288999570 ) ) ;
#50666 = CARTESIAN_POINT ( 'NONE',  ( -9.379486438909999890, -78.02756575905399927, -0.7977647835019999745 ) ) ;
#50667 = EDGE_CURVE ( 'NONE', #25175, #7399, #49143, .T. ) ;
#50669 = CARTESIAN_POINT ( 'NONE',  ( -1.150280981678749370, -80.21041666702008399, -10.98958334528740899 ) ) ;
#50668 = CARTESIAN_POINT ( 'NONE',  ( 2.891731347767999782, -83.82504052802198657, 2.709959370028000247 ) ) ;
#50670 = CARTESIAN_POINT ( 'NONE',  ( -8.650571159592999493, -79.59515194988499331, 4.057379972786000266 ) ) ;
#50671 = DIRECTION ( 'NONE',  ( 0.000000000000000000, 1.000000000000000000, 0.000000000000000000 ) ) ;
#50672 = CARTESIAN_POINT ( 'NONE',  ( -1.310679582531389498, -81.45833333333332860, 0.7554284705563444335 ) ) ;
#50673 = AXIS2_PLACEMENT_3D ( 'NONE', #39140, #43877, #52727 ) ;
#50674 = CARTESIAN_POINT ( 'NONE',  ( -6.167996266013765272, -77.17653180539056734, -8.804416017395640282 ) ) ;
#50675 = DIRECTION ( 'NONE',  ( 1.000000000000000000, 0.000000000000000000, 0.000000000000000000 ) ) ;
#50676 = ORIENTED_EDGE ( 'NONE', *, *, #46991, .T. ) ;
#50677 = ORIENTED_EDGE ( 'NONE', *, *, #24776, .F. ) ;
#50678 = CARTESIAN_POINT ( 'NONE',  ( 11.43764105185000091, -79.90228420331349923, 2.691257544168000226 ) ) ;
#50679 = LINE ( 'NONE', #23788, #10491 ) ;
#50680 = DIRECTION ( 'NONE',  ( -1.000000000000000000, 0.000000000000000000, 0.000000000000000000 ) ) ;
#50681 = VECTOR ( 'NONE', #36732, 1000.000000000000000 ) ;
#50682 = ORIENTED_EDGE ( 'NONE', *, *, #35748, .F. ) ;
#50683 = CARTESIAN_POINT ( 'NONE',  ( -1.355082891136000001, -77.73935448679299043, -11.85745557885999979 ) ) ;
#50684 = AXIS2_PLACEMENT_3D ( 'NONE', #47389, #33482, #6633 ) ;
#50685 = VERTEX_POINT ( 'NONE', #18489 ) ;
#50686 = VERTEX_POINT ( 'NONE', #35593 ) ;
#50687 = EDGE_CURVE ( 'NONE', #54581, #36547, #8522, .T. ) ;
#50688 = EDGE_LOOP ( 'NONE', ( #26614, #34674, #27632, #3754 ) ) ;
#50689 = CARTESIAN_POINT ( 'NONE',  ( 3.263030582009000202, -82.33492937544698975, -1.391710130416999869 ) ) ;
#50690 = DIRECTION ( 'NONE',  ( 0.000000000000000000, -0.7071067811866525998, -0.7071067811864425456 ) ) ;
#50691 = VERTEX_POINT ( 'NONE', #18780 ) ;
#50692 = CARTESIAN_POINT ( 'NONE',  ( 1.242748055744218760, -82.84189893657375592, -0.1341030727711693959 ) ) ;
#50693 = ORIENTED_EDGE ( 'NONE', *, *, #42170, .F. ) ;
#50694 = CARTESIAN_POINT ( 'NONE',  ( -1.242284077307689305, -79.59059820921201833, 0.1573562424055395537 ) ) ;
#50695 = CARTESIAN_POINT ( 'NONE',  ( -8.771572603219439657, -77.88508160123497248, -4.151306042262981499 ) ) ;
#50696 = CARTESIAN_POINT ( 'NONE',  ( 0.000000000000000000, -87.59999999999999432, -9.599999999999999645 ) ) ;
#50697 = ADVANCED_FACE ( 'NONE', ( #45659 ), #13176, .F. ) ;
#50698 = CARTESIAN_POINT ( 'NONE',  ( -8.485281374238999419, -55.54999999966999980, 8.485281374238999419 ) ) ;
#50699 = CARTESIAN_POINT ( 'NONE',  ( 3.202161418990787212, -0.9218749995132479169, 1.046229558418831473 ) ) ;
#50700 = CARTESIAN_POINT ( 'NONE',  ( 10.97835188747000146, -75.93304601283999489, -2.133021021907000048 ) ) ;
#50701 = B_SPLINE_CURVE_WITH_KNOTS ( 'NONE', 3,
 ( #17022, #44764, #22019, #40330, #21157, #53039, #39738, #13455, #48332, #31451, #4013, #30868, #48904, #40027, #58040, #53321, #17600, #34719 ),
 .UNSPECIFIED., .F., .F.,
 ( 4, 2, 2, 2, 2, 2, 2, 2, 4 ),
 ( 0.000000000000000000, 0.1250000000000000000, 0.2500000000000000000, 0.3750000000000000000, 0.5000000000000000000, 0.6250000000000000000, 0.7500000000000000000, 0.8750000000000000000, 1.000000000000000000 ),
 .UNSPECIFIED. ) ;
#50702 = CYLINDRICAL_SURFACE ( 'NONE', #53301, 3.600000000000000089 ) ;
#50703 = ADVANCED_FACE ( 'NONE', ( #227 ), #26479, .F. ) ;
#50704 = CARTESIAN_POINT ( 'NONE',  ( 0.000000000000000000, -76.00000000000000000, 0.000000000000000000 ) ) ;
#50705 = CARTESIAN_POINT ( 'NONE',  ( -7.691916945423999508, -57.04634220890999785, -10.42274798266000069 ) ) ;
#50706 = CARTESIAN_POINT ( 'NONE',  ( 7.406672800339156204, -78.79889337847342290, -5.541606015867000856 ) ) ;
#50707 = CARTESIAN_POINT ( 'NONE',  ( 7.328371322744000160, -77.76668501420199675, -5.905229698647000092 ) ) ;
#50708 = FACE_OUTER_BOUND ( 'NONE', #56613, .T. ) ;
#50709 = CARTESIAN_POINT ( 'NONE',  ( -10.24927991466481458, -80.12999227341786934, -3.994845400455109719 ) ) ;
#50710 = CARTESIAN_POINT ( 'NONE',  ( -11.98418414837124324, -77.95952000033295803, -0.9817159035101585829 ) ) ;
#50711 = CIRCLE ( 'NONE', #13898, 1.000000000000000000 ) ;
#50712 = CARTESIAN_POINT ( 'NONE',  ( 2.636359243785999951, -80.84653455456798099, 2.958984748685999921 ) ) ;
#50713 = FACE_OUTER_BOUND ( 'NONE', #25941, .T. ) ;
#50714 = DIRECTION ( 'NONE',  ( 0.000000000000000000, -1.000000000000000000, 0.000000000000000000 ) ) ;
#50715 = CARTESIAN_POINT ( 'NONE',  ( 0.03615408296859652648, -82.97326937661254931, 1.249771234374210449 ) ) ;
#50716 = CARTESIAN_POINT ( 'NONE',  ( 2.946159983835261897, -77.05000000000001137, -9.062386480552282464 ) ) ;
#50717 = DIRECTION ( 'NONE',  ( 1.000000000000000000, 0.000000000000000000, 0.000000000000000000 ) ) ;
#50718 = CARTESIAN_POINT ( 'NONE',  ( 5.821064686149081346, -79.99999999999998579, 7.358320351470873710 ) ) ;
#50719 = DIRECTION ( 'NONE',  ( 1.411450211591999950E-10, -6.386278974555000074E-09, -1.000000000000000000 ) ) ;
#50720 = AXIS2_PLACEMENT_3D ( 'NONE', #1166, #23861, #28577 ) ;
#50721 = LINE ( 'NONE', #51010, #21740 ) ;
#50722 = CARTESIAN_POINT ( 'NONE',  ( -2.061613410425999771, -23.20570014476000154, -12.83797036855999885 ) ) ;
#50723 = DIRECTION ( 'NONE',  ( -0.7071067811865475727, 0.000000000000000000, -0.7071067811865475727 ) ) ;
#50724 = CARTESIAN_POINT ( 'NONE',  ( 1.072256020167000168, -2.194262446210000217, -3.316546452965000391 ) ) ;
#50725 = CARTESIAN_POINT ( 'NONE',  ( 12.78037829248000001, -24.29316779390000036, 1.812823010630000065 ) ) ;
#50726 = CARTESIAN_POINT ( 'NONE',  ( 0.7681833999686451531, -80.67708333333332860, -0.9995835529977240563 ) ) ;
#50727 = CARTESIAN_POINT ( 'NONE',  ( -7.319319664381377599, -77.51649663083381370, -7.993250365100486476 ) ) ;
#50728 = DIRECTION ( 'NONE',  ( 0.000000000000000000, -1.000000000000000000, 0.000000000000000000 ) ) ;
#50729 = CIRCLE ( 'NONE', #36543, 0.5000000000000000000 ) ;
#50731 = CARTESIAN_POINT ( 'NONE',  ( -1.779623408260310846, -24.13630869023863568, -12.71471627657074066 ) ) ;
#50730 = CARTESIAN_POINT ( 'NONE',  ( 1.669849926066999890, -60.17228600383999293, 12.48404299555999941 ) ) ;
#50732 = CARTESIAN_POINT ( 'NONE',  ( -1.684993323399000209, -75.86946921342000394, -11.94349415379999968 ) ) ;
#50733 = ORIENTED_EDGE ( 'NONE', *, *, #23041, .F. ) ;
#50734 = CARTESIAN_POINT ( 'NONE',  ( 3.962859907113000180, -85.75721544543100094, 0.04150063856765000281 ) ) ;
#50735 = CARTESIAN_POINT ( 'NONE',  ( 6.471694488619999852, -80.60357658748300480, 9.391741773560999818 ) ) ;
#50736 = CARTESIAN_POINT ( 'NONE',  ( 8.112428353360469302, -78.31019145401509718, -4.445158527088241662 ) ) ;
#50737 = CARTESIAN_POINT ( 'NONE',  ( 12.54980660771999901, -61.84777352133000505, -0.05651102257804999779 ) ) ;
#50738 = CARTESIAN_POINT ( 'NONE',  ( -10.86658628928999981, -76.92162226719798923, -2.781249891074999869 ) ) ;
#50739 = DIRECTION ( 'NONE',  ( -0.7071067811865475727, 0.000000000000000000, -0.7071067811865475727 ) ) ;
#50740 = CARTESIAN_POINT ( 'NONE',  ( 5.949632932387999951, -78.00648151147798615, -7.711132450962999485 ) ) ;
#50741 = CARTESIAN_POINT ( 'NONE',  ( 12.50000000000000000, -55.55000000209000177, 1.750000000000000000 ) ) ;
#50742 = CARTESIAN_POINT ( 'NONE',  ( 7.954951288349001004, -60.04999999966999980, -9.722718241315000398 ) ) ;
#50743 = CARTESIAN_POINT ( 'NONE',  ( 11.00000000000000000, -81.00000000000000000, -2.369510767747999942E-13 ) ) ;
#50744 = EDGE_LOOP ( 'NONE', ( #17484, #19228, #21650, #8914 ) ) ;
#50745 = CARTESIAN_POINT ( 'NONE',  ( -10.75000000000000000, -78.50000000000000000, 0.000000000000000000 ) ) ;
#50746 = CARTESIAN_POINT ( 'NONE',  ( 3.862060628231000159, -80.54547121896008832, 10.58270681924999934 ) ) ;
#50747 = LINE ( 'NONE', #7017, #29952 ) ;
#50748 = ORIENTED_EDGE ( 'NONE', *, *, #33219, .F. ) ;
#50749 = CARTESIAN_POINT ( 'NONE',  ( -0.9612450871864000046, -78.73905986043699556, -0.9244371432244999909 ) ) ;
#50750 = CARTESIAN_POINT ( 'NONE',  ( 8.768124086549999419, -55.65000000488999632, -7.919595949288999570 ) ) ;
#50751 = ORIENTED_EDGE ( 'NONE', *, *, #57025, .F. ) ;
#50752 = CARTESIAN_POINT ( 'NONE',  ( 8.905881360917000222, -79.06849849426399146, 8.286615985300000986 ) ) ;
#50753 = CARTESIAN_POINT ( 'NONE',  ( 2.255546383061999727, -78.07046773478798229, -10.87004418268000094 ) ) ;
#50754 = CARTESIAN_POINT ( 'NONE',  ( 7.764217752279196638, -61.05600304927079947, -10.21028588420891126 ) ) ;
#50755 = ORIENTED_EDGE ( 'NONE', *, *, #2161, .T. ) ;
#50756 = EDGE_LOOP ( 'NONE', ( #40735, #34445, #51776, #54798 ) ) ;
#50757 = ADVANCED_FACE ( 'NONE', ( #19073 ), #5777, .T. ) ;
#50758 = B_SPLINE_CURVE_WITH_KNOTS ( 'NONE', 3,
 ( #56564, #53001, #29965, #43281, #21122, #4790, #57137, #34397, #16704, #9219 ),
 .UNSPECIFIED., .F., .F.,
 ( 4, 2, 2, 2, 4 ),
 ( 0.000000000000000000, 0.1250000000000028033, 0.2500000000000056066, 0.5000000000000012212, 1.000000000000000000 ),
 .UNSPECIFIED. ) ;
#50759 = CARTESIAN_POINT ( 'NONE',  ( -1.162396057392936166, -80.57013522272643513, 0.4596509125629028580 ) ) ;
#50760 = EDGE_CURVE ( 'NONE', #20196, #42760, #37938, .T. ) ;
#50761 = CARTESIAN_POINT ( 'NONE',  ( 8.944729675425000082, -79.67334768894899355, 3.923329690209000908 ) ) ;
#50762 = ORIENTED_EDGE ( 'NONE', *, *, #52987, .F. ) ;
#50763 = CARTESIAN_POINT ( 'NONE',  ( 12.66001647282000064, -54.16746073337000666, 1.381678996660000047 ) ) ;
#50764 = CARTESIAN_POINT ( 'NONE',  ( -7.601397897754999633, -23.25000000000000000, 9.369164850722000892 ) ) ;
#50765 = ORIENTED_EDGE ( 'NONE', *, *, #41128, .F. ) ;
#50766 = CARTESIAN_POINT ( 'NONE',  ( -12.77301895549999955, -25.05186686373999905, -1.052127376137000025 ) ) ;
#50767 = CARTESIAN_POINT ( 'NONE',  ( -8.123853732960998997, -77.08675194988499868, 4.915330883505999893 ) ) ;
#50768 = CARTESIAN_POINT ( 'NONE',  ( 3.715423405847853466, -82.70470561765866080, -0.7897406471633323655 ) ) ;
#50769 = CARTESIAN_POINT ( 'NONE',  ( 1.343749999883000035, -77.90625000011999646, 3.156563468101999814E-09 ) ) ;
#50770 = CARTESIAN_POINT ( 'NONE',  ( -10.15788331741117645, -76.62184280497177724, 3.765280591527957910 ) ) ;
#50771 = EDGE_CURVE ( 'NONE', #33815, #2535, #28392, .T. ) ;
#50772 = CARTESIAN_POINT ( 'NONE',  ( 7.267042919475000140, -76.96477995979998354, -6.172551194186000068 ) ) ;
#50773 = CARTESIAN_POINT ( 'NONE',  ( 1.297392051789066025, -78.14223917446591372, 0.7709785167501194136 ) ) ;
#50774 = CARTESIAN_POINT ( 'NONE',  ( -3.206845790991853740, -80.35729166409527124, -2.475673254574849214 ) ) ;
#50775 = ORIENTED_EDGE ( 'NONE', *, *, #4415, .F. ) ;
#50776 = CARTESIAN_POINT ( 'NONE',  ( -10.77133038182000035, -76.55754729621000365, -5.959359258312999508 ) ) ;
#50777 = CARTESIAN_POINT ( 'NONE',  ( 0.5460188671879216971, -2.211847916353453236, 3.477752717589034592 ) ) ;
#50778 = DIRECTION ( 'NONE',  ( 1.000000000000000000, 0.000000000000000000, 0.000000000000000000 ) ) ;
#50780 = ADVANCED_FACE ( 'NONE', ( #55079 ), #4241, .F. ) ;
#50779 = CARTESIAN_POINT ( 'NONE',  ( -3.417863094299999904, -78.41531695063000029, 11.50296535110000029 ) ) ;
#50781 = CARTESIAN_POINT ( 'NONE',  ( -0.6669403506045999963, -76.18678200654200339, -12.26286337364000012 ) ) ;
#50782 = DIRECTION ( 'NONE',  ( 0.000000000000000000, 1.000000000000000000, 0.000000000000000000 ) ) ;
#50783 = CARTESIAN_POINT ( 'NONE',  ( 3.006733838401902670, -2.820045760104889165, -1.232120965224751563 ) ) ;
#50784 = CARTESIAN_POINT ( 'NONE',  ( -11.90430176566012577, -78.06094887269661342, -1.649208845716615635 ) ) ;
#50785 = DIRECTION ( 'NONE',  ( 0.000000000000000000, -1.000000000000000000, 0.000000000000000000 ) ) ;
#50786 = EDGE_CURVE ( 'NONE', #50040, #22044, #10512, .T. ) ;
#50787 = ORIENTED_EDGE ( 'NONE', *, *, #18085, .T. ) ;
#50788 = CARTESIAN_POINT ( 'NONE',  ( -0.4696505103051999974, -83.11672773667999081, -1.267043746813000249 ) ) ;
#50789 = CARTESIAN_POINT ( 'NONE',  ( 11.44417895085271475, -78.02916666666666856, -3.075537641221520069 ) ) ;
#50790 = DIRECTION ( 'NONE',  ( 0.000000000000000000, -1.000000000000000000, 0.000000000000000000 ) ) ;
#50791 = CARTESIAN_POINT ( 'NONE',  ( 0.000000000000000000, -75.10000000284179578, -8.299999997157998521 ) ) ;
#50792 = CARTESIAN_POINT ( 'NONE',  ( -3.708003915733999900, -3.317513707840999970, -1.109421345883999876 ) ) ;
#50793 = CARTESIAN_POINT ( 'NONE',  ( 4.358044849164000922, -77.23133731782699840, -11.11047130621000001 ) ) ;
#50794 = CARTESIAN_POINT ( 'NONE',  ( 7.350012343602999820, -77.40102789785198922, -6.223385617129999936 ) ) ;
#50795 = CIRCLE ( 'NONE', #31879, 14.00000000000000000 ) ;
#50796 = CARTESIAN_POINT ( 'NONE',  ( -10.58828373193520456, -76.16399079984034870, 5.094882559088077301 ) ) ;
#50797 = CARTESIAN_POINT ( 'NONE',  ( -8.065049863481000614, -78.96773976718499455, 7.357332172019000360 ) ) ;
#50798 = CARTESIAN_POINT ( 'NONE',  ( 1.504274447196337405, -85.80681307243298761, 3.466210801031209154 ) ) ;
#50799 = ORIENTED_EDGE ( 'NONE', *, *, #36699, .F. ) ;
#50800 = CARTESIAN_POINT ( 'NONE',  ( 10.54796701376999835, -75.84310348540464020, 6.346365727669000201 ) ) ;
#50801 = CARTESIAN_POINT ( 'NONE',  ( 9.505949683908001546, -79.00000000000000000, -6.906476714433999575 ) ) ;
#50802 = CARTESIAN_POINT ( 'NONE',  ( -1.538071403319991814, -76.91458333333332575, -11.75000000000000355 ) ) ;
#50803 = CARTESIAN_POINT ( 'NONE',  ( -0.5193979750644999172, -79.11168714277798131, -10.96331347381999954 ) ) ;
#50804 = EDGE_CURVE ( 'NONE', #55909, #37146, #48553, .T. ) ;
#50805 = CARTESIAN_POINT ( 'NONE',  ( -6.043427764450833628, -77.81666666666667709, 10.48543666025107335 ) ) ;
#50806 = CARTESIAN_POINT ( 'NONE',  ( -7.858535633446000368, -79.69256872134099012, -5.635447047609000393 ) ) ;
#50807 = CARTESIAN_POINT ( 'NONE',  ( 9.636775127281000053, -17.55967715742000124, -7.948072248884999524 ) ) ;
#50808 = CARTESIAN_POINT ( 'NONE',  ( 1.250000000000000000, -18.75000000000000000, 12.50000000000000000 ) ) ;
#50809 = ORIENTED_EDGE ( 'NONE', *, *, #33229, .T. ) ;
#50810 = LINE ( 'NONE', #23051, #55018 ) ;
#50811 = AXIS2_PLACEMENT_3D ( 'NONE', #23084, #689, #45247 ) ;
#50812 = CARTESIAN_POINT ( 'NONE',  ( -11.52726388849324657, -79.53165972776588433, 2.674423737329086670 ) ) ;
#50813 = CARTESIAN_POINT ( 'NONE',  ( -2.218415739201539338, -78.39678895079168797, 3.679255581759628413 ) ) ;
#50814 = CARTESIAN_POINT ( 'NONE',  ( -3.680468777719496654, -77.85277880226108493, 11.44633469405415838 ) ) ;
#50816 = CARTESIAN_POINT ( 'NONE',  ( -0.8894962667724020111, -81.53855449988152770, 0.8777776201967760761 ) ) ;
#50815 = CARTESIAN_POINT ( 'NONE',  ( -1.296534853615000094, -81.67286366981399226, -0.2440552883437999976 ) ) ;
#50817 = CARTESIAN_POINT ( 'NONE',  ( -0.2721136687859672665, -79.22683890273980012, 11.21372209014444898 ) ) ;
#50818 = CARTESIAN_POINT ( 'NONE',  ( -7.034477742621340290, -76.99999999999998579, -6.292097733782652469 ) ) ;
#50819 = CARTESIAN_POINT ( 'NONE',  ( 14.00000000000000000, -9.337822431690000258, 5.544480874192999735E-06 ) ) ;
#50820 = CARTESIAN_POINT ( 'NONE',  ( 1.210822168571035418, -79.86458333333334281, 9.250000000000007105 ) ) ;
#50821 = CARTESIAN_POINT ( 'NONE',  ( 10.03798773386740706, -79.48458675554202557, 4.654823617294058025 ) ) ;
#50822 = LINE ( 'NONE', #9786, #34667 ) ;
#50823 = ORIENTED_EDGE ( 'NONE', *, *, #27264, .F. ) ;
#50824 = ORIENTED_EDGE ( 'NONE', *, *, #11193, .T. ) ;
#50825 = CARTESIAN_POINT ( 'NONE',  ( 4.594620150137028958, -77.73500000000001364, 8.363081028749707713 ) ) ;
#50826 = CARTESIAN_POINT ( 'NONE',  ( 5.979471860834143726, -78.77211117144966579, -8.933429240604114696 ) ) ;
#50827 = VECTOR ( 'NONE', #33161, 1000.000000000000000 ) ;
#50828 = ORIENTED_EDGE ( 'NONE', *, *, #14350, .F. ) ;
#50829 = DIRECTION ( 'NONE',  ( 0.000000000000000000, -1.000000000000000000, 0.000000000000000000 ) ) ;
#50830 = CARTESIAN_POINT ( 'NONE',  ( -3.304281735504577266, -83.13229168162348515, 0.9680142999968018858 ) ) ;
#50831 = CIRCLE ( 'NONE', #49871, 0.5000000000000006661 ) ;
#50832 = CARTESIAN_POINT ( 'NONE',  ( -7.664471376495262334, -79.34928386457644933, 5.612613647751031110 ) ) ;
#50833 = CARTESIAN_POINT ( 'NONE',  ( 9.414507962652001183, -62.06263135892999827, 8.652357372810001834 ) ) ;
#50835 = EDGE_CURVE ( 'NONE', #41674, #43048, #47980, .T. ) ;
#50834 = CARTESIAN_POINT ( 'NONE',  ( 5.936735104356777981, -76.21482328080708157, -10.65773319741336067 ) ) ;
#50836 = CARTESIAN_POINT ( 'NONE',  ( -11.86126082642098112, -78.56111604135236348, -1.682403921698609306 ) ) ;
#50837 = ORIENTED_EDGE ( 'NONE', *, *, #49719, .T. ) ;
#50838 = DIRECTION ( 'NONE',  ( 0.000000000000000000, -1.000000000000000000, 0.000000000000000000 ) ) ;
#50839 = ORIENTED_EDGE ( 'NONE', *, *, #57256, .T. ) ;
#50840 = CARTESIAN_POINT ( 'NONE',  ( 9.110268537203129569, -77.36402492828145228, 1.602260397345456333 ) ) ;
#50841 = CIRCLE ( 'NONE', #8500, 9.549999999999998934 ) ;
#50842 = DIRECTION ( 'NONE',  ( 0.000000000000000000, 0.000000000000000000, -1.000000000000000000 ) ) ;
#50843 = CARTESIAN_POINT ( 'NONE',  ( 9.051070938631999852, -77.66981590335299757, 3.499832029064999794 ) ) ;
#50844 = FACE_OUTER_BOUND ( 'NONE', #30379, .T. ) ;
#50845 = CONICAL_SURFACE ( 'NONE', #58369, 10.90000000000000036, 0.7853981633972997312 ) ;
#50846 = DIRECTION ( 'NONE',  ( 0.000000000000000000, 0.000000000000000000, 1.000000000000000000 ) ) ;
#50847 = CARTESIAN_POINT ( 'NONE',  ( 1.623578234368999951, -77.96668092124998850, 0.1125035222880000074 ) ) ;
#50848 = CARTESIAN_POINT ( 'NONE',  ( -3.809176057898999712, -78.63855496681158286, 1.220059858830999877 ) ) ;
#50849 = CARTESIAN_POINT ( 'NONE',  ( -0.6002759491738461906, -79.18521723992915895, -1.096379978449760095 ) ) ;
#50850 = CARTESIAN_POINT ( 'NONE',  ( -6.384381598444999639, -78.85377266276799446, 8.884114358872000849 ) ) ;
#50851 = CARTESIAN_POINT ( 'NONE',  ( -7.622785526030999570, -23.78712283485999990, -10.47836401506999948 ) ) ;
#50852 = EDGE_CURVE ( 'NONE', #50169, #3901, #55700, .T. ) ;
#50853 = B_SPLINE_CURVE_WITH_KNOTS ( 'NONE', 3,
 ( #21931, #53830, #8656, #35801, #43818, #3646, #34638, #31363, #17217, #49407, #8360, #30208, #8075, #48253, #26642, #52666, #21649, #13365 ),
 .UNSPECIFIED., .F., .F.,
 ( 4, 2, 2, 2, 2, 2, 2, 2, 4 ),
 ( 0.000000000000000000, 0.1250000000000000278, 0.2500000000000000000, 0.3750000000000001110, 0.5000000000000001110, 0.6250000000000001110, 0.7500000000000002220, 0.8750000000000001110, 1.000000000000000000 ),
 .UNSPECIFIED. ) ;
#50854 = CARTESIAN_POINT ( 'NONE',  ( 7.553659961756574504, -79.10220767479606252, 5.794321821515795889 ) ) ;
#50855 = CARTESIAN_POINT ( 'NONE',  ( 2.588169404531000417, -84.14231094026499136, 2.425479093844999934 ) ) ;
#50856 = VERTEX_POINT ( 'NONE', #8676 ) ;
#50857 = DIRECTION ( 'NONE',  ( 0.9999999999999994449, -3.428909149164998022E-08, -7.232769372636995941E-12 ) ) ;
#50858 = CARTESIAN_POINT ( 'NONE',  ( -4.650415628119000111, -76.36880274324299478, -10.64070859955000081 ) ) ;
#50859 = CARTESIAN_POINT ( 'NONE',  ( 9.692338806031742138, -77.88577333623729260, 4.653132537965349869 ) ) ;
#50860 = CARTESIAN_POINT ( 'NONE',  ( 3.925078296951999501, -78.41454232321599704, 11.31856107452000160 ) ) ;
#50861 = DIRECTION ( 'NONE',  ( 0.000000000000000000, -1.000000000000000000, 0.000000000000000000 ) ) ;
#50862 = CARTESIAN_POINT ( 'NONE',  ( 2.813943391462377264, -78.95432111614685766, 10.47071761770257758 ) ) ;
#50863 = CARTESIAN_POINT ( 'NONE',  ( -1.847034434715450368, -2.667702848378502800, 3.076255871586204726 ) ) ;
#50864 = CARTESIAN_POINT ( 'NONE',  ( 9.099057355994125018, -80.89508958227955304, 5.728627856209059566 ) ) ;
#50865 = CARTESIAN_POINT ( 'NONE',  ( -1.518219907972000016, -78.46707723970298787, 9.290113175764000530 ) ) ;
#50866 = CARTESIAN_POINT ( 'NONE',  ( 3.106054555984663956, -86.07390000031791999, -1.382904586457472496 ) ) ;
#50867 = CARTESIAN_POINT ( 'NONE',  ( 1.606468910658999993, -78.09549303256399355, -10.91425636589999826 ) ) ;
#50868 = CARTESIAN_POINT ( 'NONE',  ( -10.51110168223000052, -76.10674174704419670, 6.351495789100000344 ) ) ;
#50869 = CARTESIAN_POINT ( 'NONE',  ( -9.092652447878998956, -80.44016134263529239, -6.437458829046000197 ) ) ;
#50870 = ORIENTED_EDGE ( 'NONE', *, *, #25882, .F. ) ;
#50871 = CARTESIAN_POINT ( 'NONE',  ( 2.065394024360999836, -60.22161432612999477, -12.82193048530000112 ) ) ;
#50872 = CARTESIAN_POINT ( 'NONE',  ( 6.557611461288021637, -80.42306247819995235, 8.547703452968136162 ) ) ;
#50873 =( GEOMETRIC_REPRESENTATION_CONTEXT ( 3 ) GLOBAL_UNCERTAINTY_ASSIGNED_CONTEXT ( ( #13262 ) ) GLOBAL_UNIT_ASSIGNED_CONTEXT ( ( #3121, #3403, #45013 ) ) REPRESENTATION_CONTEXT ( 'NONE', 'WORKASPACE' ) );
#50874 = CARTESIAN_POINT ( 'NONE',  ( -10.17713110909000029, -76.73157247464199315, 4.716330562529999604 ) ) ;
#50875 = CARTESIAN_POINT ( 'NONE',  ( 8.212410987726999068, -78.06403359845799628, -6.936771999183999782 ) ) ;
#50876 = CARTESIAN_POINT ( 'NONE',  ( -12.85140862681000051, -20.24439829998999940, 1.980464483675000054 ) ) ;
#50877 = CARTESIAN_POINT ( 'NONE',  ( 3.591098859228397444, -85.56041668048763427, 1.791456720771969824 ) ) ;
#50878 = B_SPLINE_CURVE_WITH_KNOTS ( 'NONE', 3,
 ( #22402, #17099, #35978, #27114, #49583, #44547, #16821, #39816, #26521, #53119, #30945, #54002, #7950, #4101, #12667, #9, #31237, #25953 ),
 .UNSPECIFIED., .F., .F.,
 ( 4, 2, 2, 2, 2, 2, 2, 2, 4 ),
 ( 0.000000000000000000, 0.1250000000000000000, 0.2500000000000000000, 0.3750000000000000000, 0.5000000000000000000, 0.6250000000000000000, 0.7500000000000000000, 0.8750000000000000000, 1.000000000000000000 ),
 .UNSPECIFIED. ) ;
#50879 = EDGE_CURVE ( 'NONE', #1186, #23001, #2052, .T. ) ;
#50880 = CARTESIAN_POINT ( 'NONE',  ( -10.75000000000000000, -78.50615977947786917, -0.8321152720825113480 ) ) ;
#50881 = DIRECTION ( 'NONE',  ( -0.7071067811865474617, 0.000000000000000000, 0.7071067811865474617 ) ) ;
#50882 = CARTESIAN_POINT ( 'NONE',  ( 1.289384742053000021, -84.23744503318798138, 3.968318193697000673 ) ) ;
#50883 = CARTESIAN_POINT ( 'NONE',  ( 1.199500263597268246, -80.30208333333334281, 0.9218200799623752495 ) ) ;
#50884 = FACE_OUTER_BOUND ( 'NONE', #30756, .T. ) ;
#50885 = CARTESIAN_POINT ( 'NONE',  ( -6.686799317902000439, -76.85100271990599197, -9.062045808939998892 ) ) ;
#50886 = CARTESIAN_POINT ( 'NONE',  ( 0.5818457612699999837, -81.04221672439999224, -1.560998038830999857 ) ) ;
#50887 = CARTESIAN_POINT ( 'NONE',  ( 0.9355514851091999429, -78.83229613799998958, 0.9313545561094999092 ) ) ;
#50888 = CARTESIAN_POINT ( 'NONE',  ( -12.00000000000000000, -77.79999999999999716, 0.000000000000000000 ) ) ;
#50889 = CARTESIAN_POINT ( 'NONE',  ( -1.010492441417754073, -81.31676120415845332, -1.123586503558430039 ) ) ;
#50890 = VECTOR ( 'NONE', #43893, 1000.000000000000114 ) ;
#50891 = LINE ( 'NONE', #24305, #40295 ) ;
#50892 = EDGE_LOOP ( 'NONE', ( #48788, #43045, #94 ) ) ;
#50893 = DIRECTION ( 'NONE',  ( 0.7071067811865475727, 0.000000000000000000, -0.7071067811865475727 ) ) ;
#50894 = CARTESIAN_POINT ( 'NONE',  ( 0.6298731215011567075, -80.93400402381369929, 1.093396141891215922 ) ) ;
#50895 = ORIENTED_EDGE ( 'NONE', *, *, #36182, .F. ) ;
#50896 = CARTESIAN_POINT ( 'NONE',  ( 0.4784268551903346767, -81.75636360286721072, -1.154745182890940081 ) ) ;
#50897 = CARTESIAN_POINT ( 'NONE',  ( 10.97276992925000094, -79.71710299282599976, 1.140199307644999882 ) ) ;
#50898 = DIRECTION ( 'NONE',  ( -1.000000000000000000, 0.000000000000000000, 0.000000000000000000 ) ) ;
#50899 = EDGE_LOOP ( 'NONE', ( #25247, #18275, #15668, #22749 ) ) ;
#50900 = ORIENTED_EDGE ( 'NONE', *, *, #27746, .F. ) ;
#50901 = CARTESIAN_POINT ( 'NONE',  ( -0.5177863484446000308, -82.19630592153200155, -1.254600239572999820 ) ) ;
#50902 = ORIENTED_EDGE ( 'NONE', *, *, #17045, .T. ) ;
#50903 = ORIENTED_EDGE ( 'NONE', *, *, #36496, .F. ) ;
#50904 = CARTESIAN_POINT ( 'NONE',  ( -0.9218200799623775810, -81.92708333334323356, 1.199500263597266247 ) ) ;
#50905 = FACE_OUTER_BOUND ( 'NONE', #55610, .T. ) ;
#50906 = DIRECTION ( 'NONE',  ( 1.000000000000000000, 0.000000000000000000, 0.000000000000000000 ) ) ;
#50907 = CARTESIAN_POINT ( 'NONE',  ( 0.7501952194293379783, -80.62708332301558301, -3.361068624121959392 ) ) ;
#50908 = ADVANCED_FACE ( 'NONE', ( #44397 ), #8380, .F. ) ;
#50909 = CARTESIAN_POINT ( 'NONE',  ( 1.811390969245943783, -78.24081207420749706, -9.070829909341801667 ) ) ;
#50910 = CARTESIAN_POINT ( 'NONE',  ( 1.407171709420440342, -78.13541666666665719, -10.74999999999999822 ) ) ;
#50911 = VERTEX_POINT ( 'NONE', #39964 ) ;
#50913 = ORIENTED_EDGE ( 'NONE', *, *, #44777, .T. ) ;
#50912 = EDGE_CURVE ( 'NONE', #53705, #23434, #40954, .T. ) ;
#50914 = CARTESIAN_POINT ( 'NONE',  ( -9.136563440606458641, -77.58766556716409468, 1.443667254356420404 ) ) ;
#50915 = CARTESIAN_POINT ( 'NONE',  ( 9.188870790291835178, -77.67333333333333201, 2.784684813981615825 ) ) ;
#50916 = CARTESIAN_POINT ( 'NONE',  ( -1.250000000000000000, -81.49999999999998579, 0.000000000000000000 ) ) ;
#50917 = CARTESIAN_POINT ( 'NONE',  ( -1.103931348463426776, -17.37916251878369778, 12.50298439259127292 ) ) ;
#50918 = CARTESIAN_POINT ( 'NONE',  ( -9.139898499914998808, -77.18571961563208106, 2.826942883852999966 ) ) ;
#50919 = DIRECTION ( 'NONE',  ( -1.000000000000000000, 0.000000000000000000, 0.000000000000000000 ) ) ;
#50920 = CARTESIAN_POINT ( 'NONE',  ( 0.4075231696620134625, -85.94906435298663894, 3.946922339886002273 ) ) ;
#50921 = CARTESIAN_POINT ( 'NONE',  ( -11.68767212001980127, -76.87916666666666288, 3.140974612311317138 ) ) ;
#50922 = CARTESIAN_POINT ( 'NONE',  ( 1.249711497515000103, -79.84934566756000152, -0.7711480544179000196 ) ) ;
#50923 = CARTESIAN_POINT ( 'NONE',  ( -12.71658872084999992, -23.31584731985000047, -1.931087888240000217 ) ) ;
#50924 = EDGE_CURVE ( 'NONE', #45083, #16241, #55771, .T. ) ;
#50925 = CARTESIAN_POINT ( 'NONE',  ( 0.007752153121785848242, -76.57482323936264379, 11.74990054534275963 ) ) ;
#50926 = CARTESIAN_POINT ( 'NONE',  ( 3.277187423977000247, -80.84699166913398471, -2.586436307216999797 ) ) ;
#50928 = VECTOR ( 'NONE', #24664, 1000.000000000000000 ) ;
#50927 = CARTESIAN_POINT ( 'NONE',  ( -10.36221646771999971, -55.57876216348000042, 7.631895822728999690 ) ) ;
#50929 = CARTESIAN_POINT ( 'NONE',  ( 4.299985066278999568, -78.90906001420199800, 8.680515821880000260 ) ) ;
#50930 = CARTESIAN_POINT ( 'NONE',  ( -9.662176860537863732, -76.63657409603162307, -4.763807680900224106 ) ) ;
#50931 = CARTESIAN_POINT ( 'NONE',  ( -7.620037552712999762, -18.79433113555000290, -10.53559761427999852 ) ) ;
#50932 = AXIS2_PLACEMENT_3D ( 'NONE', #51201, #47071, #6307 ) ;
#50934 = CARTESIAN_POINT ( 'NONE',  ( -0.9151233253627000241, -78.28670764420459705, -0.9701162038759999495 ) ) ;
#50933 = CARTESIAN_POINT ( 'NONE',  ( -0.3926218265389256890, -78.79583333333334849, 1.460959015002472050 ) ) ;
#50935 = CARTESIAN_POINT ( 'NONE',  ( 12.00000000000000000, -78.16041666666669130, 1.570796326794922093 ) ) ;
#50936 = CARTESIAN_POINT ( 'NONE',  ( -1.250000000000000000, -80.59999999999999432, 0.000000000000000000 ) ) ;
#50937 = CARTESIAN_POINT ( 'NONE',  ( -3.370587613551000228, -1.830292672027000078, 0.9429417476038000068 ) ) ;
#50938 = CARTESIAN_POINT ( 'NONE',  ( 9.739528811734443181, -77.20000000000001705, -4.689215945816418873 ) ) ;
#50939 = VERTEX_POINT ( 'NONE', #5995 ) ;
#50940 = CARTESIAN_POINT ( 'NONE',  ( 1.439896632895334649, -78.33541666666666003, -10.99999999999999822 ) ) ;
#50941 = LINE ( 'NONE', #45935, #45506 ) ;
#50942 = CARTESIAN_POINT ( 'NONE',  ( -5.913068375556633782, -77.61521835660632007, 10.26311275136223244 ) ) ;
#50943 = CARTESIAN_POINT ( 'NONE',  ( 12.54902678216000034, -61.80971938179000347, -0.4616712539286000339 ) ) ;
#50944 = CARTESIAN_POINT ( 'NONE',  ( 1.799475304559999822, -57.04828923575999511, 12.69616050746999925 ) ) ;
#50945 = CARTESIAN_POINT ( 'NONE',  ( -1.338697082642999803, -78.06479906940001001, -12.94399764267999942 ) ) ;
#50946 = CARTESIAN_POINT ( 'NONE',  ( 10.74992915973507479, -79.35045861777548737, 0.04600403722853010913 ) ) ;
#50947 = CARTESIAN_POINT ( 'NONE',  ( 1.250000000000000000, -60.04999999966999980, -12.50000000000000000 ) ) ;
#50948 = CARTESIAN_POINT ( 'NONE',  ( -1.250000000000000000, -18.75000000000000000, 12.00000000000000000 ) ) ;
#50949 = CARTESIAN_POINT ( 'NONE',  ( 0.9943957917579000494, -77.87515876690598304, -11.12098945592000021 ) ) ;
#50950 =( GEOMETRIC_REPRESENTATION_CONTEXT ( 3 ) GLOBAL_UNCERTAINTY_ASSIGNED_CONTEXT ( ( #15398 ) ) GLOBAL_UNIT_ASSIGNED_CONTEXT ( ( #35539, #53568, #44132 ) ) REPRESENTATION_CONTEXT ( 'NONE', 'WORKASPACE' ) );
#50951 = CARTESIAN_POINT ( 'NONE',  ( 1.456666284817000001, -81.58220334850499000, -0.3834374542928999929 ) ) ;
#50952 = CARTESIAN_POINT ( 'NONE',  ( 4.598371993787000456, -78.81419514476064592, -8.567308531191999421 ) ) ;
#50954 = DIRECTION ( 'NONE',  ( 0.000000000000000000, 1.000000000000000000, 0.000000000000000000 ) ) ;
#50953 = CARTESIAN_POINT ( 'NONE',  ( -2.400634063566000176, -84.18579177382198964, 2.889347057923999706 ) ) ;
#50955 = CARTESIAN_POINT ( 'NONE',  ( -8.650571159592999493, -79.53504805011499457, 4.057379972786000266 ) ) ;
#50956 = CARTESIAN_POINT ( 'NONE',  ( 0.000000000000000000, -80.79999999999999716, -6.099999999999782041 ) ) ;
#50957 = FACE_BOUND ( 'NONE', #28065, .T. ) ;
#50958 = EDGE_CURVE ( 'NONE', #35853, #50685, #32183, .T. ) ;
#50959 = CARTESIAN_POINT ( 'NONE',  ( -3.630949683904999947, -76.04999999999999716, 11.17491406647000041 ) ) ;
#50960 = CARTESIAN_POINT ( 'NONE',  ( 7.069026043852319141, -79.73437500013776003, -6.033943149941224604 ) ) ;
#50961 = EDGE_LOOP ( 'NONE', ( #43337, #23560, #51842, #31621, #27015, #24618, #32635, #7248, #32171, #41151 ) ) ;
#50962 = ORIENTED_EDGE ( 'NONE', *, *, #38706, .T. ) ;
#50963 = CARTESIAN_POINT ( 'NONE',  ( 4.847151869481000297, -79.04368020031598974, 11.00961342987999991 ) ) ;
#50964 = PLANE ( 'NONE',  #35915 ) ;
#50965 = CARTESIAN_POINT ( 'NONE',  ( 12.00000000000000000, -75.80000000000001137, -2.990830162875999918E-13 ) ) ;
#50966 = ORIENTED_EDGE ( 'NONE', *, *, #40673, .F. ) ;
#50967 = CARTESIAN_POINT ( 'NONE',  ( -3.532272164985999829, -77.52231996340199771, 11.39993665757999963 ) ) ;
#50968 = EDGE_LOOP ( 'NONE', ( #6781, #61, #23566 ) ) ;
#50969 = B_SPLINE_SURFACE_WITH_KNOTS ( 'NONE', 3, 3, ( 
 ( #43509, #21064, #57079, #16643, #58239, #23392, #40527, #18972, #10116, #32518, #27514, #45261, #27222, #45852, #23100, #36094, #41110, #9236, #49690 ),
 ( #41404, #412, #53819, #701, #40820, #13945, #18098, #32231, #50273, #40227, #13652, #4809, #35788, #18683, #22809, #9821, #54111, #13355, #36963 ),
 ( #31647, #31353, #36675, #26930, #121, #49985, #31941, #17802, #18390, #36381, #54407, #9529, #14233, #49394, #45555, #5101, #54691, #44961, #28096 ),
 ( #46145, #27805, #987, #54976, #14525, #5670, #50562, #8943, #4516, #22517, #50858, #55860, #28682, #51150, #24268, #41693, #10705, #38128, #46734 ) ),
 .UNSPECIFIED., .F., .F., .F.,
 ( 4, 4 ),
 ( 4, 1, 1, 1, 1, 1, 1, 1, 1, 1, 1, 1, 1, 1, 1, 1, 4 ),
 ( -0.1772706441294000235, 1.177270644128999955 ),
 ( -0.008015739112864999488, 0.01803541300395000019, 0.04408656512076000039, 0.07013771723757000753, 0.09618886935437999386, 0.1222400214711999999, 0.1482911735880000081, 0.1743423257047999886, 0.2003934778215999968, 0.2264446299384000050, 0.2524957820552999888, 0.2785469341721000247, 0.3045980862889000051, 0.3306492384056999856, 0.3567003905224999660, 0.3827515426393000020, 0.4088026947561000379 ),
 .UNSPECIFIED. ) ;
#50970 = ORIENTED_EDGE ( 'NONE', *, *, #46657, .T. ) ;
#50971 = CIRCLE ( 'NONE', #33952, 10.34999999999999964 ) ;
#50972 = CARTESIAN_POINT ( 'NONE',  ( -10.75000000000000000, -79.00000000000000000, 0.000000000000000000 ) ) ;
#50973 = TOROIDAL_SURFACE ( 'NONE', #25495, 8.500000000000000000, 2.000000000000000000 ) ;
#50974 = ORIENTED_EDGE ( 'NONE', *, *, #57349, .T. ) ;
#50975 = CARTESIAN_POINT ( 'NONE',  ( -3.543871218327000250, -80.17042173478499478, 0.1598027556938000082 ) ) ;
#50976 = LINE ( 'NONE', #46267, #24199 ) ;
#50977 = EDGE_LOOP ( 'NONE', ( #3523, #44649, #40574, #13182 ) ) ;
#50978 = CARTESIAN_POINT ( 'NONE',  ( 0.9194760088113610452, -82.79137680920143794, -0.8462349433019908940 ) ) ;
#50979 = CARTESIAN_POINT ( 'NONE',  ( -7.627487525399000212, -55.50221245779999890, 10.35845608624000036 ) ) ;
#50981 = ADVANCED_FACE ( 'NONE', ( #10739 ), #1589, .T. ) ;
#50980 = EDGE_LOOP ( 'NONE', ( #42459, #51713, #56176, #25074, #40877, #41273 ) ) ;
#50982 = DIRECTION ( 'NONE',  ( 0.000000000000000000, 1.000000000000000000, 0.000000000000000000 ) ) ;
#50983 = CARTESIAN_POINT ( 'NONE',  ( 3.248398814366682430, -78.19774372165396414, 9.144491945039828096 ) ) ;
#50984 = CARTESIAN_POINT ( 'NONE',  ( -0.6606141896019371851, -79.80000000000001137, -11.78048067788835773 ) ) ;
#50985 = CARTESIAN_POINT ( 'NONE',  ( -10.63937949802054383, -80.08894649173862490, 1.537974160709378202 ) ) ;
#50986 = CARTESIAN_POINT ( 'NONE',  ( 6.688842324857636079, -78.77930637062392805, 10.27946156281801571 ) ) ;
#50987 = CARTESIAN_POINT ( 'NONE',  ( -7.456816947376000648, -78.69473898445177440, 6.210200510404997765 ) ) ;
#50988 = CARTESIAN_POINT ( 'NONE',  ( 10.97835188747000146, -76.00083456611598365, -2.133021021907000048 ) ) ;
#50989 = CARTESIAN_POINT ( 'NONE',  ( -5.237477409016258356, -76.51604757055756068, 9.510330503777982614 ) ) ;
#50990 = B_SPLINE_CURVE_WITH_KNOTS ( 'NONE', 3,
 ( #46968, #6496, #24506, #42522, #2090, #20088, #38080, #53388, #45140, #31521, #12371, #49264 ),
 .UNSPECIFIED., .F., .F.,
 ( 4, 2, 2, 2, 2, 4 ),
 ( 0.000000000000000000, 0.2500000000000000000, 0.5000000000000000000, 0.7500000000000000000, 0.8750000000000000000, 1.000000000000000000 ),
 .UNSPECIFIED. ) ;
#50991 = CARTESIAN_POINT ( 'NONE',  ( -7.640030264136999705, -55.49283319101999723, -10.18491080491000034 ) ) ;
#50992 = ADVANCED_FACE ( 'NONE', ( #52905 ), #14281, .F. ) ;
#50993 = CARTESIAN_POINT ( 'NONE',  ( -6.532098792667899723, -78.66264509723824006, -6.549319641915878343 ) ) ;
#50994 = CARTESIAN_POINT ( 'NONE',  ( 5.036904867883157166, -76.53953860386789643, 10.61617713185392908 ) ) ;
#50995 = AXIS2_PLACEMENT_3D ( 'NONE', #5410, #32255, #50300 ) ;
#50996 = CARTESIAN_POINT ( 'NONE',  ( 4.194094809819000069, -77.90806001420200744, 8.205866028503001175 ) ) ;
#50997 = CARTESIAN_POINT ( 'NONE',  ( 0.3292142484335000563, -79.27918825649700807, -1.292352404326999826 ) ) ;
#50998 = EDGE_CURVE ( 'NONE', #55898, #13579, #43768, .T. ) ;
#50999 = CARTESIAN_POINT ( 'NONE',  ( -6.333048277618449795, -80.17656323135794594, -8.998749364487563795 ) ) ;
#51000 = CARTESIAN_POINT ( 'NONE',  ( 0.5999999999999999778, -23.15000000000000213, -10.98362417419999915 ) ) ;
#51001 = CARTESIAN_POINT ( 'NONE',  ( -1.390911224239000044, -81.80467549782599690, -3.888944045958999673 ) ) ;
#51002 = CARTESIAN_POINT ( 'NONE',  ( -9.486170818179999742, -77.70791332859900535, -1.784886728388999977 ) ) ;
#51003 = CARTESIAN_POINT ( 'NONE',  ( 0.000000000000000000, -76.00000000000000000, 0.000000000000000000 ) ) ;
#51004 = CARTESIAN_POINT ( 'NONE',  ( 0.3908001115028792993, -82.94971160634423768, 1.187542448887068725 ) ) ;
#51005 = LINE ( 'NONE', #32089, #42441 ) ;
#51006 = CARTESIAN_POINT ( 'NONE',  ( -3.699999999670000150, -79.00321104920828930, -1.552506213169860872E-14 ) ) ;
#51007 = CARTESIAN_POINT ( 'NONE',  ( -7.374560639699019760, -79.32708333333330586, 9.596002108778129980 ) ) ;
#51008 = CARTESIAN_POINT ( 'NONE',  ( -7.919595949288999570, -55.64999999964999233, 9.050966799188000067 ) ) ;
#51009 = CARTESIAN_POINT ( 'NONE',  ( 0.000000000000000000, -0.2000000000000000111, 0.000000000000000000 ) ) ;
#51010 = CARTESIAN_POINT ( 'NONE',  ( -10.42531125068999920, -23.26485145404000221, 7.624341767093000044 ) ) ;
#51011 = CARTESIAN_POINT ( 'NONE',  ( -0.9184750406504611497, -79.77639907747951042, 1.199933283862223421 ) ) ;
#51012 = FACE_OUTER_BOUND ( 'NONE', #55688, .T. ) ;
#51013 = CARTESIAN_POINT ( 'NONE',  ( -3.230363664242999810, -78.16799805011500268, -9.171071524558000121 ) ) ;
#51014 = DIRECTION ( 'NONE',  ( -1.776356839400000238E-14, -1.000000000000000000, -1.184237892933000067E-14 ) ) ;
#51015 = VECTOR ( 'NONE', #32071, 1000.000000000000000 ) ;
#51016 = CARTESIAN_POINT ( 'NONE',  ( 12.27743704900000132, -77.62500106391100019, 0.2455986337158999888 ) ) ;
#51017 = EDGE_CURVE ( 'NONE', #12253, #34855, #53605, .T. ) ;
#51018 = CARTESIAN_POINT ( 'NONE',  ( -0.5135400118894599686, -25.17868533858884561, -12.70453250099059872 ) ) ;
#51019 = CARTESIAN_POINT ( 'NONE',  ( 4.287309447300000187, -76.40953882784999962, -11.27418668890000042 ) ) ;
#51020 = VERTEX_POINT ( 'NONE', #30449 ) ;
#51021 = B_SPLINE_SURFACE_WITH_KNOTS ( 'NONE', 3, 3, ( 
 ( #38363, #2371, #33922, #51384 ),
 ( #47831, #56385, #56672, #6493 ),
 ( #21222, #33640, #38938, #11518 ),
 ( #11229, #10941, #7648, #51681 ),
 ( #29496, #29775, #12083, #39227 ),
 ( #25647, #16515, #42808, #38653 ),
 ( #29208, #57240, #7362, #47551 ),
 ( #2937, #52526, #47255, #7076 ),
 ( #33351, #25362, #34207, #25078 ),
 ( #43102, #43378, #42519, #2087 ),
 ( #56098, #15644, #6786, #58109 ),
 ( #27099, #53385, #22387, #48968 ),
 ( #13525, #31221, #35359, #4388 ),
 ( #17970, #12652, #26226, #21796 ),
 ( #53688, #44528, #57814, #17373 ),
 ( #12931, #4084, #4686, #40398 ),
 ( #57425, #44832, #17672, #45136 ) ),
 .UNSPECIFIED., .F., .F., .F.,
 ( 4, 1, 1, 1, 1, 1, 1, 1, 1, 1, 1, 1, 1, 1, 4 ),
 ( 4, 4 ),
 ( -0.01011786823685000003, 0.000000000000000000, 0.08333333333333001192, 0.1666666666667000196, 0.2500000000000000000, 0.3333333333333000081, 0.4166666666666999919, 0.5000000000000000000, 0.5833333333333000637, 0.6666666666667000474, 0.7500000000000000000, 0.8333333333333000637, 0.9166666666667000474, 1.000000000000000000, 1.010371592463000123 ),
 ( -0.3559705548529999986, 1.357613344763000107 ),
 .UNSPECIFIED. ) ;
#51022 = CARTESIAN_POINT ( 'NONE',  ( -1.664832167514000094, -85.27621544543099219, -3.596430821289000157 ) ) ;
#51023 = CARTESIAN_POINT ( 'NONE',  ( -1.111829811609999830, -80.32601340704829340, -11.23414193798999960 ) ) ;
#51024 = CARTESIAN_POINT ( 'NONE',  ( 8.350655305475967793, -78.31463735380187074, -3.978570201286235619 ) ) ;
#51025 = DIRECTION ( 'NONE',  ( 0.000000000000000000, -1.000000000000000000, 0.000000000000000000 ) ) ;
#51026 = CARTESIAN_POINT ( 'NONE',  ( 11.19952915612999966, -78.14725770227899204, -0.6234238306063999424 ) ) ;
#51027 = CARTESIAN_POINT ( 'NONE',  ( 9.713032445540614290, -24.52293762691880374, -7.970418356296344875 ) ) ;
#51028 = CARTESIAN_POINT ( 'NONE',  ( -4.441436338936000539, -78.97991978438899707, -8.545575054271999704 ) ) ;
#51029 = CARTESIAN_POINT ( 'NONE',  ( -0.5544740949720999845, -82.29082582312000227, 1.570928860995999932 ) ) ;
#51030 = CARTESIAN_POINT ( 'NONE',  ( 4.000000000000000000, -78.72610001270986402, 0.000000000000000000 ) ) ;
#51031 = CARTESIAN_POINT ( 'NONE',  ( 9.966176356049450291, -81.00000000000000000, -4.720956196838709928 ) ) ;
#51032 = ORIENTED_EDGE ( 'NONE', *, *, #38408, .T. ) ;
#51033 = EDGE_CURVE ( 'NONE', #34714, #47194, #21028, .T. ) ;
#51034 = PLANE ( 'NONE',  #24916 ) ;
#51035 = CARTESIAN_POINT ( 'NONE',  ( 5.620590082324000036, -80.36488510293838772, -9.763102121971000358 ) ) ;
#51036 = CARTESIAN_POINT ( 'NONE',  ( 2.887050208512827787, -78.99159464002811148, -2.426921481828515859 ) ) ;
#51037 = VERTEX_POINT ( 'NONE', #29582 ) ;
#51038 = EDGE_CURVE ( 'NONE', #18787, #37143, #2954, .T. ) ;
#51039 = CARTESIAN_POINT ( 'NONE',  ( -1.159125165887999964, -77.64758214605309661, 0.4678983327651999868 ) ) ;
#51040 = CARTESIAN_POINT ( 'NONE',  ( -9.222505265117137085, -77.51202912837678127, -1.397969593980213476 ) ) ;
#51041 = DIRECTION ( 'NONE',  ( 1.000000000000000000, 0.000000000000000000, 0.000000000000000000 ) ) ;
#51042 = ORIENTED_EDGE ( 'NONE', *, *, #30527, .T. ) ;
#51043 = CIRCLE ( 'NONE', #9510, 13.94827586206999825 ) ;
#51044 = CARTESIAN_POINT ( 'NONE',  ( -7.733454931756999606, -78.68868807833099766, 9.390218602554998739 ) ) ;
#51045 = CARTESIAN_POINT ( 'NONE',  ( -1.346801222098000128, -77.94142625569698168, 11.24181324638000135 ) ) ;
#51046 = CARTESIAN_POINT ( 'NONE',  ( -1.799475304559999822, -21.75171076523999858, 12.69616050742999924 ) ) ;
#51047 = VERTEX_POINT ( 'NONE', #57330 ) ;
#51048 = ORIENTED_EDGE ( 'NONE', *, *, #38593, .T. ) ;
#51049 = CARTESIAN_POINT ( 'NONE',  ( -1.229694712338595508, -80.58624861086376256, 0.2234822223714939271 ) ) ;
#51050 = CARTESIAN_POINT ( 'NONE',  ( -13.94764600793045517, -33.10361340872000113, -0.1325532415315603119 ) ) ;
#51051 = CARTESIAN_POINT ( 'NONE',  ( 6.653382217586999658, -79.70582034720699482, 7.150748904218000135 ) ) ;
#51052 = ORIENTED_EDGE ( 'NONE', *, *, #36384, .F. ) ;
#51053 = CARTESIAN_POINT ( 'NONE',  ( -7.970415440577942157, -54.27707676769661305, 9.713035532171998554 ) ) ;
#51054 = CARTESIAN_POINT ( 'NONE',  ( 10.18248259416120938, -24.29095036201641022, -7.792398156871034764 ) ) ;
#51055 = ORIENTED_EDGE ( 'NONE', *, *, #29337, .F. ) ;
#51056 = AXIS2_PLACEMENT_3D ( 'NONE', #47486, #5842, #19433 ) ;
#51057 = CARTESIAN_POINT ( 'NONE',  ( 2.787247272279751886, -80.74587480725163857, -10.40638828497226953 ) ) ;
#51058 = CARTESIAN_POINT ( 'NONE',  ( 9.621717086613145398, -24.62064477552555175, 8.060172378175863628 ) ) ;
#51059 = VECTOR ( 'NONE', #55157, 1000.000000000000114 ) ;
#51060 = CARTESIAN_POINT ( 'NONE',  ( 3.365092916910764398, -82.58831665972199687, -0.7152753179581305965 ) ) ;
#51061 = CARTESIAN_POINT ( 'NONE',  ( 1.495357591784101325, -17.44123662637737837, -12.70444646759294116 ) ) ;
#51062 = DIRECTION ( 'NONE',  ( 0.000000000000000000, -1.000000000000000000, 0.000000000000000000 ) ) ;
#51063 = CARTESIAN_POINT ( 'NONE',  ( -0.5677917205621726415, -86.25171438276198899, 4.566314625519950710 ) ) ;
#51064 = CARTESIAN_POINT ( 'NONE',  ( 9.532486246840001343, -76.90082656998458788, -2.044978076835000103 ) ) ;
#51065 = CARTESIAN_POINT ( 'NONE',  ( 1.523426795032935654, -78.58841195298964521, -0.2098259862101924111 ) ) ;
#51066 = ADVANCED_FACE ( 'NONE', ( #2172 ), #8025, .T. ) ;
#51067 = CARTESIAN_POINT ( 'NONE',  ( 2.081936059911246861, -80.70416666796184302, -3.476221075145997208 ) ) ;
#51068 = CARTESIAN_POINT ( 'NONE',  ( -6.024415200221000077, -76.43302873236000039, 10.73507988388000101 ) ) ;
#51069 = CARTESIAN_POINT ( 'NONE',  ( -0.2056945464814999847, -80.79322239898399971, 1.601533168507999871 ) ) ;
#51070 = EDGE_CURVE ( 'NONE', #41164, #22489, #3615, .T. ) ;
#51071 = DIRECTION ( 'NONE',  ( 0.000000000000000000, 0.000000000000000000, -1.000000000000000000 ) ) ;
#51072 = CARTESIAN_POINT ( 'NONE',  ( 7.633501923173000137, -60.00104675737999571, -10.36289748054999826 ) ) ;
#51073 = CARTESIAN_POINT ( 'NONE',  ( 9.000511195990998914, -79.36010635638000110, 8.067084866081000172 ) ) ;
#51074 = CARTESIAN_POINT ( 'NONE',  ( 6.725657209017000149, -77.23867228970199506, -9.843613558058999402 ) ) ;
#51075 = CARTESIAN_POINT ( 'NONE',  ( 6.055527902613000002, -78.11999999999999034, 7.319875806370000682 ) ) ;
#51076 = CARTESIAN_POINT ( 'NONE',  ( -10.14999999999999858, -87.09999999999999432, 0.000000000000000000 ) ) ;
#51077 = CARTESIAN_POINT ( 'NONE',  ( 6.044717002249641702, -77.88304938243121001, 10.38669683180858527 ) ) ;
#51078 = CARTESIAN_POINT ( 'NONE',  ( -5.268979267983999293, -78.66391321173168194, 9.902321347348999936 ) ) ;
#51079 = ORIENTED_EDGE ( 'NONE', *, *, #29959, .F. ) ;
#51080 = CARTESIAN_POINT ( 'NONE',  ( -1.281643947269487605, -81.20542284418931445, 0.8013805647649642205 ) ) ;
#51081 = CARTESIAN_POINT ( 'NONE',  ( -9.463706838924000664, -77.33890260894099811, -1.161272537025000107 ) ) ;
#51082 = CARTESIAN_POINT ( 'NONE',  ( 10.42531124905999995, -23.26485148473999942, 7.624341765453999997 ) ) ;
#51083 = LINE ( 'NONE', #42216, #38065 ) ;
#51084 = CARTESIAN_POINT ( 'NONE',  ( -2.631409671617999990, -2.359887446210000128, -2.838311312396000208 ) ) ;
#51085 = CARTESIAN_POINT ( 'NONE',  ( -6.817533650000999756, -78.08600697782200939, -9.935643240620999350 ) ) ;
#51086 = CARTESIAN_POINT ( 'NONE',  ( -0.5506691749702000704, -77.82738533478698173, -9.615090921292999582 ) ) ;
#51087 = EDGE_CURVE ( 'NONE', #18726, #20471, #34996, .T. ) ;
#51089 = CARTESIAN_POINT ( 'NONE',  ( 1.229229935955506336, -77.05286458334455801, 9.397135416926557738 ) ) ;
#51088 = CARTESIAN_POINT ( 'NONE',  ( -4.168399266842356177, -76.10359643177146438, 10.99644600840660758 ) ) ;
#51090 = CARTESIAN_POINT ( 'NONE',  ( -0.4696505103051999974, -82.67677767037399406, -1.267043746813000249 ) ) ;
#51091 = CARTESIAN_POINT ( 'NONE',  ( -2.611770760767388566, -85.80681307243297340, 3.525481195051840100 ) ) ;
#51092 = VERTEX_POINT ( 'NONE', #38743 ) ;
#51093 = CARTESIAN_POINT ( 'NONE',  ( 12.71005379439144178, -24.29489531514696665, 1.687596143071744770 ) ) ;
#51094 = EDGE_CURVE ( 'NONE', #16896, #44068, #9579, .T. ) ;
#51095 = CARTESIAN_POINT ( 'NONE',  ( 9.499549289235639904, -79.50042064254546403, 0.05021470316550929319 ) ) ;
#51096 = CARTESIAN_POINT ( 'NONE',  ( -5.917523019358058356, -76.88333333333329733, -10.26699006316253282 ) ) ;
#51097 = VECTOR ( 'NONE', #57278, 1000.000000000000000 ) ;
#51098 = CARTESIAN_POINT ( 'NONE',  ( 10.85730540529999999, -79.25214891444099408, 1.607151491820999922 ) ) ;
#51099 = CARTESIAN_POINT ( 'NONE',  ( -0.5328894382976427924, -79.19002943946934181, -1.131072528211912953 ) ) ;
#51100 = CARTESIAN_POINT ( 'NONE',  ( -10.68954194898181775, -80.08091480521125050, 2.624713457052874510 ) ) ;
#51101 = CARTESIAN_POINT ( 'NONE',  ( 3.185501216392000234, -79.99134998740498759, 9.130619404448999887 ) ) ;
#51102 = CARTESIAN_POINT ( 'NONE',  ( 10.18948933931999967, -18.78467389927000042, -7.645397892299000020 ) ) ;
#51103 = CARTESIAN_POINT ( 'NONE',  ( 8.696932689530999738, -76.29999999999999716, 6.318691462144000681 ) ) ;
#51104 = VERTEX_POINT ( 'NONE', #43191 ) ;
#51105 = CONICAL_SURFACE ( 'NONE', #25612, 10.09999999997999964, 0.7853981633972997312 ) ;
#51106 = CARTESIAN_POINT ( 'NONE',  ( -10.99991520232270936, -76.33543575793046898, 2.019904293929638772 ) ) ;
#51107 = CARTESIAN_POINT ( 'NONE',  ( 10.47020627418438643, -79.77083333333332860, 2.813789756862283387 ) ) ;
#51108 = CARTESIAN_POINT ( 'NONE',  ( 9.422193216980595309, -77.25680711302858583, 7.547672206128430261 ) ) ;
#51109 = EDGE_CURVE ( 'NONE', #6729, #56422, #16285, .T. ) ;
#51110 = LINE ( 'NONE', #10664, #11026 ) ;
#51111 = CARTESIAN_POINT ( 'NONE',  ( -11.06509191825306004, -79.36302061774877359, -1.839932010799510964 ) ) ;
#51112 = FACE_OUTER_BOUND ( 'NONE', #40577, .T. ) ;
#51113 = DIRECTION ( 'NONE',  ( 0.000000000000000000, 1.000000000000000000, 0.000000000000000000 ) ) ;
#51114 = CARTESIAN_POINT ( 'NONE',  ( -0.8488654463164000408, -78.64882235081999795, -0.9950929470245999386 ) ) ;
#51115 = CARTESIAN_POINT ( 'NONE',  ( 8.696932689530999738, -76.29999999999999716, 6.318691462144000681 ) ) ;
#51116 = CARTESIAN_POINT ( 'NONE',  ( 3.303053640057958429, -79.09942690050905867, -10.46697929272314731 ) ) ;
#51117 = EDGE_CURVE ( 'NONE', #7313, #47577, #16322, .T. ) ;
#51118 = DIRECTION ( 'NONE',  ( 0.000000000000000000, 1.000000000000000000, 0.000000000000000000 ) ) ;
#51119 = EDGE_LOOP ( 'NONE', ( #5858, #37005, #51565, #3244 ) ) ;
#51120 = EDGE_LOOP ( 'NONE', ( #40422, #1487, #42690 ) ) ;
#51121 = CARTESIAN_POINT ( 'NONE',  ( -0.5475862000146000108, -78.49998998579799547, -10.00738244094000073 ) ) ;
#51122 = CARTESIAN_POINT ( 'NONE',  ( 7.815245125686015371, -78.78981169969108578, -7.382265784365210415 ) ) ;
#51123 = ORIENTED_EDGE ( 'NONE', *, *, #31916, .F. ) ;
#51124 = CARTESIAN_POINT ( 'NONE',  ( 9.934825859755001431, -17.37633188891999936, 7.968960864700001423 ) ) ;
#51125 = CARTESIAN_POINT ( 'NONE',  ( 0.000000000000000000, -9.295797029142999435, 0.000000000000000000 ) ) ;
#51126 = CARTESIAN_POINT ( 'NONE',  ( -7.209704553483001099, -78.17110306078001258, 9.484251963051999468 ) ) ;
#51127 = CARTESIAN_POINT ( 'NONE',  ( 9.830801209645999350, -60.89088557979000171, 7.765011064359000237 ) ) ;
#51128 = CARTESIAN_POINT ( 'NONE',  ( -1.127572418632452944, -76.93174530860108007, 12.14745662550945760 ) ) ;
#51129 = CARTESIAN_POINT ( 'NONE',  ( 11.97758669317381930, -77.80149520948634745, 0.2396004080751424348 ) ) ;
#51130 = CARTESIAN_POINT ( 'NONE',  ( 5.865103843792000227, -78.50268001718499988, -9.561319920857000554 ) ) ;
#51131 = ORIENTED_EDGE ( 'NONE', *, *, #41988, .F. ) ;
#51132 = CARTESIAN_POINT ( 'NONE',  ( -8.532660243322236937, -25.12798380540222709, 9.433531203469305737 ) ) ;
#51133 = VERTEX_POINT ( 'NONE', #52336 ) ;
#51134 = CARTESIAN_POINT ( 'NONE',  ( 7.827287555285567855, -77.39497157051955867, 4.939251125549445121 ) ) ;
#51135 = CARTESIAN_POINT ( 'NONE',  ( -5.876696946710000091, -77.57078597849198331, -9.346046374399000101 ) ) ;
#51136 = AXIS2_PLACEMENT_3D ( 'NONE', #37027, #10180, #37902 ) ;
#51137 = CARTESIAN_POINT ( 'NONE',  ( 1.508441505249127790, -77.71417431448334412, 11.11513442064821966 ) ) ;
#51138 = EDGE_CURVE ( 'NONE', #27991, #30862, #34592, .T. ) ;
#51139 = CARTESIAN_POINT ( 'NONE',  ( -1.140592747978000032, -79.04901557144499691, -0.9947442812858000583 ) ) ;
#51140 = CARTESIAN_POINT ( 'NONE',  ( -1.826212728074999792, -76.35785197021000670, -12.51879797594000010 ) ) ;
#51141 = CARTESIAN_POINT ( 'NONE',  ( 0.000000000000000000, -79.99999999999998579, 0.000000000000000000 ) ) ;
#51142 = CARTESIAN_POINT ( 'NONE',  ( 1.328072050606999843, -78.58978245110000671, -0.9406846882429998891 ) ) ;
#51143 = CARTESIAN_POINT ( 'NONE',  ( 0.2631036358232000105, -79.61995726186898992, -11.04575348828999992 ) ) ;
#51144 = CARTESIAN_POINT ( 'NONE',  ( -9.292748675297000105, -77.02431167140100854, -2.067979918156000352 ) ) ;
#51145 = CARTESIAN_POINT ( 'NONE',  ( 2.062673488738000049, -60.12452529330000317, -12.82904091341000097 ) ) ;
#51146 = CARTESIAN_POINT ( 'NONE',  ( 8.244744731391815407, -79.09176881386157731, 4.761212502374692512 ) ) ;
#51147 = CARTESIAN_POINT ( 'NONE',  ( 3.086296569003000201, -85.51626360600299392, 1.743485741791999999 ) ) ;
#51148 = ORIENTED_EDGE ( 'NONE', *, *, #28425, .T. ) ;
#51149 = CARTESIAN_POINT ( 'NONE',  ( -10.28202908126049664, -77.20000000000000284, 3.778194283757810190 ) ) ;
#51150 = CARTESIAN_POINT ( 'NONE',  ( -10.26075081888999918, -76.23781109130798939, 5.437666049857999617 ) ) ;
#51151 = CARTESIAN_POINT ( 'NONE',  ( 9.337418898828111935, -77.89153506836979091, 5.340059034472213639 ) ) ;
#51152 = CARTESIAN_POINT ( 'NONE',  ( -11.48784787867999846, -78.08899053812999114, -3.397854551190000016 ) ) ;
#51153 = CARTESIAN_POINT ( 'NONE',  ( -8.252512830340000605, -17.06594982557999884, 9.650910120430999939 ) ) ;
#51154 = CARTESIAN_POINT ( 'NONE',  ( -1.127782339217550778, -78.21133870775913977, 0.5953878299651829131 ) ) ;
#51155 = CARTESIAN_POINT ( 'NONE',  ( -2.550741782276678027, -2.812450179095209446, -2.527267954782760118 ) ) ;
#51156 = CARTESIAN_POINT ( 'NONE',  ( 10.28406176041941755, -80.87383273565515651, 3.134224279283850390 ) ) ;
#51157 = CARTESIAN_POINT ( 'NONE',  ( -0.1492691421716000055, -77.95544831538099118, 9.412168359664999429 ) ) ;
#51159 = ADVANCED_FACE ( 'NONE', ( #46035 ), #47273, .F. ) ;
#51158 = FACE_OUTER_BOUND ( 'NONE', #43482, .T. ) ;
#51160 = CARTESIAN_POINT ( 'NONE',  ( 5.066356038949999530, -77.79589325954400181, 9.799682181994000985 ) ) ;
#51161 = CARTESIAN_POINT ( 'NONE',  ( 12.07535958108000074, -76.88541377483805661, -2.237927141218000404 ) ) ;
#51162 = CARTESIAN_POINT ( 'NONE',  ( -10.48543666025109111, -78.34166666666665435, -6.043427764450793660 ) ) ;
#51163 = ORIENTED_EDGE ( 'NONE', *, *, #54172, .T. ) ;
#51164 = CIRCLE ( 'NONE', #268, 0.5000000000000006661 ) ;
#51165 = CARTESIAN_POINT ( 'NONE',  ( 0.1510373474112000070, -81.63162929444700922, 1.325052402434999888 ) ) ;
#51166 = CARTESIAN_POINT ( 'NONE',  ( 1.632307027704000157, -60.46927189524000568, -12.46200249215000078 ) ) ;
#51167 = DIRECTION ( 'NONE',  ( 1.000000000000000000, 0.000000000000000000, 0.000000000000000000 ) ) ;
#51168 = CARTESIAN_POINT ( 'NONE',  ( -2.309466437479000156, -77.65760813670300422, 10.97654204954999990 ) ) ;
#51169 = CARTESIAN_POINT ( 'NONE',  ( -4.399243655502999673, -79.71736428708098288, 10.05537673064999815 ) ) ;
#51170 = CARTESIAN_POINT ( 'NONE',  ( 7.645398488021999839, -23.21531609142999741, -10.18948971874999998 ) ) ;
#51171 = CARTESIAN_POINT ( 'NONE',  ( -3.522477044106106181, -86.08072918608876023, 1.921747906583619159 ) ) ;
#51172 = CARTESIAN_POINT ( 'NONE',  ( 7.929877441717000153, -77.26081807572799676, -8.610461240849000220 ) ) ;
#51173 = CARTESIAN_POINT ( 'NONE',  ( -10.27342224347103894, -54.73842478142423573, -7.712153330297224052 ) ) ;
#51174 = CARTESIAN_POINT ( 'NONE',  ( -2.682899408521000062, -83.38942953870899544, -3.195089342158999646 ) ) ;
#51175 = CARTESIAN_POINT ( 'NONE',  ( 0.3926218265389220807, -79.64583333333334281, -1.460959015002473382 ) ) ;
#51176 = ADVANCED_FACE ( 'NONE', ( #31832 ), #12385, .F. ) ;
#51177 = CARTESIAN_POINT ( 'NONE',  ( 7.619712398427999744, -55.39595871828999663, -10.35409979025000027 ) ) ;
#51178 = CARTESIAN_POINT ( 'NONE',  ( -7.012165219465999577, -77.20507517892998806, 8.812689912465000219 ) ) ;
#51179 = CARTESIAN_POINT ( 'NONE',  ( -1.387963714323000142, -79.78297531344000504, 0.9213108730841000904 ) ) ;
#51180 = DIRECTION ( 'NONE',  ( 0.000000000000000000, 1.000000000000000000, 0.000000000000000000 ) ) ;
#51181 = DIRECTION ( 'NONE',  ( 0.000000000000000000, 1.000000000000000000, 1.487781318828000208E-14 ) ) ;
#51182 = CARTESIAN_POINT ( 'NONE',  ( 1.411403051189575431, -81.52931625501098267, 0.5428011461610074972 ) ) ;
#51183 = CIRCLE ( 'NONE', #53051, 2.000000000000000000 ) ;
#51184 = CARTESIAN_POINT ( 'NONE',  ( 0.000000000000000000, -77.59999999938000315, 0.000000000000000000 ) ) ;
#51185 = VERTEX_POINT ( 'NONE', #49579 ) ;
#51186 = CARTESIAN_POINT ( 'NONE',  ( 0.9661093279367058972, -79.79552230973584415, -0.7934550806089618602 ) ) ;
#51187 = FACE_OUTER_BOUND ( 'NONE', #55672, .T. ) ;
#51188 = EDGE_CURVE ( 'NONE', #54320, #31102, #51980, .T. ) ;
#51189 = ORIENTED_EDGE ( 'NONE', *, *, #44879, .F. ) ;
#51190 = CARTESIAN_POINT ( 'NONE',  ( -1.032281996597182339, -81.64822189729572699, -0.7051746695584234503 ) ) ;
#51191 = EDGE_CURVE ( 'NONE', #21517, #20749, #5559, .T. ) ;
#51192 = CARTESIAN_POINT ( 'NONE',  ( 2.368087569675000115, -80.31630253886619641, 10.55620284977000090 ) ) ;
#51193 = CARTESIAN_POINT ( 'NONE',  ( -7.648026766715999791, -55.54999999381000464, -10.12290050087000104 ) ) ;
#51194 = VERTEX_POINT ( 'NONE', #45740 ) ;
#51195 = ORIENTED_EDGE ( 'NONE', *, *, #19257, .T. ) ;
#51196 = CARTESIAN_POINT ( 'NONE',  ( 0.7721134610030000456, -81.21483193069099116, -1.304907259309999956 ) ) ;
#51197 = ORIENTED_EDGE ( 'NONE', *, *, #50535, .T. ) ;
#51198 = LINE ( 'NONE', #40868, #37745 ) ;
#51199 = ORIENTED_EDGE ( 'NONE', *, *, #49843, .T. ) ;
#51200 = CARTESIAN_POINT ( 'NONE',  ( 0.9212224518303000487, -17.18045898161000196, 12.54670315981999984 ) ) ;
#51201 = CARTESIAN_POINT ( 'NONE',  ( 4.000000000000000000, -75.00000000000001421, 0.5999999999999999778 ) ) ;
#51202 = CARTESIAN_POINT ( 'NONE',  ( 0.000000000000000000, 0.000000000000000000, 0.000000000000000000 ) ) ;
#51203 = CARTESIAN_POINT ( 'NONE',  ( 0.2387542509232137289, -82.09166665063389701, -3.402624595228084026 ) ) ;
#51204 = AXIS2_PLACEMENT_3D ( 'NONE', #16163, #51318, #2022 ) ;
#51205 = CARTESIAN_POINT ( 'NONE',  ( 11.68767212001979594, -76.52916666666243373, -3.140974612311341563 ) ) ;
#51206 = CARTESIAN_POINT ( 'NONE',  ( 6.153210332247711634, -78.28297894785262656, -6.906877943483819671 ) ) ;
#51207 = DIRECTION ( 'NONE',  ( -1.000000000000000000, 0.000000000000000000, 0.000000000000000000 ) ) ;
#51208 = ORIENTED_EDGE ( 'NONE', *, *, #1472, .F. ) ;
#51209 = ORIENTED_EDGE ( 'NONE', *, *, #26606, .F. ) ;
#51210 = CARTESIAN_POINT ( 'NONE',  ( -9.137867255240424313, -77.58773879498612303, 1.435393631043841989 ) ) ;
#51211 = CARTESIAN_POINT ( 'NONE',  ( -0.7681833999686477066, -81.42708333333332860, 0.9995835529977223910 ) ) ;
#51212 = EDGE_CURVE ( 'NONE', #29156, #54663, #9127, .T. ) ;
#51213 = CARTESIAN_POINT ( 'NONE',  ( 1.217390015787464197, -61.61893024884950165, -12.70229597944889299 ) ) ;
#51214 = CARTESIAN_POINT ( 'NONE',  ( -7.843978203195000276, -77.71975302678599462, 5.713380375430999969 ) ) ;
#51215 = FACE_OUTER_BOUND ( 'NONE', #54159, .T. ) ;
#51216 = CARTESIAN_POINT ( 'NONE',  ( 0.9995835529977233902, -79.80208333333334281, 0.7681833999686461523 ) ) ;
#51217 = CARTESIAN_POINT ( 'NONE',  ( -6.043427764450833628, -76.81666666666666288, 10.48543666025107335 ) ) ;
#51218 = CARTESIAN_POINT ( 'NONE',  ( -1.376297233339999870, -80.16529921676999493, 0.7875294559552000750 ) ) ;
#51219 = CARTESIAN_POINT ( 'NONE',  ( 8.838834764832000701, -23.25000000000000000, 8.838834764832000701 ) ) ;
#51220 = CARTESIAN_POINT ( 'NONE',  ( -1.516401113037979309, -76.58467496875395852, 11.74961971174281672 ) ) ;
#51221 = CARTESIAN_POINT ( 'NONE',  ( 9.151068819668228826, -79.24609374760862579, -7.813608010562005823 ) ) ;
#51223 = TOROIDAL_SURFACE ( 'NONE', #30450, 13.50000000000000000, 0.5000000000000000000 ) ;
#51222 = CARTESIAN_POINT ( 'NONE',  ( -10.35398565885000011, -55.39211376237999929, 7.619387877908000206 ) ) ;
#51224 = CARTESIAN_POINT ( 'NONE',  ( 8.188916213828999702, -78.86551001420200180, 5.175217742376999830 ) ) ;
#51225 = CARTESIAN_POINT ( 'NONE',  ( -10.97916666637321192, -80.22083333335037025, -1.151917308728376499 ) ) ;
#51226 = CARTESIAN_POINT ( 'NONE',  ( -7.647736468634000140, -18.27704514451999884, -10.13404651205999940 ) ) ;
#51228 = CARTESIAN_POINT ( 'NONE',  ( 14.00000000000000000, -32.66217755555999958, 5.544640309757999441E-06 ) ) ;
#51227 = DIRECTION ( 'NONE',  ( -1.000000000000000000, 0.000000000000000000, 0.000000000000000000 ) ) ;
#51229 = CARTESIAN_POINT ( 'NONE',  ( -12.00000000000000000, -78.39999999999999147, 0.000000000000000000 ) ) ;
#51230 = LINE ( 'NONE', #10782, #12789 ) ;
#51231 = CARTESIAN_POINT ( 'NONE',  ( -6.912545260079999920, -78.39582039176799810, -8.891046157644998615 ) ) ;
#51232 = CARTESIAN_POINT ( 'NONE',  ( -3.517875660386507342, -1.245963598631521396, 0.1758881523666950553 ) ) ;
#51233 = ORIENTED_EDGE ( 'NONE', *, *, #47920, .T. ) ;
#51234 = CARTESIAN_POINT ( 'NONE',  ( 8.813891479838931176, -61.81010130340824560, 8.872963529851991993 ) ) ;
#51235 = CONICAL_SURFACE ( 'NONE', #5988, 1.249999999985999866, 0.7853981633972997312 ) ;
#51236 = CARTESIAN_POINT ( 'NONE',  ( 11.75000000000000000, -77.45000000000000284, 1.043320980279999928E-14 ) ) ;
#51237 = CARTESIAN_POINT ( 'NONE',  ( 1.182180303898404006, -78.37658685848882101, 0.4056014702486911983 ) ) ;
#51238 = CARTESIAN_POINT ( 'NONE',  ( 8.462293916759000112, -79.74502648735098376, 4.390897894491000208 ) ) ;
#51239 = CARTESIAN_POINT ( 'NONE',  ( 12.52785477537251246, -18.20586572947235382, -1.668513103012997600 ) ) ;
#51240 = CARTESIAN_POINT ( 'NONE',  ( 9.448045098518800700, -79.38977526190863898, 5.154015187206609561 ) ) ;
#51241 = AXIS2_PLACEMENT_3D ( 'NONE', #55724, #37404, #55425 ) ;
#51242 = CARTESIAN_POINT ( 'NONE',  ( 0.000000000000000000, -5.899999999999999467, 0.000000000000000000 ) ) ;
#51243 = VECTOR ( 'NONE', #49862, 1000.000000000000114 ) ;
#51244 = EDGE_CURVE ( 'NONE', #46717, #1524, #36274, .T. ) ;
#51245 = CARTESIAN_POINT ( 'NONE',  ( 0.000000000000000000, -69.16102867818000277, 0.000000000000000000 ) ) ;
#51246 = CARTESIAN_POINT ( 'NONE',  ( -6.629376284316999879, -77.75416360879198407, -9.119063026537000738 ) ) ;
#51247 = EDGE_CURVE ( 'NONE', #42116, #48636, #175, .T. ) ;
#51248 = CARTESIAN_POINT ( 'NONE',  ( -1.490129969386999820, -81.86435186793200103, -0.2200309544077999890 ) ) ;
#51249 = CARTESIAN_POINT ( 'NONE',  ( -0.08911090410158063746, -81.98124066240951890, 1.246717735211338107 ) ) ;
#51250 = CARTESIAN_POINT ( 'NONE',  ( -0.5382333298950999767, -78.14126107556998591, -9.397951872088000869 ) ) ;
#51252 = LINE ( 'NONE', #47124, #50928 ) ;
#51251 = CARTESIAN_POINT ( 'NONE',  ( 3.426173274723999906, -82.06136777077499289, -1.262550693616000030 ) ) ;
#51253 = DIRECTION ( 'NONE',  ( 0.000000000000000000, 0.000000000000000000, -1.000000000000000000 ) ) ;
#51254 = DIRECTION ( 'NONE',  ( 0.000000000000000000, -1.000000000000000000, -1.567610190497999989E-13 ) ) ;
#51255 = CARTESIAN_POINT ( 'NONE',  ( 6.263868601946986914, -80.27490189587713587, -8.736624837916803443 ) ) ;
#51256 = DIRECTION ( 'NONE',  ( 0.7071067811865475727, 0.000000000000000000, -0.7071067811865475727 ) ) ;
#51257 = DIRECTION ( 'NONE',  ( 0.000000000000000000, 1.000000000000000000, 0.000000000000000000 ) ) ;
#51258 = ORIENTED_EDGE ( 'NONE', *, *, #52320, .F. ) ;
#51259 = ORIENTED_EDGE ( 'NONE', *, *, #10230, .F. ) ;
#51260 = CARTESIAN_POINT ( 'NONE',  ( 3.714552462503000196, -79.48391337144799706, 11.44155784250999908 ) ) ;
#51261 = DIRECTION ( 'NONE',  ( 0.000000000000000000, 1.000000000000000000, 0.000000000000000000 ) ) ;
#51262 = EDGE_CURVE ( 'NONE', #37664, #33033, #32702, .T. ) ;
#51263 = CARTESIAN_POINT ( 'NONE',  ( 7.958763980604000032, -17.52301961031999866, 9.723170659100999202 ) ) ;
#51264 = ORIENTED_EDGE ( 'NONE', *, *, #53083, .F. ) ;
#51265 = CARTESIAN_POINT ( 'NONE',  ( -8.524893907337000698, -77.68509585594499356, -8.352346156331998728 ) ) ;
#51266 = ORIENTED_EDGE ( 'NONE', *, *, #36869, .T. ) ;
#51267 = EDGE_LOOP ( 'NONE', ( #19387, #56617, #20258, #22126 ) ) ;
#51268 = CARTESIAN_POINT ( 'NONE',  ( 0.000000000000000000, 0.000000000000000000, 0.000000000000000000 ) ) ;
#51269 = ORIENTED_EDGE ( 'NONE', *, *, #22853, .T. ) ;
#51270 = CIRCLE ( 'NONE', #35208, 9.000000000000000000 ) ;
#51271 = CARTESIAN_POINT ( 'NONE',  ( 3.537262634168000019, -79.45518468237709442, 0.2633306235646999949 ) ) ;
#51272 = CARTESIAN_POINT ( 'NONE',  ( 9.035652705983848065, -79.17456789375879112, 2.932964697886948802 ) ) ;
#51273 = EDGE_LOOP ( 'NONE', ( #23293, #34159, #4737, #21007 ) ) ;
#51274 = CARTESIAN_POINT ( 'NONE',  ( 0.2515381494466178980, -82.74157260121474167, -1.224160487734374358 ) ) ;
#51275 = VERTEX_POINT ( 'NONE', #5276 ) ;
#51276 = CARTESIAN_POINT ( 'NONE',  ( 11.00000000000000000, -77.34999999999999432, 0.000000000000000000 ) ) ;
#51277 = EDGE_LOOP ( 'NONE', ( #46557, #26306, #54915, #20405 ) ) ;
#51278 = CARTESIAN_POINT ( 'NONE',  ( -9.010298068253861814, -79.12116754975356514, -2.421818492791191879 ) ) ;
#51279 = CARTESIAN_POINT ( 'NONE',  ( -0.8773474274045136578, -78.82551938010156789, -1.226174542836929726 ) ) ;
#51280 = CARTESIAN_POINT ( 'NONE',  ( -0.5337471080167767168, -79.79999999999999716, -11.78542848578489455 ) ) ;
#51281 = DIRECTION ( 'NONE',  ( 0.000000000000000000, -1.000000000000000000, 0.000000000000000000 ) ) ;
#51282 = CARTESIAN_POINT ( 'NONE',  ( -1.004305231718999991, -1.000000000000000000, 3.090933677959000203 ) ) ;
#51283 = CARTESIAN_POINT ( 'NONE',  ( 3.248345031020999585, -78.09783857274324248, 9.144340540792999406 ) ) ;
#51284 = CARTESIAN_POINT ( 'NONE',  ( 10.02574878253000001, -76.55263728987598881, 4.955627619753999902 ) ) ;
#51285 = CARTESIAN_POINT ( 'NONE',  ( 2.510256491861835748, -79.99607450634006511, -9.173255752048776301 ) ) ;
#51286 = CARTESIAN_POINT ( 'NONE',  ( -7.705119999413000187, -58.55171076491000548, -10.24996238027999951 ) ) ;
#51287 = CARTESIAN_POINT ( 'NONE',  ( -7.969114183967002774, -78.64255665622569325, -4.697662469176757227 ) ) ;
#51288 = CARTESIAN_POINT ( 'NONE',  ( 8.453463329604378629, -76.51059011408864308, 8.160894682271043976 ) ) ;
#51289 = CARTESIAN_POINT ( 'NONE',  ( 4.816281158205000246, -77.73841001420198893, -8.085802691758997796 ) ) ;
#51290 = CARTESIAN_POINT ( 'NONE',  ( 0.5173218454072999739, -79.47763875002098644, 1.229208833401000067 ) ) ;
#51291 = DIRECTION ( 'NONE',  ( -1.000000000000000000, 0.000000000000000000, -2.582635147408000164E-11 ) ) ;
#51292 = CARTESIAN_POINT ( 'NONE',  ( -2.873112605672330400, -3.061334993885013400, 1.555068913299749278 ) ) ;
#51293 = CARTESIAN_POINT ( 'NONE',  ( 1.686223813997999921, -79.51992549782627862, 3.168656936234999666 ) ) ;
#51295 = EDGE_CURVE ( 'NONE', #34022, #29378, #17171, .T. ) ;
#51294 = CARTESIAN_POINT ( 'NONE',  ( -11.31676683693000030, -79.47839125786400416, 4.558499636902999974 ) ) ;
#51296 = CARTESIAN_POINT ( 'NONE',  ( -10.75000000000000000, -78.10000000000000853, 0.000000000000000000 ) ) ;
#51297 = CARTESIAN_POINT ( 'NONE',  ( 0.4743252877779617904, -82.94407894522871061, 1.156479017802467757 ) ) ;
#51298 = DIRECTION ( 'NONE',  ( 0.000000000000000000, -1.000000000000000000, 0.000000000000000000 ) ) ;
#51299 = CARTESIAN_POINT ( 'NONE',  ( -6.649705511044121664, -76.27700826535622980, -9.687362245905358549 ) ) ;
#51300 = CARTESIAN_POINT ( 'NONE',  ( -0.3125244749084483131, -82.00520833143282573, -1.470171615151792288 ) ) ;
#51301 = CARTESIAN_POINT ( 'NONE',  ( 0.3664097479246324340, -24.97190017500190606, 12.50575740043579387 ) ) ;
#51302 = LINE ( 'NONE', #37701, #5444 ) ;
#51303 = CARTESIAN_POINT ( 'NONE',  ( 0.8962411872155999770, -81.45069461833000446, 0.9875868993909000526 ) ) ;
#51304 = CARTESIAN_POINT ( 'NONE',  ( 3.938458446976999205, -79.30999999999998806, -8.369650235310999165 ) ) ;
#51305 = DIRECTION ( 'NONE',  ( -1.000000000000000000, 0.000000000000000000, 0.000000000000000000 ) ) ;
#51306 = PLANE ( 'NONE',  #27289 ) ;
#51307 = CARTESIAN_POINT ( 'NONE',  ( 3.132406251486010262, -77.80199808890452573, 10.30751908724726462 ) ) ;
#51308 = CARTESIAN_POINT ( 'NONE',  ( 9.723174505952000501, -24.47697504198000118, 7.958760297001999717 ) ) ;
#51309 = CARTESIAN_POINT ( 'NONE',  ( 0.2613587267741000475, -79.47689468395957135, -10.97249781033000282 ) ) ;
#51310 = CARTESIAN_POINT ( 'NONE',  ( 12.15240475282999988, -75.92640692754000042, 1.205235442679999824 ) ) ;
#51311 = VERTEX_POINT ( 'NONE', #36565 ) ;
#51312 = CARTESIAN_POINT ( 'NONE',  ( 2.081307824277000229, -85.99771544543098400, 3.372558905200000456 ) ) ;
#51313 = CARTESIAN_POINT ( 'NONE',  ( 7.941842383120999216, -80.39595877905549060, -8.023044940210999343 ) ) ;
#51314 = ADVANCED_FACE ( 'NONE', ( #13834 ), #39606, .F. ) ;
#51315 = CARTESIAN_POINT ( 'NONE',  ( 8.822708684726574546, -78.32582670471354902, -2.780085958306391269 ) ) ;
#51316 = CARTESIAN_POINT ( 'NONE',  ( 8.803761571624066917, -53.58431590314945225, 9.164326402650994297 ) ) ;
#51317 = CARTESIAN_POINT ( 'NONE',  ( -7.803863155890000236, -78.33791210329199828, 8.057160196619001624 ) ) ;
#51318 = DIRECTION ( 'NONE',  ( 0.000000000000000000, 1.000000000000000000, 0.000000000000000000 ) ) ;
#51319 = CARTESIAN_POINT ( 'NONE',  ( 9.617254819657999221, -78.63883383484099454, -0.5114877307952000463 ) ) ;
#51320 = CARTESIAN_POINT ( 'NONE',  ( -1.519662023741000123, -82.92241797422099125, -0.6825586799200999977 ) ) ;
#51321 = CARTESIAN_POINT ( 'NONE',  ( 2.872516177058867193, -80.22864583377563008, -10.68547302994066506 ) ) ;
#51322 = AXIS2_PLACEMENT_3D ( 'NONE', #17856, #57701, #31406 ) ;
#51323 = CARTESIAN_POINT ( 'NONE',  ( 0.3219823053856999961, -79.63291798508399211, -1.582258297802999980 ) ) ;
#51324 = ORIENTED_EDGE ( 'NONE', *, *, #45373, .T. ) ;
#51325 = CARTESIAN_POINT ( 'NONE',  ( -0.2201363562291999698, -79.36327907013999550, -1.483758735329000045 ) ) ;
#51326 = CARTESIAN_POINT ( 'NONE',  ( 0.2350766928662207378, -78.89591687295829558, -3.468875016500294173 ) ) ;
#51327 = ORIENTED_EDGE ( 'NONE', *, *, #10077, .T. ) ;
#51328 = CARTESIAN_POINT ( 'NONE',  ( -0.5996107393304999089, -78.54644797271500067, 1.191235959310000148 ) ) ;
#51329 = EDGE_CURVE ( 'NONE', #12818, #33527, #29370, .T. ) ;
#51330 = CARTESIAN_POINT ( 'NONE',  ( 7.305616453585000336, -79.99970782078999321, 8.949732329072000780 ) ) ;
#51331 = VERTEX_POINT ( 'NONE', #27986 ) ;
#51332 = CARTESIAN_POINT ( 'NONE',  ( -1.863462560416999869, -78.14610176985598855, 12.02123279331999939 ) ) ;
#51333 = CARTESIAN_POINT ( 'NONE',  ( 8.223067162435999222, -77.93193257914899164, 7.942492809189998226 ) ) ;
#51334 = CARTESIAN_POINT ( 'NONE',  ( 7.083968241731952276, -78.68188980497933471, -8.167169251009076092 ) ) ;
#51335 = ORIENTED_EDGE ( 'NONE', *, *, #35209, .T. ) ;
#51336 = EDGE_LOOP ( 'NONE', ( #48243, #1540, #22186, #742, #19965, #35164, #19581 ) ) ;
#51337 = CARTESIAN_POINT ( 'NONE',  ( 0.6909066256383181726, -80.42853791983925760, 1.041600136228693518 ) ) ;
#51338 = LINE ( 'NONE', #56052, #42708 ) ;
#51339 = CARTESIAN_POINT ( 'NONE',  ( -8.396223008680999911, -80.29268748536451028, -4.990405176070999538 ) ) ;
#51340 = EDGE_LOOP ( 'NONE', ( #19859, #47436, #49504, #34092 ) ) ;
#51341 = CARTESIAN_POINT ( 'NONE',  ( 12.68625206992999921, -55.03580249152999926, 1.886949102778999965 ) ) ;
#51342 = CARTESIAN_POINT ( 'NONE',  ( -1.596083865962000026, -78.46008588794200023, 10.79943897993000057 ) ) ;
#51343 = ORIENTED_EDGE ( 'NONE', *, *, #32267, .F. ) ;
#51344 = CARTESIAN_POINT ( 'NONE',  ( -12.72397319114999981, -23.22144180305999939, -1.930910316632999946 ) ) ;
#51345 = CARTESIAN_POINT ( 'NONE',  ( -8.383077572658999443, -77.47094415034599990, 4.458862939031999595 ) ) ;
#51346 = DIRECTION ( 'NONE',  ( 0.000000000000000000, 1.000000000000000000, 0.000000000000000000 ) ) ;
#51347 = CARTESIAN_POINT ( 'NONE',  ( 3.325196253812411573, -82.46277143088778416, -0.7067949879676419522 ) ) ;
#51348 = CARTESIAN_POINT ( 'NONE',  ( 12.25000000000000000, -80.79999999999999716, 0.000000000000000000 ) ) ;
#51349 = CARTESIAN_POINT ( 'NONE',  ( 9.378599967755729239, -78.27782913613843618, -2.572029467843342854 ) ) ;
#51350 = CIRCLE ( 'NONE', #16445, 1.750000000000002442 ) ;
#51351 = CARTESIAN_POINT ( 'NONE',  ( 6.969509891012999780, -76.97926403785729121, 6.817479844763999708 ) ) ;
#51352 = CARTESIAN_POINT ( 'NONE',  ( 0.8454482194665522421, -79.17736002063097089, 1.250557891722181347 ) ) ;
#51353 = B_SPLINE_CURVE_WITH_KNOTS ( 'NONE', 3,
 ( #14625, #32617, #50669, #37354 ),
 .UNSPECIFIED., .F., .F.,
 ( 4, 4 ),
 ( 0.000000000000000000, 0.1666666723472590150 ),
 .UNSPECIFIED. ) ;
#51354 = CARTESIAN_POINT ( 'NONE',  ( 0.9191423324976545350, -82.13020835052557800, -3.906387138476612009 ) ) ;
#51355 = CARTESIAN_POINT ( 'NONE',  ( -10.77133038182000035, -76.52288062955000214, -5.959359258312999508 ) ) ;
#51356 = CARTESIAN_POINT ( 'NONE',  ( 5.413904038987179312, -77.66666666666664298, -9.393203674808262349 ) ) ;
#51357 = EDGE_CURVE ( 'NONE', #10018, #13012, #35278, .T. ) ;
#51358 = CARTESIAN_POINT ( 'NONE',  ( 3.168171656089809662, -2.135114130757833184, 1.534604590466864593 ) ) ;
#51359 = CARTESIAN_POINT ( 'NONE',  ( 0.000000000000000000, -13.07071424677999971, 0.000000000000000000 ) ) ;
#51360 = CARTESIAN_POINT ( 'NONE',  ( 10.16243366810999937, -79.15072372342999074, -6.864696462387000153 ) ) ;
#51361 = CARTESIAN_POINT ( 'NONE',  ( 7.144724566336000393, -76.45948425134299953, 9.988770583665001368 ) ) ;
#51362 = FACE_OUTER_BOUND ( 'NONE', #8265, .T. ) ;
#51363 = EDGE_CURVE ( 'NONE', #12731, #43330, #18086, .T. ) ;
#51364 = CARTESIAN_POINT ( 'NONE',  ( 2.330792175847127723, -2.789315473941151424, -2.264371410303323007 ) ) ;
#51365 = CARTESIAN_POINT ( 'NONE',  ( -10.34990674316884629, -78.00757902561348089, 6.106564444846865669 ) ) ;
#51366 = CARTESIAN_POINT ( 'NONE',  ( 0.000000000000000000, -80.99999999999998579, 0.000000000000000000 ) ) ;
#51367 = ORIENTED_EDGE ( 'NONE', *, *, #43887, .T. ) ;
#51368 = DIRECTION ( 'NONE',  ( 0.000000000000000000, 0.000000000000000000, 1.000000000000000000 ) ) ;
#51369 = CARTESIAN_POINT ( 'NONE',  ( 9.139046933839001241, -77.16779404701080125, 2.935455237353000069 ) ) ;
#51370 = FACE_OUTER_BOUND ( 'NONE', #57414, .T. ) ;
#51371 = CARTESIAN_POINT ( 'NONE',  ( 0.000000000000000000, -80.79999999999999716, 0.000000000000000000 ) ) ;
#51372 = CARTESIAN_POINT ( 'NONE',  ( -3.846372246388999994, -2.785499118045999811, 0.4309855142524999794 ) ) ;
#51373 = CARTESIAN_POINT ( 'NONE',  ( 4.975516581814000361, -78.09966785968099146, -11.10075516933000017 ) ) ;
#51374 = CARTESIAN_POINT ( 'NONE',  ( -8.803456334546002182, -77.80598958818299593, -4.166395597179999299 ) ) ;
#51376 = DIRECTION ( 'NONE',  ( 1.000000000000000000, 0.000000000000000000, 0.000000000000000000 ) ) ;
#51375 = CARTESIAN_POINT ( 'NONE',  ( -10.43153131021861668, -76.16150389033835211, 5.412220054083467957 ) ) ;
#51377 = CARTESIAN_POINT ( 'NONE',  ( -7.105843098096999988, -79.45799394121699777, 8.287482117959999783 ) ) ;
#51378 = CARTESIAN_POINT ( 'NONE',  ( -10.46802440259882694, -79.58158398553671020, 2.476077618161485638 ) ) ;
#51379 = ORIENTED_EDGE ( 'NONE', *, *, #12772, .F. ) ;
#51380 = CARTESIAN_POINT ( 'NONE',  ( 0.6295237254636258939, -82.16666666666665719, -1.092232985442821658 ) ) ;
#51381 = FACE_OUTER_BOUND ( 'NONE', #31706, .T. ) ;
#51382 = ADVANCED_FACE ( 'NONE', ( #41003 ), #42623, .F. ) ;
#51383 = CARTESIAN_POINT ( 'NONE',  ( -3.165411199172029288, -2.479166666666666519, 0.8506806241676482250 ) ) ;
#51384 = CARTESIAN_POINT ( 'NONE',  ( -7.660431276897000430, -59.99179487629999841, 10.01749742442000191 ) ) ;
#51385 = VECTOR ( 'NONE', #23303, 1000.000000000000000 ) ;
#51386 = CYLINDRICAL_SURFACE ( 'NONE', #6277, 10.75000000000000000 ) ;
#51387 = CARTESIAN_POINT ( 'NONE',  ( -9.189896052897999823, -79.61787340482499076, 3.010092405580000019 ) ) ;
#51388 = CARTESIAN_POINT ( 'NONE',  ( 8.220399303327999618, -17.18050618273999675, -9.523318109998999859 ) ) ;
#51389 = DIRECTION ( 'NONE',  ( -1.000000000000000000, 0.000000000000000000, 0.000000000000000000 ) ) ;
#51390 = ORIENTED_EDGE ( 'NONE', *, *, #30318, .F. ) ;
#51391 = CARTESIAN_POINT ( 'NONE',  ( 6.793663275700000170, -79.45312102823399414, -8.982210410292001512 ) ) ;
#51392 = DIRECTION ( 'NONE',  ( 0.000000000000000000, 1.000000000000000000, 0.000000000000000000 ) ) ;
#51393 = CARTESIAN_POINT ( 'NONE',  ( -11.62703158103455436, -79.06212265249649818, -1.840488976840387592 ) ) ;
#51394 = CARTESIAN_POINT ( 'NONE',  ( 1.974456470848767298, -78.70000000000000284, 3.418760428718595090 ) ) ;
#51395 = CARTESIAN_POINT ( 'NONE',  ( 9.214665511417440058, -77.75938025394714259, 7.882923799935633191 ) ) ;
#51396 = B_SPLINE_CURVE_WITH_KNOTS ( 'NONE', 3,
 ( #11073, #29053, #24921, #2213, #38203, #28755, #24347, #42938, #2492, #42358, #20498, #1928, #19921, #56223, #41767, #19335, #28168, #37911 ),
 .UNSPECIFIED., .F., .F.,
 ( 4, 2, 2, 2, 2, 2, 2, 2, 4 ),
 ( 0.000000000000000000, 0.1250000000000000278, 0.2500000000000000555, 0.3750000000000000000, 0.5000000000000000000, 0.6250000000000000000, 0.7500000000000000000, 0.8750000000000001110, 1.000000000000000000 ),
 .UNSPECIFIED. ) ;
#51399 = CARTESIAN_POINT ( 'NONE',  ( -0.1211015312307294062, -81.48306870518814549, 1.244369522078131451 ) ) ;
#51398 = CIRCLE ( 'NONE', #15520, 14.00000000000000000 ) ;
#51397 = CARTESIAN_POINT ( 'NONE',  ( 1.290211209374999779, -81.42480055290900509, 0.2755370129015000114 ) ) ;
#51400 = EDGE_CURVE ( 'NONE', #20349, #36091, #43051, .T. ) ;
#51401 = CARTESIAN_POINT ( 'NONE',  ( 0.5516207887802486720, -78.81080817526184035, -1.149250216138818725 ) ) ;
#51402 = CARTESIAN_POINT ( 'NONE',  ( 0.000000000000000000, -0.1000000063292999924, 0.000000000000000000 ) ) ;
#51403 = CARTESIAN_POINT ( 'NONE',  ( 1.930989179114000143, -58.55453807205000061, -12.80896991324999945 ) ) ;
#51404 = EDGE_CURVE ( 'NONE', #44068, #56968, #24156, .T. ) ;
#51405 = FACE_OUTER_BOUND ( 'NONE', #32182, .T. ) ;
#51406 = DIRECTION ( 'NONE',  ( 0.000000000000000000, -1.000000000000000000, 0.000000000000000000 ) ) ;
#51407 = CARTESIAN_POINT ( 'NONE',  ( -1.250000000000000000, -80.49999999999998579, 0.000000000000000000 ) ) ;
#51408 = CARTESIAN_POINT ( 'NONE',  ( 12.70556836324529471, -53.57227722633783173, -0.2641978055039549966 ) ) ;
#51409 = ORIENTED_EDGE ( 'NONE', *, *, #7186, .F. ) ;
#51410 = ORIENTED_EDGE ( 'NONE', *, *, #41542, .T. ) ;
#51411 = CARTESIAN_POINT ( 'NONE',  ( 4.634228027295999475, -77.71608998579800698, 8.886345528036001085 ) ) ;
#51412 = CARTESIAN_POINT ( 'NONE',  ( 8.509671453119294071, -78.79784401220496193, -6.569625457439239646 ) ) ;
#51413 = ORIENTED_EDGE ( 'NONE', *, *, #57070, .F. ) ;
#51414 = FACE_OUTER_BOUND ( 'NONE', #30489, .T. ) ;
#51415 = EDGE_CURVE ( 'NONE', #35917, #14347, #6793, .T. ) ;
#51416 = CARTESIAN_POINT ( 'NONE',  ( -9.465687769217371539, -79.39306401481779574, 0.8068586129222159453 ) ) ;
#51417 = CARTESIAN_POINT ( 'NONE',  ( 10.72365324215999927, -78.45851024155000175, -5.189861527858999679 ) ) ;
#51418 = CARTESIAN_POINT ( 'NONE',  ( 10.75022122707607508, -79.83959204947723265, -1.407073340423293351 ) ) ;
#51419 = DIRECTION ( 'NONE',  ( -0.7071067811865474617, 0.000000000000000000, 0.7071067811865474617 ) ) ;
#51420 = CARTESIAN_POINT ( 'NONE',  ( 10.12290050124000018, -23.24999999991999644, 7.648026767085999822 ) ) ;
#51421 = CARTESIAN_POINT ( 'NONE',  ( 10.93160348586000019, -79.10187956322499758, 2.513594203403000105 ) ) ;
#51422 = CONICAL_SURFACE ( 'NONE', #54234, 4.199999999676998996, 0.7853981633972997312 ) ;
#51423 = ORIENTED_EDGE ( 'NONE', *, *, #28429, .F. ) ;
#51424 = CYLINDRICAL_SURFACE ( 'NONE', #57637, 3.250000000000000000 ) ;
#51425 = ORIENTED_EDGE ( 'NONE', *, *, #460, .T. ) ;
#51426 = CARTESIAN_POINT ( 'NONE',  ( 8.143624268315699410, -77.38946596373423858, 4.387306811431966658 ) ) ;
#51427 = DIRECTION ( 'NONE',  ( 0.000000000000000000, 0.000000000000000000, -1.000000000000000000 ) ) ;
#51428 = CARTESIAN_POINT ( 'NONE',  ( 9.144505818845814815, -77.55075625647234006, -6.496123635900521442 ) ) ;
#51429 = UNCERTAINTY_MEASURE_WITH_UNIT (LENGTH_MEASURE( 1.000000000000000082E-05 ), #40420, 'distance_accuracy_value', 'NONE');
#51430 = CARTESIAN_POINT ( 'NONE',  ( -1.585290096527000259, -78.00715048044240518, -0.3067070840873000193 ) ) ;
#51431 = AXIS2_PLACEMENT_3D ( 'NONE', #15350, #23906, #29487 ) ;
#51432 = CARTESIAN_POINT ( 'NONE',  ( -12.64701918103000011, -76.24633340635999446, -0.3107468859061999766 ) ) ;
#51433 = CARTESIAN_POINT ( 'NONE',  ( -0.9465222407332000154, -81.55663953507000485, -0.8164530897714000757 ) ) ;
#51434 = CARTESIAN_POINT ( 'NONE',  ( -0.1732310466989999687, -77.71390310378998834, 1.530487294790999986 ) ) ;
#51435 = ADVANCED_FACE ( 'NONE', ( #2319 ), #33586, .F. ) ;
#51436 = CARTESIAN_POINT ( 'NONE',  ( 7.366954953549999630, -79.67614197053399039, -8.234431878459000487 ) ) ;
#51437 = DIRECTION ( 'NONE',  ( 0.000000000000000000, -1.000000000000000000, 0.000000000000000000 ) ) ;
#51438 = DIRECTION ( 'NONE',  ( -0.7071067811865475727, 0.000000000000000000, -0.7071067811865475727 ) ) ;
#51439 = CARTESIAN_POINT ( 'NONE',  ( -7.648026766715999791, -55.54999999381000464, -10.12290050087000104 ) ) ;
#51440 = CARTESIAN_POINT ( 'NONE',  ( -3.377848665726999933, -86.11751568233700027, 0.3691513799601000012 ) ) ;
#51441 = ORIENTED_EDGE ( 'NONE', *, *, #9040, .T. ) ;
#51442 = CARTESIAN_POINT ( 'NONE',  ( -10.72633970217810173, -77.20000000000001705, 2.335726820744686183 ) ) ;
#51443 = CARTESIAN_POINT ( 'NONE',  ( -0.3234604031741999952, -79.72023290324000300, 1.671883997359000062 ) ) ;
#51444 = CARTESIAN_POINT ( 'NONE',  ( 9.576252206595992078, -77.88770107411112065, 4.884226988090900612 ) ) ;
#51445 = CARTESIAN_POINT ( 'NONE',  ( 11.36821324764999908, -77.85835662174498850, -3.778861202892000115 ) ) ;
#51446 = CARTESIAN_POINT ( 'NONE',  ( -9.243145380820950052, -53.88347263101093176, 8.441178781459031555 ) ) ;
#51447 = CARTESIAN_POINT ( 'NONE',  ( -1.254928322143489483, -78.73609231238140183, 0.2213947216297834919 ) ) ;
#51448 = CARTESIAN_POINT ( 'NONE',  ( -3.478185120108102879, -3.237645463075707220, 0.5448900037327830681 ) ) ;
#51449 = DIRECTION ( 'NONE',  ( -1.000000000000000000, 0.000000000000000000, 0.000000000000000000 ) ) ;
#51450 = CARTESIAN_POINT ( 'NONE',  ( -8.852983674280999082, -78.67307212613098955, -3.506430706099999739 ) ) ;
#51451 = CARTESIAN_POINT ( 'NONE',  ( 1.666698456705999920, -55.60818260126999490, -12.50018138918999888 ) ) ;
#51452 = CARTESIAN_POINT ( 'NONE',  ( 4.205198518925999274, -77.11498468449899235, -10.19892346455999999 ) ) ;
#51453 = CARTESIAN_POINT ( 'NONE',  ( -12.27595451888000078, -76.14772448534918681, 0.3505736730271999391 ) ) ;
#51454 = CARTESIAN_POINT ( 'NONE',  ( -1.570796326794885012, -78.41458333333332575, -12.00000000000000178 ) ) ;
#51455 = CARTESIAN_POINT ( 'NONE',  ( -0.5870063249280824680, -81.73668083619796221, -1.130609457767802972 ) ) ;
#51456 = ORIENTED_EDGE ( 'NONE', *, *, #50804, .F. ) ;
#51457 = CARTESIAN_POINT ( 'NONE',  ( 0.7341740840635999632, -80.93705256711200491, -1.113348630318000021 ) ) ;
#51458 = CARTESIAN_POINT ( 'NONE',  ( 1.667269374591999975, -60.00939883451999890, -12.49858097732999873 ) ) ;
#51459 = CARTESIAN_POINT ( 'NONE',  ( 5.940599228801999379E-14, -5.950000000028880187, -13.94999999997000018 ) ) ;
#51460 = CARTESIAN_POINT ( 'NONE',  ( 3.895497176768000003, -77.11288127666699665, 10.51870773133999926 ) ) ;
#51461 = CARTESIAN_POINT ( 'NONE',  ( 8.867070753125000593, -78.50939305077599784, -6.468312982590000537 ) ) ;
#51462 = CARTESIAN_POINT ( 'NONE',  ( -1.814565153809999759E-14, -79.00000000000000000, 0.000000000000000000 ) ) ;
#51463 = CARTESIAN_POINT ( 'NONE',  ( -0.9577436045183314040, -83.51770832516572796, -3.937309471672632455 ) ) ;
#51464 = CARTESIAN_POINT ( 'NONE',  ( -2.552548608664000351, -76.46843057132498700, 11.88149999858000072 ) ) ;
#51465 = CARTESIAN_POINT ( 'NONE',  ( 7.295133564347398014, -78.51976047057470964, 9.212451541599802951 ) ) ;
#51466 = CARTESIAN_POINT ( 'NONE',  ( -1.250000000000000000, -77.10000000000000853, 0.5000000000000000000 ) ) ;
#51467 = ORIENTED_EDGE ( 'NONE', *, *, #1809, .T. ) ;
#51468 = CARTESIAN_POINT ( 'NONE',  ( -0.07152028281723200875, -79.97993409046794966, 1.247844452081509292 ) ) ;
#51469 = CARTESIAN_POINT ( 'NONE',  ( -0.9218200799623716968, -79.57291666666667140, -1.199500263597270910 ) ) ;
#51470 = CARTESIAN_POINT ( 'NONE',  ( 7.631889106307999882, -55.57878585374000124, -10.36222439673000117 ) ) ;
#51471 = CIRCLE ( 'NONE', #35392, 5.000000000000000888 ) ;
#51472 = CARTESIAN_POINT ( 'NONE',  ( -8.859962374443000499, -78.12620263911298935, 6.959166695099000322 ) ) ;
#51473 = CARTESIAN_POINT ( 'NONE',  ( 1.431169160529000006, -78.21216375143998789, 0.09917081181617999619 ) ) ;
#51474 = LINE ( 'NONE', #11031, #14117 ) ;
#51475 = CARTESIAN_POINT ( 'NONE',  ( -1.454013506048745130, -81.77223631312656948, -0.4159240082623796297 ) ) ;
#51476 = CARTESIAN_POINT ( 'NONE',  ( -0.2580402550692753594, -83.23804571606062552, 1.489083542988291153 ) ) ;
#51477 = CARTESIAN_POINT ( 'NONE',  ( 0.4990820023277747763, -79.75804326553362955, -1.145820899119790681 ) ) ;
#51478 = CIRCLE ( 'NONE', #32595, 10.14999999999999858 ) ;
#51479 = CARTESIAN_POINT ( 'NONE',  ( -10.21026245498356033, -54.54392421755085962, 7.764236519575772100 ) ) ;
#51480 = VERTEX_POINT ( 'NONE', #29439 ) ;
#51481 = CARTESIAN_POINT ( 'NONE',  ( -1.144794046686379296, -81.63306042909437110, -0.5017307455195174626 ) ) ;
#51482 = FILL_AREA_STYLE_COLOUR ( '', #12406 ) ;
#51483 = CARTESIAN_POINT ( 'NONE',  ( 5.828547835401000299, -78.55992220834100692, -9.501726143737998953 ) ) ;
#51484 = CARTESIAN_POINT ( 'NONE',  ( -1.135826688880000157, -81.40663953506998496, -0.9797437077257000748 ) ) ;
#51485 = EDGE_LOOP ( 'NONE', ( #27609, #21748, #38723 ) ) ;
#51486 = VERTEX_POINT ( 'NONE', #6733 ) ;
#51487 = CARTESIAN_POINT ( 'NONE',  ( 0.09183084214940000212, -80.97252787813199859, 1.414788531112000092 ) ) ;
#51488 = ORIENTED_EDGE ( 'NONE', *, *, #33072, .F. ) ;
#51489 = CARTESIAN_POINT ( 'NONE',  ( 9.401479492988663367, -79.98662458792078667, -1.597696805283046917 ) ) ;
#51490 = ORIENTED_EDGE ( 'NONE', *, *, #40054, .F. ) ;
#51491 = CARTESIAN_POINT ( 'NONE',  ( 2.062323307449999810, -18.77286846807999865, 12.83634826442999888 ) ) ;
#51492 = CARTESIAN_POINT ( 'NONE',  ( -11.11771682179999843, -80.33756661863206716, 1.751409206030000165 ) ) ;
#51493 = PRODUCT_CONTEXT ( 'NONE', #55283, 'mechanical' ) ;
#51494 = EDGE_CURVE ( 'NONE', #20252, #29379, #16193, .T. ) ;
#51495 = B_SPLINE_CURVE_WITH_KNOTS ( 'NONE', 3,
 ( #28369, #10385, #36655, #36365, #37524, #27497, #55542, #51132, #5945, #18952, #13928, #45833, #49968, #10686, #394, #15093, #23660, #41965, #37235, #33089, #54391, #32212, #10098, #45538 ),
 .UNSPECIFIED., .F., .F.,
 ( 4, 2, 2, 2, 2, 2, 2, 2, 2, 2, 2, 4 ),
 ( 0.000000000000000000, 0.1250000000000006661, 0.2500000000000013323, 0.3750000000000019984, 0.4375000000000026645, 0.5000000000000033307, 0.6250000000000039968, 0.7500000000000046629, 0.8125000000000049960, 0.8437500000000042188, 0.8750000000000035527, 1.000000000000000000 ),
 .UNSPECIFIED. ) ;
#51496 = CARTESIAN_POINT ( 'NONE',  ( -12.51072239526000196, -63.10294702885996543, 0.7871079366006996647 ) ) ;
#51497 = CARTESIAN_POINT ( 'NONE',  ( 5.143522193159038025, -78.27208594951937926, -7.687965448588824913 ) ) ;
#51498 = CARTESIAN_POINT ( 'NONE',  ( -10.39759693597000023, -79.72892006072399340, -4.208097972746998927 ) ) ;
#51499 = EDGE_LOOP ( 'NONE', ( #53730, #25599, #52653, #28254 ) ) ;
#51500 = ORIENTED_EDGE ( 'NONE', *, *, #45812, .F. ) ;
#51501 = CARTESIAN_POINT ( 'NONE',  ( -8.840280758047018850, -77.57624239855847748, 2.722759996602876598 ) ) ;
#51502 = CARTESIAN_POINT ( 'NONE',  ( 11.00000000000000000, -77.84999999999999432, 0.000000000000000000 ) ) ;
#51503 = CARTESIAN_POINT ( 'NONE',  ( 10.81758370282001103, -76.04999999999998295, -2.303648478522546394 ) ) ;
#51504 = CARTESIAN_POINT ( 'NONE',  ( -0.1538805260928999830, -78.14611046371997816, 9.702939253146000809 ) ) ;
#51505 = DIRECTION ( 'NONE',  ( -1.000000000000000000, 0.000000000000000000, 0.000000000000000000 ) ) ;
#51506 = CARTESIAN_POINT ( 'NONE',  ( -10.21381326473999884, -19.22870851082999977, 7.668949790020999302 ) ) ;
#51507 = CARTESIAN_POINT ( 'NONE',  ( 11.59177481778000107, -78.97584316692000073, -2.749920651092999879 ) ) ;
#51508 = EDGE_CURVE ( 'NONE', #46033, #26247, #10295, .T. ) ;
#51509 = CARTESIAN_POINT ( 'NONE',  ( -1.563706488702000019, -81.30232256240998368, -0.6734635195847999967 ) ) ;
#51510 = CARTESIAN_POINT ( 'NONE',  ( 1.250000000000000000, -80.25000000000000000, 0.000000000000000000 ) ) ;
#51511 = CARTESIAN_POINT ( 'NONE',  ( -1.387074871800343834, -79.71753748822699492, 0.5993129225438764696 ) ) ;
#51512 = CARTESIAN_POINT ( 'NONE',  ( -7.750101915720000179, -78.38956332859899589, 6.177086609340000756 ) ) ;
#51513 = CARTESIAN_POINT ( 'NONE',  ( -5.427146848547155678, -80.40833333333752364, -9.396180599229785102 ) ) ;
#51514 = CARTESIAN_POINT ( 'NONE',  ( 1.799490225533999732, -22.77152778045000048, -12.64500484462999985 ) ) ;
#51515 = AXIS2_PLACEMENT_3D ( 'NONE', #16301, #2150, #11584 ) ;
#51517 = CARTESIAN_POINT ( 'NONE',  ( -1.112801787005999854, -79.30619658827799867, -0.6258220204580999813 ) ) ;
#51516 = CARTESIAN_POINT ( 'NONE',  ( 1.499999999999999778, -78.66041666666669130, 0.1963495408493654004 ) ) ;
#51518 = CARTESIAN_POINT ( 'NONE',  ( 0.000000000000000000, -4.000000000000000000, 0.000000000000000000 ) ) ;
#51519 = FACE_OUTER_BOUND ( 'NONE', #2315, .T. ) ;
#51520 = DIRECTION ( 'NONE',  ( -0.7071067811865475727, 0.000000000000000000, -0.7071067811865475727 ) ) ;
#51521 = EDGE_CURVE ( 'NONE', #34745, #28917, #49386, .T. ) ;
#51522 = FACE_OUTER_BOUND ( 'NONE', #44959, .T. ) ;
#51523 = CARTESIAN_POINT ( 'NONE',  ( -1.875163999714702712, -1.330382934593637323, -2.984421498244137716 ) ) ;
#51524 = VECTOR ( 'NONE', #8562, 1000.000000000000000 ) ;
#51525 = ORIENTED_EDGE ( 'NONE', *, *, #45471, .F. ) ;
#51526 = CARTESIAN_POINT ( 'NONE',  ( 4.801183948431940074, -78.95833333333332860, -10.79468190471654410 ) ) ;
#51527 = ADVANCED_FACE ( 'NONE', ( #15884 ), #53735, .F. ) ;
#51528 = CARTESIAN_POINT ( 'NONE',  ( -1.798336774613000122, -55.60355501915000076, 12.61277771564000005 ) ) ;
#51529 = CARTESIAN_POINT ( 'NONE',  ( 1.185568982899148693, -78.37591526493211802, 0.3956926376703175929 ) ) ;
#51530 = AXIS2_PLACEMENT_3D ( 'NONE', #52442, #17283, #43297 ) ;
#51531 = CARTESIAN_POINT ( 'NONE',  ( 1.659133085963000021, -80.03182264566298443, -9.498693983952000153 ) ) ;
#51532 = CARTESIAN_POINT ( 'NONE',  ( -12.66316398243999863, -53.62133896622000151, -0.04044089952534000304 ) ) ;
#51533 = DIRECTION ( 'NONE',  ( 6.735284179502000863E-11, -1.000000000000000000, 0.000000000000000000 ) ) ;
#51534 = CARTESIAN_POINT ( 'NONE',  ( 3.514783469115777770, -79.44852014850161481, 10.18303985929887823 ) ) ;
#51535 = CARTESIAN_POINT ( 'NONE',  ( -9.738811118029000014, -79.44331332859900385, -0.02447652147661999802 ) ) ;
#51536 = DIRECTION ( 'NONE',  ( 0.000000000000000000, -1.000000000000000000, 0.000000000000000000 ) ) ;
#51537 = CARTESIAN_POINT ( 'NONE',  ( 10.81029799801000024, -78.05327334234998204, -0.4981644331059998931 ) ) ;
#51538 = CARTESIAN_POINT ( 'NONE',  ( -1.306825378516000002, -81.39410433555399038, -0.7490716765632000618 ) ) ;
#51539 = CARTESIAN_POINT ( 'NONE',  ( -0.8481231068849000021, -79.03194514476065535, 9.686304223355000076 ) ) ;
#51540 = CARTESIAN_POINT ( 'NONE',  ( -0.1492691421716000055, -78.39707553773099846, 9.412168359664999429 ) ) ;
#51542 = CARTESIAN_POINT ( 'NONE',  ( -0.4254240051736286610, -2.885416666666666519, 3.249999999999997780 ) ) ;
#51541 = CARTESIAN_POINT ( 'NONE',  ( -3.181650608227999832, -82.74278679062099684, 2.362856221671000068 ) ) ;
#51543 = CARTESIAN_POINT ( 'NONE',  ( 7.507056363060000237, -79.88925584965399196, -5.572808305725000189 ) ) ;
#51544 = FACE_OUTER_BOUND ( 'NONE', #6452, .T. ) ;
#51545 = CARTESIAN_POINT ( 'NONE',  ( 7.605146568930318374, -80.28753541715676079, -7.597634579134508570 ) ) ;
#51546 = ADVANCED_FACE ( 'NONE', ( #3457 ), #47359, .F. ) ;
#51547 = FACE_OUTER_BOUND ( 'NONE', #30999, .T. ) ;
#51548 = CARTESIAN_POINT ( 'NONE',  ( -9.500000000000000000, -77.38958333333332007, 1.243547092045920399 ) ) ;
#51549 = ORIENTED_EDGE ( 'NONE', *, *, #47673, .T. ) ;
#51550 = CARTESIAN_POINT ( 'NONE',  ( 10.43959491470999978, -79.77472838834199820, -5.976816984917999953 ) ) ;
#51551 = CARTESIAN_POINT ( 'NONE',  ( 0.000000000000000000, -77.50000000000000000, -3.799999999999999822 ) ) ;
#51552 = CARTESIAN_POINT ( 'NONE',  ( -0.5999999999999999778, -5.200000000000000178, 4.000000000000000000 ) ) ;
#51553 = ORIENTED_EDGE ( 'NONE', *, *, #19022, .F. ) ;
#51554 = CARTESIAN_POINT ( 'NONE',  ( -7.587128856971000701, -78.55323394950600857, 9.212544607993001122 ) ) ;
#51555 = VERTEX_POINT ( 'NONE', #39470 ) ;
#51556 = VECTOR ( 'NONE', #28923, 1000.000000000000000 ) ;
#51557 = ORIENTED_EDGE ( 'NONE', *, *, #9161, .T. ) ;
#51558 = CARTESIAN_POINT ( 'NONE',  ( 6.606377239730313988, -78.82291666666665719, 8.596418555780454440 ) ) ;
#51559 = CARTESIAN_POINT ( 'NONE',  ( -11.44417895085270942, -77.32083333333335418, -3.075537641221545826 ) ) ;
#51560 = AXIS2_PLACEMENT_3D ( 'NONE', #43078, #24773, #20632 ) ;
#51561 = CARTESIAN_POINT ( 'NONE',  ( -3.238485901480999907, -78.60716621652929348, 1.037469946420999989 ) ) ;
#51562 = CARTESIAN_POINT ( 'NONE',  ( 4.313834340563736269, -79.23712179264661870, 8.463837022421156320 ) ) ;
#51563 = ORIENTED_EDGE ( 'NONE', *, *, #12281, .F. ) ;
#51564 = CARTESIAN_POINT ( 'NONE',  ( 0.2560571373808674389, -82.74185738613888930, -1.223228159499044398 ) ) ;
#51565 = ORIENTED_EDGE ( 'NONE', *, *, #45634, .F. ) ;
#51566 = CARTESIAN_POINT ( 'NONE',  ( -7.612971414697999428, -55.47547470607999998, 10.53003223722000037 ) ) ;
#51567 = ORIENTED_EDGE ( 'NONE', *, *, #45353, .T. ) ;
#51568 = DIRECTION ( 'NONE',  ( 0.000000000000000000, 1.000000000000000000, 0.000000000000000000 ) ) ;
#51569 = CARTESIAN_POINT ( 'NONE',  ( 0.2655774789948861514, -78.38858963195251306, -1.510445311185437456 ) ) ;
#51570 = CIRCLE ( 'NONE', #32691, 0.8000000000000000444 ) ;
#51571 = CARTESIAN_POINT ( 'NONE',  ( 11.76049068545964005, -79.80000000000002558, 0.9294003827681622809 ) ) ;
#51572 = DIRECTION ( 'NONE',  ( -1.000000000000000000, 0.000000000000000000, 0.000000000000000000 ) ) ;
#51573 = CARTESIAN_POINT ( 'NONE',  ( 12.21492819193520774, -78.69308421639392748, -1.097028228127378435 ) ) ;
#51574 = CARTESIAN_POINT ( 'NONE',  ( -8.592320330817999618, -78.21153388925924332, 4.510292750937000328 ) ) ;
#51575 = CARTESIAN_POINT ( 'NONE',  ( 9.776276929627000456, -75.97575262412699715, -5.431214116490000521 ) ) ;
#51576 = CARTESIAN_POINT ( 'NONE',  ( 9.400053674151607197, -79.57946385258328803, -2.458488295831327441 ) ) ;
#51577 = EDGE_CURVE ( 'NONE', #42525, #15494, #30321, .T. ) ;
#51578 = CARTESIAN_POINT ( 'NONE',  ( 10.99999999999999822, -78.46041666666668846, 1.439896632895345086 ) ) ;
#51579 = DIRECTION ( 'NONE',  ( 0.000000000000000000, 1.000000000000000000, 0.000000000000000000 ) ) ;
#51580 = CARTESIAN_POINT ( 'NONE',  ( 4.873378631631000601, -76.55225832436200051, -9.988483505024001730 ) ) ;
#51581 = CARTESIAN_POINT ( 'NONE',  ( -7.279424256080870848, -78.65297865939129451, -5.707278038144436572 ) ) ;
#51582 = CARTESIAN_POINT ( 'NONE',  ( 2.331141250342373183, -76.55869204935913785, 11.51617495810127600 ) ) ;
#51583 = B_SPLINE_CURVE_WITH_KNOTS ( 'NONE', 3,
 ( #19497, #6497, #19796, #18635, #15061, #18919, #5619, #41064, #37492, #54646 ),
 .UNSPECIFIED., .F., .F.,
 ( 4, 2, 2, 2, 4 ),
 ( 0.000000000000000000, 0.2500000000000000000, 0.5000000000000000000, 0.7500000000000000000, 1.000000000000000000 ),
 .UNSPECIFIED. ) ;
#51584 = CARTESIAN_POINT ( 'NONE',  ( -5.645349303483418346, -80.18225419666993048, -9.440761718514824707 ) ) ;
#51585 = CARTESIAN_POINT ( 'NONE',  ( 7.596835002782697188, -77.10208333333333997, 5.838193839761710358 ) ) ;
#51586 = CARTESIAN_POINT ( 'NONE',  ( 1.394409823850000008, -80.48192549782599770, -3.307470144239999854 ) ) ;
#51587 = CARTESIAN_POINT ( 'NONE',  ( -1.777040666284000148, -79.89549482803428759, 12.07019270111999987 ) ) ;
#51588 = CARTESIAN_POINT ( 'NONE',  ( -9.932012650257558306, -78.06882224905531587, 4.112984229135753012 ) ) ;
#51589 = CARTESIAN_POINT ( 'NONE',  ( 1.022162451771789549, -82.89907212072580478, 0.7192351975817576903 ) ) ;
#51590 = FACE_OUTER_BOUND ( 'NONE', #5931, .T. ) ;
#51591 = DIRECTION ( 'NONE',  ( 0.000000000000000000, 1.000000000000000000, 0.000000000000000000 ) ) ;
#51592 = CARTESIAN_POINT ( 'NONE',  ( 10.01332852689000141, -23.28056535155999995, 7.654537165468999760 ) ) ;
#51593 = CARTESIAN_POINT ( 'NONE',  ( -0.6454797251259661861, -24.88806512139862903, 12.50471521368227990 ) ) ;
#51594 = EDGE_CURVE ( 'NONE', #43980, #26528, #13342, .T. ) ;
#51595 = CARTESIAN_POINT ( 'NONE',  ( 0.9218200799623742503, -77.67708333333335702, -1.199500263597268912 ) ) ;
#51596 = CARTESIAN_POINT ( 'NONE',  ( -0.1834469635243000107, -79.21327907014000402, -1.236465612773999911 ) ) ;
#51597 = FACE_BOUND ( 'NONE', #29094, .T. ) ;
#51598 = AXIS2_PLACEMENT_3D ( 'NONE', #10547, #23816, #24113 ) ;
#51599 = CARTESIAN_POINT ( 'NONE',  ( 4.421533069776005576, -77.79180160825917767, 9.823367980291944690 ) ) ;
#51600 = FACE_OUTER_BOUND ( 'NONE', #11912, .T. ) ;
#51601 = CARTESIAN_POINT ( 'NONE',  ( -8.758795259761319230, -79.80031661833969281, 6.307149791603988476 ) ) ;
#51602 = CARTESIAN_POINT ( 'NONE',  ( 1.379264194910999830, -76.12150170015999606, 11.98273499079000004 ) ) ;
#51603 = VERTEX_POINT ( 'NONE', #35905 ) ;
#51604 = AXIS2_PLACEMENT_3D ( 'NONE', #20993, #22665, #4059 ) ;
#51605 = CARTESIAN_POINT ( 'NONE',  ( -3.027477083952000214, -85.15596544543099355, -2.223903009527000041 ) ) ;
#51606 = CARTESIAN_POINT ( 'NONE',  ( 0.3809989338272000703, -80.14893166943579672, 11.39926455542999939 ) ) ;
#51607 = AXIS2_PLACEMENT_3D ( 'NONE', #49088, #22212, #26343 ) ;
#51608 = CARTESIAN_POINT ( 'NONE',  ( 9.184444922356584939, -78.34058259241612632, -1.099429577161610938 ) ) ;
#51609 = DIRECTION ( 'NONE',  ( -0.7071067811865474617, 0.000000000000000000, -0.7071067811865474617 ) ) ;
#51610 = CARTESIAN_POINT ( 'NONE',  ( -11.14038684213999986, -78.39238478929600262, 1.307628137226999998 ) ) ;
#51611 = CARTESIAN_POINT ( 'NONE',  ( 12.54673671095000209, -53.97796527404000244, -0.9173654211234000266 ) ) ;
#51612 = CARTESIAN_POINT ( 'NONE',  ( -6.791097082272000485, -77.89278619496199951, -6.981453725808999700 ) ) ;
#51613 = AXIS2_PLACEMENT_3D ( 'NONE', #35826, #45295, #49127 ) ;
#51614 = CARTESIAN_POINT ( 'NONE',  ( 1.431241028886999889, -81.59607445691000294, -0.8524881072380000591 ) ) ;
#51615 = LINE ( 'NONE', #56323, #18043 ) ;
#51616 = CARTESIAN_POINT ( 'NONE',  ( -1.583750823903000038, -80.47633258256199440, 0.3147260902806000016 ) ) ;
#51617 = ADVANCED_FACE ( 'NONE', ( #23212 ), #12431, .F. ) ;
#51618 = ORIENTED_EDGE ( 'NONE', *, *, #1428, .T. ) ;
#51619 = CARTESIAN_POINT ( 'NONE',  ( -7.919595949288999570, -57.79999999967000690, 8.909545442949999838 ) ) ;
#51620 = CARTESIAN_POINT ( 'NONE',  ( -3.336363063059238687, -78.72637457323575916, -0.7471181105293197566 ) ) ;
#51621 = ORIENTED_EDGE ( 'NONE', *, *, #10642, .T. ) ;
#51622 = CARTESIAN_POINT ( 'NONE',  ( -0.6568659331174000471, -78.09409575648280111, 1.160647793301999853 ) ) ;
#51623 = CARTESIAN_POINT ( 'NONE',  ( 10.62704985177000161, -78.53487766400598957, -3.023855997759000047 ) ) ;
#51624 = CARTESIAN_POINT ( 'NONE',  ( 12.71658872087999903, -60.11584731951999316, 1.931087888240000217 ) ) ;
#51625 = CARTESIAN_POINT ( 'NONE',  ( -1.250000000000000000, -80.59999999999999432, 0.000000000000000000 ) ) ;
#51626 = ORIENTED_EDGE ( 'NONE', *, *, #3432, .F. ) ;
#51627 = CARTESIAN_POINT ( 'NONE',  ( -12.04425331849999914, -78.77007602460300006, -1.708359618215999909 ) ) ;
#51628 = CARTESIAN_POINT ( 'NONE',  ( -11.04512294322999999, -77.57457916904299111, -2.489477414621999785 ) ) ;
#51629 = CARTESIAN_POINT ( 'NONE',  ( -0.7035581186724901848, -77.48024153129969704, 10.74957510668601834 ) ) ;
#51631 = EDGE_LOOP ( 'NONE', ( #41094, #31985, #58101 ) ) ;
#51630 = B_SPLINE_CURVE_WITH_KNOTS ( 'NONE', 3,
 ( #49545, #45711, #18250, #14097, #27078, #10260 ),
 .UNSPECIFIED., .F., .F.,
 ( 4, 2, 4 ),
 ( 0.000000000000000000, 0.5000000000000000000, 1.000000000000000000 ),
 .UNSPECIFIED. ) ;
#51632 = ORIENTED_EDGE ( 'NONE', *, *, #17478, .T. ) ;
#51633 = CARTESIAN_POINT ( 'NONE',  ( 0.6030484120316327301, -80.43496411464462881, 1.095119744681182228 ) ) ;
#51634 = CARTESIAN_POINT ( 'NONE',  ( -5.314024065878000691, -77.20733998579800073, -7.926018785099000041 ) ) ;
#51635 = CARTESIAN_POINT ( 'NONE',  ( -5.809791519574999619, -79.43600129156250489, 7.851562197947999699 ) ) ;
#51636 = ORIENTED_EDGE ( 'NONE', *, *, #11984, .T. ) ;
#51637 = CARTESIAN_POINT ( 'NONE',  ( -12.71162862749995526, -24.23964265629794568, -1.720599174824705813 ) ) ;
#51638 = CARTESIAN_POINT ( 'NONE',  ( -0.4035379437255999791, -79.19546714899098561, -10.90928609572000063 ) ) ;
#51639 = ORIENTED_EDGE ( 'NONE', *, *, #267, .F. ) ;
#51640 = CARTESIAN_POINT ( 'NONE',  ( -12.44210192979000063, -24.08432059816999882, -1.464837683472000052 ) ) ;
#51641 = CARTESIAN_POINT ( 'NONE',  ( 9.475051992780000987, -77.75466915034600390, -0.6170397550469999270 ) ) ;
#51642 = CIRCLE ( 'NONE', #53506, 1.000000000000000000 ) ;
#51643 = CARTESIAN_POINT ( 'NONE',  ( 12.80090744921000123, -59.56232687415000271, -1.980532734072999901 ) ) ;
#51644 = CARTESIAN_POINT ( 'NONE',  ( 9.546815223802999739, -54.11472046612000497, 8.130854305859999798 ) ) ;
#51645 = CARTESIAN_POINT ( 'NONE',  ( 0.000000000000000000, -0.1000000063292999924, -3.699999993671000187 ) ) ;
#51646 = CARTESIAN_POINT ( 'NONE',  ( -12.50000000000000000, -60.04999999657000131, -1.750000000000000000 ) ) ;
#51647 = ADVANCED_FACE ( 'NONE', ( #45963 ), #18500, .T. ) ;
#51648 = B_SPLINE_CURVE_WITH_KNOTS ( 'NONE', 3,
 ( #12154, #56745, #52033, #16305, #11588, #34282, #29851, #47904, #7436, #25437, #52602, #30140, #8881, #18037, #31000, #21866, #26876, #44902 ),
 .UNSPECIFIED., .F., .F.,
 ( 4, 2, 2, 2, 2, 2, 2, 2, 4 ),
 ( 0.000000000000000000, 0.1250000000000000555, 0.2500000000000001110, 0.3750000000000001665, 0.5000000000000001110, 0.6250000000000001110, 0.7500000000000002220, 0.8750000000000001110, 1.000000000000000000 ),
 .UNSPECIFIED. ) ;
#51649 = CARTESIAN_POINT ( 'NONE',  ( 7.070456480284000200, -76.81002177417249754, -6.005572703287999303 ) ) ;
#51650 = AXIS2_PLACEMENT_3D ( 'NONE', #46330, #10593, #37149 ) ;
#51651 = CARTESIAN_POINT ( 'NONE',  ( -0.1181554223150161204, -79.23090075405382038, 1.505089927673818773 ) ) ;
#51652 = CARTESIAN_POINT ( 'NONE',  ( -5.539808784079886195, -79.68333333333332291, -9.611650271896841957 ) ) ;
#51653 = EDGE_CURVE ( 'NONE', #15394, #1613, #236, .T. ) ;
#51654 = CARTESIAN_POINT ( 'NONE',  ( 10.54796701376999835, -75.74110257978999527, 6.346365727669000201 ) ) ;
#51655 = CARTESIAN_POINT ( 'NONE',  ( 10.75000000000000355, -77.73958333333331439, -1.407171709420407035 ) ) ;
#51656 = CARTESIAN_POINT ( 'NONE',  ( -9.500000000000000000, -77.89999999999999147, 0.000000000000000000 ) ) ;
#51657 = CARTESIAN_POINT ( 'NONE',  ( 9.038948602550000544, -62.13262223832000331, -9.029786144045999663 ) ) ;
#51658 = CIRCLE ( 'NONE', #22376, 1.250000000000000000 ) ;
#51659 = CARTESIAN_POINT ( 'NONE',  ( -3.417863094299999904, -78.34598361729999283, 11.50296535110000029 ) ) ;
#51660 = CARTESIAN_POINT ( 'NONE',  ( 8.135116633385999663, -76.88348855772599677, 9.200136113044999675 ) ) ;
#51661 = CARTESIAN_POINT ( 'NONE',  ( 5.838193839761669501, -78.72291666666666288, 7.596835002782726498 ) ) ;
#51662 = CARTESIAN_POINT ( 'NONE',  ( -5.205522333151648695, -77.46053809305541904, 10.88972242663192880 ) ) ;
#51663 = CARTESIAN_POINT ( 'NONE',  ( -4.152600241220000044, -79.34482178677752984, -10.41988588363999924 ) ) ;
#51664 = ADVANCED_FACE ( 'NONE', ( #32053 ), #45670, .F. ) ;
#51665 = ORIENTED_EDGE ( 'NONE', *, *, #18523, .T. ) ;
#51666 = CARTESIAN_POINT ( 'NONE',  ( -0.7953408400917133525, -80.83092108792313013, -1.285395336168587033 ) ) ;
#51667 = CARTESIAN_POINT ( 'NONE',  ( 2.317704416658000088, -76.97337147138669877, -9.426556171238999582 ) ) ;
#51668 = FACE_OUTER_BOUND ( 'NONE', #44189, .T. ) ;
#51669 = FACE_OUTER_BOUND ( 'NONE', #17485, .T. ) ;
#51670 = CARTESIAN_POINT ( 'NONE',  ( 3.628014619811000152, -2.572693282128000192, 1.348272186933000105 ) ) ;
#51671 = CARTESIAN_POINT ( 'NONE',  ( 11.88272347344000046, -77.27212751510998601, 1.999161996513999950 ) ) ;
#51672 = CARTESIAN_POINT ( 'NONE',  ( -7.484045594489000308, -78.71555212030999371, 6.232877124219999843 ) ) ;
#51674 = CARTESIAN_POINT ( 'NONE',  ( 5.790379962074457154, -77.02682291667791503, 7.536004869419408614 ) ) ;
#51673 = CARTESIAN_POINT ( 'NONE',  ( -9.763989801682905423, -76.15250257597224959, 6.535952189803941437 ) ) ;
#51675 = CARTESIAN_POINT ( 'NONE',  ( -1.433413778493000112, -78.64090365116300063, -10.60928646434000200 ) ) ;
#51676 = CARTESIAN_POINT ( 'NONE',  ( -10.54819193961059121, -79.58468236046442712, 2.072783446717219924 ) ) ;
#51677 = EDGE_LOOP ( 'NONE', ( #55467, #47069, #10936, #48865 ) ) ;
#51678 = CARTESIAN_POINT ( 'NONE',  ( -0.9870767835202882701, -80.96949413944575724, -1.171048524979026118 ) ) ;
#51679 = CARTESIAN_POINT ( 'NONE',  ( -2.421407277241032219, -77.99599274655952286, 9.009652519855267272 ) ) ;
#51680 = CARTESIAN_POINT ( 'NONE',  ( -3.250000000000001776, -2.489583333333333037, 0.4254240051736045136 ) ) ;
#51681 = CARTESIAN_POINT ( 'NONE',  ( -7.659225027833000077, -60.48266641633000518, 9.963489011801000217 ) ) ;
#51682 = CARTESIAN_POINT ( 'NONE',  ( -10.48173540582233976, -80.07564442187884879, 3.336307010942487938 ) ) ;
#51683 = CARTESIAN_POINT ( 'NONE',  ( -7.869048196118999527, -79.03113044843098578, 5.428549196144000000 ) ) ;
#51684 = CARTESIAN_POINT ( 'NONE',  ( -7.624341764923000753, -18.73514850530999709, -10.42531124853000080 ) ) ;
#51685 = CARTESIAN_POINT ( 'NONE',  ( -12.70619604129606373, -54.33855724441426815, -1.571828507127614127 ) ) ;
#51686 = VERTEX_POINT ( 'NONE', #5210 ) ;
#51687 = CARTESIAN_POINT ( 'NONE',  ( -1.646570173782999857, -78.66326708118100441, 11.14103995232000166 ) ) ;
#51688 = CARTESIAN_POINT ( 'NONE',  ( 11.02013089939147683, -76.58625517782145664, -1.906531608818739176 ) ) ;
#51689 = CARTESIAN_POINT ( 'NONE',  ( 0.000000000000000000, -6.000000000000000000, 0.000000000000000000 ) ) ;
#51691 = CARTESIAN_POINT ( 'NONE',  ( -12.50000000000000000, -26.93717104351999936, -1.871243407866999974E-13 ) ) ;
#51690 = CARTESIAN_POINT ( 'NONE',  ( 5.137083998358000336, -77.31100733245999379, -10.56753840748999984 ) ) ;
#51692 = CARTESIAN_POINT ( 'NONE',  ( -0.6199991881899920010, -79.06523188490864129, 1.113316751120226211 ) ) ;
#51693 = CARTESIAN_POINT ( 'NONE',  ( -8.627274293348017764, -77.00000000000002842, 3.431425210218347122 ) ) ;
#51694 = CARTESIAN_POINT ( 'NONE',  ( 2.062503053667999797, -58.55736537918999574, -12.92177931905999877 ) ) ;
#51695 = EDGE_CURVE ( 'NONE', #33149, #40044, #41219, .T. ) ;
#51696 = AXIS2_PLACEMENT_3D ( 'NONE', #10004, #54584, #18573 ) ;
#51697 = CARTESIAN_POINT ( 'NONE',  ( 0.05681272259054000184, -79.27140911722999306, -1.352556977364000046 ) ) ;
#51698 = CARTESIAN_POINT ( 'NONE',  ( -1.980584515752000119, -23.26485146623999967, 12.76303204602000108 ) ) ;
#51699 = CARTESIAN_POINT ( 'NONE',  ( 1.250000000000000000, -78.25000000000000000, 0.000000000000000000 ) ) ;
#51700 = CARTESIAN_POINT ( 'NONE',  ( 9.647254834573999460, -79.94705612754898993, -1.526580663425000095 ) ) ;
#51701 = ORIENTED_EDGE ( 'NONE', *, *, #48777, .F. ) ;
#51702 = ORIENTED_EDGE ( 'NONE', *, *, #30669, .T. ) ;
#51703 = CARTESIAN_POINT ( 'NONE',  ( -11.98432456299000037, -77.28116005809600608, -3.448566798086999619 ) ) ;
#51704 = CARTESIAN_POINT ( 'NONE',  ( 2.102229583188283346, -78.74079288752511729, -10.54235425007153992 ) ) ;
#51705 = ORIENTED_EDGE ( 'NONE', *, *, #16481, .F. ) ;
#51706 = CARTESIAN_POINT ( 'NONE',  ( 7.624757993428000091, -18.19647951307999989, 10.47516388919000008 ) ) ;
#51707 = CARTESIAN_POINT ( 'NONE',  ( 1.460959015002472494, -80.17083333333334849, 0.3926218265389232465 ) ) ;
#51708 = CARTESIAN_POINT ( 'NONE',  ( 3.035209552710000036, -78.97670186241998636, -11.67368974080000044 ) ) ;
#51709 = CARTESIAN_POINT ( 'NONE',  ( 8.909545442949999838, -55.64999999967000122, -8.061017305527000687 ) ) ;
#51710 = DIRECTION ( 'NONE',  ( 0.000000000000000000, -1.000000000000000000, 0.000000000000000000 ) ) ;
#51711 = CARTESIAN_POINT ( 'NONE',  ( 0.1963495408493571015, -79.86458333333331439, 1.500000000000000444 ) ) ;
#51712 = CARTESIAN_POINT ( 'NONE',  ( 11.15679540746000065, -79.59213373725799556, 1.159321710118000004 ) ) ;
#51713 = ORIENTED_EDGE ( 'NONE', *, *, #34135, .F. ) ;
#51714 = DIRECTION ( 'NONE',  ( 0.000000000000000000, -1.000000000000000000, 0.000000000000000000 ) ) ;
#51715 = EDGE_LOOP ( 'NONE', ( #46326, #47104 ) ) ;
#51716 = ADVANCED_FACE ( 'NONE', ( #36781 ), #13468, .F. ) ;
#51717 = CARTESIAN_POINT ( 'NONE',  ( 8.640831906552849162, -77.37907852117427865, 3.303617862035461261 ) ) ;
#51718 = CARTESIAN_POINT ( 'NONE',  ( -10.47078769031000078, -78.01612189980698986, -3.499536356729999742 ) ) ;
#51719 = CARTESIAN_POINT ( 'NONE',  ( 6.330072429688197388, -78.17719214551432572, 9.260226347063357011 ) ) ;
#51720 = CARTESIAN_POINT ( 'NONE',  ( -1.256882289721999779, -78.56440746632799232, 0.6559773548962000156 ) ) ;
#51721 = CARTESIAN_POINT ( 'NONE',  ( 1.250000000000000000, -55.54999999966999980, -12.50000000000000000 ) ) ;
#51722 = AXIS2_PLACEMENT_3D ( 'NONE', #433, #31961, #13078 ) ;
#51723 = FACE_OUTER_BOUND ( 'NONE', #24218, .T. ) ;
#51724 = CARTESIAN_POINT ( 'NONE',  ( 1.623578234368999951, -78.14432989285998588, 0.1125035222880000074 ) ) ;
#51725 = CARTESIAN_POINT ( 'NONE',  ( -7.613962745610000304, -18.69360215052999763, 10.53101990620000095 ) ) ;
#51726 = CARTESIAN_POINT ( 'NONE',  ( 3.941639820121999094, -79.33903371854199804, 10.32188786877999931 ) ) ;
#51727 = CARTESIAN_POINT ( 'NONE',  ( -11.15966350340000091, -79.61955349143056537, 4.490997254915999548 ) ) ;
#51728 = FACE_OUTER_BOUND ( 'NONE', #42589, .T. ) ;
#51729 = EDGE_CURVE ( 'NONE', #11813, #55607, #35605, .T. ) ;
#51730 = CARTESIAN_POINT ( 'NONE',  ( 3.432844757780000311, -83.90181010973100229, -0.8928306503459999544 ) ) ;
#51731 = ORIENTED_EDGE ( 'NONE', *, *, #18366, .T. ) ;
#51732 = CARTESIAN_POINT ( 'NONE',  ( 1.570796326794910547, -79.53541666666666288, -11.99999999999999822 ) ) ;
#51733 = CARTESIAN_POINT ( 'NONE',  ( 0.6229729438976999711, -81.23621153953999396, 1.458184003450999855 ) ) ;
#51734 = CARTESIAN_POINT ( 'NONE',  ( -1.407167113863494023, -79.21473436249412714, -10.75055113178693844 ) ) ;
#51735 = EDGE_CURVE ( 'NONE', #16241, #44715, #3907, .T. ) ;
#51736 = CARTESIAN_POINT ( 'NONE',  ( 6.444980599754999595, -77.80409799089798639, -10.09843005143000028 ) ) ;
#51737 = CARTESIAN_POINT ( 'NONE',  ( -7.658894278891000162, -18.79060682915999791, 10.01676917982000070 ) ) ;
#51738 = CARTESIAN_POINT ( 'NONE',  ( 0.7278917586638090631, -78.57707606855669269, 1.047022026650526794 ) ) ;
#51739 = CARTESIAN_POINT ( 'NONE',  ( -11.02533051454918400, -76.36625311331162891, 4.903865969626981069 ) ) ;
#51740 = CARTESIAN_POINT ( 'NONE',  ( 9.430214174385252335, -80.89008252689569645, 5.160773662914198034 ) ) ;
#51741 = CARTESIAN_POINT ( 'NONE',  ( 1.846868607710999921, -78.50252915135698117, 9.341276817324001058 ) ) ;
#51742 = CARTESIAN_POINT ( 'NONE',  ( 1.933650113858000230, -55.39213746940999528, -12.70909635752000177 ) ) ;
#51743 = CARTESIAN_POINT ( 'NONE',  ( -10.95663201459999847, -78.44956549158798964, 1.286059498161999937 ) ) ;
#51744 = CARTESIAN_POINT ( 'NONE',  ( 4.196317941609000179, -80.68300621547570017, -10.07146971829999949 ) ) ;
#51745 = CARTESIAN_POINT ( 'NONE',  ( -1.254047611068101142, -81.16422748949325694, -0.2299481821587232855 ) ) ;
#51746 = VERTEX_POINT ( 'NONE', #13169 ) ;
#51747 = DIRECTION ( 'NONE',  ( 0.000000000000000000, 1.000000000000000000, 0.000000000000000000 ) ) ;
#51748 = CARTESIAN_POINT ( 'NONE',  ( 2.062323307449999810, -60.02713153159000115, -12.83634826445999977 ) ) ;
#51749 = CARTESIAN_POINT ( 'NONE',  ( -7.342356150419299787, -55.61035107872125849, 8.190836719257353238 ) ) ;
#51750 = CARTESIAN_POINT ( 'NONE',  ( -10.58728162385000005, -77.73931716570899653, 3.705074683290000337 ) ) ;
#51751 = CARTESIAN_POINT ( 'NONE',  ( 5.330173052271000245, -78.26479829579199077, 9.594439332582000546 ) ) ;
#51752 = CARTESIAN_POINT ( 'NONE',  ( -0.8459884596345884633, -79.42721677660425428, -1.250127555251149047 ) ) ;
#51753 = CARTESIAN_POINT ( 'NONE',  ( 4.048411298789319268, -83.94166666306279012, -0.1471474844110896574 ) ) ;
#51754 = CARTESIAN_POINT ( 'NONE',  ( -10.12290050255000118, -60.04999997790999799, 7.648026768390999486 ) ) ;
#51755 = DIRECTION ( 'NONE',  ( -0.7071067811865475727, 0.000000000000000000, -0.7071067811865475727 ) ) ;
#51756 = CARTESIAN_POINT ( 'NONE',  ( 3.973865631610368432, -79.15970006417956029, -8.444888605590360697 ) ) ;
#51757 = ORIENTED_EDGE ( 'NONE', *, *, #29220, .T. ) ;
#51758 = CARTESIAN_POINT ( 'NONE',  ( -0.9200625262326408427, -80.04125824231630304, 0.8460283513402829803 ) ) ;
#51759 = ADVANCED_FACE ( 'NONE', ( #54225 ), #19018, .T. ) ;
#51760 = CARTESIAN_POINT ( 'NONE',  ( -11.00000000000000000, -78.19999999999998863, 0.000000000000000000 ) ) ;
#51761 = CARTESIAN_POINT ( 'NONE',  ( -8.192247052095000370, -78.30244779722698922, -7.574872137178000564 ) ) ;
#51762 = CARTESIAN_POINT ( 'NONE',  ( -12.00000000000000178, -76.81041666666666856, -1.570796326794897890 ) ) ;
#51763 = CARTESIAN_POINT ( 'NONE',  ( 6.043427764450807871, -79.46666666666666856, -10.48543666025108934 ) ) ;
#51764 = CARTESIAN_POINT ( 'NONE',  ( -7.624341764906000130, -55.53514850498000044, -10.42531124851000079 ) ) ;
#51765 = CARTESIAN_POINT ( 'NONE',  ( 0.3895721858179450048, -82.99511992827669360, -1.461044772055308361 ) ) ;
#51766 = CARTESIAN_POINT ( 'NONE',  ( -1.124179317452199900, -79.63649961456538051, -0.5465545694080121697 ) ) ;
#51767 = EDGE_CURVE ( 'NONE', #35617, #17140, #35031, .T. ) ;
#51768 = VECTOR ( 'NONE', #50193, 1000.000000000000114 ) ;
#51769 = CARTESIAN_POINT ( 'NONE',  ( -10.41144070831380120, -55.27453159746022493, 7.610433246081189651 ) ) ;
#51770 = ORIENTED_EDGE ( 'NONE', *, *, #17071, .T. ) ;
#51771 = B_SPLINE_CURVE_WITH_KNOTS ( 'NONE', 3,
 ( #37972, #11994, #6976, #25556 ),
 .UNSPECIFIED., .F., .F.,
 ( 4, 4 ),
 ( 0.7499999933975610711, 1.000000000000000000 ),
 .UNSPECIFIED. ) ;
#51772 = EDGE_CURVE ( 'NONE', #52707, #18726, #9058, .T. ) ;
#51773 = CARTESIAN_POINT ( 'NONE',  ( 1.667936688463999895, -19.23513569609999863, 12.53239398062000198 ) ) ;
#51774 = DIRECTION ( 'NONE',  ( 0.000000000000000000, 1.000000000000000000, 0.000000000000000000 ) ) ;
#51775 = ORIENTED_EDGE ( 'NONE', *, *, #28319, .F. ) ;
#51776 = ORIENTED_EDGE ( 'NONE', *, *, #53892, .F. ) ;
#51777 = CARTESIAN_POINT ( 'NONE',  ( -12.79895942951000087, -54.99538174351000208, -2.015930660723999956 ) ) ;
#51778 = ORIENTED_EDGE ( 'NONE', *, *, #51729, .F. ) ;
#51779 = ORIENTED_EDGE ( 'NONE', *, *, #37648, .F. ) ;
#51780 = CARTESIAN_POINT ( 'NONE',  ( 0.5506765233277000071, -16.74045707756000212, 12.77514798311000099 ) ) ;
#51781 = CARTESIAN_POINT ( 'NONE',  ( 10.01578477942999967, -77.35596644471499417, 4.342743515613999961 ) ) ;
#51782 = AXIS2_PLACEMENT_3D ( 'NONE', #19907, #20484, #11344 ) ;
#51783 = DIRECTION ( 'NONE',  ( 1.000000000000000000, 0.000000000000000000, 0.000000000000000000 ) ) ;
#51784 = ADVANCED_BREP_SHAPE_REPRESENTATION ( '', ( #17297, #43526 ), #53938 ) ;
#51785 = CARTESIAN_POINT ( 'NONE',  ( -9.050966799188000067, -59.94999999967000548, 7.919595949288999570 ) ) ;
#51786 = CARTESIAN_POINT ( 'NONE',  ( 9.797588846018999931, -78.94441332859899774, 0.1600704101387999956 ) ) ;
#51787 = CARTESIAN_POINT ( 'NONE',  ( -1.787026317784608631, -78.20960545061939229, -9.075693917138710987 ) ) ;
#51788 = CARTESIAN_POINT ( 'NONE',  ( -7.409043029364259958, -79.44809193424394778, 5.667876244604902247 ) ) ;
#51789 = ORIENTED_EDGE ( 'NONE', *, *, #18288, .T. ) ;
#51790 = VERTEX_POINT ( 'NONE', #10517 ) ;
#51791 = CARTESIAN_POINT ( 'NONE',  ( 12.60354432329999952, -59.55100837068999908, 1.750000000001000089 ) ) ;
#51792 = CARTESIAN_POINT ( 'NONE',  ( -11.36512682855694933, -76.92683455540999660, -3.982123233434259557 ) ) ;
#51793 = CARTESIAN_POINT ( 'NONE',  ( -12.77562710770000187, -62.06233677629000312, -0.5428386295904999992 ) ) ;
#51794 = CARTESIAN_POINT ( 'NONE',  ( -0.1538805260929999863, -78.20641338939098830, 9.702939253146000809 ) ) ;
#51795 = CARTESIAN_POINT ( 'NONE',  ( -0.1636246173744726473, -79.88541666666664298, 1.249999999999999112 ) ) ;
#51796 = CARTESIAN_POINT ( 'NONE',  ( 9.872209700914000408, -78.94710244883999906, -6.668650957345999331 ) ) ;
#51797 = CARTESIAN_POINT ( 'NONE',  ( 1.511505244404999893, -80.48109529231999204, 0.4793209935110999687 ) ) ;
#51798 = FACE_OUTER_BOUND ( 'NONE', #54311, .T. ) ;
#51799 = CARTESIAN_POINT ( 'NONE',  ( -10.78576251690998689, -76.66714693325138796, 4.661353383015510943 ) ) ;
#51800 = CYLINDRICAL_SURFACE ( 'NONE', #36071, 1.500000000000000000 ) ;
#51801 = CARTESIAN_POINT ( 'NONE',  ( -9.516265623847999677, -53.97460635707999899, 8.227505979398999969 ) ) ;
#51802 = CARTESIAN_POINT ( 'NONE',  ( -0.8644569908188000085, -78.82506332859900056, 9.872851397518997985 ) ) ;
#51803 = CARTESIAN_POINT ( 'NONE',  ( -1.407069491366080172, -76.71471916496845722, -10.74971761791662672 ) ) ;
#51804 = CARTESIAN_POINT ( 'NONE',  ( -7.633088938756000807, -18.60992532424000245, -10.18115029113000070 ) ) ;
#51806 = CARTESIAN_POINT ( 'NONE',  ( 0.000000000000000000, -87.29999999999999716, 0.000000000000000000 ) ) ;
#51805 = DIRECTION ( 'NONE',  ( -1.000000000000000000, 0.000000000000000000, 0.000000000000000000 ) ) ;
#51807 = AXIS2_PLACEMENT_3D ( 'NONE', #8843, #18806, #824 ) ;
#51808 = CARTESIAN_POINT ( 'NONE',  ( -0.4250565598266470846, -1.216173826220077414, -3.248535750966747848 ) ) ;
#51809 = CARTESIAN_POINT ( 'NONE',  ( -4.124900980777000292, -80.39812822292799410, 10.39307513819000128 ) ) ;
#51810 = CARTESIAN_POINT ( 'NONE',  ( 9.722718241315000398, -60.04999999966999980, 7.954951288349001004 ) ) ;
#51811 = DIRECTION ( 'NONE',  ( 0.000000000000000000, -1.000000000000000000, 0.000000000000000000 ) ) ;
#51812 = CARTESIAN_POINT ( 'NONE',  ( 3.351413303022582557, -1.530878857503674695, 1.345052432851818747 ) ) ;
#51813 = EDGE_LOOP ( 'NONE', ( #3789, #33141, #57757, #32284 ) ) ;
#51814 = CARTESIAN_POINT ( 'NONE',  ( -9.500000000000000000, -77.39999999999999147, 0.000000000000000000 ) ) ;
#51815 = DIRECTION ( 'NONE',  ( -1.000000000000000000, 0.000000000000000000, 0.000000000000000000 ) ) ;
#51816 = CARTESIAN_POINT ( 'NONE',  ( 0.000000000000000000, -46.09579702914000165, 0.000000000000000000 ) ) ;
#51817 = CARTESIAN_POINT ( 'NONE',  ( 1.250000728980784181, -78.35225028680585524, 0.03536658250550711591 ) ) ;
#51818 = CARTESIAN_POINT ( 'NONE',  ( -8.807539493945000686, -79.35970150572998705, 3.924989019749000274 ) ) ;
#51819 = CIRCLE ( 'NONE', #21611, 13.89999999999999858 ) ;
#51820 = CARTESIAN_POINT ( 'NONE',  ( -10.68082442906623797, -77.08973694601026239, 1.407256659424358070 ) ) ;
#51821 = DIRECTION ( 'NONE',  ( 0.000000000000000000, 1.000000000000000000, 0.000000000000000000 ) ) ;
#51822 = CARTESIAN_POINT ( 'NONE',  ( 2.157438503070702840, -79.45895713229609214, 10.55436150663177663 ) ) ;
#51823 = AXIS2_PLACEMENT_3D ( 'NONE', #51268, #15528, #14931 ) ;
#51824 = EDGE_CURVE ( 'NONE', #29475, #47200, #15226, .T. ) ;
#51825 = DIRECTION ( 'NONE',  ( 0.000000000000000000, 1.000000000000000000, 0.000000000000000000 ) ) ;
#51826 = CARTESIAN_POINT ( 'NONE',  ( 2.264809212410999647E-14, -92.79999999999999716, 0.000000000000000000 ) ) ;
#51827 = ADVANCED_FACE ( 'NONE', ( #14635 ), #2248, .F. ) ;
#51828 = CARTESIAN_POINT ( 'NONE',  ( -0.008152559635135000343, -77.74587287048397855, 10.94781514982000203 ) ) ;
#51829 = CARTESIAN_POINT ( 'NONE',  ( 9.516658938990653738, -76.39971689995223869, -6.891841626549551236 ) ) ;
#51830 = CARTESIAN_POINT ( 'NONE',  ( 8.230685248251999653, -77.89996571856799790, -7.517341346183999740 ) ) ;
#51831 = DIRECTION ( 'NONE',  ( 0.000000000000000000, 1.000000000000000000, 0.000000000000000000 ) ) ;
#51832 = DIRECTION ( 'NONE',  ( 0.000000000000000000, -1.000000000000000000, 0.000000000000000000 ) ) ;
#51833 = CARTESIAN_POINT ( 'NONE',  ( -1.210822168571075830, -78.38541666666668561, 9.250000000000000000 ) ) ;
#51834 = CARTESIAN_POINT ( 'NONE',  ( -10.71369944335148183, -77.57916666666665151, 2.879226727952040932 ) ) ;
#51835 = CARTESIAN_POINT ( 'NONE',  ( 7.429570834404548130, -80.28571891368410718, -7.771422698336870383 ) ) ;
#51836 = CARTESIAN_POINT ( 'NONE',  ( 0.000000000000000000, -0.2000000000000000111, 0.000000000000000000 ) ) ;
#51837 = LINE ( 'NONE', #1961, #262 ) ;
#51838 = EDGE_CURVE ( 'NONE', #33222, #2177, #49183, .T. ) ;
#51839 = CARTESIAN_POINT ( 'NONE',  ( 8.348735229153000148, -78.94600801619300512, 8.268078378528999295 ) ) ;
#51840 = DIRECTION ( 'NONE',  ( -1.000000000000000000, 0.000000000000000000, 0.000000000000000000 ) ) ;
#51841 = DIRECTION ( 'NONE',  ( 0.000000000000000000, -1.000000000000000000, 0.000000000000000000 ) ) ;
#51842 = ORIENTED_EDGE ( 'NONE', *, *, #9953, .F. ) ;
#51843 = CARTESIAN_POINT ( 'NONE',  ( 12.50745077490000057, -17.00005551713000074, -2.011911479242000131E-09 ) ) ;
#51844 = ORIENTED_EDGE ( 'NONE', *, *, #36092, .F. ) ;
#51845 = ORIENTED_EDGE ( 'NONE', *, *, #54774, .T. ) ;
#51846 = CARTESIAN_POINT ( 'NONE',  ( -3.075537641221531615, -77.40416666666668277, -11.44417895085270942 ) ) ;
#51847 = CARTESIAN_POINT ( 'NONE',  ( -3.522252620761999964, -78.93456160447509262, -0.6907526756895999709 ) ) ;
#51848 = CARTESIAN_POINT ( 'NONE',  ( 7.698542609049095375, -79.19952453424221517, 5.565885376627822900 ) ) ;
#51849 = EDGE_CURVE ( 'NONE', #22214, #36179, #55971, .T. ) ;
#51850 = VERTEX_POINT ( 'NONE', #50965 ) ;
#51851 = CARTESIAN_POINT ( 'NONE',  ( 7.601397897754999633, -60.04999999725999515, -10.07627163191000008 ) ) ;
#51852 = ORIENTED_EDGE ( 'NONE', *, *, #2432, .F. ) ;
#51853 = CARTESIAN_POINT ( 'NONE',  ( 0.000000000000000000, -92.39999999999999147, 0.000000000000000000 ) ) ;
#51854 = ORIENTED_EDGE ( 'NONE', *, *, #45586, .F. ) ;
#51855 = LINE ( 'NONE', #11410, #17707 ) ;
#51856 = CARTESIAN_POINT ( 'NONE',  ( 0.9293276542485822134, -78.57344452540336022, 1.219933349864354977 ) ) ;
#51857 = CARTESIAN_POINT ( 'NONE',  ( -7.533402290670649926, -79.79999999999999716, -9.189679446819413400 ) ) ;
#51858 = CARTESIAN_POINT ( 'NONE',  ( -8.652941401739491667, -80.04965019796203762, 6.378618437432542976 ) ) ;
#51859 = VECTOR ( 'NONE', #24813, 1000.000000000000227 ) ;
#51860 = CARTESIAN_POINT ( 'NONE',  ( 10.16273287016798754, -79.15293570561394176, -6.864898572566356272 ) ) ;
#51861 = CARTESIAN_POINT ( 'NONE',  ( 0.4132205903738334074, -86.09999999999998010, -3.926276861431333920 ) ) ;
#51862 = CARTESIAN_POINT ( 'NONE',  ( -1.660522255173999984, -76.78854216438499236, 11.05968181062000077 ) ) ;
#51863 = CARTESIAN_POINT ( 'NONE',  ( -3.574427999287489222, -79.75479980213101783, 9.034856847799710877 ) ) ;
#51864 = CARTESIAN_POINT ( 'NONE',  ( -0.5175072279577125345, -76.97066086130449492, -9.610596997971313726 ) ) ;
#51865 = CARTESIAN_POINT ( 'NONE',  ( 7.729696734268999947, -76.57734026635199598, -7.985700370870999265 ) ) ;
#51866 = CARTESIAN_POINT ( 'NONE',  ( -3.532846115401338860, -78.69390980651986922, -8.548707026569838163 ) ) ;
#51867 = CARTESIAN_POINT ( 'NONE',  ( -1.193181427976999887, -77.39188667140099653, 9.445003550666001502 ) ) ;
#51868 = CARTESIAN_POINT ( 'NONE',  ( -1.154258600661999923, -79.71986326112400434, -0.6680293646364998672 ) ) ;
#51869 = CARTESIAN_POINT ( 'NONE',  ( 0.000000000000000000, -69.16102867818000277, 0.000000000000000000 ) ) ;
#51870 = CARTESIAN_POINT ( 'NONE',  ( 8.300970689365438915, -77.09166666666668277, 4.784380313523563188 ) ) ;
#51871 = CARTESIAN_POINT ( 'NONE',  ( 2.498944011016999589, -80.84653455456798099, 2.804753272470999814 ) ) ;
#51872 = CARTESIAN_POINT ( 'NONE',  ( -2.502260836693999568, -79.61742578125399916, -11.94101425180999954 ) ) ;
#51873 = CARTESIAN_POINT ( 'NONE',  ( -9.295691395107468225, -78.05822132751052322, 5.400626663501747693 ) ) ;
#51874 = CARTESIAN_POINT ( 'NONE',  ( -0.08551465511880061710, -82.98103542870875060, 1.246841896993040155 ) ) ;
#51875 =( NAMED_UNIT ( * ) PLANE_ANGLE_UNIT ( ) SI_UNIT ( $, .RADIAN. ) );
#51876 = CARTESIAN_POINT ( 'NONE',  ( 3.430559350187999623, -83.94574735065199889, -0.8923151533959999826 ) ) ;
#51877 = CARTESIAN_POINT ( 'NONE',  ( 10.59551070212000035, -21.75648180056000314, 7.678690995204998870 ) ) ;
#51878 = CARTESIAN_POINT ( 'NONE',  ( -7.761030428359000588, -60.88151201342000007, -9.835168816246000034 ) ) ;
#51879 = CARTESIAN_POINT ( 'NONE',  ( -4.784380313523575623, -78.31666666666669130, 8.300970689365433586 ) ) ;
#51880 = CARTESIAN_POINT ( 'NONE',  ( -0.7068627984950999199, -81.05379363128199088, 1.130893941374999878 ) ) ;
#51881 = MECHANICAL_DESIGN_GEOMETRIC_PRESENTATION_REPRESENTATION (  '', ( #36766 ), #39628 ) ;
#51882 = CARTESIAN_POINT ( 'NONE',  ( -12.61271781521000079, -18.80306329050999992, -1.798333084007999849 ) ) ;
#51883 = CARTESIAN_POINT ( 'NONE',  ( 12.66322140209000047, -25.18161935732999623, 0.1487435796151999889 ) ) ;
#51884 = CARTESIAN_POINT ( 'NONE',  ( -9.429661037469928786, -77.99063298084412565, -5.207437231424048463 ) ) ;
#51885 = CARTESIAN_POINT ( 'NONE',  ( -11.75346344166169743, -78.20980192672932674, -1.536536421794175489 ) ) ;
#51886 = B_SPLINE_CURVE_WITH_KNOTS ( 'NONE', 3,
 ( #48273, #25810, #29649, #20524, #30520, #16384, #21379, #52402 ),
 .UNSPECIFIED., .F., .F.,
 ( 4, 2, 2, 4 ),
 ( 0.7143499438395097823, 0.8571749719197548911, 0.9285874859598775011, 1.000000000000000000 ),
 .UNSPECIFIED. ) ;
#51887 = CARTESIAN_POINT ( 'NONE',  ( -12.49999990534960226, -49.87071424677999687, -0.001538265197294672385 ) ) ;
#51888 = CARTESIAN_POINT ( 'NONE',  ( 8.663048543576998384, -75.68023594616001049, -9.028321399273000480 ) ) ;
#51889 = EDGE_LOOP ( 'NONE', ( #608, #33879, #14161, #52487 ) ) ;
#51890 = LINE ( 'NONE', #21154, #17282 ) ;
#51891 = CARTESIAN_POINT ( 'NONE',  ( 12.61117499584999813, -60.01550664522000034, 1.798980867982999943 ) ) ;
#51892 = CARTESIAN_POINT ( 'NONE',  ( -8.799409365152000007, -79.31836356187000092, -8.853116023008999136 ) ) ;
#51893 = CARTESIAN_POINT ( 'NONE',  ( 12.65987793659000005, -53.86302453462000273, -0.9847129294438998759 ) ) ;
#51894 = CARTESIAN_POINT ( 'NONE',  ( -9.721291027688000241, -77.32430961238299005, 0.5965459135820000425 ) ) ;
#51895 = B_SPLINE_CURVE_WITH_KNOTS ( 'NONE', 3,
 ( #11150, #33553, #6701, #24120, #29124, #20571, #47170, #29412, #37698, #6988, #34416, #6405, #52164, #24712, #42138, #24993, #43014, #38856 ),
 .UNSPECIFIED., .F., .F.,
 ( 4, 2, 2, 2, 2, 2, 2, 2, 4 ),
 ( 0.000000000000000000, 0.1249999999999999722, 0.2500000000000000000, 0.3750000000000000000, 0.5000000000000001110, 0.6250000000000001110, 0.7500000000000000000, 0.8750000000000000000, 1.000000000000000000 ),
 .UNSPECIFIED. ) ;
#51896 = CARTESIAN_POINT ( 'NONE',  ( -11.79999999988000070, -18.85000000520999919, -0.5999999998848000171 ) ) ;
#51897 = CARTESIAN_POINT ( 'NONE',  ( 0.000000000000000000, -75.15999999999999659, 0.000000000000000000 ) ) ;
#51898 = DIRECTION ( 'NONE',  ( -0.9999999999995751176, 0.000000000000000000, -9.217549095371770968E-07 ) ) ;
#51899 = ORIENTED_EDGE ( 'NONE', *, *, #17131, .F. ) ;
#51900 = CARTESIAN_POINT ( 'NONE',  ( 0.000000000000000000, -81.10000000285099020, -7.000000000000000000 ) ) ;
#51901 = AXIS2_PLACEMENT_3D ( 'NONE', #28851, #11741, #51898 ) ;
#51902 = CARTESIAN_POINT ( 'NONE',  ( 0.4866655842918644614, -78.90438882479159588, -3.447293470213554034 ) ) ;
#51903 = VERTEX_POINT ( 'NONE', #28200 ) ;
#51904 = EDGE_CURVE ( 'NONE', #670, #35536, #15523, .T. ) ;
#51905 = CARTESIAN_POINT ( 'NONE',  ( -0.9420598709024999851, -79.19141207666899618, -0.8215979549846998964 ) ) ;
#51906 = CARTESIAN_POINT ( 'NONE',  ( 9.366620387600999464, -79.01244768766198945, -5.860402389062000061 ) ) ;
#51907 = CARTESIAN_POINT ( 'NONE',  ( 10.90625000000000000, -80.29374999999798490, -5.301077343649000152E-10 ) ) ;
#51908 = CARTESIAN_POINT ( 'NONE',  ( 6.233047529871999615, -78.88050366622999832, 9.960502923565000444 ) ) ;
#51909 = VERTEX_POINT ( 'NONE', #46841 ) ;
#51910 = CARTESIAN_POINT ( 'NONE',  ( 11.71313121114000033, -78.98711054799299802, -3.284064838691000077 ) ) ;
#51911 = CARTESIAN_POINT ( 'NONE',  ( 8.143733331677999843, -77.86805683836598746, 7.865865880590998671 ) ) ;
#51912 = ORIENTED_EDGE ( 'NONE', *, *, #34287, .F. ) ;
#51913 = ORIENTED_EDGE ( 'NONE', *, *, #26314, .F. ) ;
#51914 = CARTESIAN_POINT ( 'NONE',  ( -0.8719868943402252492, -80.53708738304344195, 0.8952310760180179905 ) ) ;
#51915 =( GEOMETRIC_REPRESENTATION_CONTEXT ( 3 ) GLOBAL_UNCERTAINTY_ASSIGNED_CONTEXT ( ( #47875 ) ) GLOBAL_UNIT_ASSIGNED_CONTEXT ( ( #376, #48774, #4186 ) ) REPRESENTATION_CONTEXT ( 'NONE', 'WORKASPACE' ) );
#51916 = CARTESIAN_POINT ( 'NONE',  ( 9.542482966934999311, -76.87973998579799684, 0.04799272824659999576 ) ) ;
#51917 = CARTESIAN_POINT ( 'NONE',  ( -2.116314338179000387, -80.35763280188051283, -9.535298106756000536 ) ) ;
#51918 = ADVANCED_FACE ( 'NONE', ( #20248 ), #28501, .T. ) ;
#51919 = ORIENTED_EDGE ( 'NONE', *, *, #38292, .T. ) ;
#51920 = CARTESIAN_POINT ( 'NONE',  ( -12.72966770606090670, -23.76881200365143698, -1.931346186345864746 ) ) ;
#51921 = CARTESIAN_POINT ( 'NONE',  ( 6.695505957611000092, -78.89586737597099386, 8.622387486181999350 ) ) ;
#51922 = AXIS2_PLACEMENT_3D ( 'NONE', #52619, #47343, #43766 ) ;
#51923 = VERTEX_POINT ( 'NONE', #55090 ) ;
#51924 = CARTESIAN_POINT ( 'NONE',  ( -8.595201249227393703, -80.65211028413133931, -6.605388001086274663 ) ) ;
#51925 = CARTESIAN_POINT ( 'NONE',  ( -0.7479529023060000892, -77.62856915034599581, -9.465622776916999825 ) ) ;
#51926 = CARTESIAN_POINT ( 'NONE',  ( 12.76303204298000082, -60.06485150663000638, -1.980584515756000030 ) ) ;
#51927 = FACE_OUTER_BOUND ( 'NONE', #20123, .T. ) ;
#51928 = CARTESIAN_POINT ( 'NONE',  ( 0.9218200799623692543, -81.22291666666669130, 1.199500263597272687 ) ) ;
#51929 = CARTESIAN_POINT ( 'NONE',  ( 5.896171905175000560, -77.86999999999999034, 7.127247495676000355 ) ) ;
#51930 = CARTESIAN_POINT ( 'NONE',  ( 6.905509799642000068, -76.92767797598149571, 6.754875825283999546 ) ) ;
#51931 = DIRECTION ( 'NONE',  ( -2.678911359553000079E-11, 1.000000000000000000, -2.678929432950999965E-11 ) ) ;
#51932 = CARTESIAN_POINT ( 'NONE',  ( 3.845056324898657785, -82.38072918665125144, -1.147388926672712639 ) ) ;
#51933 = CARTESIAN_POINT ( 'NONE',  ( 3.295079792876999925, -76.30143611710998641, 11.86077433336000020 ) ) ;
#51934 = AXIS2_PLACEMENT_3D ( 'NONE', #29574, #19065, #18769 ) ;
#51935 = EDGE_CURVE ( 'NONE', #10344, #8584, #37364, .T. ) ;
#51936 = CARTESIAN_POINT ( 'NONE',  ( 0.000000000000000000, -81.10000000285099020, -8.099999997149000208 ) ) ;
#51937 = AXIS2_PLACEMENT_3D ( 'NONE', #541, #27058, #54535 ) ;
#51938 = CARTESIAN_POINT ( 'NONE',  ( 7.069026039852619014, -77.18437499998694307, -6.033943155702938377 ) ) ;
#51939 = CARTESIAN_POINT ( 'NONE',  ( 9.422842877325999567, -62.05952027250000214, -8.643944052328999206 ) ) ;
#51940 = CARTESIAN_POINT ( 'NONE',  ( 9.369164850722000892, -23.25000000000000000, -7.601397897754999633 ) ) ;
#51941 = CARTESIAN_POINT ( 'NONE',  ( -7.650089724727000551, -76.56980357461999631, -9.607224057717001386 ) ) ;
#51942 = CARTESIAN_POINT ( 'NONE',  ( -9.500000000000000000, -78.88958333333330586, 1.243547092045920399 ) ) ;
#51943 = CARTESIAN_POINT ( 'NONE',  ( -11.88755474194624817, -78.03426394915543085, 2.371826327494228615 ) ) ;
#51944 = DIRECTION ( 'NONE',  ( 0.000000000000000000, -1.000000000000000000, 0.000000000000000000 ) ) ;
#51945 = ORIENTED_EDGE ( 'NONE', *, *, #56303, .F. ) ;
#51946 = CARTESIAN_POINT ( 'NONE',  ( -0.06677702975030901100, -80.87140776427570188, -1.508501679119423677 ) ) ;
#51947 = CARTESIAN_POINT ( 'NONE',  ( -3.484330481557000425, -77.42609236341799317, 8.711138713857000226 ) ) ;
#51948 = CARTESIAN_POINT ( 'NONE',  ( 0.000000000000000000, 0.000000000000000000, -12.00000000000000000 ) ) ;
#51949 = CARTESIAN_POINT ( 'NONE',  ( -1.199500263597270022, -78.55208333333332860, -0.9218200799623730290 ) ) ;
#51950 = CARTESIAN_POINT ( 'NONE',  ( -1.781396697799999984, -3.385272489337999957, 3.079626043334999785 ) ) ;
#51951 = CARTESIAN_POINT ( 'NONE',  ( -11.92228046151999976, -78.42521964476598839, 2.416973144693999931 ) ) ;
#51952 = CARTESIAN_POINT ( 'NONE',  ( -0.1544424224854999972, -78.14707553773099846, 9.738369639964998825 ) ) ;
#51954 = CARTESIAN_POINT ( 'NONE',  ( 10.14950121162999963, -19.24922972541000021, -7.674627477474999182 ) ) ;
#51953 = CARTESIAN_POINT ( 'NONE',  ( -4.649632569072141841, -76.10711892059522654, 10.80545511456402608 ) ) ;
#51955 = CARTESIAN_POINT ( 'NONE',  ( -10.90022919700999893, -79.02221245318798992, 0.6003077901278000006 ) ) ;
#51956 = CARTESIAN_POINT ( 'NONE',  ( -9.946797292890842357, -79.56914397919975102, 4.077092203015069138 ) ) ;
#51957 = ORIENTED_EDGE ( 'NONE', *, *, #25410, .F. ) ;
#51958 = CARTESIAN_POINT ( 'NONE',  ( 1.500000000000000222, -81.13359037631325066, -0.3093141193355204432 ) ) ;
#51959 = LINE ( 'NONE', #29494, #11665 ) ;
#51960 = TOROIDAL_SURFACE ( 'NONE', #50071, 17.50000000000000000, 5.000000000000000000 ) ;
#51961 = CARTESIAN_POINT ( 'NONE',  ( 1.997276839918466829, -2.322916666666665630, 2.598917237794090784 ) ) ;
#51962 = CARTESIAN_POINT ( 'NONE',  ( -0.5849273512657638951, -82.25000000000000000, -1.109837523374604729 ) ) ;
#51963 = CARTESIAN_POINT ( 'NONE',  ( -1.980584515756000030, -18.73514849905999924, 12.76303204340999997 ) ) ;
#51964 = DIRECTION ( 'NONE',  ( 0.000000000000000000, 0.000000000000000000, -1.000000000000000000 ) ) ;
#51965 = CYLINDRICAL_SURFACE ( 'NONE', #1336, 0.6000000000000008660 ) ;
#51966 = CARTESIAN_POINT ( 'NONE',  ( -8.082524092276882399, -79.04166666666665719, -4.658475568430820779 ) ) ;
#51967 = ORIENTED_EDGE ( 'NONE', *, *, #50436, .T. ) ;
#51968 = CARTESIAN_POINT ( 'NONE',  ( 11.18604332926000033, -79.01733954020500050, -1.306292155029999957 ) ) ;
#51969 = CARTESIAN_POINT ( 'NONE',  ( -1.432444700303164398, -76.23510798997345717, 11.09171988620980187 ) ) ;
#51970 = CARTESIAN_POINT ( 'NONE',  ( -3.616527695712999702, -1.759176978014000081, -0.5438149879621999583 ) ) ;
#51971 = CARTESIAN_POINT ( 'NONE',  ( 7.685661446562000343, -79.50000000000000000, -5.583959896778000420 ) ) ;
#51972 = ADVANCED_FACE ( 'NONE', ( #11395 ), #43544, .T. ) ;
#51973 = CARTESIAN_POINT ( 'NONE',  ( 0.8462078165385277240, -81.41624116930810828, 0.9198965729622936571 ) ) ;
#51974 = B_SPLINE_CURVE_WITH_KNOTS ( 'NONE', 3,
 ( #54379, #17180, #22187, #8322, #9498, #3890, #21892, #21610, #49953, #58210, #44059, #17771, #39617, #57623, #35760, #35166, #53790, #37222, #36643, #23066, #15382, #41080, #10088, #1820, #46703, #27483, #5933, #23364, #54662, #36933, #33376, #28067, #5356, #46114, #37810, #42257, #10675, #55831, #19521, #6224, #32489, #15080, #55532, #10371, #51412, #5639, #19817, #32201, #14203, #45525, #51122, #27777, #5070, #50241, #9791, #41956, #671, #18656, #41375, #957, #33077, #28654, #1526, #28359, #24239, #45820, #46406, #18941, #23938, #23649, #54945, #37514, #14496, #50533, #41662, #1241, #19231, #55238, #14784, #32781, #50826, #24818, #16254, #6518, #51988, #43701, #30088, #10965, #47855, #6810, #20110, #20390, #57264, #11542, #47281, #29519, #21246, #25674, #52551, #39248, #2962, #56977, #15667, #16539, #38965, #52269, #16830, #47575, #3257, #33664, #38101, #28948, #34519, #11252, #34812, #51704, #29232, #25385, #46990, #24528, #42833, #2394, #12106, #48141, #15957, #11823, #7672, #38676, #56408, #42543, #20960, #56121, #2111, #38388, #7384, #43400, #33948, #7101, #25100, #43124, #2683, #20677, #56696, #34232, #29799, #39542, #49591, #4711, #17995, #39827, #27122, #30382, #13553, #22710, #12392, #9137, #35689, #54012, #49288, #45162, #48421, #44266, #22112, #57548, #40723, #48992, #58134, #21823, #315, #4111, #3821, #48706, #26829, #40121 ),
 .UNSPECIFIED., .F., .F.,
 ( 4, 2, 2, 2, 1, 1, 1, 2, 2, 2, 2, 1, 1, 1, 1, 1, 2, 2, 2, 2, 2, 1, 1, 1, 1, 2, 2, 2, 1, 2, 2, 1, 1, 1, 1, 1, 1, 2, 2, 2, 2, 2, 1, 1, 1, 2, 2, 2, 2, 1, 1, 1, 2, 2, 2, 2, 1, 1, 1, 2, 2, 2, 1, 1, 1, 1, 1, 2, 2, 2, 2, 2, 1, 1, 1, 1, 2, 2, 2, 2, 1, 1, 2, 2, 2, 2, 2, 2, 2, 1, 1, 1, 2, 2, 2, 1, 1, 2, 2, 1, 1, 2, 2, 2, 2, 1, 2, 2, 1, 2, 4 ),
 ( 0.000000000000000000, 0.03125000000001028344, 0.04687500000001543904, 0.05468750000001802031, 0.05859375000001933176, 0.06054687500001998401, 0.06152343750002028933, 0.06201171875002044198, 0.06250000000002059464, 0.09375000000002767231, 0.1093750000000312250, 0.1171875000000330153, 0.1210937500000338479, 0.1230468750000342781, 0.1240234375000345557, 0.1245117187500346806, 0.1247558593750347222, 0.1250000000000347500, 0.1562500000000413836, 0.1718750000000447142, 0.1796875000000463518, 0.1835937500000472122, 0.1855468750000476008, 0.1865234375000477673, 0.1870117187500478784, 0.1872558593750479339, 0.1875000000000479894, 0.2031250000000475731, 0.2109375000000473233, 0.2148437500000472122, 0.2187500000000471012, 0.2343750000000465461, 0.2421875000000462408, 0.2460937500000460743, 0.2480468750000459355, 0.2490234375000458522, 0.2495117187500458522, 0.2497558593750458522, 0.2500000000000458522, 0.2656250000000456857, 0.2734375000000455191, 0.2773437500000454081, 0.2792968750000453526, 0.2802734375000452416, 0.2807617187500451861, 0.2810058593750451861, 0.2812500000000451306, 0.2968750000000437428, 0.3046875000000430767, 0.3085937500000427991, 0.3105468750000426326, 0.3115234375000425771, 0.3120117187500426326, 0.3125000000000426326, 0.3281250000000437983, 0.3359375000000443534, 0.3398437500000446865, 0.3417968750000447975, 0.3427734375000449085, 0.3432617187500449640, 0.3437500000000450195, 0.3593750000000483502, 0.3671875000000500711, 0.3710937500000509592, 0.3730468750000513478, 0.3740234375000516254, 0.3745117187500517364, 0.3747558593750517919, 0.3750000000000517919, 0.4062500000000540679, 0.4218750000000552336, 0.4296875000000557887, 0.4335937500000561218, 0.4355468750000562883, 0.4365234375000562883, 0.4370117187500562328, 0.4372558593750562328, 0.4375000000000562328, 0.4687500000000556777, 0.4843750000000553446, 0.4921875000000552336, 0.4960937500000551226, 0.4980468750000550671, 0.5000000000000550671, 0.5625000000000539568, 0.6250000000000528466, 0.6406250000000527356, 0.6425781250000527356, 0.6435546875000526246, 0.6445312500000526246, 0.6484375000000526246, 0.6562500000000525135, 0.6875000000000519584, 0.7500000000000506262, 0.8125000000000492939, 0.8437500000000486278, 0.8476562500000485167, 0.8496093750000485167, 0.8500976562500485167, 0.8505859375000484057, 0.8515625000000484057, 0.8593750000000480727, 0.8750000000000474065, 0.9062500000000462963, 0.9218750000000457412, 0.9238281250000458522, 0.9248046875000452971, 0.9257812500000447420, 0.9296875000000424105, 0.9375000000000376366, 1.000000000000000000 ),
 .UNSPECIFIED. ) ;
#51975 = EDGE_CURVE ( 'NONE', #46551, #25542, #50168, .T. ) ;
#51976 = FACE_OUTER_BOUND ( 'NONE', #5844, .T. ) ;
#51977 = VECTOR ( 'NONE', #1731, 1000.000000000000114 ) ;
#51978 = CARTESIAN_POINT ( 'NONE',  ( 10.12290050255000118, -60.04999997790999799, -7.648026768390999486 ) ) ;
#51979 = CARTESIAN_POINT ( 'NONE',  ( 12.50728321921977937, -61.79975184134804778, 0.1774118161309094777 ) ) ;
#51980 = CIRCLE ( 'NONE', #43499, 1.750000000000000000 ) ;
#51981 = CARTESIAN_POINT ( 'NONE',  ( 10.89560438185736579, -76.15405317179865108, -1.138875632008489180 ) ) ;
#51982 = CARTESIAN_POINT ( 'NONE',  ( 10.75008527255733881, -78.36041959662934175, 1.407065630674559698 ) ) ;
#51983 = CARTESIAN_POINT ( 'NONE',  ( 12.70249541833965345, -53.83496187159536817, -0.9988462570306496646 ) ) ;
#51984 = EDGE_LOOP ( 'NONE', ( #307, #54148, #47572, #31401 ) ) ;
#51985 = ADVANCED_FACE ( 'NONE', ( #37070 ), #51105, .T. ) ;
#51986 = EDGE_LOOP ( 'NONE', ( #39813, #40865, #9052, #54675 ) ) ;
#51987 = CARTESIAN_POINT ( 'NONE',  ( 4.364318959196999970, -76.91231541335099564, -11.68200350210999972 ) ) ;
#51988 = CARTESIAN_POINT ( 'NONE',  ( 5.563604409980168697, -78.76841996384091260, -9.198609774334910227 ) ) ;
#51989 = EDGE_LOOP ( 'NONE', ( #13617, #46555 ) ) ;
#51990 = CARTESIAN_POINT ( 'NONE',  ( 10.18127254044999930, -18.61355771719999908, 7.633407132383000615 ) ) ;
#51991 = CARTESIAN_POINT ( 'NONE',  ( -5.539808784079931492, -77.61666666666667425, 9.611650271896815312 ) ) ;
#51992 = CARTESIAN_POINT ( 'NONE',  ( 0.1380878923454642859, -53.57265597645798749, 12.70555840928343017 ) ) ;
#51993 = CARTESIAN_POINT ( 'NONE',  ( -3.220107333416999840, -77.56377916175999587, 12.38709272308999942 ) ) ;
#51994 = DIRECTION ( 'NONE',  ( 0.7071067811865475727, 0.000000000000000000, 0.7071067811865475727 ) ) ;
#51995 = CARTESIAN_POINT ( 'NONE',  ( -1.499999999971000086, -77.75000000002998490, -1.761798912373000190E-09 ) ) ;
#51996 = DIRECTION ( 'NONE',  ( 0.000000000000000000, 0.000000000000000000, -1.000000000000000000 ) ) ;
#51997 = CARTESIAN_POINT ( 'NONE',  ( -2.848564863371000122, -78.93846150521399352, -10.84913769893999991 ) ) ;
#51998 = ORIENTED_EDGE ( 'NONE', *, *, #44777, .F. ) ;
#51999 = DIRECTION ( 'NONE',  ( 0.7071067811865474617, -0.7071067811865474617, -1.236215424745081016E-09 ) ) ;
#52000 =( GEOMETRIC_REPRESENTATION_CONTEXT ( 3 ) GLOBAL_UNCERTAINTY_ASSIGNED_CONTEXT ( ( #11845 ) ) GLOBAL_UNIT_ASSIGNED_CONTEXT ( ( #2180, #46186, #1027 ) ) REPRESENTATION_CONTEXT ( 'NONE', 'WORKASPACE' ) );
#52001 = ORIENTED_EDGE ( 'NONE', *, *, #39474, .F. ) ;
#52002 = CARTESIAN_POINT ( 'NONE',  ( 5.510598863588248797, -77.27593132977736445, -7.429347641380793732 ) ) ;
#52003 = CARTESIAN_POINT ( 'NONE',  ( -3.203604947276999848, -77.88888306514598980, 10.56508708803000118 ) ) ;
#52004 = CARTESIAN_POINT ( 'NONE',  ( -11.87500000004000000, -79.12500000004000356, -1.061343742159000057E-08 ) ) ;
#52005 = CARTESIAN_POINT ( 'NONE',  ( -5.751514107123901987, -77.93206505849833832, -9.630248929252696044 ) ) ;
#52006 = UNCERTAINTY_MEASURE_WITH_UNIT (LENGTH_MEASURE( 1.000000000000000082E-05 ), #38750, 'distance_accuracy_value', 'NONE');
#52007 = CARTESIAN_POINT ( 'NONE',  ( -1.183003490338000008, -79.14322140577399978, -0.6653023415106000815 ) ) ;
#52008 = CARTESIAN_POINT ( 'NONE',  ( -8.414570695956999913, -59.94999999967000548, 8.414570695956999913 ) ) ;
#52009 = CARTESIAN_POINT ( 'NONE',  ( -1.407171709420465211, -80.88541666666667140, 10.74999999999999467 ) ) ;
#52010 = CARTESIAN_POINT ( 'NONE',  ( 1.621809933883000099, -78.64546402086999421, 0.1356303529659999840 ) ) ;
#52011 = CARTESIAN_POINT ( 'NONE',  ( -7.627487525417000036, -18.70221245812999911, 10.35845608625999859 ) ) ;
#52012 = CARTESIAN_POINT ( 'NONE',  ( 9.696433660856000003, -79.28284900987598860, 5.296892287724999981 ) ) ;
#52013 = CARTESIAN_POINT ( 'NONE',  ( -3.206516299415000049, -2.013032031398999777, -0.5298615117031000299 ) ) ;
#52014 = CARTESIAN_POINT ( 'NONE',  ( 2.952107475776000189, -82.34482020574199623, -1.687956242112000016 ) ) ;
#52015 = ORIENTED_EDGE ( 'NONE', *, *, #14507, .T. ) ;
#52016 = CARTESIAN_POINT ( 'NONE',  ( -0.8956573524961000121, -81.41095650773000614, -1.447939571232000011 ) ) ;
#52017 = AXIS2_PLACEMENT_3D ( 'NONE', #21423, #16999, #39712 ) ;
#52018 = CARTESIAN_POINT ( 'NONE',  ( 0.3786699527928999442, -79.97286976367999500, -1.660248773968999947 ) ) ;
#52019 = FACE_OUTER_BOUND ( 'NONE', #5337, .T. ) ;
#52020 = CARTESIAN_POINT ( 'NONE',  ( -10.26943924278000075, -78.45527103163399829, 6.168847710360999770 ) ) ;
#52021 = CARTESIAN_POINT ( 'NONE',  ( -9.310166272083998606, -16.86468533975999762, 8.596757084891999412 ) ) ;
#52022 = ADVANCED_FACE ( 'NONE', ( #33217 ), #46550, .T. ) ;
#52023 = VECTOR ( 'NONE', #38020, 1000.000000000000000 ) ;
#52024 = CARTESIAN_POINT ( 'NONE',  ( 8.098718378555803454, -78.90743983794655492, 7.103735875983660186 ) ) ;
#52025 = CARTESIAN_POINT ( 'NONE',  ( -2.930423846477897776, -2.296787813417054736, -1.954655114040125374 ) ) ;
#52026 = DIRECTION ( 'NONE',  ( -8.742284675758000260E-11, -1.000000000000000000, -2.562965951460999736E-09 ) ) ;
#52027 = CARTESIAN_POINT ( 'NONE',  ( 9.191740907676001271, -78.87203893003398036, -2.486449962426000138 ) ) ;
#52028 = CARTESIAN_POINT ( 'NONE',  ( 1.576170184336000091, -54.63913032751000287, -12.55466896101999907 ) ) ;
#52029 = CARTESIAN_POINT ( 'NONE',  ( -4.457153411444000568, -77.55076617252800020, -10.09135857296999994 ) ) ;
#52030 = CARTESIAN_POINT ( 'NONE',  ( -10.88526732619999926, -81.03202613352289063, -0.7446763694950000456 ) ) ;
#52031 = CARTESIAN_POINT ( 'NONE',  ( 0.9577060863230739685, -80.95750822540561842, 0.8401837386943417085 ) ) ;
#52032 = ORIENTED_EDGE ( 'NONE', *, *, #15765, .F. ) ;
#52033 = CARTESIAN_POINT ( 'NONE',  ( -9.009247259181927703, -78.97916666666665719, 2.421167930323307793 ) ) ;
#52034 = CARTESIAN_POINT ( 'NONE',  ( -1.758095523364999968, -60.52291663846999370, -12.57362173518999882 ) ) ;
#52035 = CARTESIAN_POINT ( 'NONE',  ( -4.006190475301194098, -78.54828561723799396, -2.263637441416614493 ) ) ;
#52036 = CARTESIAN_POINT ( 'NONE',  ( -8.649885944100999424, -77.82102619471399407, -7.141259254888000285 ) ) ;
#52037 = CARTESIAN_POINT ( 'NONE',  ( 9.632126701410999914, -79.15963541743298038, 5.261763182588000021 ) ) ;
#52038 = FACE_OUTER_BOUND ( 'NONE', #20666, .T. ) ;
#52039 = CARTESIAN_POINT ( 'NONE',  ( 2.343872625036407698, -85.67604168173227208, 3.257443233898490664 ) ) ;
#52040 = LINE ( 'NONE', #29858, #57179 ) ;
#52041 = CARTESIAN_POINT ( 'NONE',  ( 0.000000000000000000, -74.64999999999999147, 0.000000000000000000 ) ) ;
#52042 = LINE ( 'NONE', #34581, #12599 ) ;
#52043 = ORIENTED_EDGE ( 'NONE', *, *, #15325, .T. ) ;
#52044 = CARTESIAN_POINT ( 'NONE',  ( -0.3763322838831557604, -79.99938371673916038, 1.195031458938746738 ) ) ;
#52045 = CARTESIAN_POINT ( 'NONE',  ( -1.838192502620780822, -75.79999999999998295, -11.63589874194363816 ) ) ;
#52046 = SHAPE_REPRESENTATION ( 'Spring', ( #43526 ), #13324 ) ;
#52047 = CARTESIAN_POINT ( 'NONE',  ( -3.770495512267000304, -79.08134268642398013, 10.61660482251999937 ) ) ;
#52048 = EDGE_CURVE ( 'NONE', #3338, #22170, #6368, .T. ) ;
#52049 = CARTESIAN_POINT ( 'NONE',  ( 9.596002108778172612, -76.99791666666666856, -7.374560639698962028 ) ) ;
#52050 = LINE ( 'NONE', #39034, #55635 ) ;
#52051 = DIRECTION ( 'NONE',  ( 0.000000000000000000, -1.000000000000000000, 0.000000000000000000 ) ) ;
#52052 = CARTESIAN_POINT ( 'NONE',  ( 1.491775814946131984, -83.08621709869576932, -0.2501303660045399169 ) ) ;
#52053 = CARTESIAN_POINT ( 'NONE',  ( 0.4182184111412154404, -79.75227781930720994, -1.179636507925768907 ) ) ;
#52054 = CARTESIAN_POINT ( 'NONE',  ( -7.635226873531286707, -55.03391307102463514, 10.36745167320620808 ) ) ;
#52055 = ORIENTED_EDGE ( 'NONE', *, *, #38636, .F. ) ;
#52056 = CARTESIAN_POINT ( 'NONE',  ( 1.930989179114000143, -20.24546192895000019, 12.80896991329000123 ) ) ;
#52057 =( LENGTH_UNIT ( ) NAMED_UNIT ( * ) SI_UNIT ( .MILLI., .METRE. ) );
#52058 = CARTESIAN_POINT ( 'NONE',  ( 3.075537641221509411, -76.15416666666668277, 11.44417895085272008 ) ) ;
#52059 = VERTEX_POINT ( 'NONE', #6076 ) ;
#52060 = EDGE_CURVE ( 'NONE', #52807, #4267, #26158, .T. ) ;
#52061 = ORIENTED_EDGE ( 'NONE', *, *, #14664, .F. ) ;
#52062 = CARTESIAN_POINT ( 'NONE',  ( -12.55458938217999965, -54.63720883353000346, -1.575070636625000242 ) ) ;
#52063 = VECTOR ( 'NONE', #5436, 1000.000000000000000 ) ;
#52064 = ORIENTED_EDGE ( 'NONE', *, *, #3816, .F. ) ;
#52065 = ORIENTED_EDGE ( 'NONE', *, *, #36471, .T. ) ;
#52066 = CARTESIAN_POINT ( 'NONE',  ( 10.53494356938999843, -23.22715052988000295, 7.618393677165000710 ) ) ;
#52067 = CARTESIAN_POINT ( 'NONE',  ( 4.161322419204999790, -76.72953055567299430, -10.09251018087000062 ) ) ;
#52068 = CARTESIAN_POINT ( 'NONE',  ( -0.7554284705563480973, -78.08333333333334281, -1.310679582531387277 ) ) ;
#52069 = CARTESIAN_POINT ( 'NONE',  ( 1.914689014128999833, -78.55246332859900349, 9.610012265935001352 ) ) ;
#52070 = CARTESIAN_POINT ( 'NONE',  ( -2.195394413746336593, -78.20598208360085835, -8.990872906390226404 ) ) ;
#52071 = FACE_OUTER_BOUND ( 'NONE', #45480, .T. ) ;
#52072 = ORIENTED_EDGE ( 'NONE', *, *, #44758, .T. ) ;
#52073 = ORIENTED_EDGE ( 'NONE', *, *, #23431, .T. ) ;
#52074 = CARTESIAN_POINT ( 'NONE',  ( -5.331231741419041548, -77.52388645747066676, 7.560242739789973854 ) ) ;
#52075 = CARTESIAN_POINT ( 'NONE',  ( -12.70255466318980631, -24.74616562079560467, 1.306323829446151885 ) ) ;
#52076 = CYLINDRICAL_SURFACE ( 'NONE', #7843, 12.00000000000000000 ) ;
#52077 = CARTESIAN_POINT ( 'NONE',  ( -9.626984307556000431, -78.32010870590698914, 1.221426423741999834 ) ) ;
#52078 = CIRCLE ( 'NONE', #11534, 12.57042253521000141 ) ;
#52079 = CARTESIAN_POINT ( 'NONE',  ( 7.641012305222999679, -23.28917723430000208, 10.18589226631999978 ) ) ;
#52080 = CARTESIAN_POINT ( 'NONE',  ( 1.500000000000000000, -79.25000000000000000, 0.000000000000000000 ) ) ;
#52081 = CARTESIAN_POINT ( 'NONE',  ( -0.3271848554491046945, -79.89583333333330017, 1.217465845835393301 ) ) ;
#52082 = DIRECTION ( 'NONE',  ( 0.000000000000000000, 0.000000000000000000, -1.000000000000000000 ) ) ;
#52083 = CARTESIAN_POINT ( 'NONE',  ( 1.449190734180999973, -79.97597904509999012, -0.8942388842271000726 ) ) ;
#52084 = FACE_OUTER_BOUND ( 'NONE', #36349, .T. ) ;
#52085 = CARTESIAN_POINT ( 'NONE',  ( -10.15323015671000029, -54.56919784871999468, 7.760928569184999404 ) ) ;
#52086 = CARTESIAN_POINT ( 'NONE',  ( 7.981661899572999985, -77.80008667140099021, 4.815606314103999530 ) ) ;
#52087 = DIRECTION ( 'NONE',  ( -1.000000000000000000, 0.000000000000000000, 0.000000000000000000 ) ) ;
#52088 = CARTESIAN_POINT ( 'NONE',  ( 1.667916687331000070, -18.70151115557999688, -12.49168451098999988 ) ) ;
#52089 = EDGE_CURVE ( 'NONE', #13029, #44413, #10815, .T. ) ;
#52091 = CARTESIAN_POINT ( 'NONE',  ( 1.667260628941999778, -18.79057987526000062, -12.49858003894999925 ) ) ;
#52090 = DIRECTION ( 'NONE',  ( -1.000000000000000000, 0.000000000000000000, 0.000000000000000000 ) ) ;
#52092 = CARTESIAN_POINT ( 'NONE',  ( 9.250000000000000000, -79.34999999999999432, 0.000000000000000000 ) ) ;
#52093 = CARTESIAN_POINT ( 'NONE',  ( 4.491149118889000036, -80.08742432477399120, -10.11991891289999934 ) ) ;
#52094 = CARTESIAN_POINT ( 'NONE',  ( 12.76303204522000101, -23.26485147686999966, 1.980584515753000208 ) ) ;
#52095 = CARTESIAN_POINT ( 'NONE',  ( 1.068619641472000170, -1.999647048965999874, -3.652926003266999899 ) ) ;
#52096 = CARTESIAN_POINT ( 'NONE',  ( -1.137713819132262438, -1.150991845674092851, 3.439702573946882946 ) ) ;
#52097 = EDGE_CURVE ( 'NONE', #12955, #46203, #24384, .T. ) ;
#52098 = ORIENTED_EDGE ( 'NONE', *, *, #38137, .T. ) ;
#52099 = CARTESIAN_POINT ( 'NONE',  ( -2.843405644759636086, -1.560134993415584370, 1.636542488881060464 ) ) ;
#52100 = CARTESIAN_POINT ( 'NONE',  ( 7.685661446562000343, -79.50000000000000000, -5.583959896778000420 ) ) ;
#52101 = CARTESIAN_POINT ( 'NONE',  ( 1.133628739905723437, -78.38499154607053754, 0.5281210143588952466 ) ) ;
#52102 = CARTESIAN_POINT ( 'NONE',  ( -8.544252929325999446, -79.92036243689798880, 4.229201381545000693 ) ) ;
#52103 = AXIS2_PLACEMENT_3D ( 'NONE', #20415, #10987, #28968 ) ;
#52104 = CARTESIAN_POINT ( 'NONE',  ( -1.407080327196711611, -76.98557767287246634, 10.75010754519202294 ) ) ;
#52105 = FACE_OUTER_BOUND ( 'NONE', #10589, .T. ) ;
#52106 = CARTESIAN_POINT ( 'NONE',  ( -11.70000000000000107, -79.79999999999999716, 0.000000000000000000 ) ) ;
#52107 = CYLINDRICAL_SURFACE ( 'NONE', #54008, 11.00000000000000000 ) ;
#52108 = PLANE ( 'NONE',  #42354 ) ;
#52109 = FACE_BOUND ( 'NONE', #49926, .T. ) ;
#52110 = CARTESIAN_POINT ( 'NONE',  ( 4.742897571346999186, -78.03146995713699141, -9.867095245577001350 ) ) ;
#52111 = CARTESIAN_POINT ( 'NONE',  ( 8.858913794315254719, -76.39276943178882107, -7.721635716659831061 ) ) ;
#52112 = CARTESIAN_POINT ( 'NONE',  ( -10.47919054151000040, -77.73654766055700804, -3.800153439748000128 ) ) ;
#52113 = CARTESIAN_POINT ( 'NONE',  ( -7.401612602209000968, -79.20614514476065438, -6.305503003149000030 ) ) ;
#52114 = CARTESIAN_POINT ( 'NONE',  ( 0.4422131289978999957, -78.97643549037999833, -1.603741477255999914 ) ) ;
#52115 = CARTESIAN_POINT ( 'NONE',  ( -9.429275737370000243, -77.33986768295099523, -1.157047565421999824 ) ) ;
#52116 = CARTESIAN_POINT ( 'NONE',  ( 0.9218200799623694763, -78.82291666666668561, 1.199500263597272465 ) ) ;
#52117 = CARTESIAN_POINT ( 'NONE',  ( 0.5999999999999999778, -5.000000000000000000, 4.000000000000000000 ) ) ;
#52118 = CARTESIAN_POINT ( 'NONE',  ( 0.3926218265389159190, -81.35416666666667140, 1.460959015002474715 ) ) ;
#52119 = DIRECTION ( 'NONE',  ( 0.000000000000000000, -1.000000000000000000, -1.378526922243000102E-14 ) ) ;
#52120 = CARTESIAN_POINT ( 'NONE',  ( -1.135826688880000157, -81.30663953507000485, -0.9797437077257000748 ) ) ;
#52121 = CIRCLE ( 'NONE', #37011, 1.500000000000000000 ) ;
#52122 = AXIS2_PLACEMENT_3D ( 'NONE', #16790, #11505, #25063 ) ;
#52123 = CARTESIAN_POINT ( 'NONE',  ( -12.02912753549999891, -79.49775441913300256, 0.08506824670321999626 ) ) ;
#52124 = CARTESIAN_POINT ( 'NONE',  ( 4.784380313523521444, -78.63333333333332575, 8.300970689365463784 ) ) ;
#52125 = CARTESIAN_POINT ( 'NONE',  ( 3.385018580295000135, -79.47270349199298778, -10.74130410002999980 ) ) ;
#52126 = ORIENTED_EDGE ( 'NONE', *, *, #26694, .T. ) ;
#52127 = ADVANCED_FACE ( 'NONE', ( #33517 ), #30813, .T. ) ;
#52128 = CARTESIAN_POINT ( 'NONE',  ( 1.930860503532993544, -23.77417505915895291, 12.72930866331734734 ) ) ;
#52129 = ADVANCED_FACE ( 'NONE', ( #56839 ), #120, .T. ) ;
#52130 = ORIENTED_EDGE ( 'NONE', *, *, #47082, .T. ) ;
#52131 = EDGE_LOOP ( 'NONE', ( #50828, #4107 ) ) ;
#52132 = CARTESIAN_POINT ( 'NONE',  ( 0.000000000000000000, -75.15999999999999659, 0.000000000000000000 ) ) ;
#52133 = VERTEX_POINT ( 'NONE', #30530 ) ;
#52134 = CARTESIAN_POINT ( 'NONE',  ( -3.276755629569999773, -78.81431117999389357, 1.049729901832000101 ) ) ;
#52135 = CARTESIAN_POINT ( 'NONE',  ( 4.159563559845795844, -79.23853427882175993, 8.541212464559901463 ) ) ;
#52136 = ORIENTED_EDGE ( 'NONE', *, *, #48250, .F. ) ;
#52137 = CARTESIAN_POINT ( 'NONE',  ( 0.2456986548642498824, -82.74120455909647376, -1.225335228240030050 ) ) ;
#52138 = CARTESIAN_POINT ( 'NONE',  ( -7.641012305206999145, -55.51082276539999327, 10.18589226629999978 ) ) ;
#52139 = ORIENTED_EDGE ( 'NONE', *, *, #6029, .F. ) ;
#52140 = CARTESIAN_POINT ( 'NONE',  ( -0.8256138858706347783, -79.53279254742548687, 0.9417001439504392168 ) ) ;
#52141 = CARTESIAN_POINT ( 'NONE',  ( 0.6432483788054168539, -78.59024951571676354, 1.390064027832063731 ) ) ;
#52142 = CIRCLE ( 'NONE', #26649, 0.5000000000000001110 ) ;
#52143 = DIRECTION ( 'NONE',  ( -0.7071067811865474617, 0.000000000000000000, -0.7071067811865474617 ) ) ;
#52144 = CARTESIAN_POINT ( 'NONE',  ( -6.907231294620150841, -80.03091450954583763, 8.236999994290794547 ) ) ;
#52145 = CYLINDRICAL_SURFACE ( 'NONE', #24903, 14.00000000000000000 ) ;
#52146 = EDGE_CURVE ( 'NONE', #22854, #2820, #49222, .T. ) ;
#52147 = CARTESIAN_POINT ( 'NONE',  ( 3.380118192975939184, -86.40321104920799655, -1.504925579246137568 ) ) ;
#52148 = CARTESIAN_POINT ( 'NONE',  ( 8.154961773732001262, -76.14386894535999772, 7.653135223926000208 ) ) ;
#52149 = CARTESIAN_POINT ( 'NONE',  ( 0.000000000000000000, -76.75499999999999545, 0.000000000000000000 ) ) ;
#52150 = CARTESIAN_POINT ( 'NONE',  ( 1.439896632895284911, -78.56458333333330302, 11.00000000000000355 ) ) ;
#52151 = VECTOR ( 'NONE', #49811, 1000.000000000000114 ) ;
#52152 = CARTESIAN_POINT ( 'NONE',  ( -1.633132813051000110, -76.84572286667699359, 10.87725817015999930 ) ) ;
#52153 = CARTESIAN_POINT ( 'NONE',  ( -5.137582680770506727, -78.67826736333080362, -7.691962846148583388 ) ) ;
#52154 = CARTESIAN_POINT ( 'NONE',  ( 1.722150539371000155, -77.64636167140099587, -9.363010803921000047 ) ) ;
#52155 = CARTESIAN_POINT ( 'NONE',  ( -1.327128730425999992, -79.67025063774299554, 0.1315503032697999675 ) ) ;
#52156 = CARTESIAN_POINT ( 'NONE',  ( -9.722718241315000398, -18.55321828668999729, -7.954951288349001004 ) ) ;
#52157 = DIRECTION ( 'NONE',  ( 1.000000000000000000, 0.000000000000000000, 0.000000000000000000 ) ) ;
#52158 = CARTESIAN_POINT ( 'NONE',  ( -3.613802140370000249, -78.36136788790179253, 0.5226175732511999517 ) ) ;
#52159 = AXIS2_PLACEMENT_3D ( 'NONE', #5468, #22894, #46523 ) ;
#52160 = CARTESIAN_POINT ( 'NONE',  ( -10.19309198600624811, -78.07437978168276516, 3.419625436452577549 ) ) ;
#52161 = DIRECTION ( 'NONE',  ( 0.000000000000000000, -1.000000000000000000, 0.000000000000000000 ) ) ;
#52162 = CARTESIAN_POINT ( 'NONE',  ( 0.000000000000000000, -52.49705297114005020, 12.53545825868000207 ) ) ;
#52163 = CARTESIAN_POINT ( 'NONE',  ( 3.130966520949999943, -82.62299735065199968, 1.661977487544999965 ) ) ;
#52164 = CARTESIAN_POINT ( 'NONE',  ( 0.7681833999686413783, -80.32291666666668561, 0.9995835529977274980 ) ) ;
#52165 = CARTESIAN_POINT ( 'NONE',  ( 6.233047529871999615, -78.88050366622999832, 9.960502923565000444 ) ) ;
#52166 = ADVANCED_FACE ( 'NONE', ( #34380 ), #35814, .F. ) ;
#52167 = CIRCLE ( 'NONE', #29507, 1.750000000000000000 ) ;
#52168 = CARTESIAN_POINT ( 'NONE',  ( 2.813789756862240754, -80.14583333333330017, -10.47020627418439886 ) ) ;
#52169 = DIRECTION ( 'NONE',  ( 0.000000000000000000, -1.000000000000000000, 0.000000000000000000 ) ) ;
#52170 = CARTESIAN_POINT ( 'NONE',  ( 10.53003236235000095, -60.12452273675999947, 7.612971540294999784 ) ) ;
#52171 = CARTESIAN_POINT ( 'NONE',  ( 0.9218200799623741393, -80.57708333333334849, -1.199500263597268690 ) ) ;
#52172 = CARTESIAN_POINT ( 'NONE',  ( 12.83838776459000108, -23.20596988487999823, 2.062170466181000528 ) ) ;
#52173 = CARTESIAN_POINT ( 'NONE',  ( 11.15501740173857037, -78.42093623943294745, -3.786043910604230955 ) ) ;
#52174 = CARTESIAN_POINT ( 'NONE',  ( 1.733997378023099056, -23.52383216769529639, -12.54437956612015626 ) ) ;
#52175 = CARTESIAN_POINT ( 'NONE',  ( 11.12361694604000029, -76.79944983679999382, -4.717657731420999312 ) ) ;
#52176 = ORIENTED_EDGE ( 'NONE', *, *, #34552, .T. ) ;
#52177 = DIRECTION ( 'NONE',  ( 0.000000000000000000, 1.000000000000000000, 0.000000000000000000 ) ) ;
#52178 = CARTESIAN_POINT ( 'NONE',  ( 0.000000000000000000, 4.040000000000000036, 0.000000000000000000 ) ) ;
#52179 = CARTESIAN_POINT ( 'NONE',  ( 0.9961526269716999282, -81.04823719390898873, 0.8517633278984999556 ) ) ;
#52180 = CARTESIAN_POINT ( 'NONE',  ( -12.47891010869000006, -78.75756776420000449, -0.3053857658451999968 ) ) ;
#52181 = FACE_OUTER_BOUND ( 'NONE', #1160, .T. ) ;
#52182 = CARTESIAN_POINT ( 'NONE',  ( -3.509962959857999554, -78.29774788529299201, 8.968465308258000590 ) ) ;
#52183 = CARTESIAN_POINT ( 'NONE',  ( 4.171885727129999388, -85.47133100267899408, 0.04387387242050999614 ) ) ;
#52184 = CARTESIAN_POINT ( 'NONE',  ( -1.620259408620695396, -79.98748962049585032, 10.62691779879149401 ) ) ;
#52185 = CARTESIAN_POINT ( 'NONE',  ( 1.130428667122000075, -80.17865684227599843, -1.152972209120999958 ) ) ;
#52186 = EDGE_LOOP ( 'NONE', ( #5148, #39588, #42553, #21535, #33443, #58131 ) ) ;
#52187 = CARTESIAN_POINT ( 'NONE',  ( 9.549999999953000085, -76.40000000004698677, -5.125981083096999748E-10 ) ) ;
#52188 = CARTESIAN_POINT ( 'NONE',  ( 2.332848451437957937, -78.97236559110959320, -2.708295505596481689 ) ) ;
#52189 = EDGE_LOOP ( 'NONE', ( #52344, #43275, #53580, #43481 ) ) ;
#52190 = CARTESIAN_POINT ( 'NONE',  ( -8.603527126503999867, -78.31782986146299663, 6.757746467621000619 ) ) ;
#52191 = AXIS2_PLACEMENT_3D ( 'NONE', #55709, #6104, #45402 ) ;
#52192 = FILL_AREA_STYLE ('',( #34153 ) ) ;
#52193 = CARTESIAN_POINT ( 'NONE',  ( -11.16546426881000009, -79.79336997964799139, 1.922701916112000031 ) ) ;
#52194 = VERTEX_POINT ( 'NONE', #14749 ) ;
#52195 = CARTESIAN_POINT ( 'NONE',  ( 11.60231809276000092, -78.91938348357999189, -3.252995651540999678 ) ) ;
#52196 = EDGE_LOOP ( 'NONE', ( #8571, #43734, #29576, #34582 ) ) ;
#52197 = VERTEX_POINT ( 'NONE', #29488 ) ;
#52198 = CARTESIAN_POINT ( 'NONE',  ( -0.1244589946783580814, -80.48333614422827509, 1.244172789713544613 ) ) ;
#52199 = CONICAL_SURFACE ( 'NONE', #19079, 5.199999999809000073, 0.7853981633972997312 ) ;
#52200 = CARTESIAN_POINT ( 'NONE',  ( 1.405334851866475443, -61.11492947527372621, 12.50716844841787356 ) ) ;
#52201 = CARTESIAN_POINT ( 'NONE',  ( 6.653382217586999658, -79.94552603410404856, 7.150748904218000135 ) ) ;
#52202 = VERTEX_POINT ( 'NONE', #41925 ) ;
#52203 = CARTESIAN_POINT ( 'NONE',  ( 2.597747286150731583, -2.403326232176795862, 1.995542179488032808 ) ) ;
#52204 = ORIENTED_EDGE ( 'NONE', *, *, #16396, .T. ) ;
#52205 = CARTESIAN_POINT ( 'NONE',  ( -11.38660623898999980, -79.08028002244630272, -4.554589311945999697 ) ) ;
#52206 = CARTESIAN_POINT ( 'NONE',  ( 4.897371265365999982, -76.90054805011499184, 7.847181321287999722 ) ) ;
#52207 = CARTESIAN_POINT ( 'NONE',  ( 9.395773752806999113, -54.09509747810999869, 8.188237371196001035 ) ) ;
#52208 = ADVANCED_FACE ( 'NONE', ( #23616 ), #17920, .F. ) ;
#52209 = CARTESIAN_POINT ( 'NONE',  ( 8.792808668242045655, -16.77303577624769559, -9.175550543643495871 ) ) ;
#52210 = CARTESIAN_POINT ( 'NONE',  ( -0.1963495408493673156, -78.28541666666667709, 1.499999999999999556 ) ) ;
#52211 = CARTESIAN_POINT ( 'NONE',  ( 5.896171905175000560, -77.96999999999999886, 7.127247495676000355 ) ) ;
#52212 = CARTESIAN_POINT ( 'NONE',  ( 6.586108526242999694, -80.17391735373439587, 8.810401493720998900 ) ) ;
#52213 = CYLINDRICAL_SURFACE ( 'NONE', #52636, 1.750000000000001332 ) ;
#52214 = CARTESIAN_POINT ( 'NONE',  ( 3.281285156496776878, -82.30364585245855835, -2.308832152369716173 ) ) ;
#52215 = CARTESIAN_POINT ( 'NONE',  ( 7.568503529865000523, -76.27030647614999737, 9.708412483427999007 ) ) ;
#52216 = FACE_OUTER_BOUND ( 'NONE', #19664, .T. ) ;
#52217 = CARTESIAN_POINT ( 'NONE',  ( -7.471200359486886988, -79.35399621689622052, -5.924110288814695480 ) ) ;
#52218 = DIRECTION ( 'NONE',  ( 0.000000000000000000, 0.000000000000000000, 1.000000000000000000 ) ) ;
#52219 = CARTESIAN_POINT ( 'NONE',  ( 10.35410175341000105, -60.20399325318000194, -7.619715687221999545 ) ) ;
#52220 = CARTESIAN_POINT ( 'NONE',  ( 7.081057523560999378, -79.15664967202000923, -10.01287680343000019 ) ) ;
#52221 = CARTESIAN_POINT ( 'NONE',  ( 3.654181830570000233, -86.09999999999999432, -1.626946572303000105 ) ) ;
#52222 = CARTESIAN_POINT ( 'NONE',  ( -9.500000000000000000, -78.89999999999999147, 0.000000000000000000 ) ) ;
#52223 = EDGE_CURVE ( 'NONE', #3961, #31318, #49556, .T. ) ;
#52224 = B_SPLINE_CURVE_WITH_KNOTS ( 'NONE', 3,
 ( #14753, #32752, #62, #50800, #44903, #27163, #40470, #49927, #13592, #9179, #45202, #40761, #355, #18333, #31884, #5040, #36326, #54350, #41056, #13890, #9472, #36618, #54639, #42805, #46377, #2084, #10937, #15932, #7072, #47251, #6782, #25075, #24790, #6196, #2367 ),
 .UNSPECIFIED., .F., .F.,
 ( 4, 1, 1, 1, 1, 1, 1, 1, 1, 1, 1, 1, 1, 1, 1, 1, 1, 1, 1, 1, 1, 1, 1, 1, 1, 1, 1, 1, 1, 1, 1, 1, 4 ),
 ( 0.000000000000000000, 0.01250092184359906378, 0.04500086039013131284, 0.07750079893666367292, 0.1100007374831958179, 0.1425006760297282682, 0.1750006145762605103, 0.2075005531227929745, 0.2400004916693252166, 0.2725004302158574587, 0.3050003687623897286, 0.3375003073089221650, 0.3700002458554544349, 0.4025001844019868713, 0.4350001229485191412, 0.4675000614950513556, 0.5000000000415836254, 0.5324999385881158398, 0.5649998771346483872, 0.5974998156811806016, 0.6299997542277130380, 0.6624996927742452524, 0.6949996313207776888, 0.7274995698673097921, 0.7599995084138420065, 0.7924994469603744429, 0.8249993855069067683, 0.8574993240534392047, 0.8899992625999714191, 0.9224992011465038555, 0.9549991396930359588, 0.9874990782395683953, 1.000000000000000000 ),
 .UNSPECIFIED. ) ;
#52225 = CARTESIAN_POINT ( 'NONE',  ( 0.000000000000000000, -82.25000000001401190, 0.000000000000000000 ) ) ;
#52226 = CARTESIAN_POINT ( 'NONE',  ( 0.4626184419780025592, -79.89972753181358200, -1.439301428628166679 ) ) ;
#52227 = CARTESIAN_POINT ( 'NONE',  ( -6.105583392804999399, -77.45220173038597977, 7.123643952372000321 ) ) ;
#52228 = DIRECTION ( 'NONE',  ( 1.000000000000000000, 0.000000000000000000, 0.000000000000000000 ) ) ;
#52229 = CARTESIAN_POINT ( 'NONE',  ( 1.532229594834795705, -24.12298963131433638, 12.51228690880953387 ) ) ;
#52230 = CARTESIAN_POINT ( 'NONE',  ( -1.647164036128999864, -2.055236014850999826, -3.153578910874000218 ) ) ;
#52231 = CARTESIAN_POINT ( 'NONE',  ( 10.33787006668000075, -78.23531443679999597, 6.411783922571999916 ) ) ;
#52232 = CARTESIAN_POINT ( 'NONE',  ( 9.292856425461000214, -78.54500914553598534, 2.915907262279999745 ) ) ;
#52233 = EDGE_CURVE ( 'NONE', #13108, #35472, #41679, .T. ) ;
#52235 = CARTESIAN_POINT ( 'NONE',  ( 1.310116429410000061, -79.00133983115898673, 0.1554359553024000085 ) ) ;
#52234 = CARTESIAN_POINT ( 'NONE',  ( -11.52085783181860812, -76.18387217134889511, 2.307947444626160305 ) ) ;
#52236 = CARTESIAN_POINT ( 'NONE',  ( 0.4644997175289000135, -82.99273121958398747, 1.393065715888999856 ) ) ;
#52237 = DIRECTION ( 'NONE',  ( 0.000000000000000000, -1.000000000000000000, 0.000000000000000000 ) ) ;
#52238 = ORIENTED_EDGE ( 'NONE', *, *, #20894, .F. ) ;
#52239 = CARTESIAN_POINT ( 'NONE',  ( -10.18589226631999978, -18.71082276572999703, -7.641012305223999768 ) ) ;
#52240 = CARTESIAN_POINT ( 'NONE',  ( 1.151100648512999980, -79.05851746904299659, 11.98613337465000050 ) ) ;
#52241 = EDGE_CURVE ( 'NONE', #40940, #37542, #6665, .T. ) ;
#52242 = CARTESIAN_POINT ( 'NONE',  ( -1.053982531448302229, -79.36617011479219741, -9.467004606927948984 ) ) ;
#52243 = CARTESIAN_POINT ( 'NONE',  ( -2.194599507562917218, -80.00000000000001421, -9.198212786487998116 ) ) ;
#52244 = DIRECTION ( 'NONE',  ( 1.000000000000000000, 0.000000000000000000, 0.000000000000000000 ) ) ;
#52245 = FACE_OUTER_BOUND ( 'NONE', #51984, .T. ) ;
#52246 = CARTESIAN_POINT ( 'NONE',  ( -4.668381075099000022, -79.12153427173898024, 8.594720803921001462 ) ) ;
#52247 = CARTESIAN_POINT ( 'NONE',  ( 3.140974612311376646, -78.04583333333330586, -11.68767212001978706 ) ) ;
#52248 = CARTESIAN_POINT ( 'NONE',  ( 2.421167930323352646, -79.14583333333334281, -9.009247259181915268 ) ) ;
#52249 = ORIENTED_EDGE ( 'NONE', *, *, #47602, .T. ) ;
#52250 = CARTESIAN_POINT ( 'NONE',  ( -1.660550560716740121, -76.73674682975610040, 11.05987033582087165 ) ) ;
#52251 = CARTESIAN_POINT ( 'NONE',  ( -4.656159886366224576, -78.95671637029290935, 10.88172775970164707 ) ) ;
#52252 = CARTESIAN_POINT ( 'NONE',  ( -0.03204386105641582327, -78.67390000031814168, 3.399848995318665246 ) ) ;
#52253 = CARTESIAN_POINT ( 'NONE',  ( 0.4565975880176471602, -81.44548833070547289, 1.163485847307625942 ) ) ;
#52254 = CARTESIAN_POINT ( 'NONE',  ( 1.356773869401999955, -79.53033845299998461, -0.9668579442890000708 ) ) ;
#52255 = AXIS2_PLACEMENT_3D ( 'NONE', #57431, #48870, #25265 ) ;
#52256 = ORIENTED_EDGE ( 'NONE', *, *, #5956, .T. ) ;
#52257 = CARTESIAN_POINT ( 'NONE',  ( -0.9110512128634435935, -78.58818742932150769, 0.8906210113203995027 ) ) ;
#52258 = CARTESIAN_POINT ( 'NONE',  ( -7.880615083743071736, -76.99999999999998579, 4.906469375586612003 ) ) ;
#52259 = CARTESIAN_POINT ( 'NONE',  ( 1.667961430005999945, -58.54888345776999614, -12.58335110162999904 ) ) ;
#52260 = EDGE_CURVE ( 'NONE', #35193, #37266, #21731, .T. ) ;
#52261 = CARTESIAN_POINT ( 'NONE',  ( 8.899186938124000079, -76.04999999999999716, -6.465637775218000094 ) ) ;
#52262 = CARTESIAN_POINT ( 'NONE',  ( -1.250000000000000000, -78.50000000000000000, 0.000000000000000000 ) ) ;
#52263 = AXIS2_PLACEMENT_3D ( 'NONE', #54794, #14336, #28195 ) ;
#52264 = CARTESIAN_POINT ( 'NONE',  ( 9.767191983224998708, -79.45996625367898503, 0.05162932631433000269 ) ) ;
#52265 = ORIENTED_EDGE ( 'NONE', *, *, #30039, .T. ) ;
#52266 = ORIENTED_EDGE ( 'NONE', *, *, #11850, .F. ) ;
#52267 = CARTESIAN_POINT ( 'NONE',  ( 11.79063559949999984, -77.03526362826599438, 4.061698893270999200 ) ) ;
#52268 = APPLICATION_CONTEXT ( 'automotive_design' ) ;
#52269 = CARTESIAN_POINT ( 'NONE',  ( 3.187863135131073111, -78.74905765371072164, -10.27228247429871999 ) ) ;
#52270 = ORIENTED_EDGE ( 'NONE', *, *, #56196, .F. ) ;
#52271 = CARTESIAN_POINT ( 'NONE',  ( 7.636247231030999671, -18.23676232879999759, 10.30460520062000107 ) ) ;
#52272 = CARTESIAN_POINT ( 'NONE',  ( -2.935661446561999899, -79.50000000000000000, -9.035036904803998681 ) ) ;
#52273 = CARTESIAN_POINT ( 'NONE',  ( -9.396085398178614767, -75.85208333333332575, -7.220923959705254802 ) ) ;
#52274 = CARTESIAN_POINT ( 'NONE',  ( 5.488019371950999314, -76.92165190241000516, 11.73632836356999931 ) ) ;
#52275 = CARTESIAN_POINT ( 'NONE',  ( -1.500000000000000000, -78.00000000000000000, 0.000000000000000000 ) ) ;
#52276 = CYLINDRICAL_SURFACE ( 'NONE', #17337, 4.100000000000000533 ) ;
#52277 = CARTESIAN_POINT ( 'NONE',  ( 3.106054555984329113, -86.12609999968211127, -1.382904586457928353 ) ) ;
#52278 = CARTESIAN_POINT ( 'NONE',  ( -7.301194973305000779, -79.26529762123598744, 8.515319286630999684 ) ) ;
#52279 = CARTESIAN_POINT ( 'NONE',  ( -0.8787709177018370177, -79.98266234880088632, 9.208350210453216889 ) ) ;
#52280 = EDGE_LOOP ( 'NONE', ( #2182, #26030, #47130, #48776 ) ) ;
#52281 = CARTESIAN_POINT ( 'NONE',  ( -8.190859204290999784, -55.64999999967000122, 7.342331066867000544 ) ) ;
#52282 = ORIENTED_EDGE ( 'NONE', *, *, #57070, .T. ) ;
#52283 = CARTESIAN_POINT ( 'NONE',  ( -11.10294551207000069, -79.60724697177198550, 1.911422329490000127 ) ) ;
#52284 = CARTESIAN_POINT ( 'NONE',  ( 5.650948687534441461, -77.27745941166017474, -7.323274689015353722 ) ) ;
#52285 = CARTESIAN_POINT ( 'NONE',  ( 1.217465845835394855, -83.22916666666665719, -0.3271848554490981997 ) ) ;
#52286 = CARTESIAN_POINT ( 'NONE',  ( -10.05549647464921570, -78.31337386052332761, 4.970774552467315921 ) ) ;
#52287 = CARTESIAN_POINT ( 'NONE',  ( 1.384987510431000102, -77.86983073899280328, 0.3030985439221999811 ) ) ;
#52288 = CARTESIAN_POINT ( 'NONE',  ( 0.000000000000000000, -78.00000000000000000, 7.200000000000000178 ) ) ;
#52289 = DIRECTION ( 'NONE',  ( 0.000000000000000000, 1.000000000000000000, 0.000000000000000000 ) ) ;
#52290 = CARTESIAN_POINT ( 'NONE',  ( -1.560595261880000084, -77.80670572008999386, 0.4619550309703999713 ) ) ;
#52291 = CARTESIAN_POINT ( 'NONE',  ( -12.71658889741000031, -18.68415522710999710, -1.931087888049999979 ) ) ;
#52292 = CARTESIAN_POINT ( 'NONE',  ( -7.705142895586000407, -21.75083378359999742, 10.24998526315000014 ) ) ;
#52293 = CARTESIAN_POINT ( 'NONE',  ( -8.112440615085001028, -78.55244779722698922, -7.501079983178001065 ) ) ;
#52294 = ADVANCED_FACE ( 'NONE', ( #11161 ), #8967, .F. ) ;
#52295 = CARTESIAN_POINT ( 'NONE',  ( -10.06692847398348434, -23.70343452288557984, -7.655995225932134218 ) ) ;
#52296 = CARTESIAN_POINT ( 'NONE',  ( 0.000000000000000000, -78.59999999921299718, 0.000000000000000000 ) ) ;
#52297 = TOROIDAL_SURFACE ( 'NONE', #1403, 1.250000000000000000, 0.5000000000000000000 ) ;
#52298 = CARTESIAN_POINT ( 'NONE',  ( -3.453171399369999950, -1.863032031399000088, -0.5706200895263999762 ) ) ;
#52299 = DIRECTION ( 'NONE',  ( 1.000000000000000000, 0.000000000000000000, 0.000000000000000000 ) ) ;
#52300 = VERTEX_POINT ( 'NONE', #27608 ) ;
#52301 = EDGE_CURVE ( 'NONE', #15146, #34611, #49093, .T. ) ;
#52302 = CARTESIAN_POINT ( 'NONE',  ( -1.623947472758999977, -83.30573296103600001, 0.5113958356693000251 ) ) ;
#52303 = AXIS2_PLACEMENT_3D ( 'NONE', #54410, #18975, #31356 ) ;
#52304 = CARTESIAN_POINT ( 'NONE',  ( 1.349451115848000038, -80.09934566756000152, -0.8326934693224998796 ) ) ;
#52305 = CARTESIAN_POINT ( 'NONE',  ( 0.5999999999999999778, -18.84999999999000053, 11.79999999999999893 ) ) ;
#52306 = CARTESIAN_POINT ( 'NONE',  ( -10.86788298907000083, -77.60066286050300732, -5.040355520269000245 ) ) ;
#52307 = DIRECTION ( 'NONE',  ( 0.000000000000000000, -1.000000000000000000, 0.000000000000000000 ) ) ;
#52308 = CARTESIAN_POINT ( 'NONE',  ( 0.5269479332349999989, -83.06056507816398948, 1.580352090963000000 ) ) ;
#52309 = CARTESIAN_POINT ( 'NONE',  ( 0.7960987979667577541, -2.106806941851198989, 3.429641257530567255 ) ) ;
#52310 = CARTESIAN_POINT ( 'NONE',  ( -3.339615680726000235, -78.59305584965399305, 9.131854552393999569 ) ) ;
#52311 = CARTESIAN_POINT ( 'NONE',  ( -3.833926501619000060, -77.73508576487398614, -8.716156481626001096 ) ) ;
#52312 = CARTESIAN_POINT ( 'NONE',  ( 8.414570695956999913, -59.94999999967000548, -8.414570695956999913 ) ) ;
#52313 = CARTESIAN_POINT ( 'NONE',  ( 0.2583767295275999909, -78.65347427100999766, -10.91369642039000176 ) ) ;
#52314 = CARTESIAN_POINT ( 'NONE',  ( 7.342331066867000544, -59.94999999967000548, 8.190859204290999784 ) ) ;
#52315 = CARTESIAN_POINT ( 'NONE',  ( -1.165026237870049997, -81.11652304393463453, 0.5177110879644187813 ) ) ;
#52316 = VERTEX_POINT ( 'NONE', #45650 ) ;
#52317 = CARTESIAN_POINT ( 'NONE',  ( 0.000000000000000000, -87.20000000000000284, 0.000000000000000000 ) ) ;
#52318 = CIRCLE ( 'NONE', #14618, 9.549999999999998934 ) ;
#52319 = CARTESIAN_POINT ( 'NONE',  ( -12.22925423141000145, -79.83317873820959676, -1.014767581180999967 ) ) ;
#52320 = EDGE_CURVE ( 'NONE', #17174, #26247, #50068, .T. ) ;
#52321 = DIRECTION ( 'NONE',  ( 0.000000000000000000, -1.000000000000000000, 0.000000000000000000 ) ) ;
#52322 = CARTESIAN_POINT ( 'NONE',  ( -10.54491486739000017, -77.86157840498900384, -3.823987582478999947 ) ) ;
#52323 = CARTESIAN_POINT ( 'NONE',  ( 10.87588596538000019, -79.60911308675498788, -1.476184626237000197 ) ) ;
#52324 = DIRECTION ( 'NONE',  ( 0.000000000000000000, -1.000000000000000000, 0.000000000000000000 ) ) ;
#52325 = CARTESIAN_POINT ( 'NONE',  ( -1.930860503549513663, -18.22582494086907090, 12.72930866331778432 ) ) ;
#52326 = CARTESIAN_POINT ( 'NONE',  ( 0.4138966918734000022, -76.20430140319000145, -12.14554839628999972 ) ) ;
#52327 = DIRECTION ( 'NONE',  ( -1.000000000000000000, 0.000000000000000000, 0.000000000000000000 ) ) ;
#52328 = CARTESIAN_POINT ( 'NONE',  ( -7.635939347819122425, -60.57525282287573276, 10.36595956262699580 ) ) ;
#52329 = EDGE_LOOP ( 'NONE', ( #40869, #41805, #54302, #37523 ) ) ;
#52330 = CARTESIAN_POINT ( 'NONE',  ( -10.33279081301000168, -79.73946642284398933, -4.181869747484999955 ) ) ;
#52331 = CARTESIAN_POINT ( 'NONE',  ( -1.178384143479807022, -80.07328496558248787, 0.4165272804027306819 ) ) ;
#52332 = DIRECTION ( 'NONE',  ( 1.000000000000000000, 0.000000000000000000, 0.000000000000000000 ) ) ;
#52333 = CARTESIAN_POINT ( 'NONE',  ( -3.006161377376999955, -78.57568030843599161, 10.85780494109000038 ) ) ;
#52334 = CARTESIAN_POINT ( 'NONE',  ( -12.71658872087999903, -60.11584731951999316, -1.931087888240000217 ) ) ;
#52335 = PLANE ( 'NONE',  #37719 ) ;
#52336 = CARTESIAN_POINT ( 'NONE',  ( -14.00000000000000000, -32.70420297070000260, 0.000000000000000000 ) ) ;
#52337 = CARTESIAN_POINT ( 'NONE',  ( -1.144681710389366502, -82.79268177178988708, 0.9866455203037115540 ) ) ;
#52338 = ADVANCED_FACE ( 'NONE', ( #39733 ), #4728, .F. ) ;
#52339 = CARTESIAN_POINT ( 'NONE',  ( -0.9895445474833923782, -79.65312179139979776, -0.7673432424604474944 ) ) ;
#52340 = CARTESIAN_POINT ( 'NONE',  ( 2.062597265787999845, -22.78461666469000235, 12.87024489156999962 ) ) ;
#52341 =( NAMED_UNIT ( * ) PLANE_ANGLE_UNIT ( ) SI_UNIT ( $, .RADIAN. ) );
#52342 = AXIS2_PLACEMENT_3D ( 'NONE', #52746, #26160, #21443 ) ;
#52343 = CARTESIAN_POINT ( 'NONE',  ( -12.44180635029999848, -24.09260544925000147, 1.459447571597000115 ) ) ;
#52344 = ORIENTED_EDGE ( 'NONE', *, *, #18774, .T. ) ;
#52345 = ORIENTED_EDGE ( 'NONE', *, *, #11660, .T. ) ;
#52346 = PLANE ( 'NONE',  #32393 ) ;
#52347 = TOROIDAL_SURFACE ( 'NONE', #24984, 13.50000000000000000, 0.5000000000000000000 ) ;
#52348 = ORIENTED_EDGE ( 'NONE', *, *, #7679, .T. ) ;
#52349 = B_SPLINE_CURVE_WITH_KNOTS ( 'NONE', 3,
 ( #33733, #20465, #5706, #42901, #14852, #28424, #19883, #24308, #42322, #50894, #33442, #6295, #55897, #24598, #41728, #55601 ),
 .UNSPECIFIED., .F., .F.,
 ( 4, 2, 1, 2, 1, 2, 2, 2, 4 ),
 ( 0.000000000000000000, 0.1249999999999998890, 0.2499999999999998335, 0.3749999999999998335, 0.4999999999999998890, 0.6249999999999998890, 0.7499999999999998890, 0.8749999999999998890, 1.000000000000000000 ),
 .UNSPECIFIED. ) ;
#52351 = ADVANCED_FACE ( 'NONE', ( #41199 ), #789, .T. ) ;
#52350 = ORIENTED_EDGE ( 'NONE', *, *, #23570, .F. ) ;
#52352 = CARTESIAN_POINT ( 'NONE',  ( 0.3926218265389159190, -81.85416666667249785, 1.460959015002474715 ) ) ;
#52353 = CARTESIAN_POINT ( 'NONE',  ( 10.50536548972000084, -77.30149375871098982, -2.968612793496999913 ) ) ;
#52354 = CARTESIAN_POINT ( 'NONE',  ( 1.750000000001000089, -59.55077028460999600, 12.60356226396000068 ) ) ;
#52355 = CARTESIAN_POINT ( 'NONE',  ( 6.721258625739999992, -78.37826332859900447, -7.130431436203999773 ) ) ;
#52356 = VECTOR ( 'NONE', #18467, 1000.000000000000000 ) ;
#52357 = CARTESIAN_POINT ( 'NONE',  ( -3.292086955815877847, -78.19615833579152309, -8.644430884715466945 ) ) ;
#52358 = CARTESIAN_POINT ( 'NONE',  ( -1.255625495614115295, -79.38580225533669932, 9.243491999774299472 ) ) ;
#52359 = ORIENTED_EDGE ( 'NONE', *, *, #1601, .F. ) ;
#52360 = EDGE_LOOP ( 'NONE', ( #16222, #12536, #11342, #7733, #17289, #33299 ) ) ;
#52361 = CARTESIAN_POINT ( 'NONE',  ( -3.114065545470247276, -77.50245480038890378, 8.710212348931921866 ) ) ;
#52362 = CARTESIAN_POINT ( 'NONE',  ( 6.393001003723999709, -77.13539953215739331, 9.000752526674000720 ) ) ;
#52363 = CARTESIAN_POINT ( 'NONE',  ( 11.00000000000000178, -78.34292008887531722, -0.9786566581934403874 ) ) ;
#52364 = CARTESIAN_POINT ( 'NONE',  ( 6.240531904507999883, -78.14956573113299498, 7.431451467605000083 ) ) ;
#52365 = CARTESIAN_POINT ( 'NONE',  ( 7.641012386038000592, -18.71082434677000350, 10.18589234708000113 ) ) ;
#52366 = CARTESIAN_POINT ( 'NONE',  ( -0.9995835529977281642, -79.94791666666664298, 0.7681833999686391579 ) ) ;
#52367 = CARTESIAN_POINT ( 'NONE',  ( 11.10498291493000167, -80.16715056412299134, -1.830582403018000015 ) ) ;
#52368 = CYLINDRICAL_SURFACE ( 'NONE', #40096, 1.750000000000000000 ) ;
#52369 = ADVANCED_FACE ( 'NONE', ( #25155 ), #11598, .F. ) ;
#52370 = CARTESIAN_POINT ( 'NONE',  ( -7.919595949288999570, -59.94999999967000548, -8.768124086712999699 ) ) ;
#52371 = CARTESIAN_POINT ( 'NONE',  ( -9.699677589918225706, -76.65189001212350206, 6.631369083228229933 ) ) ;
#52372 = ADVANCED_FACE ( 'NONE', ( #7154 ), #24873, .F. ) ;
#52373 = CARTESIAN_POINT ( 'NONE',  ( -4.000000000000000000, -75.00000000000001421, 0.5999999999999999778 ) ) ;
#52374 = CARTESIAN_POINT ( 'NONE',  ( 8.377812017747999107, -78.73796332859900815, 5.294595800518999695 ) ) ;
#52375 = CARTESIAN_POINT ( 'NONE',  ( -7.615853692923001184, -78.63150737603899643, 9.247423260715999405 ) ) ;
#52376 = CARTESIAN_POINT ( 'NONE',  ( -12.71466317168545679, -60.93795986706020074, 1.778778223980820306 ) ) ;
#52378 = FACE_OUTER_BOUND ( 'NONE', #48504, .T. ) ;
#52377 = CARTESIAN_POINT ( 'NONE',  ( 9.009514222719491983, -78.37087597555611751, 2.421282354168349471 ) ) ;
#52379 = CARTESIAN_POINT ( 'NONE',  ( 3.247140714122291438, -1.341038642068812736, -0.4257306128977228488 ) ) ;
#52380 = CARTESIAN_POINT ( 'NONE',  ( -10.81434145419000181, -79.94637966341998947, -2.373591376386999574 ) ) ;
#52381 = CARTESIAN_POINT ( 'NONE',  ( 10.80251317621999974, -78.09622061874799215, 3.184285419974999698 ) ) ;
#52383 = DIRECTION ( 'NONE',  ( 0.9859154929577472748, 0.1672442547470080754, 0.000000000000000000 ) ) ;
#52382 =( BOUNDED_SURFACE ( )  B_SPLINE_SURFACE ( 3, 3, ( 
 ( #16379, #12234, #11951, #20519, #47695, #26587, #2234 ),
 ( #53776, #33785, #7518, #38517, #20232, #56532, #16091 ),
 ( #11381, #34073, #31015, #25515, #49053, #11668, #29642 ),
 ( #44621, #7225, #25228, #4177, #22174, #75, #27472 ),
 ( #5624, #18054, #23348, #40773, #54070, #54362, #32766 ),
 ( #22763, #13606, #32473, #45509, #367, #55221, #36919 ),
 ( #49940, #4762, #28053, #46099, #13902, #27176, #14768 ),
 ( #23635, #18640, #41648, #19217, #50813, #36046, #41360 ),
 ( #54930, #31602, #49645, #18347, #41069, #9191, #45806 ),
 ( #45214, #5341, #50227, #18924, #36337, #36632, #5055 ),
 ( #31896, #942, #9485, #23053, #655, #9774, #27763 ),
 ( #2097, #46391, #6503, #10950, #19801, #24512, #2381 ),
 ( #15368, #37795, #56107, #33059, #56681, #1513, #16237 ),
 ( #42239, #46975, #28638, #52252, #38661, #15653, #33650 ),
 ( #55518, #20094, #51394, #55815, #28931, #5916, #42528 ) ),
 .UNSPECIFIED., .F., .F., .T. ) 
 B_SPLINE_SURFACE_WITH_KNOTS ( ( 4, 1, 1, 1, 1, 1, 1, 1, 1, 1, 1, 1, 4 ),
 ( 4, 3, 4 ),
 ( 0.009836358966825000175, 0.09153389967814999639, 0.1732269073519000224, 0.2549246240467999969, 0.3366128957582000258, 0.4183102327763000283, 0.5000049915179999305, 0.5816997512343000665, 0.6633971206824998967, 0.7450853986059999823, 0.8267830947368000061, 0.9084761241232000017, 0.9901736240545999657 ),
 ( 0.000000000000000000, 0.5000000000000000000, 1.000000000000000000 ),
 .UNSPECIFIED. ) 
 GEOMETRIC_REPRESENTATION_ITEM ( )  RATIONAL_B_SPLINE_SURFACE ( (
 ( 1.000000000000000000, 0.8025111804430778983, 0.8025111804430778983, 1.000000000000000000, 0.8025111804430778983, 0.8025111804430778983, 1.000000000000000000),
 ( 1.000000000000000000, 0.8025111804430778983, 0.8025111804430778983, 1.000000000000000000, 0.8025111804430778983, 0.8025111804430778983, 1.000000000000000000),
 ( 1.000000000000000000, 0.8025111804430778983, 0.8025111804430778983, 1.000000000000000000, 0.8025111804430778983, 0.8025111804430778983, 1.000000000000000000),
 ( 1.000000000000000000, 0.8025111804430778983, 0.8025111804430778983, 1.000000000000000000, 0.8025111804430778983, 0.8025111804430778983, 1.000000000000000000),
 ( 1.000000000000000000, 0.8025111804430778983, 0.8025111804430778983, 1.000000000000000000, 0.8025111804430778983, 0.8025111804430778983, 1.000000000000000000),
 ( 1.000000000000000000, 0.8025111804430778983, 0.8025111804430778983, 1.000000000000000000, 0.8025111804430778983, 0.8025111804430778983, 1.000000000000000000),
 ( 1.000000000000000000, 0.8025111804430778983, 0.8025111804430778983, 1.000000000000000000, 0.8025111804430778983, 0.8025111804430778983, 1.000000000000000000),
 ( 1.000000000000000000, 0.8025111804430778983, 0.8025111804430778983, 1.000000000000000000, 0.8025111804430778983, 0.8025111804430778983, 1.000000000000000000),
 ( 1.000000000000000000, 0.8025111804430778983, 0.8025111804430778983, 1.000000000000000000, 0.8025111804430778983, 0.8025111804430778983, 1.000000000000000000),
 ( 1.000000000000000000, 0.8025111804430778983, 0.8025111804430778983, 1.000000000000000000, 0.8025111804430778983, 0.8025111804430778983, 1.000000000000000000),
 ( 1.000000000000000000, 0.8025111804430778983, 0.8025111804430778983, 1.000000000000000000, 0.8025111804430778983, 0.8025111804430778983, 1.000000000000000000),
 ( 1.000000000000000000, 0.8025111804430778983, 0.8025111804430778983, 1.000000000000000000, 0.8025111804430778983, 0.8025111804430778983, 1.000000000000000000),
 ( 1.000000000000000000, 0.8025111804430778983, 0.8025111804430778983, 1.000000000000000000, 0.8025111804430778983, 0.8025111804430778983, 1.000000000000000000),
 ( 1.000000000000000000, 0.8025111804430778983, 0.8025111804430778983, 1.000000000000000000, 0.8025111804430778983, 0.8025111804430778983, 1.000000000000000000),
 ( 1.000000000000000000, 0.8025111804430778983, 0.8025111804430778983, 1.000000000000000000, 0.8025111804430778983, 0.8025111804430778983, 1.000000000000000000) ) ) 
 REPRESENTATION_ITEM ( '' )  SURFACE ( )  );
#52384 = CARTESIAN_POINT ( 'NONE',  ( 1.750000000000000000, -55.55000000278000272, 12.50000000000000000 ) ) ;
#52385 = EDGE_LOOP ( 'NONE', ( #20178, #22403, #5538, #4189 ) ) ;
#52386 = DIRECTION ( 'NONE',  ( 0.7071067811865475727, 0.000000000000000000, -0.7071067811865475727 ) ) ;
#52387 = CARTESIAN_POINT ( 'NONE',  ( -1.750000000000000000, -60.04999999657000131, 12.50000000000000000 ) ) ;
#52388 = VECTOR ( 'NONE', #7924, 1000.000000000000000 ) ;
#52389 = CARTESIAN_POINT ( 'NONE',  ( 1.062401685567854859, -78.39434672560830109, 0.6596734765841812953 ) ) ;
#52390 = EDGE_CURVE ( 'NONE', #58211, #44781, #17996, .T. ) ;
#52391 = CARTESIAN_POINT ( 'NONE',  ( -0.06531150999164000992, -3.507872475527999967, 3.644635206812000039 ) ) ;
#52392 = CARTESIAN_POINT ( 'NONE',  ( 3.858758824815000210, -80.05130441783499862, -8.679482335691000472 ) ) ;
#52393 = CARTESIAN_POINT ( 'NONE',  ( 8.596118241356434098, -76.90225025436217265, 6.606116134054767386 ) ) ;
#52394 = FACE_OUTER_BOUND ( 'NONE', #12952, .T. ) ;
#52395 = CARTESIAN_POINT ( 'NONE',  ( 1.997276839918477265, -3.177083333333333481, -2.598917237794082791 ) ) ;
#52396 = CARTESIAN_POINT ( 'NONE',  ( 0.000000000000000000, -75.00000000000000000, 0.000000000000000000 ) ) ;
#52397 = PLANE ( 'NONE',  #33489 ) ;
#52398 = CARTESIAN_POINT ( 'NONE',  ( -8.664714296349000477, -77.25360149971999135, 6.868106230948000324 ) ) ;
#52399 = CARTESIAN_POINT ( 'NONE',  ( -0.004069935249280053416, -76.32474826787533573, -11.74984247143509464 ) ) ;
#52400 = CARTESIAN_POINT ( 'NONE',  ( 5.119217263405000828, -77.54589325954400181, 9.901929871541000239 ) ) ;
#52401 = CARTESIAN_POINT ( 'NONE',  ( 1.148655909719971113, -81.88235501812725659, 0.4929135997214548759 ) ) ;
#52402 = CARTESIAN_POINT ( 'NONE',  ( -1.004305231718999991, -1.000000000000000000, 3.090933677959000203 ) ) ;
#52403 = CARTESIAN_POINT ( 'NONE',  ( 8.838834764832000701, -18.75000000000000000, -8.838834764832000701 ) ) ;
#52404 = CARTESIAN_POINT ( 'NONE',  ( -9.009247259181929479, -78.47916666666665719, 2.421167930323313566 ) ) ;
#52405 = CARTESIAN_POINT ( 'NONE',  ( -3.395896365324738486, -0.7630208295731387702, -0.9134964888522767446 ) ) ;
#52406 = CARTESIAN_POINT ( 'NONE',  ( 7.043910409642034409, -80.28198538032874865, -8.120786863705317771 ) ) ;
#52407 = CARTESIAN_POINT ( 'NONE',  ( 10.65248731882857491, -79.86234087736364984, 1.664133241301937405 ) ) ;
#52408 = CARTESIAN_POINT ( 'NONE',  ( -1.134730520616228144, -81.33997286840332208, -0.9788030900385257249 ) ) ;
#52409 = CARTESIAN_POINT ( 'NONE',  ( 10.43959491470999978, -79.70693983506599523, -5.976816984917999953 ) ) ;
#52410 = CARTESIAN_POINT ( 'NONE',  ( -9.500000000000007105, -78.78958333333333997, 1.243547092045919733 ) ) ;
#52411 = DIRECTION ( 'NONE',  ( -1.000000000000000000, 0.000000000000000000, 0.000000000000000000 ) ) ;
#52412 = VERTEX_POINT ( 'NONE', #56752 ) ;
#52413 = DIRECTION ( 'NONE',  ( -0.8965517241377957136, -0.4429390544366978988, -5.195107294457976971E-07 ) ) ;
#52414 = ORIENTED_EDGE ( 'NONE', *, *, #25946, .F. ) ;
#52416 = EDGE_CURVE ( 'NONE', #11264, #30968, #26088, .T. ) ;
#52415 = ORIENTED_EDGE ( 'NONE', *, *, #14756, .T. ) ;
#52417 = CARTESIAN_POINT ( 'NONE',  ( 0.4254240051736071226, -1.364583333333333037, 3.250000000000001776 ) ) ;
#52418 = VERTEX_POINT ( 'NONE', #12163 ) ;
#52419 = CARTESIAN_POINT ( 'NONE',  ( -1.194548181431000167, -81.98044359648298496, -3.339855766669999948 ) ) ;
#52420 = CARTESIAN_POINT ( 'NONE',  ( 2.753209777146519599, -79.25137801636039114, 9.093106921346176819 ) ) ;
#52421 = CIRCLE ( 'NONE', #34478, 0.5000000000000006661 ) ;
#52422 = ORIENTED_EDGE ( 'NONE', *, *, #20733, .F. ) ;
#52423 = CARTESIAN_POINT ( 'NONE',  ( 0.2465309757704703397, -82.74125708629129861, -1.225171777312197952 ) ) ;
#52424 = FACE_OUTER_BOUND ( 'NONE', #25973, .T. ) ;
#52425 = ORIENTED_EDGE ( 'NONE', *, *, #27902, .T. ) ;
#52426 = CARTESIAN_POINT ( 'NONE',  ( 0.5606705885283177482, -79.43831444490541571, 1.120598156864235584 ) ) ;
#52427 = CARTESIAN_POINT ( 'NONE',  ( 0.5698392209909881601, -79.09439922511995746, 1.421990052734795729 ) ) ;
#52428 = CARTESIAN_POINT ( 'NONE',  ( 17.50000000000000000, -21.00000000000000000, 0.000000000000000000 ) ) ;
#52429 = CIRCLE ( 'NONE', #23216, 0.8000000000000000444 ) ;
#52430 = CARTESIAN_POINT ( 'NONE',  ( -0.5999999999999999778, -18.84999999999999787, 10.98362417419999915 ) ) ;
#52431 = CARTESIAN_POINT ( 'NONE',  ( 3.112536659741943268, -86.17851879815597727, -1.385790604991126607 ) ) ;
#52432 = CARTESIAN_POINT ( 'NONE',  ( 7.995633008690000487, -76.71329633841800444, 7.819446035993999899 ) ) ;
#52433 = DIRECTION ( 'NONE',  ( -1.000000000000000000, 0.000000000000000000, 0.000000000000000000 ) ) ;
#52434 = CARTESIAN_POINT ( 'NONE',  ( -6.760013919724102038, -78.62708333333333144, 8.796335266379953666 ) ) ;
#52435 = CARTESIAN_POINT ( 'NONE',  ( 1.819226710355999810, -76.82064092468800709, 10.84768487502000056 ) ) ;
#52436 = DIRECTION ( 'NONE',  ( 0.000000000000000000, 0.000000000000000000, -1.000000000000000000 ) ) ;
#52437 = EDGE_CURVE ( 'NONE', #35953, #45142, #16595, .T. ) ;
#52438 = CARTESIAN_POINT ( 'NONE',  ( -10.69668321983107973, -80.11953358945446269, -2.665761377985893077 ) ) ;
#52439 = CARTESIAN_POINT ( 'NONE',  ( -0.9650089711215688038, -2.999625284671528558, 3.117517381082792305 ) ) ;
#52440 = CARTESIAN_POINT ( 'NONE',  ( -2.879346558283000235, -78.56178455456850429, -2.412654453515000075 ) ) ;
#52441 = CARTESIAN_POINT ( 'NONE',  ( -4.129275505618361208, -78.00639181381374954, 9.925283770886389689 ) ) ;
#52442 = CARTESIAN_POINT ( 'NONE',  ( 0.000000000000000000, -75.67500000000001137, 0.000000000000000000 ) ) ;
#52443 = CARTESIAN_POINT ( 'NONE',  ( -2.624566716334498562, -80.99486133380281672, 10.45026324297856313 ) ) ;
#52444 = CARTESIAN_POINT ( 'NONE',  ( 3.122208683565999898, -85.38874735065199673, -1.678325600246000082 ) ) ;
#52445 = CARTESIAN_POINT ( 'NONE',  ( -11.74981921324623535, -76.20131312293446513, -0.2383779811271709292 ) ) ;
#52446 = CARTESIAN_POINT ( 'NONE',  ( 10.42274798264000069, -21.75365779208000205, 7.691916945395000482 ) ) ;
#52447 = CARTESIAN_POINT ( 'NONE',  ( -8.950141054477999347, -62.00112627243999697, -8.958565985388998953 ) ) ;
#52448 = CARTESIAN_POINT ( 'NONE',  ( -8.485281374238999419, -23.25000000000000000, 8.485281374238999419 ) ) ;
#52449 = EDGE_CURVE ( 'NONE', #17089, #18212, #41649, .T. ) ;
#52450 = CARTESIAN_POINT ( 'NONE',  ( -1.500000000000000222, -77.51041666666668561, -0.1963495408493622085 ) ) ;
#52452 = ADVANCED_FACE ( 'NONE', ( #7731 ), #55723, .F. ) ;
#52451 = CARTESIAN_POINT ( 'NONE',  ( 5.246383657897999875, -77.06100733245999379, -10.79237965019999912 ) ) ;
#52453 = LINE ( 'NONE', #53027, #54536 ) ;
#52454 = CARTESIAN_POINT ( 'NONE',  ( 5.330173052271000245, -78.14419244445099366, 9.594439332582000546 ) ) ;
#52455 = CARTESIAN_POINT ( 'NONE',  ( 1.232226823824839501, -24.52290911267632723, -12.50408896749732968 ) ) ;
#52456 = CARTESIAN_POINT ( 'NONE',  ( -0.4636611700996999819, -76.79051831062999156, -12.20320586788999861 ) ) ;
#52457 = ORIENTED_EDGE ( 'NONE', *, *, #14587, .T. ) ;
#52458 = CARTESIAN_POINT ( 'NONE',  ( -10.87500000000999911, -76.17499999999400018, 1.221063213659000093E-09 ) ) ;
#52459 = CARTESIAN_POINT ( 'NONE',  ( 3.518657424385000176, -85.83735716284299144, -1.566607219110000004 ) ) ;
#52460 = CARTESIAN_POINT ( 'NONE',  ( 12.65987830577000040, -61.73692962272999551, 0.9847759095506000149 ) ) ;
#52461 = CARTESIAN_POINT ( 'NONE',  ( -3.269659986048999656, -78.85953063649999706, -12.04652652115999878 ) ) ;
#52462 = CARTESIAN_POINT ( 'NONE',  ( 12.49996905247000001, -55.60797343434000339, -1.666511841116000037 ) ) ;
#52463 = CARTESIAN_POINT ( 'NONE',  ( -4.724527880064000485, -78.87325255039799288, 8.267358256580001452 ) ) ;
#52464 = CARTESIAN_POINT ( 'NONE',  ( 4.038192700013000014, -83.90181010973100229, -1.050272432624000052 ) ) ;
#52465 = CARTESIAN_POINT ( 'NONE',  ( 4.210840025191989078, -79.94311247203964399, 9.890888605214144036 ) ) ;
#52466 = FACE_OUTER_BOUND ( 'NONE', #28205, .T. ) ;
#52467 = VERTEX_POINT ( 'NONE', #39024 ) ;
#52468 = CIRCLE ( 'NONE', #3450, 1.000000000000000000 ) ;
#52469 = CARTESIAN_POINT ( 'NONE',  ( -8.796335266379989193, -78.75208333333333144, -6.760013919724055853 ) ) ;
#52470 = EDGE_CURVE ( 'NONE', #54661, #52194, #54746, .T. ) ;
#52471 = DIRECTION ( 'NONE',  ( 0.8090169943749183634, 0.000000000000000000, -0.5877852522925132162 ) ) ;
#52472 = CIRCLE ( 'NONE', #1581, 11.65000000000000036 ) ;
#52473 = ORIENTED_EDGE ( 'NONE', *, *, #54435, .T. ) ;
#52474 = VECTOR ( 'NONE', #53437, 1000.000000000000114 ) ;
#52475 = CARTESIAN_POINT ( 'NONE',  ( 3.292343003156000147, -79.02013871977898418, -10.43303857396000112 ) ) ;
#52476 = CARTESIAN_POINT ( 'NONE',  ( 12.69616050744000013, -58.55171076491000548, 1.799475304559999822 ) ) ;
#52477 = CARTESIAN_POINT ( 'NONE',  ( -3.551539514618999860, -80.34199133049699526, -10.51033889552999945 ) ) ;
#52478 = VECTOR ( 'NONE', #57376, 1000.000000000000000 ) ;
#52479 = ORIENTED_EDGE ( 'NONE', *, *, #27937, .T. ) ;
#52480 = ORIENTED_EDGE ( 'NONE', *, *, #27126, .T. ) ;
#52482 = ADVANCED_FACE ( 'NONE', ( #30442 ), #34580, .T. ) ;
#52481 = EDGE_LOOP ( 'NONE', ( #43619, #41522, #9497, #10437 ) ) ;
#52483 = CARTESIAN_POINT ( 'NONE',  ( 0.4761608617425592271, -80.44399108949784249, 1.155693504187701448 ) ) ;
#52484 = ADVANCED_FACE ( 'NONE', ( #52612 ), #44038, .F. ) ;
#52485 = CARTESIAN_POINT ( 'NONE',  ( -10.19607599377606633, -78.15737564367177015, 5.890537601704129322 ) ) ;
#52486 = CARTESIAN_POINT ( 'NONE',  ( 5.496668217546000434, -80.30272527494601320, -8.073860231047000013 ) ) ;
#52487 = ORIENTED_EDGE ( 'NONE', *, *, #47567, .F. ) ;
#52488 = EDGE_LOOP ( 'NONE', ( #47068, #46474, #55982, #13269 ) ) ;
#52489 = CARTESIAN_POINT ( 'NONE',  ( 8.438902753042999194, -78.73539140552688309, -8.898539530003999332 ) ) ;
#52490 = CARTESIAN_POINT ( 'NONE',  ( -2.265513919728744163, -78.99318692756679638, -3.757367528743593699 ) ) ;
#52491 = CARTESIAN_POINT ( 'NONE',  ( 10.15833271780000047, -54.58011549179999378, 7.756208840337999177 ) ) ;
#52492 = CARTESIAN_POINT ( 'NONE',  ( 7.921329716887100858, -17.44906234264657741, -10.04564005581343267 ) ) ;
#52493 = DIRECTION ( 'NONE',  ( 0.000000000000000000, 1.000000000000000000, 0.000000000000000000 ) ) ;
#52494 = CARTESIAN_POINT ( 'NONE',  ( -3.230870548382956287, -78.14717913613844757, -9.172510579469401293 ) ) ;
#52495 = CARTESIAN_POINT ( 'NONE',  ( -11.18477258988041179, -80.85528771549159899, -0.7651659436797575431 ) ) ;
#52496 = DIRECTION ( 'NONE',  ( 0.7071067811865474617, 0.000000000000000000, 0.7071067811865474617 ) ) ;
#52497 = CARTESIAN_POINT ( 'NONE',  ( 8.733346097342675307, -78.82335531160738640, -3.049546898630470348 ) ) ;
#52498 = CARTESIAN_POINT ( 'NONE',  ( -3.438348731682000281, -76.55047324479998849, -11.82003900998999946 ) ) ;
#52499 = AXIS2_PLACEMENT_3D ( 'NONE', #44741, #53302, #12845 ) ;
#52500 = CARTESIAN_POINT ( 'NONE',  ( 0.9271659294403999940, -81.29032046129098887, 4.067789135191000049 ) ) ;
#52501 = CARTESIAN_POINT ( 'NONE',  ( 7.747477005942000616, -78.01746001420200116, -6.119465872965999864 ) ) ;
#52502 = CARTESIAN_POINT ( 'NONE',  ( -0.3271848554491046945, -83.39583333333332860, 1.217465845835393301 ) ) ;
#52503 = CARTESIAN_POINT ( 'NONE',  ( 6.688645397968000950, -78.77709438844000545, 10.27915892414000076 ) ) ;
#52504 = CARTESIAN_POINT ( 'NONE',  ( -3.164411967817999827, -77.10257917258499560, -11.86639179494000018 ) ) ;
#52505 = CARTESIAN_POINT ( 'NONE',  ( -2.486604901413195901, -78.79583333333337691, 9.252740428348989354 ) ) ;
#52506 = AXIS2_PLACEMENT_3D ( 'NONE', #30776, #53522, #26352 ) ;
#52507 = CARTESIAN_POINT ( 'NONE',  ( 12.50686498856084228, -24.30484291404728481, -1.423095204833430438 ) ) ;
#52508 = CARTESIAN_POINT ( 'NONE',  ( -12.50000000000000000, -60.04999999657000131, -1.750000000000000000 ) ) ;
#52509 = CONICAL_SURFACE ( 'NONE', #17650, 0.6999999997695030007, 0.7853981633972997312 ) ;
#52510 = CARTESIAN_POINT ( 'NONE',  ( 1.081520234856472307, -80.43617599348539215, -1.105279526349218111 ) ) ;
#52511 = CYLINDRICAL_SURFACE ( 'NONE', #17425, 1.750000000000001332 ) ;
#52512 = DIRECTION ( 'NONE',  ( 0.000000000000000000, -1.000000000000000000, 0.000000000000000000 ) ) ;
#52513 = CARTESIAN_POINT ( 'NONE',  ( 1.310679582531387943, -78.70833333333332860, -0.7554284705563468760 ) ) ;
#52514 = CARTESIAN_POINT ( 'NONE',  ( 1.848759863635999867, -2.800056440563999605, 3.039663599590999965 ) ) ;
#52515 = CARTESIAN_POINT ( 'NONE',  ( 11.86727826211999925, -77.24499819968599468, -2.088899193827999934 ) ) ;
#52516 = CARTESIAN_POINT ( 'NONE',  ( -3.549595971449000409, -78.17549936685999512, 9.069733410961998032 ) ) ;
#52518 = CARTESIAN_POINT ( 'NONE',  ( -0.5351185351402000245, -79.15017770130199892, 1.205899990410000067 ) ) ;
#52517 = CARTESIAN_POINT ( 'NONE',  ( -12.70556836343000029, -53.57227722738999631, 1.774192865971000122E-09 ) ) ;
#52519 = CARTESIAN_POINT ( 'NONE',  ( 0.5015714934020000237, -83.05604790835199935, 1.504246450876000063 ) ) ;
#52520 = FACE_OUTER_BOUND ( 'NONE', #1350, .T. ) ;
#52521 = ORIENTED_EDGE ( 'NONE', *, *, #30353, .T. ) ;
#52522 = CARTESIAN_POINT ( 'NONE',  ( 5.462882135474435685, -78.73756601347038497, 10.73736906863111251 ) ) ;
#52523 = CARTESIAN_POINT ( 'NONE',  ( -3.728673265761000000, -79.59119008599400047, 11.44942132006000080 ) ) ;
#52524 = CARTESIAN_POINT ( 'NONE',  ( 0.3341971779677385679, -79.37780856233311511, -9.519315069472982671 ) ) ;
#52525 = CARTESIAN_POINT ( 'NONE',  ( -3.708203932498999933, -79.79999999999999716, 11.41267819554000162 ) ) ;
#52526 = CARTESIAN_POINT ( 'NONE',  ( -8.596763593984000806, -61.93532396089999992, 9.310159863737000663 ) ) ;
#52527 = CARTESIAN_POINT ( 'NONE',  ( 0.000000000000000000, -90.29999999999999716, 0.000000000000000000 ) ) ;
#52528 = CARTESIAN_POINT ( 'NONE',  ( -9.775952618636999603, -79.78297254464997934, -1.505437160947000086 ) ) ;
#52529 = CARTESIAN_POINT ( 'NONE',  ( -10.42531125070999920, -60.06485145371000556, 7.624341767111000756 ) ) ;
#52530 = CARTESIAN_POINT ( 'NONE',  ( -12.76303204291999904, -55.53514849259999409, -1.980584515756000030 ) ) ;
#52531 = ORIENTED_EDGE ( 'NONE', *, *, #55086, .F. ) ;
#52532 = CARTESIAN_POINT ( 'NONE',  ( -12.70556836343000029, -53.57227722738999631, 1.774192865971000122E-09 ) ) ;
#52533 = CARTESIAN_POINT ( 'NONE',  ( 4.510348846891466756, -79.20585849186471705, -10.94228070689720234 ) ) ;
#52534 = CARTESIAN_POINT ( 'NONE',  ( -9.609463960252000447, -79.75128667140099026, 0.6773526969735000902 ) ) ;
#52535 = EDGE_CURVE ( 'NONE', #48909, #2755, #31050, .T. ) ;
#52536 = CARTESIAN_POINT ( 'NONE',  ( -1.500000000000000000, -78.39999999999999147, 0.000000000000000000 ) ) ;
#52537 = ADVANCED_FACE ( 'NONE', ( #17162 ), #40767, .F. ) ;
#52538 = CARTESIAN_POINT ( 'NONE',  ( 1.640574411872000038, -79.53428134424000007, 0.2893137654249999802 ) ) ;
#52539 = VERTEX_POINT ( 'NONE', #36625 ) ;
#52540 = LINE ( 'NONE', #20381, #5868 ) ;
#52541 = CARTESIAN_POINT ( 'NONE',  ( -8.749250031325688681, -76.99999999999998579, 3.121704046829004486 ) ) ;
#52542 = CARTESIAN_POINT ( 'NONE',  ( 1.799475295154000065, -57.04916621739000249, -12.69619287815999975 ) ) ;
#52543 = VECTOR ( 'NONE', #37328, 1000.000000000000114 ) ;
#52544 = CARTESIAN_POINT ( 'NONE',  ( 3.463640375329640531, -78.44897895074308281, 10.20056074439654914 ) ) ;
#52545 = EDGE_CURVE ( 'NONE', #57774, #9471, #29280, .T. ) ;
#52546 = CARTESIAN_POINT ( 'NONE',  ( 9.630577183392999174, -78.97287637980998909, 1.628483183780000010 ) ) ;
#52547 = ORIENTED_EDGE ( 'NONE', *, *, #35582, .T. ) ;
#52548 = VECTOR ( 'NONE', #33446, 1000.000000000000000 ) ;
#52549 = ORIENTED_EDGE ( 'NONE', *, *, #267, .T. ) ;
#52550 = CARTESIAN_POINT ( 'NONE',  ( -7.841711555745998652, -76.89807700115400735, -9.847868799306999321 ) ) ;
#52551 = CARTESIAN_POINT ( 'NONE',  ( 4.176452633942115966, -78.75676650919550070, -9.905560661817728985 ) ) ;
#52552 = CARTESIAN_POINT ( 'NONE',  ( 1.376276113774000054, -77.87323392310999282, -0.3553535975348000031 ) ) ;
#52553 = AXIS2_PLACEMENT_3D ( 'NONE', #2228, #12512, #34646 ) ;
#52554 = ORIENTED_EDGE ( 'NONE', *, *, #22940, .T. ) ;
#52555 = CARTESIAN_POINT ( 'NONE',  ( 5.102724688570000389, -77.95894361655099658, 7.811319209985999379 ) ) ;
#52556 = DIRECTION ( 'NONE',  ( 0.000000000000000000, 1.000000000000000000, 0.000000000000000000 ) ) ;
#52557 = AXIS2_PLACEMENT_3D ( 'NONE', #42117, #55103, #5797 ) ;
#52558 = CARTESIAN_POINT ( 'NONE',  ( -0.2584144827919511722, -53.57154603038791407, 12.70558781482546706 ) ) ;
#52559 = ADVANCED_FACE ( 'NONE', ( #40475 ), #45207, .F. ) ;
#52560 = CARTESIAN_POINT ( 'NONE',  ( -3.148725677322000482, -78.06332093041999087, 12.40542962523000092 ) ) ;
#52561 = CARTESIAN_POINT ( 'NONE',  ( 8.596622369410699349, -79.79792950508202409, -6.606549433422280515 ) ) ;
#52562 = DIRECTION ( 'NONE',  ( 0.000000000000000000, 0.000000000000000000, 1.000000000000000000 ) ) ;
#52563 = CARTESIAN_POINT ( 'NONE',  ( 3.194290819685381866, -86.09999999999998010, 2.320109443757771395 ) ) ;
#52564 = CARTESIAN_POINT ( 'NONE',  ( 5.745747329289000227, -78.73388662847199271, 9.633509135241000720 ) ) ;
#52565 = EDGE_CURVE ( 'NONE', #34959, #33149, #46297, .T. ) ;
#52566 = CARTESIAN_POINT ( 'NONE',  ( 1.034214221880000141E-14, 0.2999999999999999334, 0.000000000000000000 ) ) ;
#52567 = VERTEX_POINT ( 'NONE', #69 ) ;
#52568 = CARTESIAN_POINT ( 'NONE',  ( 0.000000000000000000, -80.89999999999999147, 0.000000000000000000 ) ) ;
#52569 = ORIENTED_EDGE ( 'NONE', *, *, #37977, .T. ) ;
#52570 = CARTESIAN_POINT ( 'NONE',  ( -10.71960490440000058, -78.59592221579498528, 3.466843673432000283 ) ) ;
#52571 = CARTESIAN_POINT ( 'NONE',  ( 7.535862037907478772, -77.30086240167952383, -5.364085342277994606 ) ) ;
#52572 = CARTESIAN_POINT ( 'NONE',  ( -0.9004272109156999937, -80.67671995918098560, 0.9642496934733999492 ) ) ;
#52573 = LINE ( 'NONE', #48160, #46558 ) ;
#52574 = CARTESIAN_POINT ( 'NONE',  ( 9.510318522500906369, -76.49977934536502744, 6.915946567881195328 ) ) ;
#52575 = CARTESIAN_POINT ( 'NONE',  ( -1.377158602743000060, -77.62176762208750347, -0.3366111412210999743 ) ) ;
#52576 = CARTESIAN_POINT ( 'NONE',  ( 1.980584515752000119, -55.53514853344000102, 12.76303204600000107 ) ) ;
#52577 = CARTESIAN_POINT ( 'NONE',  ( 0.000000000000000000, -76.29999999999999716, 0.000000000000000000 ) ) ;
#52578 = DIRECTION ( 'NONE',  ( 0.000000000000000000, 1.000000000000000000, 0.000000000000000000 ) ) ;
#52579 = FACE_OUTER_BOUND ( 'NONE', #11543, .T. ) ;
#52580 = CARTESIAN_POINT ( 'NONE',  ( -7.641012305223999768, -18.71082276572999703, 10.18589226631999978 ) ) ;
#52581 = CARTESIAN_POINT ( 'NONE',  ( -4.348661115406000199, -79.15007827033099375, -10.27524920185999946 ) ) ;
#52582 = CARTESIAN_POINT ( 'NONE',  ( -9.431729376590999081, -76.99603667140100072, 1.293989273348000069 ) ) ;
#52583 = CARTESIAN_POINT ( 'NONE',  ( -12.00000000000000000, -78.79999999999999716, 0.000000000000000000 ) ) ;
#52584 = B_SPLINE_CURVE_WITH_KNOTS ( 'NONE', 3,
 ( #65, #32174, #50214, #31294, #54059, #41349 ),
 .UNSPECIFIED., .F., .F.,
 ( 4, 1, 1, 4 ),
 ( 0.000000000000000000, 0.3333333311524483422, 0.6666666623049967155, 0.9999999934574449467 ),
 .UNSPECIFIED. ) ;
#52585 =( NAMED_UNIT ( * ) PLANE_ANGLE_UNIT ( ) SI_UNIT ( $, .RADIAN. ) );
#52586 = CARTESIAN_POINT ( 'NONE',  ( -2.166177946181000902, -80.00000000000000000, 9.033216284371517801 ) ) ;
#52587 = ORIENTED_EDGE ( 'NONE', *, *, #12618, .T. ) ;
#52588 = CARTESIAN_POINT ( 'NONE',  ( -1.553390134080000040, -82.86361845526398895, -0.6977077157647000316 ) ) ;
#52589 = CARTESIAN_POINT ( 'NONE',  ( -0.8477325451633000997, -79.46775351646000729, -1.148851298854000058 ) ) ;
#52590 = CARTESIAN_POINT ( 'NONE',  ( 10.75000000000000000, -79.35000000000000853, 0.000000000000000000 ) ) ;
#52591 = CARTESIAN_POINT ( 'NONE',  ( 6.444980599754999595, -77.73630943762100287, -10.09843005143000028 ) ) ;
#52592 = LINE ( 'NONE', #39863, #44791 ) ;
#52593 = CARTESIAN_POINT ( 'NONE',  ( 1.431241028886999889, -81.41842548529999135, -0.8524881072380000591 ) ) ;
#52594 = CARTESIAN_POINT ( 'NONE',  ( -1.419463091678716093, -2.342021354265884536, -3.223257765105098649 ) ) ;
#52595 = CARTESIAN_POINT ( 'NONE',  ( -0.6471704932797999188, -78.07045584965399598, 9.701898969124000516 ) ) ;
#52596 = CARTESIAN_POINT ( 'NONE',  ( 4.603815134758999505, -77.24485258715699842, -8.210729597153999748 ) ) ;
#52597 = CARTESIAN_POINT ( 'NONE',  ( -11.00000000000000000, -79.19999999999998863, 0.000000000000000000 ) ) ;
#52598 = CARTESIAN_POINT ( 'NONE',  ( -7.710118476707999768, -21.74977139563000250, 10.18499221085999906 ) ) ;
#52599 = CARTESIAN_POINT ( 'NONE',  ( 9.977465883888395837, -75.99422917656416132, 6.207251457660701632 ) ) ;
#52600 = CARTESIAN_POINT ( 'NONE',  ( -1.052442226633345967, -82.19782380993190429, -0.7179146240541253166 ) ) ;
#52601 = EDGE_LOOP ( 'NONE', ( #32050, #35092, #28875, #54808, #19379, #24293 ) ) ;
#52602 = CARTESIAN_POINT ( 'NONE',  ( 2.421167930323313566, -78.85416666666664298, 9.009247259181924150 ) ) ;
#52603 = CARTESIAN_POINT ( 'NONE',  ( 0.000000000000000000, -75.00000000000000000, -7.200000000000000178 ) ) ;
#52604 = CARTESIAN_POINT ( 'NONE',  ( 11.01099501428000060, -79.54020879888699369, -5.416862536834000430 ) ) ;
#52605 = AXIS2_PLACEMENT_3D ( 'NONE', #55233, #6220, #10083 ) ;
#52606 = CARTESIAN_POINT ( 'NONE',  ( -4.043785186575957091, -78.69999999999998863, -2.284879765406314878 ) ) ;
#52607 = CARTESIAN_POINT ( 'NONE',  ( -0.5544740949720999845, -82.23160949924999841, 1.570928860995999932 ) ) ;
#52608 = CARTESIAN_POINT ( 'NONE',  ( 2.550499813263000348, -78.51351126778098433, -10.67515654612000020 ) ) ;
#52609 = CARTESIAN_POINT ( 'NONE',  ( 9.641208724080000181, -24.43394297700999829, -7.943747389698999406 ) ) ;
#52610 = CARTESIAN_POINT ( 'NONE',  ( -0.2584144826940477091, -16.77154603077345385, 12.70558781487939015 ) ) ;
#52611 = CARTESIAN_POINT ( 'NONE',  ( -12.36772659745999903, -76.93670025537799972, 0.6901808088037000299 ) ) ;
#52612 = FACE_OUTER_BOUND ( 'NONE', #41561, .T. ) ;
#52613 = CARTESIAN_POINT ( 'NONE',  ( -8.620921568068807161, -61.96528830388043474, 9.346042573940106735 ) ) ;
#52614 = ORIENTED_EDGE ( 'NONE', *, *, #51404, .F. ) ;
#52615 = CARTESIAN_POINT ( 'NONE',  ( 2.277702604431000033, -78.28268586533900475, -10.79414087890000040 ) ) ;
#52616 = CARTESIAN_POINT ( 'NONE',  ( -0.8849959507268040371, -80.03812507728116543, 0.8823318837302972506 ) ) ;
#52617 = DIRECTION ( 'NONE',  ( -0.7071067811864980568, 0.7071067811865969777, -1.033897857523995979E-10 ) ) ;
#52618 = CARTESIAN_POINT ( 'NONE',  ( 7.994753734545000157, -78.49140324543799352, 7.938063182512999916 ) ) ;
#52619 = CARTESIAN_POINT ( 'NONE',  ( 0.000000000000000000, -75.09999999996229292, 0.000000000000000000 ) ) ;
#52620 = CARTESIAN_POINT ( 'NONE',  ( 11.75000000000000000, -77.54999999999999716, 2.316376715183999699E-14 ) ) ;
#52621 = CARTESIAN_POINT ( 'NONE',  ( -1.980584515756000030, -18.73514849905999924, 12.76303204340999997 ) ) ;
#52622 = CARTESIAN_POINT ( 'NONE',  ( -0.6952495977537009875, -82.76231604831681921, 1.343821088991839607 ) ) ;
#52623 = CARTESIAN_POINT ( 'NONE',  ( 0.8926277122277624931, -79.78871733315683912, -0.8747132943431308316 ) ) ;
#52624 = CARTESIAN_POINT ( 'NONE',  ( 4.044903269867999640, -79.05999999999998806, -8.595856998426999240 ) ) ;
#52625 = DIRECTION ( 'NONE',  ( 1.586878776513000076E-12, 1.000000000000000000, -3.446046439139999930E-10 ) ) ;
#52626 = EDGE_CURVE ( 'NONE', #38602, #46260, #36826, .T. ) ;
#52627 = CARTESIAN_POINT ( 'NONE',  ( -12.49989425040000057, -23.19225390461999936, 1.666425739591000044 ) ) ;
#52628 = VERTEX_POINT ( 'NONE', #22757 ) ;
#52629 = VERTEX_POINT ( 'NONE', #10065 ) ;
#52630 = CARTESIAN_POINT ( 'NONE',  ( -12.72554264789000023, -55.59839278072999491, -1.930240062458999928 ) ) ;
#52631 = ORIENTED_EDGE ( 'NONE', *, *, #3718, .T. ) ;
#52632 = ORIENTED_EDGE ( 'NONE', *, *, #21021, .F. ) ;
#52633 = CARTESIAN_POINT ( 'NONE',  ( 10.53559655517000060, -23.20569178316999981, 7.620036226160999959 ) ) ;
#52634 = FACE_OUTER_BOUND ( 'NONE', #34394, .T. ) ;
#52635 = CONTEXT_DEPENDENT_SHAPE_REPRESENTATION ( #57169, #9781 ) ;
#52636 = AXIS2_PLACEMENT_3D ( 'NONE', #39193, #11770, #52496 ) ;
#52637 = CARTESIAN_POINT ( 'NONE',  ( -9.721629130303000466, -78.68311332859899210, 1.228127365514999791 ) ) ;
#52638 = CARTESIAN_POINT ( 'NONE',  ( -4.686723500388265684, -79.41694709479033065, 8.065566475210284025 ) ) ;
#52639 = EDGE_CURVE ( 'NONE', #20634, #670, #22463, .T. ) ;
#52640 = ORIENTED_EDGE ( 'NONE', *, *, #46100, .T. ) ;
#52641 = ORIENTED_EDGE ( 'NONE', *, *, #23368, .T. ) ;
#52642 = CARTESIAN_POINT ( 'NONE',  ( -5.179006628193274508, -77.52228172415060214, 7.668103985437277004 ) ) ;
#52643 = CARTESIAN_POINT ( 'NONE',  ( 10.07768261906999996, -78.02607137478699428, -4.508174471003999706 ) ) ;
#52644 = CARTESIAN_POINT ( 'NONE',  ( -12.54987272481000105, -61.85113590103000547, -0.1385846084898000041 ) ) ;
#52645 = CARTESIAN_POINT ( 'NONE',  ( -9.346518596363001308, -77.80847978158598721, 2.610229778083999808 ) ) ;
#52646 = CARTESIAN_POINT ( 'NONE',  ( 7.691916945430000041, -20.24634220924000161, 10.42274798266999980 ) ) ;
#52647 = AXIS2_PLACEMENT_3D ( 'NONE', #9515, #19246, #14801 ) ;
#52648 = DIRECTION ( 'NONE',  ( 0.9999463328794432337, 0.000000000000000000, -0.01036008498777044214 ) ) ;
#52649 = CARTESIAN_POINT ( 'NONE',  ( 9.689263856727277968, -53.82111184930475645, -8.274777958929785626 ) ) ;
#52650 = CARTESIAN_POINT ( 'NONE',  ( -7.054457466615000172, -80.50123988683198206, -8.769379688592000122 ) ) ;
#52651 = CARTESIAN_POINT ( 'NONE',  ( 12.72558083409999874, -18.79866855842000106, -1.930284430576000076 ) ) ;
#52652 = CARTESIAN_POINT ( 'NONE',  ( -0.7681833999686432657, -81.07291666666668561, -0.9995835529977258327 ) ) ;
#52653 = ORIENTED_EDGE ( 'NONE', *, *, #51849, .F. ) ;
#52654 = CARTESIAN_POINT ( 'NONE',  ( -9.310166272052999403, -53.66468533943000097, 8.596757084861000209 ) ) ;
#52655 = CARTESIAN_POINT ( 'NONE',  ( -1.835125225091999823, -78.08892106756400153, 11.83842809849000055 ) ) ;
#52656 = EDGE_CURVE ( 'NONE', #44781, #52628, #28045, .T. ) ;
#52657 = CARTESIAN_POINT ( 'NONE',  ( -9.108265402975000313, -17.12189187203999907, -8.478706101062000400 ) ) ;
#52658 = B_SPLINE_CURVE_WITH_KNOTS ( 'NONE', 3,
 ( #8151, #3717, #36466, #13440, #18187, #54493, #39725, #44450, #30855, #9323, #45346, #13145, #26428, #27315, #22895, #17590, #26723, #48893 ),
 .UNSPECIFIED., .F., .F.,
 ( 4, 2, 2, 2, 2, 2, 2, 2, 4 ),
 ( 0.000000000000000000, 0.1250000000000000000, 0.2500000000000000000, 0.3750000000000000000, 0.5000000000000000000, 0.6250000000000000000, 0.7500000000000000000, 0.8750000000000000000, 1.000000000000000000 ),
 .UNSPECIFIED. ) ;
#52660 = CARTESIAN_POINT ( 'NONE',  ( -1.669724228656999987, -18.63102323466000243, -12.48434610067999984 ) ) ;
#52659 = CARTESIAN_POINT ( 'NONE',  ( 7.396983374551519219, -78.40212121928816202, 5.684573788064898103 ) ) ;
#52661 = LINE ( 'NONE', #47681, #40196 ) ;
#52662 = CARTESIAN_POINT ( 'NONE',  ( -5.049388770360000223, -80.08077773488000162, -9.976713590530000175 ) ) ;
#52663 = DIRECTION ( 'NONE',  ( -1.000000000000000000, 0.000000000000000000, 0.000000000000000000 ) ) ;
#52664 = CARTESIAN_POINT ( 'NONE',  ( 9.107239040596999402, -78.12345696174899956, 6.625115969983998987 ) ) ;
#52665 = DIRECTION ( 'NONE',  ( 0.9999999923520045408, 0.000000000000000000, 0.0001236769620550006593 ) ) ;
#52666 = CARTESIAN_POINT ( 'NONE',  ( 10.71369944335147117, -79.97083333333559096, 2.879226727952105769 ) ) ;
#52667 = ORIENTED_EDGE ( 'NONE', *, *, #21785, .T. ) ;
#52668 = CARTESIAN_POINT ( 'NONE',  ( 7.711243899566646576, -80.31159779477867744, 7.536022382359885086 ) ) ;
#52669 = CARTESIAN_POINT ( 'NONE',  ( -12.52582323437078493, -60.60939730725204555, 1.680974276192793271 ) ) ;
#52670 = CARTESIAN_POINT ( 'NONE',  ( -12.69616050747999836, -20.24828923609000242, 1.799475304559999822 ) ) ;
#52671 = CARTESIAN_POINT ( 'NONE',  ( -2.434124730054000096, -3.288321030359000474, -2.925889700817000172 ) ) ;
#52672 = CARTESIAN_POINT ( 'NONE',  ( -8.130813118348999780, -54.11476110100999648, 9.546856411314999846 ) ) ;
#52673 = CARTESIAN_POINT ( 'NONE',  ( -2.577533092820055494, -77.20624999999999716, -10.72859319707154668 ) ) ;
#52674 = DIRECTION ( 'NONE',  ( 1.000000000000000000, 0.000000000000000000, 0.000000000000000000 ) ) ;
#52675 = FACE_OUTER_BOUND ( 'NONE', #55733, .T. ) ;
#52676 = CARTESIAN_POINT ( 'NONE',  ( 1.224658201351000120, -84.55471544543098616, 3.769110384959000193 ) ) ;
#52677 = CIRCLE ( 'NONE', #41379, 1.000000000000000000 ) ;
#52678 = DIRECTION ( 'NONE',  ( 0.9999999999999693578, 2.479738204331925575E-07, 1.114546890695966335E-12 ) ) ;
#52679 = DIRECTION ( 'NONE',  ( 0.7071067811865474617, -0.7071067811865474617, 8.138997328409543352E-11 ) ) ;
#52680 = CARTESIAN_POINT ( 'NONE',  ( 7.265900323201000433, -77.62487771236999379, 8.333956192971999855 ) ) ;
#52681 = CARTESIAN_POINT ( 'NONE',  ( 9.641515966524812242, -76.40113284977830688, -6.715584340997621027 ) ) ;
#52682 = CARTESIAN_POINT ( 'NONE',  ( -10.98551332331999930, -76.63383956207499637, 1.010146990136999934 ) ) ;
#52683 = CARTESIAN_POINT ( 'NONE',  ( 1.153057336080759665, -81.88161975503362555, 0.4825267112434911687 ) ) ;
#52684 = CARTESIAN_POINT ( 'NONE',  ( 1.162132110709999999, -79.14348019970999815, 1.190372713651999925 ) ) ;
#52685 = CARTESIAN_POINT ( 'NONE',  ( 7.764258067048000811, -77.07068982153518277, 5.767450660628000492 ) ) ;
#52686 = CARTESIAN_POINT ( 'NONE',  ( -1.199500263597274685, -78.94791666666668561, 0.9218200799623673669 ) ) ;
#52687 = DIRECTION ( 'NONE',  ( 1.000000000000000000, 0.000000000000000000, 0.000000000000000000 ) ) ;
#52688 = CARTESIAN_POINT ( 'NONE',  ( -2.021764786808774250, -80.21014581661567888, -10.55807976612607391 ) ) ;
#52689 = CARTESIAN_POINT ( 'NONE',  ( 0.000000000000000000, -51.86282895648000135, 0.000000000000000000 ) ) ;
#52690 = CARTESIAN_POINT ( 'NONE',  ( -8.382314651691611829, -79.90774747778513643, -7.453751407507572146 ) ) ;
#52691 = AXIS2_PLACEMENT_3D ( 'NONE', #41307, #1758, #19168 ) ;
#52692 = CARTESIAN_POINT ( 'NONE',  ( -11.15966350340000091, -79.53565934156199546, 4.490997254915999548 ) ) ;
#52693 = EDGE_CURVE ( 'NONE', #21397, #32631, #14761, .T. ) ;
#52694 = CARTESIAN_POINT ( 'NONE',  ( 0.3271848554490964789, -81.85416666666667140, 1.217465845835395521 ) ) ;
#52695 = CARTESIAN_POINT ( 'NONE',  ( -9.103325846391999931, -78.87350394595299008, -6.630491919364000175 ) ) ;
#52696 = CARTESIAN_POINT ( 'NONE',  ( -1.135826688880000157, -81.30663953507000485, -0.9797437077257000748 ) ) ;
#52697 = EDGE_LOOP ( 'NONE', ( #4964, #36774, #31474, #49512 ) ) ;
#52698 = ADVANCED_FACE ( 'NONE', ( #37202 ), #27464, .F. ) ;
#52699 = CARTESIAN_POINT ( 'NONE',  ( -10.31421052434999908, -76.82175206120300004, 3.823226550887000030 ) ) ;
#52700 = ORIENTED_EDGE ( 'NONE', *, *, #27992, .F. ) ;
#52701 = EDGE_LOOP ( 'NONE', ( #2477, #42986, #45076, #45887, #35909 ) ) ;
#52702 = FACE_OUTER_BOUND ( 'NONE', #23287, .T. ) ;
#52703 = SURFACE_STYLE_USAGE ( .BOTH. , #57700 ) ;
#52704 = ORIENTED_EDGE ( 'NONE', *, *, #42399, .T. ) ;
#52705 = CARTESIAN_POINT ( 'NONE',  ( 3.006299185876999847, -79.77631457584399755, 1.961099271341999684 ) ) ;
#52706 = CARTESIAN_POINT ( 'NONE',  ( -2.938756882413333660, -79.29986081116008734, 9.035730373227549350 ) ) ;
#52707 = VERTEX_POINT ( 'NONE', #13895 ) ;
#52709 = EDGE_CURVE ( 'NONE', #1475, #56551, #22611, .T. ) ;
#52708 = CARTESIAN_POINT ( 'NONE',  ( 11.88041277708999921, -79.15000486637001131, -2.818394331568000233 ) ) ;
#52710 = VERTEX_POINT ( 'NONE', #54922 ) ;
#52711 = CARTESIAN_POINT ( 'NONE',  ( -7.640030264173999441, -60.10716680829000325, 10.18491080495000034 ) ) ;
#52712 = CARTESIAN_POINT ( 'NONE',  ( -12.70556836352000118, -62.02772277195000328, -2.424224025342999716E-09 ) ) ;
#52713 = ORIENTED_EDGE ( 'NONE', *, *, #9775, .T. ) ;
#52714 = CARTESIAN_POINT ( 'NONE',  ( -3.206516299415000049, -1.613032031399000088, -0.5298615117031000299 ) ) ;
#52715 = CARTESIAN_POINT ( 'NONE',  ( 3.670166320769038037, -79.79999999999999716, 11.34743833829017490 ) ) ;
#52716 = CARTESIAN_POINT ( 'NONE',  ( -10.21315268674774757, -80.07477733434343747, 3.354632155474256194 ) ) ;
#52717 = DIRECTION ( 'NONE',  ( 0.000000000000000000, 0.000000000000000000, -1.000000000000000000 ) ) ;
#52718 = CIRCLE ( 'NONE', #1825, 5.299999999999999822 ) ;
#52719 = CARTESIAN_POINT ( 'NONE',  ( -3.972981440171656331, -86.25171435493597016, -0.3803130624956269634 ) ) ;
#52720 = CARTESIAN_POINT ( 'NONE',  ( 4.903943924252999409, -76.49501613320700244, -10.05113017056000047 ) ) ;
#52721 = CARTESIAN_POINT ( 'NONE',  ( -8.848566283551813072, -79.08854166669489416, 7.961923423609528427 ) ) ;
#52722 = CARTESIAN_POINT ( 'NONE',  ( 6.760013919724038978, -78.52291666666666003, 8.796335266380001627 ) ) ;
#52723 = CARTESIAN_POINT ( 'NONE',  ( 7.649879603444000864, -76.64506733076500211, -7.903239737143000987 ) ) ;
#52724 = CYLINDRICAL_SURFACE ( 'NONE', #14277, 1.750000000000001332 ) ;
#52725 = CARTESIAN_POINT ( 'NONE',  ( -0.8465867926663999121, -80.74519081100000051, -0.9556525628790000226 ) ) ;
#52726 = AXIS2_PLACEMENT_3D ( 'NONE', #30798, #8969, #39956 ) ;
#52727 = DIRECTION ( 'NONE',  ( -1.000000000000000000, 0.000000000000000000, 0.000000000000000000 ) ) ;
#52728 = CARTESIAN_POINT ( 'NONE',  ( 0.7997484141426716153, -2.956625672363701440, 3.150668280190185300 ) ) ;
#52729 = CARTESIAN_POINT ( 'NONE',  ( -3.478367431019000033, -78.68975264934786651, -0.6823414571583998889 ) ) ;
#52730 = AXIS2_PLACEMENT_3D ( 'NONE', #39693, #12822, #17255 ) ;
#52731 = CARTESIAN_POINT ( 'NONE',  ( -9.369164850722000892, -23.25000000000000000, 7.601397897754999633 ) ) ;
#52732 = CARTESIAN_POINT ( 'NONE',  ( 1.271183301036420188, -80.96600668877975693, 10.67466081527704880 ) ) ;
#52733 = CARTESIAN_POINT ( 'NONE',  ( -3.306603397031000036, -83.34449735065199150, -1.277238313581000151 ) ) ;
#52734 = CARTESIAN_POINT ( 'NONE',  ( 1.911540947291000103, -3.115794354202999994, 3.291214574437999918 ) ) ;
#52735 = LINE ( 'NONE', #29697, #26115 ) ;
#52736 = LINE ( 'NONE', #3433, #57394 ) ;
#52737 = CARTESIAN_POINT ( 'NONE',  ( -8.300970689365467337, -78.35833333333332007, 4.784380313523513450 ) ) ;
#52738 = CARTESIAN_POINT ( 'NONE',  ( 0.7341740840635999632, -80.89327854953300800, -1.113348630318000021 ) ) ;
#52739 = CARTESIAN_POINT ( 'NONE',  ( -7.470012560788926947, -78.95333333333331893, -5.923033143556039271 ) ) ;
#52740 = FACE_OUTER_BOUND ( 'NONE', #10030, .T. ) ;
#52741 = ADVANCED_FACE ( 'NONE', ( #45502 ), #32179, .T. ) ;
#52742 = CARTESIAN_POINT ( 'NONE',  ( 1.439896632895334649, -79.83541666666666003, -10.99999999999999822 ) ) ;
#52743 = DIRECTION ( 'NONE',  ( -0.7071067811865470176, -0.7071067811865470176, -3.647649194621239524E-08 ) ) ;
#52744 = CARTESIAN_POINT ( 'NONE',  ( 12.30184311661000152, -75.83932607782000446, 1.220056246972000213 ) ) ;
#52745 = ORIENTED_EDGE ( 'NONE', *, *, #51594, .F. ) ;
#52746 = CARTESIAN_POINT ( 'NONE',  ( -12.00000000000000000, -18.75000000000000000, -1.750000000000000000 ) ) ;
#52747 = CARTESIAN_POINT ( 'NONE',  ( 8.023850137665998972, -80.46368584346849673, -8.105891195326000442 ) ) ;
#52748 = CARTESIAN_POINT ( 'NONE',  ( 12.59682790095999927, -60.18734115192999923, 1.801645751184999922 ) ) ;
#52749 = FACE_OUTER_BOUND ( 'NONE', #26743, .T. ) ;
#52750 = CARTESIAN_POINT ( 'NONE',  ( -7.648940337505000464, -77.44503301142398755, -5.852081988952999581 ) ) ;
#52751 = CARTESIAN_POINT ( 'NONE',  ( -4.136849130093000149, -83.11125530066698275, 0.5622182541971000314 ) ) ;
#52752 = CARTESIAN_POINT ( 'NONE',  ( 2.721914423158461549, -79.95511695915216421, 10.40824526415593176 ) ) ;
#52753 = CARTESIAN_POINT ( 'NONE',  ( -1.341023944040999893, -79.11523479771300060, -0.2092349045463000046 ) ) ;
#52754 = ORIENTED_EDGE ( 'NONE', *, *, #49397, .T. ) ;
#52755 = CARTESIAN_POINT ( 'NONE',  ( 0.000000000000000000, -76.75499999999999545, 0.000000000000000000 ) ) ;
#52756 = CARTESIAN_POINT ( 'NONE',  ( 0.6811966951781786017, -82.14583333333094117, 1.183578528101640437 ) ) ;
#52757 = CARTESIAN_POINT ( 'NONE',  ( -3.621447497675000182, -78.99318692614357929, -1.519545876029819695E-14 ) ) ;
#52758 = EDGE_LOOP ( 'NONE', ( #56380, #48223, #40165, #34671 ) ) ;
#52759 = CARTESIAN_POINT ( 'NONE',  ( -2.162167942093999873, -78.26164515279698719, 10.72440421974000024 ) ) ;
#52760 = CARTESIAN_POINT ( 'NONE',  ( -7.387512494710283484, -55.38467666605774298, -8.150146600852353984 ) ) ;
#52761 = CARTESIAN_POINT ( 'NONE',  ( -1.645926171036000030, -80.41978745972699016, -10.69587012110999780 ) ) ;
#52762 = EDGE_LOOP ( 'NONE', ( #9904, #53339, #39978, #1447 ) ) ;
#52763 = EDGE_CURVE ( 'NONE', #46715, #26175, #14183, .T. ) ;
#52764 = ORIENTED_EDGE ( 'NONE', *, *, #18223, .T. ) ;
#52765 = B_SPLINE_CURVE_WITH_KNOTS ( 'NONE', 3,
 ( #55256, #37533, #54965, #19538 ),
 .UNSPECIFIED., .F., .F.,
 ( 4, 4 ),
 ( 0.000000000000000000, 1.000000000000000000 ),
 .UNSPECIFIED. ) ;
#52766 = ORIENTED_EDGE ( 'NONE', *, *, #57025, .T. ) ;
#52767 = AXIS2_PLACEMENT_3D ( 'NONE', #56690, #20671, #16248 ) ;
#52768 = DIRECTION ( 'NONE',  ( 0.000000000000000000, -1.000000000000000000, 0.000000000000000000 ) ) ;
#52769 = CARTESIAN_POINT ( 'NONE',  ( -3.654181822837000215, -86.09999999943198645, 1.626946589673999854 ) ) ;
#52770 = CARTESIAN_POINT ( 'NONE',  ( 7.919595949288999570, -59.94999999967000548, 9.050966799188000067 ) ) ;
#52771 = VERTEX_POINT ( 'NONE', #50219 ) ;
#52773 = EDGE_CURVE ( 'NONE', #21248, #45320, #9767, .T. ) ;
#52772 = CARTESIAN_POINT ( 'NONE',  ( -12.70556836347999941, -25.22772277227999993, -2.424223956931999920E-09 ) ) ;
#52774 = ORIENTED_EDGE ( 'NONE', *, *, #12032, .T. ) ;
#52775 = CARTESIAN_POINT ( 'NONE',  ( -10.75045394575212399, -80.61043716274458859, -1.406899836902645973 ) ) ;
#52776 = EDGE_CURVE ( 'NONE', #39540, #13397, #33999, .T. ) ;
#52777 = CARTESIAN_POINT ( 'NONE',  ( -2.171318179221914058, -78.99318692614359350, -3.601143365367586835 ) ) ;
#52778 = CARTESIAN_POINT ( 'NONE',  ( 7.636247231009999581, -55.03676232846999739, 10.30460520059999929 ) ) ;
#52779 = CARTESIAN_POINT ( 'NONE',  ( -0.9218200799623778030, -81.32708333333334849, 1.199500263597266914 ) ) ;
#52780 = CARTESIAN_POINT ( 'NONE',  ( 7.169814592847524537, -77.37462369211782232, -9.346328727328229391 ) ) ;
#52781 = CARTESIAN_POINT ( 'NONE',  ( 1.949527607922329819, -80.21094325140447268, 11.04011390166788686 ) ) ;
#52782 = LINE ( 'NONE', #33891, #44163 ) ;
#52783 = LINE ( 'NONE', #49228, #10546 ) ;
#52784 = CIRCLE ( 'NONE', #57494, 0.6000000000000008660 ) ;
#52785 = CARTESIAN_POINT ( 'NONE',  ( -7.619389973898000434, -23.40786254230999930, 10.35398617733999949 ) ) ;
#52786 = CARTESIAN_POINT ( 'NONE',  ( 4.163343027946999619, -79.41125264934790096, 0.3101205329980999403 ) ) ;
#52787 = CARTESIAN_POINT ( 'NONE',  ( 9.468102369896000070, -78.02648667140100258, 2.380303120989999854 ) ) ;
#52788 = CARTESIAN_POINT ( 'NONE',  ( -12.65987793663000005, -17.06302453494999583, 0.9847129294438998759 ) ) ;
#52789 = CARTESIAN_POINT ( 'NONE',  ( 13.94827586207000003, -33.10361340872000113, 8.082385094115998871E-06 ) ) ;
#52790 = CARTESIAN_POINT ( 'NONE',  ( -6.620362748380999918, -76.07801071496099610, -10.34376132320999986 ) ) ;
#52791 = CARTESIAN_POINT ( 'NONE',  ( 11.00000000000000000, -79.84999999999999432, 0.000000000000000000 ) ) ;
#52792 = CARTESIAN_POINT ( 'NONE',  ( 7.943839548388014649, -78.36782549339653769, 9.082008725015928263 ) ) ;
#52793 = CARTESIAN_POINT ( 'NONE',  ( -11.75000000000000000, -78.29999999999999716, 0.000000000000000000 ) ) ;
#52794 = CARTESIAN_POINT ( 'NONE',  ( 0.01767233353438701221, -80.37544597895652032, -1.546831932022704414 ) ) ;
#52795 = CARTESIAN_POINT ( 'NONE',  ( -9.289856196000998878, -77.44054472353899143, 1.941241007807000152 ) ) ;
#52796 = CARTESIAN_POINT ( 'NONE',  ( -0.2914033309752999679, -79.01861702419900269, -1.588174433604999880 ) ) ;
#52797 = CARTESIAN_POINT ( 'NONE',  ( 0.7554284705563509839, -78.66666666666667140, -1.310679582531385945 ) ) ;
#52798 = CARTESIAN_POINT ( 'NONE',  ( -1.952863295937999899, -3.631957716005000059, -2.785027970207999637 ) ) ;
#52799 = EDGE_CURVE ( 'NONE', #42112, #26696, #41551, .T. ) ;
#52800 = CONICAL_SURFACE ( 'NONE', #57510, 9.649999999909001147, 0.7853981633972997312 ) ;
#52801 = CARTESIAN_POINT ( 'NONE',  ( 5.675825126306000001, -78.71017368086199895, 10.88946240266999865 ) ) ;
#52802 = CARTESIAN_POINT ( 'NONE',  ( 0.9218200799623694763, -80.82291666666668561, 1.199500263597272465 ) ) ;
#52804 = CARTESIAN_POINT ( 'NONE',  ( -0.8575312565364999751, -77.81063687001270068, -1.002634541711000082 ) ) ;
#52803 = CARTESIAN_POINT ( 'NONE',  ( -11.75000000000000000, -75.80000000000001137, -9.948686767780999254E-14 ) ) ;
#52805 = CARTESIAN_POINT ( 'NONE',  ( -1.167634245779999969, -83.18220886491398858, -0.6204341648412000643 ) ) ;
#52806 = CARTESIAN_POINT ( 'NONE',  ( -7.294926994005753507, -79.53446014010890508, 7.905947034046361566 ) ) ;
#52807 = VERTEX_POINT ( 'NONE', #37788 ) ;
#52808 = ADVANCED_FACE ( 'NONE', ( #33643 ), #34, .F. ) ;
#52809 = CARTESIAN_POINT ( 'NONE',  ( -7.608356748847192819, -78.82937652759582647, 9.340614718762003221 ) ) ;
#52810 = CARTESIAN_POINT ( 'NONE',  ( -9.494208634449000428, -79.13841836158600529, 7.406230482228999712 ) ) ;
#52811 = CARTESIAN_POINT ( 'NONE',  ( -9.226371719725817044, -79.26948592758979828, -2.305846157194820112 ) ) ;
#52812 = CARTESIAN_POINT ( 'NONE',  ( -8.454756037848037309, -79.99999999999997158, -3.909103053904156688 ) ) ;
#52813 = DIRECTION ( 'NONE',  ( -0.7071067811864976127, 0.7071067811865975328, 1.603636560452993712E-09 ) ) ;
#52814 = CARTESIAN_POINT ( 'NONE',  ( 0.007921339454490000653, -0.9192005770255999852, 3.538571077850000357 ) ) ;
#52815 = CARTESIAN_POINT ( 'NONE',  ( -5.346700182771000343, -80.12992104470397692, 7.765585233270999588 ) ) ;
#52816 = DIRECTION ( 'NONE',  ( 0.000000000000000000, 0.000000000000000000, 1.000000000000000000 ) ) ;
#52817 = CARTESIAN_POINT ( 'NONE',  ( 9.009247259181924150, -79.22916666666665719, -2.421167930323326001 ) ) ;
#52818 = ORIENTED_EDGE ( 'NONE', *, *, #33002, .F. ) ;
#52819 = CARTESIAN_POINT ( 'NONE',  ( -12.70228859449707493, -53.97803615216450623, 1.213484947725372409 ) ) ;
#52820 = CARTESIAN_POINT ( 'NONE',  ( -12.56594317825999951, -60.05000001354000005, 1.750000000000000000 ) ) ;
#52821 = CARTESIAN_POINT ( 'NONE',  ( -1.680996261629376765, -1.683444032095494869, -2.810092171514073200 ) ) ;
#52822 = CARTESIAN_POINT ( 'NONE',  ( -1.199500263597270244, -78.45208333333333428, -0.9218200799623728070 ) ) ;
#52823 = CARTESIAN_POINT ( 'NONE',  ( -1.570423240223999928, -80.85668197030999238, -0.5559045111934000083 ) ) ;
#52824 = ORIENTED_EDGE ( 'NONE', *, *, #13655, .F. ) ;
#52825 = CIRCLE ( 'NONE', #44347, 0.5999999999999999778 ) ;
#52826 = CARTESIAN_POINT ( 'NONE',  ( 10.97031909684999995, -77.66693593946899909, -1.702279910903999882 ) ) ;
#52827 = CARTESIAN_POINT ( 'NONE',  ( 0.5668640707187667660, -53.88340304924094681, -12.50470739225058736 ) ) ;
#52828 = CARTESIAN_POINT ( 'NONE',  ( -1.749899258081046627, -55.41283151199903045, -12.55433901288159326 ) ) ;
#52829 = B_SPLINE_CURVE_WITH_KNOTS ( 'NONE', 3,
 ( #5292, #23300, #41309, #54881, #11486, #42774, #20901, #56923, #33886, #7614, #24759, #52209, #2336, #20620, #34461, #52492, #38904, #16482, #25327, #20331, #2900, #29458, #16195, #38326 ),
 .UNSPECIFIED., .F., .F.,
 ( 4, 2, 2, 2, 2, 2, 2, 2, 2, 2, 2, 4 ),
 ( 0.000000000000000000, 0.1249999999999984457, 0.2499999999999968914, 0.3749999999999953371, 0.4374999999999954481, 0.4999999999999955591, 0.6249999999999957812, 0.7499999999999960032, 0.8124999999999968914, 0.8437499999999971134, 0.8749999999999974465, 1.000000000000000000 ),
 .UNSPECIFIED. ) ;
#52830 = CARTESIAN_POINT ( 'NONE',  ( -12.71798269383000068, -55.50221245779999890, 1.931086388578000079 ) ) ;
#52831 = CARTESIAN_POINT ( 'NONE',  ( 0.9995835529977233902, -78.30208333333332860, 0.7681833999686461523 ) ) ;
#52832 = B_SPLINE_CURVE_WITH_KNOTS ( 'NONE', 3,
 ( #28919, #37485, #46672, #6784, #46963, #5612, #33637, #51679, #42229, #18911, #29206, #1214, #931, #36904, #54918, #6197, #37197, #1501 ),
 .UNSPECIFIED., .F., .F.,
 ( 4, 2, 2, 2, 2, 2, 2, 2, 4 ),
 ( 0.000000000000000000, 0.1249999999999999167, 0.2499999999999998335, 0.3749999999999998335, 0.4999999999999998890, 0.6249999999999998890, 0.7499999999999998890, 0.8750000000000000000, 1.000000000000000000 ),
 .UNSPECIFIED. ) ;
#52833 = CARTESIAN_POINT ( 'NONE',  ( 12.74365836111949335, -55.27810168850018613, -1.980611005600377617 ) ) ;
#52834 = VERTEX_POINT ( 'NONE', #27977 ) ;
#52835 = VERTEX_POINT ( 'NONE', #32115 ) ;
#52837 = EDGE_CURVE ( 'NONE', #23718, #9803, #45215, .T. ) ;
#52836 = CARTESIAN_POINT ( 'NONE',  ( 4.405607986419999733, -76.98004247776398756, -11.79252213402000038 ) ) ;
#52838 = FACE_OUTER_BOUND ( 'NONE', #47147, .T. ) ;
#52839 = EDGE_CURVE ( 'NONE', #2738, #2249, #57834, .T. ) ;
#52840 = ORIENTED_EDGE ( 'NONE', *, *, #29472, .T. ) ;
#52841 = CARTESIAN_POINT ( 'NONE',  ( 12.52582254647517424, -18.19059700816731961, 1.680974932934241606 ) ) ;
#52842 = AXIS2_PLACEMENT_3D ( 'NONE', #7094, #43116, #11246 ) ;
#52843 = CARTESIAN_POINT ( 'NONE',  ( 2.260129142450393758, -78.99361093726523109, -9.437459368857011199 ) ) ;
#52844 = AXIS2_PLACEMENT_3D ( 'NONE', #47704, #7234, #25238 ) ;
#52845 = CARTESIAN_POINT ( 'NONE',  ( 0.2678032735624597538, -53.58567224682256835, 12.70526550765059248 ) ) ;
#52846 = CARTESIAN_POINT ( 'NONE',  ( 12.36191581903000092, -76.89772347022000076, -3.311046255921999748 ) ) ;
#52847 = CARTESIAN_POINT ( 'NONE',  ( -9.998780405325002008, -77.28743033848687105, -5.083552005986999411 ) ) ;
#52848 = CARTESIAN_POINT ( 'NONE',  ( -5.869402599192000025, -78.36567021304000491, 10.46661899222999992 ) ) ;
#52849 = CARTESIAN_POINT ( 'NONE',  ( 3.476140009347202131, -86.40321104920798234, 2.524824982687337016 ) ) ;
#52850 = CARTESIAN_POINT ( 'NONE',  ( -9.066796825632000179, -78.95177737248700112, -6.603885667862000375 ) ) ;
#52851 = CARTESIAN_POINT ( 'NONE',  ( 1.161006248771640159, -79.96550791624770227, 9.176744600133316609 ) ) ;
#52852 = CARTESIAN_POINT ( 'NONE',  ( -8.781071604798297514, -80.00280623849064909, -6.803245145519296599 ) ) ;
#52853 = EDGE_LOOP ( 'NONE', ( #22858, #26904, #24235, #17315 ) ) ;
#52854 = CARTESIAN_POINT ( 'NONE',  ( -3.006161377376999955, -79.01730753078498992, 10.85780494109000038 ) ) ;
#52855 = CARTESIAN_POINT ( 'NONE',  ( 6.151869538368270440, -77.28303250187612150, -6.911824961258240307 ) ) ;
#52856 = CARTESIAN_POINT ( 'NONE',  ( -1.290198984414000050, -80.83131689367100137, -0.5875878301326999953 ) ) ;
#52857 = CARTESIAN_POINT ( 'NONE',  ( 0.3271848554491016414, -83.14583333333332860, -1.217465845835393967 ) ) ;
#52858 = CARTESIAN_POINT ( 'NONE',  ( 12.00000000000000533, -77.14258394437167965, -1.118314842272784881 ) ) ;
#52859 = CARTESIAN_POINT ( 'NONE',  ( 0.3098463080081999554, -78.90593676564900250, 1.484230999220000013 ) ) ;
#52860 = CARTESIAN_POINT ( 'NONE',  ( -8.130811096204000776, -61.48523690322999613, -9.546858433459998849 ) ) ;
#52861 = EDGE_CURVE ( 'NONE', #33091, #25591, #56644, .T. ) ;
#52862 = CARTESIAN_POINT ( 'NONE',  ( 9.500000000000003553, -77.04166666666665719, -0.9948376736368218509 ) ) ;
#52863 = CARTESIAN_POINT ( 'NONE',  ( 9.250000000000000000, -77.84999999999999432, 0.000000000000000000 ) ) ;
#52864 = CARTESIAN_POINT ( 'NONE',  ( -11.00000000000000000, -74.59999999999999432, 0.000000000000000000 ) ) ;
#52865 = CARTESIAN_POINT ( 'NONE',  ( -7.642147947538999730, -19.21514526754999963, 10.55910102244999926 ) ) ;
#52866 = CARTESIAN_POINT ( 'NONE',  ( 2.592785862636999727, -78.70060060100799149, -10.85214546196000107 ) ) ;
#52867 = CARTESIAN_POINT ( 'NONE',  ( 10.07722254369999959, -20.25199022618999933, -7.718368845809999712 ) ) ;
#52868 = CARTESIAN_POINT ( 'NONE',  ( -1.225907436145275087, -83.08370455176279279, 0.2589396600793889558 ) ) ;
#52869 = CARTESIAN_POINT ( 'NONE',  ( 2.775476009882999584, -81.13242513063499928, 3.115010180492999936 ) ) ;
#52870 = CIRCLE ( 'NONE', #17985, 14.00000000000000000 ) ;
#52871 = VERTEX_POINT ( 'NONE', #35661 ) ;
#52873 = B_SPLINE_CURVE_WITH_KNOTS ( 'NONE', 3,
 ( #16833, #30387, #11546, #34237, #34815, #52843, #53132, #12681, #30673, #56412, #15961, #33953, #11826, #29523, #29804, #47858, #22116, #50401, #10534, #32357, #9950, #1111, #27930, #35385, #32644, #19096, #40126, #14649, #31250, #46274, #5224, #39831, #28217, #50983, #32939, #23230, #36798, #35693, #41234, #45980, #54816, #14357, #58139, #55104, #50695, #3826, #53721, #13259, #57843, #41526, #26834, #10238, #17706, #17401, #1394, #28516, #49292, #5798, #45684, #5506, #21826, #55395, #37381, #23515, #4116 ),
 .UNSPECIFIED., .F., .F.,
 ( 4, 1, 1, 1, 1, 1, 1, 1, 1, 1, 1, 1, 1, 1, 1, 1, 1, 1, 1, 1, 1, 1, 1, 1, 1, 1, 1, 1, 1, 1, 1, 1, 1, 1, 1, 1, 1, 1, 1, 1, 1, 1, 1, 1, 1, 1, 1, 1, 1, 1, 1, 1, 1, 1, 1, 1, 1, 1, 1, 1, 1, 1, 4 ),
 ( 1.368866741782499985E-09, 0.01249973857914446311, 0.02874974741936314054, 0.04499975625958181624, 0.06124976509980049194, 0.07749977394001916764, 0.09374978278023785028, 0.1099997916204565329, 0.1262498004606752156, 0.1424998093008938704, 0.1587498181411125531, 0.1749998269813312357, 0.1912498358215499183, 0.2074998446617686010, 0.2237498535019872836, 0.2399998623422059385, 0.2562498711824245934, 0.2724998800226433593, 0.2887498888628620142, 0.3049998977030806691, 0.3212499065432993239, 0.3374999153835180898, 0.3537499242237367447, 0.3699999330639553996, 0.3862499419041740545, 0.4024999507443927649, 0.4187499595846114753, 0.4349999684248301302, 0.4512499772650487850, 0.4674999861052674954, 0.4837499949454861503, 0.5000000037857047497, 0.5162500126259234046, 0.5325000214661420594, 0.5487500303063607143, 0.5650000391465793692, 0.5812500479867981351, 0.5975000568270167900, 0.6137500656672355559, 0.6300000745074542108, 0.6462500833476728657, 0.6625000921878915205, 0.6787501010281101754, 0.6950001098683288303, 0.7112501187085475962, 0.7275001275487662511, 0.7437501363889849060, 0.7600001452292036719, 0.7762501540694223268, 0.7925001629096409816, 0.8087501717498596365, 0.8250001805900781804, 0.8412501894302969463, 0.8575001982705156012, 0.8737502071107342561, 0.8900002159509529109, 0.9062502247911715658, 0.9225002336313903317, 0.9387502424716089866, 0.9550002513118276415, 0.9712502601520462964, 0.9875002689922650623, 1.000000000000000000 ),
 .UNSPECIFIED. ) ;
#52872 = CARTESIAN_POINT ( 'NONE',  ( 1.571010256693058382, -77.20000000000000284, 10.69622524930801610 ) ) ;
#52874 = CARTESIAN_POINT ( 'NONE',  ( -1.526555281555000088, -80.41514174310999863, -0.4289821568622999570 ) ) ;
#52875 = CARTESIAN_POINT ( 'NONE',  ( 10.40649676915236554, -79.32929474332972575, -2.787393060167447700 ) ) ;
#52876 = CARTESIAN_POINT ( 'NONE',  ( 11.79843486695000010, -77.30224039084099275, -2.076781258317999868 ) ) ;
#52877 = CARTESIAN_POINT ( 'NONE',  ( -8.768124086549999419, -55.65000000488999632, 7.919595949288999570 ) ) ;
#52878 = CARTESIAN_POINT ( 'NONE',  ( -1.458706046781999888, -81.67106234573999757, 0.8046341008317999810 ) ) ;
#52879 = CARTESIAN_POINT ( 'NONE',  ( 3.128537261037801720, -1.962059611134583381, -1.619158658661195016 ) ) ;
#52880 = CARTESIAN_POINT ( 'NONE',  ( -8.871933854994999535, -78.66360194988500609, -3.979018739998999354 ) ) ;
#52881 = CARTESIAN_POINT ( 'NONE',  ( 9.296715471869999803, -78.93591467081699875, -2.514846541900999988 ) ) ;
#52882 = CARTESIAN_POINT ( 'NONE',  ( 0.5390150933986999071, -53.53739108314999839, -12.77520260999999913 ) ) ;
#52883 = CARTESIAN_POINT ( 'NONE',  ( 9.771310077954293405, -75.99681162634880138, 6.525553964492908143 ) ) ;
#52884 = B_SPLINE_CURVE_WITH_KNOTS ( 'NONE', 3,
 ( #37916, #55643, #55057, #55941, #50353, #14893, #23182, #6041, #18757, #10483 ),
 .UNSPECIFIED., .F., .F.,
 ( 4, 2, 2, 2, 4 ),
 ( 1.658364595237685148E-07, 0.2500001243773446458, 0.5000000829182297268, 0.7500000414591149189, 1.000000000000000000 ),
 .UNSPECIFIED. ) ;
#52885 = CARTESIAN_POINT ( 'NONE',  ( -12.00000000000000000, -60.04999999966999980, 1.750000000000000000 ) ) ;
#52886 = ORIENTED_EDGE ( 'NONE', *, *, #3001, .T. ) ;
#52887 = EDGE_CURVE ( 'NONE', #45976, #34794, #17973, .T. ) ;
#52888 = DIRECTION ( 'NONE',  ( 0.000000000000000000, -1.000000000000000000, 0.000000000000000000 ) ) ;
#52889 = CARTESIAN_POINT ( 'NONE',  ( 3.250000000000000000, -2.350000000000000089, 0.000000000000000000 ) ) ;
#52890 = CARTESIAN_POINT ( 'NONE',  ( 9.505949683906999681, -79.00000000000000000, 6.906476714433999575 ) ) ;
#52891 = CARTESIAN_POINT ( 'NONE',  ( 5.940599228801999379E-14, -5.950000000028880187, 0.000000000000000000 ) ) ;
#52892 = AXIS2_PLACEMENT_3D ( 'NONE', #28563, #32984, #10879 ) ;
#52893 = CARTESIAN_POINT ( 'NONE',  ( 9.304500756975000897, -79.07535835443499650, -5.821536072646999571 ) ) ;
#52894 = CARTESIAN_POINT ( 'NONE',  ( 10.89973958340319449, -80.30026041666515368, 1.427624786073512508 ) ) ;
#52895 = CARTESIAN_POINT ( 'NONE',  ( 3.214918584686000003, -76.29524370419399304, 11.96249688184999904 ) ) ;
#52896 = DIRECTION ( 'NONE',  ( 0.000000000000000000, -1.000000000000000000, 0.000000000000000000 ) ) ;
#52897 = DIRECTION ( 'NONE',  ( -0.7592504785507919740, 0.04890181649404949649, -0.6489586451877930040 ) ) ;
#52898 = EDGE_LOOP ( 'NONE', ( #56728, #45821, #12758, #22035 ) ) ;
#52899 = CONICAL_SURFACE ( 'NONE', #34960, 1.099999997149000430, 0.7853981633972997312 ) ;
#52900 = CARTESIAN_POINT ( 'NONE',  ( 9.298000630789001519, -78.93635809738199782, 5.937079976835999418 ) ) ;
#52901 = CARTESIAN_POINT ( 'NONE',  ( 1.476676445040142616, -77.36242827574842806, 9.246657040384873127 ) ) ;
#52902 = CARTESIAN_POINT ( 'NONE',  ( 9.799981295308937135, -75.80000000000001137, -6.813203508582525991 ) ) ;
#52903 = CARTESIAN_POINT ( 'NONE',  ( -3.607132791900000246, -79.34186490753599230, -10.55841809546000043 ) ) ;
#52904 = CARTESIAN_POINT ( 'NONE',  ( 10.19999999921000011, -0.2000000007865999907, -1.811584077144999807E-09 ) ) ;
#52905 = FACE_OUTER_BOUND ( 'NONE', #46190, .T. ) ;
#52906 = CARTESIAN_POINT ( 'NONE',  ( -1.008405205759953738, -82.78255986396547428, 1.125655370664245591 ) ) ;
#52907 = CARTESIAN_POINT ( 'NONE',  ( -4.862705500402999981, -78.91919103528699964, -11.27607530993000040 ) ) ;
#52908 = EDGE_LOOP ( 'NONE', ( #5651, #38889, #21305, #16627, #20536 ) ) ;
#52909 = FACE_OUTER_BOUND ( 'NONE', #18625, .T. ) ;
#52910 = CARTESIAN_POINT ( 'NONE',  ( -12.70228857842963421, -61.62190589578845845, -1.213561371295317048 ) ) ;
#52911 = SURFACE_STYLE_FILL_AREA ( #12180 ) ;
#52912 = CARTESIAN_POINT ( 'NONE',  ( 9.250000000000000000, -79.24999999999998579, 0.000000000000000000 ) ) ;
#52913 = ORIENTED_EDGE ( 'NONE', *, *, #45640, .T. ) ;
#52914 = ORIENTED_EDGE ( 'NONE', *, *, #15687, .T. ) ;
#52915 = AXIS2_PLACEMENT_3D ( 'NONE', #1449, #2604, #10294 ) ;
#52916 = DIRECTION ( 'NONE',  ( 0.000000000000000000, -1.000000000000000000, 0.000000000000000000 ) ) ;
#52917 = ORIENTED_EDGE ( 'NONE', *, *, #2208, .F. ) ;
#52918 = CARTESIAN_POINT ( 'NONE',  ( 12.21456857099000004, -78.79487223422000852, -1.096995930408000142 ) ) ;
#52919 = VERTEX_POINT ( 'NONE', #36264 ) ;
#52920 = CARTESIAN_POINT ( 'NONE',  ( 2.565355593234150522, -81.00000000000000000, -10.72147822234086334 ) ) ;
#52921 = CARTESIAN_POINT ( 'NONE',  ( -2.127308605635999772, -77.68280256073698808, -10.70747048031000048 ) ) ;
#52922 = CARTESIAN_POINT ( 'NONE',  ( 4.686931394918000038, -78.92108667140098532, -8.732305124302000010 ) ) ;
#52923 = CARTESIAN_POINT ( 'NONE',  ( 11.21665020278000036, -78.44881193963800570, 0.06973997782872000395 ) ) ;
#52924 = B_SPLINE_CURVE_WITH_KNOTS ( 'NONE', 3,
 ( #18538, #41842, #9971, #14966, #41257, #9674 ),
 .UNSPECIFIED., .F., .F.,
 ( 4, 2, 4 ),
 ( 0.7142789241156584090, 0.8571394620578292045, 1.000000000000000000 ),
 .UNSPECIFIED. ) ;
#52925 = VERTEX_POINT ( 'NONE', #8814 ) ;
#52926 = VERTEX_POINT ( 'NONE', #44835 ) ;
#52927 = CARTESIAN_POINT ( 'NONE',  ( -7.126130270949447620, -77.54504099251572313, 5.897698824246291771 ) ) ;
#52928 = CARTESIAN_POINT ( 'NONE',  ( 7.528714304401000312, -77.99426166612198585, -8.074838600060001426 ) ) ;
#52929 = SURFACE_STYLE_FILL_AREA ( #6611 ) ;
#52930 = CARTESIAN_POINT ( 'NONE',  ( -12.44210192982000152, -60.88432059783999506, -1.464837683472000052 ) ) ;
#52931 = AXIS2_PLACEMENT_3D ( 'NONE', #48058, #25588, #43610 ) ;
#52932 = CARTESIAN_POINT ( 'NONE',  ( -9.157500079073999544, -78.80331380109998918, 3.211059275314999795 ) ) ;
#52933 = CARTESIAN_POINT ( 'NONE',  ( 6.110725863692000104, -75.83846457245998351, 10.43515568098000124 ) ) ;
#52934 = EDGE_CURVE ( 'NONE', #34669, #24677, #5056, .T. ) ;
#52935 = CARTESIAN_POINT ( 'NONE',  ( -9.308871466119949645, -79.41571124415816030, -1.914396136332924270 ) ) ;
#52936 = CARTESIAN_POINT ( 'NONE',  ( 9.346058022005980348, -53.63471832377268100, -8.620905970535309493 ) ) ;
#52937 = CARTESIAN_POINT ( 'NONE',  ( 7.117135278674999732, -80.19036996912898019, 8.718833803912000135 ) ) ;
#52938 = CARTESIAN_POINT ( 'NONE',  ( 12.77649734584999841, -16.69171487512999974, 0.06478328530403998364 ) ) ;
#52939 = CARTESIAN_POINT ( 'NONE',  ( 0.1636246173744697330, -81.13541666666665719, -1.249999999999999778 ) ) ;
#52940 = CARTESIAN_POINT ( 'NONE',  ( -4.658475568430814562, -78.58333333333332860, -8.082524092276884176 ) ) ;
#52941 = ORIENTED_EDGE ( 'NONE', *, *, #21040, .T. ) ;
#52942 = CARTESIAN_POINT ( 'NONE',  ( -9.647309323447000651, -79.06128768769399073, -7.468504085378000035 ) ) ;
#52943 = CARTESIAN_POINT ( 'NONE',  ( 11.99999999979999821, -23.14999999072999870, -0.7999999997951999786 ) ) ;
#52944 = CARTESIAN_POINT ( 'NONE',  ( -11.86109855473999986, -78.71289532231099884, -1.682380905046999997 ) ) ;
#52945 = CARTESIAN_POINT ( 'NONE',  ( -10.52693198617999926, -18.57847693927000066, -7.606025555766000146 ) ) ;
#52947 = CARTESIAN_POINT ( 'NONE',  ( -2.065394024360999836, -18.57838567354000148, -12.82193048528000112 ) ) ;
#52946 = CARTESIAN_POINT ( 'NONE',  ( 7.626500777253000685, -60.11584731951999316, 10.35747145894000099 ) ) ;
#52948 = CARTESIAN_POINT ( 'NONE',  ( 1.995724882004761280, -1.278606234144347820, -2.597261706781343715 ) ) ;
#52949 = CARTESIAN_POINT ( 'NONE',  ( -9.380881115328000064, -79.88761105452199729, 5.414960042740999846 ) ) ;
#52950 = DIRECTION ( 'NONE',  ( 0.000000000000000000, 1.000000000000000000, 0.000000000000000000 ) ) ;
#52951 = CARTESIAN_POINT ( 'NONE',  ( 2.988858019399999844, -77.46978472970600649, -10.85820852157999994 ) ) ;
#52952 = CARTESIAN_POINT ( 'NONE',  ( -7.355596411687169045, -79.65251264481355520, -5.642826774240620402 ) ) ;
#52953 = CARTESIAN_POINT ( 'NONE',  ( 7.524256684237999870, -80.50667270824050092, -8.371336685020999369 ) ) ;
#52954 = VERTEX_POINT ( 'NONE', #9409 ) ;
#52955 = DIRECTION ( 'NONE',  ( -1.000000000000000000, 0.000000000000000000, 0.000000000000000000 ) ) ;
#52956 = ADVANCED_FACE ( 'NONE', ( #40993 ), #23848, .F. ) ;
#52957 = CARTESIAN_POINT ( 'NONE',  ( 1.930009203937000040, -55.59900967650000325, 12.72537718775000037 ) ) ;
#52958 = LINE ( 'NONE', #17515, #48546 ) ;
#52959 = CARTESIAN_POINT ( 'NONE',  ( 0.2917981891545000095, -3.349647489337999939, -3.794822625742999556 ) ) ;
#52960 = CARTESIAN_POINT ( 'NONE',  ( 3.033202772035243910, -77.59806847599675450, -10.38096122863011495 ) ) ;
#52961 = CARTESIAN_POINT ( 'NONE',  ( -7.803863155890000236, -78.13454644346299460, 8.057160196619001624 ) ) ;
#52962 = CARTESIAN_POINT ( 'NONE',  ( -12.54987159811999931, -53.74886760158999977, 0.1385534523824999975 ) ) ;
#52963 = CARTESIAN_POINT ( 'NONE',  ( 10.14999999998000035, -87.10000000002298748, -2.878934427392999978E-10 ) ) ;
#52964 = CARTESIAN_POINT ( 'NONE',  ( -2.842643194006085672, -2.059819327590527216, 1.637870626526546136 ) ) ;
#52965 = CARTESIAN_POINT ( 'NONE',  ( -3.250000000000000000, -3.000000000000000000, 0.000000000000000000 ) ) ;
#52966 = CARTESIAN_POINT ( 'NONE',  ( -3.415687109163000112, -86.11024735065198854, 2.400462065159000069 ) ) ;
#52967 = FACE_OUTER_BOUND ( 'NONE', #30594, .T. ) ;
#52968 = EDGE_CURVE ( 'NONE', #42686, #15955, #11525, .T. ) ;
#52969 = CARTESIAN_POINT ( 'NONE',  ( 2.149016008433747960, -77.09224776600551365, -11.93500411286337659 ) ) ;
#52970 = ADVANCED_FACE ( 'NONE', ( #56032 ), #29146, .F. ) ;
#52971 = CARTESIAN_POINT ( 'NONE',  ( 9.679529469260824470, -76.40157007586634563, -6.660771595346317575 ) ) ;
#52972 = CARTESIAN_POINT ( 'NONE',  ( 0.8430560329671303865, -81.91662283780821951, 0.9225686058375374143 ) ) ;
#52973 = CARTESIAN_POINT ( 'NONE',  ( 1.750000000001000089, -56.04922971509999741, -12.60356226394999979 ) ) ;
#52974 = DIRECTION ( 'NONE',  ( 0.7071067811865475727, 0.000000000000000000, -0.7071067811865475727 ) ) ;
#52975 = CARTESIAN_POINT ( 'NONE',  ( 8.150225256662000817, -79.72064415034598994, -4.374508917085999649 ) ) ;
#52976 = CARTESIAN_POINT ( 'NONE',  ( 10.50000000000000000, -7.000000000000000000, 0.000000000000000000 ) ) ;
#52977 = CARTESIAN_POINT ( 'NONE',  ( 2.716004179693354281, -80.24554370127630420, -10.40178661565319729 ) ) ;
#52978 = DIRECTION ( 'NONE',  ( 1.000000000000000000, 0.000000000000000000, 0.000000000000000000 ) ) ;
#52979 = CARTESIAN_POINT ( 'NONE',  ( -10.20679554289983493, -17.76427274284850100, -7.770327721668349064 ) ) ;
#52980 = AXIS2_PLACEMENT_3D ( 'NONE', #26179, #3744, #21463 ) ;
#52981 = CARTESIAN_POINT ( 'NONE',  ( -6.309004353333000026, -79.14717214054400074, -10.24224633278999796 ) ) ;
#52982 = DIRECTION ( 'NONE',  ( -0.7071067811865475727, 0.000000000000000000, -0.7071067811865475727 ) ) ;
#52983 = CARTESIAN_POINT ( 'NONE',  ( -11.10951737771999959, -79.33652177698400010, -1.847319190731999905 ) ) ;
#52984 = DIRECTION ( 'NONE',  ( 0.000000000000000000, 0.7071067811866525998, -0.7071067811864425456 ) ) ;
#52985 = VERTEX_POINT ( 'NONE', #37426 ) ;
#52986 = CARTESIAN_POINT ( 'NONE',  ( -0.8898229089158170568, -25.02324531182626544, 12.70296869045239951 ) ) ;
#52987 = EDGE_CURVE ( 'NONE', #17043, #8334, #13254, .T. ) ;
#52988 = VERTEX_POINT ( 'NONE', #2308 ) ;
#52989 = CARTESIAN_POINT ( 'NONE',  ( 1.250000000000000000, -83.49999999999998579, 0.000000000000000000 ) ) ;
#52990 = VERTEX_POINT ( 'NONE', #46317 ) ;
#52991 = CARTESIAN_POINT ( 'NONE',  ( -8.838834764832000701, -60.04999999966999980, 8.838834764832000701 ) ) ;
#52992 = CARTESIAN_POINT ( 'NONE',  ( -2.377882521816736539, -78.89270832978301939, -2.490427524875605592 ) ) ;
#52993 = CARTESIAN_POINT ( 'NONE',  ( -8.741790450690999137, -79.52230326501299373, 6.538842841549999285 ) ) ;
#52994 = CARTESIAN_POINT ( 'NONE',  ( 1.686350432428000090, -79.89656500032499764, 3.168590765505000295 ) ) ;
#52995 = CARTESIAN_POINT ( 'NONE',  ( 1.305056903442745497, -79.26396365760838592, 9.410159162297995650 ) ) ;
#52996 = ORIENTED_EDGE ( 'NONE', *, *, #40154, .F. ) ;
#52997 = CARTESIAN_POINT ( 'NONE',  ( 10.56370432582567176, -78.33298816678997412, -2.300065389339300825 ) ) ;
#52998 = CARTESIAN_POINT ( 'NONE',  ( -7.732335774400000972, -78.48896835061999866, -9.449795707298999758 ) ) ;
#52999 = EDGE_LOOP ( 'NONE', ( #2654, #17998, #42759, #55802, #28611, #45607, #47079, #39620 ) ) ;
#53000 = CARTESIAN_POINT ( 'NONE',  ( 10.07627163191000008, -60.04999999657000131, -7.601397897754999633 ) ) ;
#53001 = CARTESIAN_POINT ( 'NONE',  ( -10.98363359191198185, -18.81005173319954693, 0.5998275989261885321 ) ) ;
#53002 = CARTESIAN_POINT ( 'NONE',  ( -6.975812051429156391, -80.03155649378894054, 8.179013189515927706 ) ) ;
#53003 = DIRECTION ( 'NONE',  ( 0.000000000000000000, 0.000000000000000000, -1.000000000000000000 ) ) ;
#53004 = CARTESIAN_POINT ( 'NONE',  ( -3.156875167770065271, -86.31452042059396490, 1.477445080843142300 ) ) ;
#53005 = CARTESIAN_POINT ( 'NONE',  ( -2.277808299861439512, -86.04892729347230329, 2.553837542456823595 ) ) ;
#53006 = CARTESIAN_POINT ( 'NONE',  ( -7.957538301994783403, -79.08333333335991711, 8.845314404961204247 ) ) ;
#53007 = CARTESIAN_POINT ( 'NONE',  ( -1.300465888139999970, -77.86117779481000412, -12.57433635189999954 ) ) ;
#53008 = CARTESIAN_POINT ( 'NONE',  ( 8.195399132537000142, -76.15178913831199736, -7.153224378557999863 ) ) ;
#53009 = CARTESIAN_POINT ( 'NONE',  ( -10.14948852600000073, -22.75100835510000152, 7.674614791843000106 ) ) ;
#53010 = CARTESIAN_POINT ( 'NONE',  ( -3.973259589201000530, -78.85439465482099308, 0.5748252895958999575 ) ) ;
#53011 = TOROIDAL_SURFACE ( 'NONE', #35067, 1.250000000000000000, 0.5000000000000000000 ) ;
#53012 = CARTESIAN_POINT ( 'NONE',  ( -10.04116292115999975, -56.03537109808000594, 7.682344222575999915 ) ) ;
#53013 = CARTESIAN_POINT ( 'NONE',  ( -1.549588883243708803, -3.015970767069136027, 2.856984001263128015 ) ) ;
#53014 = CARTESIAN_POINT ( 'NONE',  ( 2.110462767538999973, -79.17075264934788947, -2.847965697444999833 ) ) ;
#53015 = CARTESIAN_POINT ( 'NONE',  ( -1.103931348490902131, -24.62083748119153981, -12.50298439258945926 ) ) ;
#53016 = CARTESIAN_POINT ( 'NONE',  ( -3.308786720591999853, -83.27544503318799229, -1.278081663740999963 ) ) ;
#53017 = CARTESIAN_POINT ( 'NONE',  ( 2.534829140202000008, -2.099668092570999622, 2.839140403359000420 ) ) ;
#53018 = CARTESIAN_POINT ( 'NONE',  ( -0.9820397338569999413, -80.80308451575899653, -0.7733679338621000099 ) ) ;
#53019 = EDGE_LOOP ( 'NONE', ( #36217, #49362, #21321, #40941 ) ) ;
#53020 = CARTESIAN_POINT ( 'NONE',  ( -9.205846894779998735, -61.80798911315000055, -8.541134278117000989 ) ) ;
#53021 = EDGE_CURVE ( 'NONE', #21614, #34387, #11171, .T. ) ;
#53022 = AXIS2_PLACEMENT_3D ( 'NONE', #38698, #7694, #34256 ) ;
#53023 = CARTESIAN_POINT ( 'NONE',  ( -12.00000000000000000, -79.29999999999999716, 0.000000000000000000 ) ) ;
#53024 = CARTESIAN_POINT ( 'NONE',  ( -0.2317941695893000198, -82.28827061000599485, -1.228320586388000013 ) ) ;
#53025 = EDGE_CURVE ( 'NONE', #27418, #10196, #51615, .T. ) ;
#53026 = FACE_OUTER_BOUND ( 'NONE', #32416, .T. ) ;
#53027 = CARTESIAN_POINT ( 'NONE',  ( 12.24999999909999993, -80.79999999910000952, 7.143947115078999467E-09 ) ) ;
#53029 = FACE_OUTER_BOUND ( 'NONE', #31694, .T. ) ;
#53028 = VECTOR ( 'NONE', #27334, 1000.000000000000114 ) ;
#53030 = CARTESIAN_POINT ( 'NONE',  ( -1.165746613897999928E-14, -72.79999999999999716, 0.000000000000000000 ) ) ;
#53031 = CARTESIAN_POINT ( 'NONE',  ( 0.7751617840477000865, -76.53848582389998967, 12.18739828824000071 ) ) ;
#53032 = ORIENTED_EDGE ( 'NONE', *, *, #1601, .T. ) ;
#53033 = CIRCLE ( 'NONE', #48328, 14.00000000000000000 ) ;
#53034 = DIRECTION ( 'NONE',  ( 0.000000000000000000, 0.000000000000000000, -1.000000000000000000 ) ) ;
#53035 = CARTESIAN_POINT ( 'NONE',  ( -7.919595949288999570, -55.64999999965999677, 8.768124086712999699 ) ) ;
#53036 = EDGE_CURVE ( 'NONE', #22633, #2598, #15872, .T. ) ;
#53037 = B_SPLINE_CURVE_WITH_KNOTS ( 'NONE', 3,
 ( #49770, #14019, #23177, #41185, #775, #18752, #9897, #1059, #55638, #56800 ),
 .UNSPECIFIED., .F., .F.,
 ( 4, 2, 2, 2, 4 ),
 ( 0.000000000000000000, 0.1250000012806290195, 0.2500000025612580390, 0.3750000038418869752, 0.5000000051225159670 ),
 .UNSPECIFIED. ) ;
#53038 = CARTESIAN_POINT ( 'NONE',  ( -10.98768124890674258, -18.54978970308804875, -0.5208900350597093221 ) ) ;
#53039 = CARTESIAN_POINT ( 'NONE',  ( 7.374560639698994002, -79.07708333333330586, -9.596002108778151296 ) ) ;
#53040 = CARTESIAN_POINT ( 'NONE',  ( -8.852983674280999082, -78.98694786691399372, -3.506430706099999739 ) ) ;
#53041 = CARTESIAN_POINT ( 'NONE',  ( 1.289278921801000122, -84.26256135553198590, 3.968353856072999619 ) ) ;
#53042 = CARTESIAN_POINT ( 'NONE',  ( -1.607226962776981516, -79.98739046983742185, 10.62889775543116677 ) ) ;
#53043 = CARTESIAN_POINT ( 'NONE',  ( 1.330388504836999886, -79.83712754295498826, 0.7273297589862000034 ) ) ;
#53044 = ORIENTED_EDGE ( 'NONE', *, *, #3159, .F. ) ;
#53045 = CARTESIAN_POINT ( 'NONE',  ( 9.243118074942941576, -78.85649633572980122, 0.7011782411833578088 ) ) ;
#53046 = ORIENTED_EDGE ( 'NONE', *, *, #56315, .F. ) ;
#53047 = CARTESIAN_POINT ( 'NONE',  ( -10.10912517728183069, -60.27586858098902667, -7.634643689463517902 ) ) ;
#53048 = CARTESIAN_POINT ( 'NONE',  ( 4.007494466573000125, -79.89653890021898519, -10.71665855536000223 ) ) ;
#53049 = ORIENTED_EDGE ( 'NONE', *, *, #5216, .F. ) ;
#53050 = CARTESIAN_POINT ( 'NONE',  ( 11.98062200086999951, -77.49499819968599468, -2.108850158091000182 ) ) ;
#53051 = AXIS2_PLACEMENT_3D ( 'NONE', #52577, #2986, #15402 ) ;
#53052 = ORIENTED_EDGE ( 'NONE', *, *, #20245, .F. ) ;
#53053 = ORIENTED_EDGE ( 'NONE', *, *, #9705, .F. ) ;
#53054 = CIRCLE ( 'NONE', #33242, 0.5000000000000006661 ) ;
#53055 = CARTESIAN_POINT ( 'NONE',  ( -8.852984619042215897, -78.14157800056186431, 7.764154262050229960 ) ) ;
#53056 = CARTESIAN_POINT ( 'NONE',  ( 1.739862777674999972, -79.61076166194752091, 9.611119481339999382 ) ) ;
#53057 = B_SPLINE_SURFACE_WITH_KNOTS ( 'NONE', 3, 3, ( 
 ( #50385, #22328, #54800, #40344, #53934, #49803, #9349, #45374, #13467, #4920, #22920, #14056, #9932, #31463, #27039, #27911, #55087, #42097, #6659, #19082, #33799, #24080, #1374, #6073, #46253, #11393, #56258, #15224, #33214, #10221, #14633, #19657, #50963, #14923, #46548 ),
 ( #50678, #32919, #10514, #45961, #1667, #19370, #37658, #19959, #5490, #55673, #28198, #23787, #23495, #5781, #28498, #51260, #41509, #10812, #37362, #28792, #37947, #1095, #46839, #41801, #55377, #37068, #20244, #24382, #24671, #15809, #6366, #55968, #42394, #1964, #51839 ),
 ( #15519, #32625, #33515, #51550, #11107, #38237, #42681, #29088, #47132, #2247, #16966, #52692, #29371, #57410, #47418, #56545, #34949, #11966, #25242, #39680, #21388, #8105, #34377, #47708, #52981, #12531, #38819, #29941, #42972, #6949, #2529, #24953, #25818, #12246, #20532 ),
 ( #21676, #16682, #38530, #52409, #57116, #7237, #16106, #30237, #26101, #48280, #52123, #30528, #3392, #34086, #7819, #47995, #3112, #43262, #39401, #48560, #11681, #2817, #56837, #29656, #43845, #7530, #44125, #20812, #16391, #3674, #17247, #25529, #57689, #43547, #21103 ) ),
 .UNSPECIFIED., .F., .F., .F.,
 ( 4, 4 ),
 ( 4, 1, 1, 1, 1, 1, 1, 1, 1, 1, 1, 1, 1, 1, 1, 1, 1, 1, 1, 1, 1, 1, 1, 1, 1, 1, 1, 1, 1, 1, 1, 1, 4 ),
 ( -0.5168282991433000850, 1.516828299142999992 ),
 ( 0.4382220305164999941, 0.4561218187598000129, 0.4740216070032000073, 0.4919213952464999706, 0.5098211834899000205, 0.5277209717331999839, 0.5456207599765999783, 0.5635205482198999416, 0.5814203364632999360, 0.5993201247066000104, 0.6172199129500000048, 0.6351197011933000791, 0.6530194894366999625, 0.6709192776799999258, 0.6888190659233000002, 0.7067188541666999946, 0.7246186424100000689, 0.7425184306533999523, 0.7604182188967000267, 0.7783180071401000211, 0.7962177953833999844, 0.8141175836267999788, 0.8320173718700999421, 0.8499171601134999365, 0.8678169483568000109, 0.8857167366002000053, 0.9036165248435000796, 0.9215163130869000740, 0.9394161013301999263, 0.9573158895735999208, 0.9752156778168999951, 0.9931154660602999895, 1.011015254303999855 ),
 .UNSPECIFIED. ) ;
#53058 = ORIENTED_EDGE ( 'NONE', *, *, #33310, .T. ) ;
#53059 = CARTESIAN_POINT ( 'NONE',  ( 10.98768124890679587, -18.54978970308837916, 0.5208900350585692340 ) ) ;
#53060 = VERTEX_POINT ( 'NONE', #1442 ) ;
#53061 = CARTESIAN_POINT ( 'NONE',  ( 6.954844635478175441, -79.22307562464830255, -10.07151940748270569 ) ) ;
#53062 = CARTESIAN_POINT ( 'NONE',  ( 3.437187628289001040, -78.85171435493609238, -1.267161289092433307E-15 ) ) ;
#53063 = B_SPLINE_CURVE_WITH_KNOTS ( 'NONE', 3,
 ( #2461, #51769, #42024, #51479, #38459, #24006, #47348, #6588, #11037, #1593, #47058, #19583, #29299, #15148, #42612, #23717, #6876, #56476, #16032, #28131, #57908, #52054, #7167, #24279 ),
 .UNSPECIFIED., .F., .F.,
 ( 4, 2, 2, 2, 2, 2, 2, 2, 2, 2, 2, 4 ),
 ( 0.000000000000000000, 0.1250000000000002776, 0.2500000000000005551, 0.3750000000000008327, 0.4375000000000006106, 0.5000000000000004441, 0.6249999999999993339, 0.7499999999999983347, 0.8124999999999977796, 0.8437499999999975575, 0.8749999999999972244, 1.000000000000000000 ),
 .UNSPECIFIED. ) ;
#53064 = ADVANCED_FACE ( 'NONE', ( #29433 ), #41865, .T. ) ;
#53065 = AXIS2_PLACEMENT_3D ( 'NONE', #47548, #34202, #56381 ) ;
#53066 = CARTESIAN_POINT ( 'NONE',  ( 8.485548443509999927, -53.91931586703000079, 9.101490738433000161 ) ) ;
#53067 = FACE_OUTER_BOUND ( 'NONE', #51986, .T. ) ;
#53068 = CARTESIAN_POINT ( 'NONE',  ( 10.36935812844000004, -78.07876026662599145, -2.835297515976000327 ) ) ;
#53069 = CIRCLE ( 'NONE', #25763, 14.00000000000000000 ) ;
#53070 = CARTESIAN_POINT ( 'NONE',  ( 12.70305380116828964, -61.83154493736390833, -0.8725910145092488079 ) ) ;
#53071 = CARTESIAN_POINT ( 'NONE',  ( -1.413836290689950648, -77.82099477392877418, 0.5308369793427527572 ) ) ;
#53072 = CARTESIAN_POINT ( 'NONE',  ( 8.496400742388793503, -78.81780298388180483, -3.659025731067179876 ) ) ;
#53073 = DIRECTION ( 'NONE',  ( 0.000000000000000000, -1.000000000000000000, 0.000000000000000000 ) ) ;
#53074 = CARTESIAN_POINT ( 'NONE',  ( -1.405958995161999958, -81.93650264934798599, -3.931017140282999645 ) ) ;
#53075 = CARTESIAN_POINT ( 'NONE',  ( 5.982226491729999651, -77.14386001420199079, 7.853930782076001371 ) ) ;
#53076 = DIRECTION ( 'NONE',  ( 0.000000000000000000, 1.000000000000000000, 0.000000000000000000 ) ) ;
#53077 = FACE_OUTER_BOUND ( 'NONE', #1102, .T. ) ;
#53078 = LINE ( 'NONE', #20631, #15926 ) ;
#53079 = CARTESIAN_POINT ( 'NONE',  ( 12.50000000000000000, -39.30476012429000576, 0.000000000000000000 ) ) ;
#53080 = LINE ( 'NONE', #7341, #4599 ) ;
#53081 = CARTESIAN_POINT ( 'NONE',  ( -9.596002108778161954, -77.85208333333332575, -7.374560639698982456 ) ) ;
#53083 = EDGE_CURVE ( 'NONE', #26528, #35802, #38767, .T. ) ;
#53082 = CARTESIAN_POINT ( 'NONE',  ( 1.501221344685673476, -80.09017822003303877, -0.1728645978363567981 ) ) ;
#53084 = CARTESIAN_POINT ( 'NONE',  ( 9.380731069130998634, -77.26943616160899353, -0.1623923911645999696 ) ) ;
#53085 = CARTESIAN_POINT ( 'NONE',  ( -1.403403115923000044, -77.87752668643429388, 0.5665048067823000855 ) ) ;
#53086 = CARTESIAN_POINT ( 'NONE',  ( -7.714303428875997959, -26.30294702886003222, -12.53545825868000385 ) ) ;
#53087 = CARTESIAN_POINT ( 'NONE',  ( -1.719553322141999852, -1.968155165121999950, -3.292171862600000054 ) ) ;
#53088 = CARTESIAN_POINT ( 'NONE',  ( 4.442094508599000235, -77.09588318900199511, -11.32474889210000057 ) ) ;
#53089 = CARTESIAN_POINT ( 'NONE',  ( -1.980584515752000119, -60.06485146591000301, 12.76303204605000197 ) ) ;
#53090 = CARTESIAN_POINT ( 'NONE',  ( 1.407171709420440342, -79.13541666666665719, -10.74999999999999822 ) ) ;
#53092 = DIRECTION ( 'NONE',  ( 0.000000000000000000, -1.000000000000000000, 0.000000000000000000 ) ) ;
#53091 = LINE ( 'NONE', #53373, #31670 ) ;
#53093 = CARTESIAN_POINT ( 'NONE',  ( 1.318896022268000179, -82.92957200447399657, 0.6457249424517998992 ) ) ;
#53094 = CARTESIAN_POINT ( 'NONE',  ( -6.163538728152516022, -79.52360460267682640, 8.807809540774020007 ) ) ;
#53095 = B_SPLINE_CURVE_WITH_KNOTS ( 'NONE', 3,
 ( #11199, #16197, #42486, #42193, #43346, #33315, #20903, #56925, #11766, #33606, #38906, #24177, #7327, #15321, #55774, #2338, #46932, #47795, #2624, #16484, #1762, #38043, #15902, #51349, #34463, #19756, #52494, #24762, #2055, #6754, #6459, #12051, #46639, #33888, #51929 ),
 .UNSPECIFIED., .F., .F.,
 ( 4, 1, 1, 1, 1, 1, 1, 1, 1, 1, 1, 1, 1, 1, 1, 1, 1, 1, 1, 1, 1, 1, 1, 1, 1, 1, 1, 1, 1, 1, 1, 1, 4 ),
 ( 0.000000000000000000, 0.01250358773558132505, 0.04500335175853042990, 0.07750311578147953129, 0.1100028798044286465, 0.1425026438273777341, 0.1750024078503268354, 0.2075021718732759646, 0.2400019358962250660, 0.2725016999191742229, 0.3050014639421232965, 0.3375012279650724256, 0.3700009919880215548, 0.4025007560109706839, 0.4350005200339197575, 0.4675002840568688867, 0.5000000480798180158, 0.5324998121027670894, 0.5649995761257161631, 0.5974993401486653477, 0.6299991041716144213, 0.6624988681945634950, 0.6949986322175125686, 0.7274983962404617532, 0.7599981602634108269, 0.7924979242863599005, 0.8249976883093089741, 0.8574974523322581588, 0.8899972163552072324, 0.9224969803781563060, 0.9549967444011054907, 0.9874965084240546753, 1.000000000000000000 ),
 .UNSPECIFIED. ) ;
#53096 = ORIENTED_EDGE ( 'NONE', *, *, #6348, .T. ) ;
#53097 = CARTESIAN_POINT ( 'NONE',  ( -0.9995835529977249445, -82.05208333333328596, -0.7681833999686439318 ) ) ;
#53098 = VECTOR ( 'NONE', #12065, 1000.000000000000000 ) ;
#53099 = CARTESIAN_POINT ( 'NONE',  ( -8.792674058200999454, -79.75099187107899468, -8.226855735085999655 ) ) ;
#53100 = CARTESIAN_POINT ( 'NONE',  ( 8.982046426857383636, -79.02685948540812433, 3.153244770633860217 ) ) ;
#53101 = ADVANCED_FACE ( 'NONE', ( #6428 ), #34957, .F. ) ;
#53102 = CARTESIAN_POINT ( 'NONE',  ( 3.721465242739084189, -79.74999999999997158, 11.44722502806610365 ) ) ;
#53103 = CARTESIAN_POINT ( 'NONE',  ( -11.00000000000000888, -79.08958333333330870, 1.439896632895276252 ) ) ;
#53104 = CARTESIAN_POINT ( 'NONE',  ( 1.675401668936999933, -1.380130151312000120, 3.116766381725000201 ) ) ;
#53105 = CARTESIAN_POINT ( 'NONE',  ( -9.692328422619000960, -79.19622958825499381, 1.312170392071000169 ) ) ;
#53106 = CARTESIAN_POINT ( 'NONE',  ( 12.72394223969999949, -23.22159774865999893, -1.930881086224999876 ) ) ;
#53107 = CARTESIAN_POINT ( 'NONE',  ( -2.062673488738000049, -60.12452529330000317, 12.82904091341000097 ) ) ;
#53108 = ORIENTED_EDGE ( 'NONE', *, *, #5184, .T. ) ;
#53109 = AXIS2_PLACEMENT_3D ( 'NONE', #20868, #29997, #25294 ) ;
#53110 = CARTESIAN_POINT ( 'NONE',  ( 12.76303204517000012, -18.73514852243999940, -1.980584515753000208 ) ) ;
#53111 = CARTESIAN_POINT ( 'NONE',  ( -6.786047990210001046, -79.69408667140099567, 6.837407397534001063 ) ) ;
#53112 = CARTESIAN_POINT ( 'NONE',  ( -12.55432891853854471, -18.61272687758821576, 1.749897736042294039 ) ) ;
#53113 = CIRCLE ( 'NONE', #19112, 14.00000000000000000 ) ;
#53114 = CARTESIAN_POINT ( 'NONE',  ( -10.55911395187000146, -59.58461666436000570, -7.642160924878999673 ) ) ;
#53115 = CARTESIAN_POINT ( 'NONE',  ( -3.517605154487999819, -84.71217953870899464, -0.4593545457370999952 ) ) ;
#53116 = ORIENTED_EDGE ( 'NONE', *, *, #3, .T. ) ;
#53117 = CARTESIAN_POINT ( 'NONE',  ( 11.00000000000000000, -4.000000000000000000, 0.000000000000000000 ) ) ;
#53118 = CARTESIAN_POINT ( 'NONE',  ( -9.252740428349007118, -78.37916666666666288, 2.486604901413125734 ) ) ;
#53119 = CARTESIAN_POINT ( 'NONE',  ( -0.4254240051736147277, -1.114583333333333925, -3.250000000000000888 ) ) ;
#53120 = EDGE_LOOP ( 'NONE', ( #34314, #26436, #24741, #43775 ) ) ;
#53121 = CARTESIAN_POINT ( 'NONE',  ( 1.423904377294109791, -54.49487194733401907, 12.50677628652274898 ) ) ;
#53122 = CARTESIAN_POINT ( 'NONE',  ( -9.788022091658000079, -54.27120090369999872, -7.956349397036000859 ) ) ;
#53123 = SURFACE_STYLE_FILL_AREA ( #4405 ) ;
#53124 = CARTESIAN_POINT ( 'NONE',  ( 9.767191983224998708, -79.52026917934998096, 0.05162932631433000269 ) ) ;
#53125 = EDGE_LOOP ( 'NONE', ( #23651, #45616, #34895, #43854 ) ) ;
#53126 = ORIENTED_EDGE ( 'NONE', *, *, #17830, .F. ) ;
#53127 = CARTESIAN_POINT ( 'NONE',  ( 2.563364080296999692, -77.04950204046299689, 12.08374998559000169 ) ) ;
#53128 = DIRECTION ( 'NONE',  ( 0.000000000000000000, -0.8191989533105277221, -0.5735094374942192319 ) ) ;
#53129 = ORIENTED_EDGE ( 'NONE', *, *, #25882, .T. ) ;
#53130 = CARTESIAN_POINT ( 'NONE',  ( 7.430757984336000099, -77.49363084965399651, 5.911115298933000695 ) ) ;
#53131 = EDGE_CURVE ( 'NONE', #50685, #26598, #5661, .T. ) ;
#53132 = CARTESIAN_POINT ( 'NONE',  ( -1.182210496605485606, -78.96518710813624864, -9.632040656990779937 ) ) ;
#53133 = CARTESIAN_POINT ( 'NONE',  ( 0.4817127218574778769, -80.25663193929872818, -1.153353357640556798 ) ) ;
#53134 = CARTESIAN_POINT ( 'NONE',  ( 12.34410331423999985, -77.39726523887000553, -3.381164140480000135 ) ) ;
#53135 = EDGE_CURVE ( 'NONE', #51746, #37664, #20023, .T. ) ;
#53136 = CARTESIAN_POINT ( 'NONE',  ( 9.070694317316998934, -78.05004794253746070, 6.598531290616000078 ) ) ;
#53137 = CARTESIAN_POINT ( 'NONE',  ( -3.335532751159751452, -86.39318692614399708, 1.410355715539307830 ) ) ;
#53138 = CARTESIAN_POINT ( 'NONE',  ( 9.453938376997999882, -79.19690445950300273, 6.036651369377000087 ) ) ;
#53139 = CARTESIAN_POINT ( 'NONE',  ( 3.505028940034645046, -79.94415934739535601, 8.560182507365089677 ) ) ;
#53140 = B_SPLINE_CURVE_WITH_KNOTS ( 'NONE', 3,
 ( #15013, #51053, #41013, #54876, #32422, #18585, #1463, #46045 ),
 .UNSPECIFIED., .F., .F.,
 ( 4, 2, 2, 4 ),
 ( 0.000000000000000000, 0.5000000000000000000, 0.7500000000000000000, 1.000000000000000000 ),
 .UNSPECIFIED. ) ;
#53141 = CARTESIAN_POINT ( 'NONE',  ( 8.894932048708428241, -16.77190732484968194, 9.073469156717420603 ) ) ;
#53142 = ORIENTED_EDGE ( 'NONE', *, *, #32419, .T. ) ;
#53143 = CARTESIAN_POINT ( 'NONE',  ( -3.770495512267000304, -79.52296990877398741, 10.61660482251999937 ) ) ;
#53144 = CARTESIAN_POINT ( 'NONE',  ( -1.431006885156403508, -77.21271974587020281, -9.151478666840258569 ) ) ;
#53145 = CARTESIAN_POINT ( 'NONE',  ( 12.00000000000000000, -77.14999999999999147, 0.000000000000000000 ) ) ;
#53146 = CARTESIAN_POINT ( 'NONE',  ( 1.310116429410000061, -78.91745489434200067, 0.1554359553024000085 ) ) ;
#53147 = AXIS2_PLACEMENT_3D ( 'NONE', #9378, #22952, #50124 ) ;
#53148 = CARTESIAN_POINT ( 'NONE',  ( 2.597098890255110426, -3.158231272032415937, 2.378515465166538334 ) ) ;
#53149 = CARTESIAN_POINT ( 'NONE',  ( 12.53239398059000109, -22.76486430425999785, 1.667936688463999895 ) ) ;
#53150 = CARTESIAN_POINT ( 'NONE',  ( 5.917523019358037040, -76.63333333333329733, 10.26699006316254525 ) ) ;
#53151 = CARTESIAN_POINT ( 'NONE',  ( 9.000000000000000000, -91.89999999999999147, 2.447153590879000268E-12 ) ) ;
#53152 = CARTESIAN_POINT ( 'NONE',  ( -3.321932689531000182, -80.44999999999998863, -10.22385755016999909 ) ) ;
#53153 = CARTESIAN_POINT ( 'NONE',  ( -11.14855507251999889, -78.56013882934497872, -0.4486863643567999826 ) ) ;
#53154 = CYLINDRICAL_SURFACE ( 'NONE', #48019, 1.750000000000000000 ) ;
#53155 = DIRECTION ( 'NONE',  ( -1.000000000000000000, 0.000000000000000000, 0.000000000000000000 ) ) ;
#53156 = CARTESIAN_POINT ( 'NONE',  ( -0.4362184210878999879, -80.53117300822900404, -4.149249208457999494 ) ) ;
#53157 = ORIENTED_EDGE ( 'NONE', *, *, #21166, .T. ) ;
#53159 = EDGE_CURVE ( 'NONE', #35609, #40455, #41530, .T. ) ;
#53158 = CARTESIAN_POINT ( 'NONE',  ( 1.517511648408000013, -82.04254865883000036, -0.7726417995267998995 ) ) ;
#53160 = CARTESIAN_POINT ( 'NONE',  ( 0.6650966107743999656, -80.79425450742999715, 1.309234371339000225 ) ) ;
#53161 = LINE ( 'NONE', #30703, #46510 ) ;
#53162 = CARTESIAN_POINT ( 'NONE',  ( 10.46934363224000109, -77.35649902168898961, 5.823135730235999397 ) ) ;
#53163 = CARTESIAN_POINT ( 'NONE',  ( 4.294001957131981406, -77.00000000000001421, 8.218741086766758741 ) ) ;
#53164 = CARTESIAN_POINT ( 'NONE',  ( -1.596536837631000072, -81.73422156085000267, -0.4757406268331999533 ) ) ;
#53165 = CARTESIAN_POINT ( 'NONE',  ( 9.599999999999999645, -87.29999999999999716, 0.000000000000000000 ) ) ;
#53166 = CARTESIAN_POINT ( 'NONE',  ( -7.530775182571000315, -78.24465584965399501, -6.150709233331999037 ) ) ;
#53167 = CARTESIAN_POINT ( 'NONE',  ( -1.666727925320000026, -55.60825518191999350, -12.50018462901999960 ) ) ;
#53168 = CARTESIAN_POINT ( 'NONE',  ( 11.15287131721528802, -75.97493627132392646, 3.701768527638496398 ) ) ;
#53169 = CARTESIAN_POINT ( 'NONE',  ( 3.757989199629945709, -86.10000000000000853, 2.729540522067831265 ) ) ;
#53170 = VERTEX_POINT ( 'NONE', #5073 ) ;
#53171 = CARTESIAN_POINT ( 'NONE',  ( -1.996743696302876181, -2.174344397066610313, -2.599173734966482741 ) ) ;
#53172 = CARTESIAN_POINT ( 'NONE',  ( 11.99606675118999810, -79.59347606058199176, 2.584336171721000497 ) ) ;
#53173 = AXIS2_PLACEMENT_3D ( 'NONE', #46572, #15836, #42125 ) ;
#53174 = CARTESIAN_POINT ( 'NONE',  ( 3.999999999999606093, -78.67389998729011324, -1.484001723589534194E-15 ) ) ;
#53175 = EDGE_CURVE ( 'NONE', #12675, #24608, #19906, .T. ) ;
#53176 = CARTESIAN_POINT ( 'NONE',  ( -7.604423127187000198, -79.86606249275499181, 7.914351627518998455 ) ) ;
#53177 = ADVANCED_FACE ( 'NONE', ( #54664 ), #23940, .T. ) ;
#53178 = CARTESIAN_POINT ( 'NONE',  ( -0.04193593611748243355, -16.98990258663360109, -12.50649570005621314 ) ) ;
#53179 = CARTESIAN_POINT ( 'NONE',  ( 4.655405164384999850, -76.66483267504600008, -11.35230195258999863 ) ) ;
#53180 = CARTESIAN_POINT ( 'NONE',  ( 0.2265013221622945161, -78.57011497404765521, 11.74582188880687816 ) ) ;
#53181 = CYLINDRICAL_SURFACE ( 'NONE', #10732, 11.65000000000000036 ) ;
#53182 = ORIENTED_EDGE ( 'NONE', *, *, #18288, .F. ) ;
#53183 = AXIS2_PLACEMENT_3D ( 'NONE', #43821, #57384, #16370 ) ;
#53184 = CARTESIAN_POINT ( 'NONE',  ( 11.03163745116999905, -78.39163123734599026, 0.06858965353743999571 ) ) ;
#53185 = CARTESIAN_POINT ( 'NONE',  ( 1.152392759189329263, -79.88190785368323077, 0.4838130652222127903 ) ) ;
#53186 = LINE ( 'NONE', #31014, #44282 ) ;
#53187 = CONICAL_SURFACE ( 'NONE', #19276, 1.099999997149000430, 0.7853981633972997312 ) ;
#53188 = B_SPLINE_SURFACE_WITH_KNOTS ( 'NONE', 3, 3, ( 
 ( #33980, #2997, #52302, #16289, #47888, #6838, #25423, #43735, #43437, #52588, #2422, #30126, #35127, #43156, #12426, #20995, #24849, #48175, #7706, #3567, #30418, #48451, #53158, #39000, #44015, #57008, #21571, #29261, #42864, #20425, #25708, #2713, #52016, #20709, #16571 ),
 ( #34556, #3287, #12138, #4738, #31572, #22442, #45189, #48737, #4440, #13285, #18321, #9460, #49620, #9167, #27445, #27148, #53445, #26283, #36603, #40456, #632, #13580, #23028, #18024, #22145, #44591, #3852, #22737, #57873, #30985, #48, #44890, #30701, #49320, #53748 ),
 ( #40747, #45481, #8281, #8573, #26861, #41042, #35415, #58166, #8868, #21850, #13876, #49025, #35719, #36312, #342, #39859, #31871, #54337, #49912, #36016, #54043, #5026, #18614, #12707, #44297, #17428, #17732, #12989, #26559, #4146, #40153, #31277, #37184, #18899, #20069 ),
 ( #55492, #28905, #24196, #1779, #1199, #14741, #46950, #6476, #50788, #24486, #41916, #5317, #41621, #23325, #42212, #50199, #55198, #42501, #15340, #54626, #33034, #50492, #41332, #5594, #2071, #32740, #32448, #916, #19773, #10332, #10047, #14162, #46656, #33333, #19192 ) ),
 .UNSPECIFIED., .F., .F., .F.,
 ( 4, 4 ),
 ( 4, 1, 1, 1, 1, 1, 1, 1, 1, 1, 1, 1, 1, 1, 1, 1, 1, 1, 1, 1, 1, 1, 1, 1, 1, 1, 1, 1, 1, 1, 1, 1, 4 ),
 ( -0.1331668876848000060, 1.133166887685000068 ),
 ( -0.02000000000000000042, 0.01250000000000000069, 0.04499999999999999833, 0.07749999999999999944, 0.1100000000000000006, 0.1424999999999999878, 0.1749999999999999889, 0.2074999999999999900, 0.2399999999999999911, 0.2725000000000000200, 0.3049999999999999933, 0.3375000000000000222, 0.3699999999999999956, 0.4025000000000000244, 0.4349999999999999978, 0.4675000000000000266, 0.5000000000000000000, 0.5324999999999999734, 0.5649999999999999467, 0.5975000000000000311, 0.6300000000000000044, 0.6624999999999999778, 0.6949999999999999512, 0.7275000000000000355, 0.7600000000000000089, 0.7924999999999999822, 0.8249999999999999556, 0.8575000000000000400, 0.8900000000000000133, 0.9224999999999999867, 0.9549999999999999600, 0.9875000000000000444, 1.020000000000000018 ),
 .UNSPECIFIED. ) ;
#53189 = CARTESIAN_POINT ( 'NONE',  ( -4.348661115406000199, -78.83620252954798957, -10.27524920185999946 ) ) ;
#53190 = CARTESIAN_POINT ( 'NONE',  ( -8.838834764832000701, -23.25000000000000000, -8.838834764832000701 ) ) ;
#53191 = CARTESIAN_POINT ( 'NONE',  ( 10.98363357722939959, -23.18990228819981780, 0.5998278677060745467 ) ) ;
#53192 = CARTESIAN_POINT ( 'NONE',  ( -10.98364304930883506, -23.23021036682267138, 0.5996544714383779118 ) ) ;
#53193 = CARTESIAN_POINT ( 'NONE',  ( -4.187998665200000303, -78.72928582732099301, 11.54367560014000205 ) ) ;
#53194 = EDGE_LOOP ( 'NONE', ( #37160, #13696, #33221, #11631 ) ) ;
#53195 = EDGE_CURVE ( 'NONE', #54081, #8704, #1243, .T. ) ;
#53196 = CARTESIAN_POINT ( 'NONE',  ( 0.000000000000000000, -45.69638659094999866, 0.000000000000000000 ) ) ;
#53197 = CARTESIAN_POINT ( 'NONE',  ( -9.393203674808288994, -78.45833333333331439, 5.413904038987134015 ) ) ;
#53198 = ORIENTED_EDGE ( 'NONE', *, *, #1839, .T. ) ;
#53199 = VERTEX_POINT ( 'NONE', #675 ) ;
#53200 = LINE ( 'NONE', #22778, #22031 ) ;
#53201 = ORIENTED_EDGE ( 'NONE', *, *, #2760, .F. ) ;
#53202 = CARTESIAN_POINT ( 'NONE',  ( -9.067527500126635331, -79.72528127043524648, 2.911084842785973681 ) ) ;
#53203 = EDGE_LOOP ( 'NONE', ( #8803, #23308, #13699, #5220 ) ) ;
#53204 = CARTESIAN_POINT ( 'NONE',  ( -10.68161435044807561, -81.00000000000001421, -1.590318374505752974 ) ) ;
#53205 = EDGE_CURVE ( 'NONE', #45494, #44485, #50536, .T. ) ;
#53206 = ADVANCED_FACE ( 'NONE', ( #41958 ), #14788, .T. ) ;
#53207 = CARTESIAN_POINT ( 'NONE',  ( 8.353603324983998490, -78.83708998579800209, -4.904950430745999235 ) ) ;
#53208 = CARTESIAN_POINT ( 'NONE',  ( -9.121286397524418277, -78.11412521488340133, -1.606255959880608319 ) ) ;
#53209 = CARTESIAN_POINT ( 'NONE',  ( -8.982117338527000783, -79.71499958499398986, 6.718606902359000266 ) ) ;
#53210 = AXIS2_PLACEMENT_3D ( 'NONE', #33958, #6816, #2117 ) ;
#53211 = ORIENTED_EDGE ( 'NONE', *, *, #55070, .F. ) ;
#53212 = ORIENTED_EDGE ( 'NONE', *, *, #28903, .F. ) ;
#53213 = CARTESIAN_POINT ( 'NONE',  ( -6.342524396040097656, -77.53526462310868794, 6.737273603580285375 ) ) ;
#53214 = CARTESIAN_POINT ( 'NONE',  ( -3.203604947276999848, -77.70797428813398255, 10.56508708803000118 ) ) ;
#53215 = DIRECTION ( 'NONE',  ( -4.222595588675998455E-09, 0.9999999999999998890, 1.485890747956999830E-08 ) ) ;
#53216 = CARTESIAN_POINT ( 'NONE',  ( -0.1538805260929999863, -78.26671631506198423, 9.702939253146000809 ) ) ;
#53217 = CARTESIAN_POINT ( 'NONE',  ( -2.499318294468000357, -76.30897654196999724, 12.72266421702999928 ) ) ;
#53218 = CARTESIAN_POINT ( 'NONE',  ( -9.106090911476261596, -79.42266151531977414, -2.710111362998674167 ) ) ;
#53219 = CARTESIAN_POINT ( 'NONE',  ( 10.36597025940859673, -55.02476146821044978, -7.635927901479407254 ) ) ;
#53220 = CARTESIAN_POINT ( 'NONE',  ( -3.493617039247999934, -80.40847481238299110, -10.33892454317000187 ) ) ;
#53221 = CARTESIAN_POINT ( 'NONE',  ( 12.77657003524999979, -16.68789974453000369, -0.1588669551756000109 ) ) ;
#53222 = CIRCLE ( 'NONE', #26823, 10.20000000000000107 ) ;
#53223 = CARTESIAN_POINT ( 'NONE',  ( -9.636781270573999691, -24.44031362782000016, -7.948066289838000564 ) ) ;
#53224 = CARTESIAN_POINT ( 'NONE',  ( -9.497676279887681261, -79.29010717161661148, 1.243618956522032581 ) ) ;
#53225 = VERTEX_POINT ( 'NONE', #5359 ) ;
#53226 = FACE_OUTER_BOUND ( 'NONE', #23798, .T. ) ;
#53227 = CYLINDRICAL_SURFACE ( 'NONE', #25894, 0.5000000000000004441 ) ;
#53228 = CARTESIAN_POINT ( 'NONE',  ( -8.148905501844000199, -78.76715395315800095, -8.781309899900000104 ) ) ;
#53229 = CARTESIAN_POINT ( 'NONE',  ( -9.641218323609999530, -17.56606991914999938, -7.943737929428000832 ) ) ;
#53231 = DIRECTION ( 'NONE',  ( 0.000000000000000000, 1.000000000000000000, 0.000000000000000000 ) ) ;
#53230 = CARTESIAN_POINT ( 'NONE',  ( 0.6054113949338107981, -78.46981924737423242, 9.249594591320265735 ) ) ;
#53232 = CARTESIAN_POINT ( 'NONE',  ( 3.654181830570000233, -86.12610001270999760, -1.626946572303000105 ) ) ;
#53233 = CARTESIAN_POINT ( 'NONE',  ( 10.35845608626999947, -60.09778754156999980, -7.627487525433000570 ) ) ;
#53234 = CARTESIAN_POINT ( 'NONE',  ( -12.05000000000000071, -75.80000000000001137, 0.000000000000000000 ) ) ;
#53235 = CARTESIAN_POINT ( 'NONE',  ( 1.514497777301999859, -77.68767547371999171, 11.15976079676000055 ) ) ;
#53236 = LINE ( 'NONE', #12784, #53383 ) ;
#53237 = CARTESIAN_POINT ( 'NONE',  ( -1.715212302772999742, -80.93623568429859461, -11.12438410773000186 ) ) ;
#53238 = ORIENTED_EDGE ( 'NONE', *, *, #36575, .F. ) ;
#53239 = CARTESIAN_POINT ( 'NONE',  ( 3.251169438796622124, -1.361878590890881702, 0.4257723127115868866 ) ) ;
#53240 = CARTESIAN_POINT ( 'NONE',  ( 1.666727925320000026, -55.60825518191999350, 12.50018462901999960 ) ) ;
#53241 = CARTESIAN_POINT ( 'NONE',  ( -12.92177931909999877, -20.24263462181000151, 2.062503053667999797 ) ) ;
#53242 = CARTESIAN_POINT ( 'NONE',  ( -1.744125200577000045, -3.548756781514999847, 2.929807332647999640 ) ) ;
#53243 = CARTESIAN_POINT ( 'NONE',  ( -9.457500717944000712, -78.24349181547098908, -6.031068363571000290 ) ) ;
#53244 = CARTESIAN_POINT ( 'NONE',  ( -7.596835002782709623, -77.35208333333333997, -5.838193839761696147 ) ) ;
#53245 = DIRECTION ( 'NONE',  ( -1.040691342546000016E-11, 1.000000000000000000, 2.038009761064000191E-09 ) ) ;
#53246 = CARTESIAN_POINT ( 'NONE',  ( 0.5390150933989998894, -62.06260891619000120, 12.77520261008999825 ) ) ;
#53247 = CARTESIAN_POINT ( 'NONE',  ( 12.77306291386999959, -16.94129324301999873, 1.041150512314999999 ) ) ;
#53248 = CARTESIAN_POINT ( 'NONE',  ( 3.474219449940000537, -82.38249735065198820, -1.986484532523000279 ) ) ;
#53249 = CARTESIAN_POINT ( 'NONE',  ( 0.000000000000000000, -87.59999999999999432, 0.000000000000000000 ) ) ;
#53250 = CARTESIAN_POINT ( 'NONE',  ( 10.66169269867642022, -77.16340856471717302, -5.782336216534432971 ) ) ;
#53251 = AXIS2_PLACEMENT_3D ( 'NONE', #1001, #18986, #46159 ) ;
#53252 = CARTESIAN_POINT ( 'NONE',  ( -3.527598694514999966, -78.37623792800799549, -10.69532371905999923 ) ) ;
#53253 = CARTESIAN_POINT ( 'NONE',  ( -14.00000000000000000, -9.295797029142999435, 0.000000000000000000 ) ) ;
#53254 = CARTESIAN_POINT ( 'NONE',  ( 0.07936805562503999878, -79.52232578389998707, -1.463935019116999747 ) ) ;
#53255 = AXIS2_PLACEMENT_3D ( 'NONE', #34560, #7423, #12993 ) ;
#53256 = CARTESIAN_POINT ( 'NONE',  ( 9.670530767802999250, -77.01847108759879745, -0.1674091926992999912 ) ) ;
#53257 = CARTESIAN_POINT ( 'NONE',  ( -1.143843590492619189, -82.69330820015007077, 0.9859688983279260022 ) ) ;
#53258 = CARTESIAN_POINT ( 'NONE',  ( -12.09999999997999964, -92.79999999999999716, -2.688213410018000232E-10 ) ) ;
#53259 = CARTESIAN_POINT ( 'NONE',  ( -5.945647593938746311, -80.17843449223505559, -8.956060015876818881 ) ) ;
#53260 = CARTESIAN_POINT ( 'NONE',  ( -9.393203674808267678, -77.04166666666665719, -5.413904038987171319 ) ) ;
#53261 = CARTESIAN_POINT ( 'NONE',  ( -10.42531125074000009, -18.73514854687000053, -7.624341767140999870 ) ) ;
#53262 = EDGE_CURVE ( 'NONE', #1042, #5144, #53558, .T. ) ;
#53263 = ORIENTED_EDGE ( 'NONE', *, *, #49590, .F. ) ;
#53264 = CARTESIAN_POINT ( 'NONE',  ( 8.441163350041684055, -53.88348045719643409, 9.243160719878805054 ) ) ;
#53265 = CIRCLE ( 'NONE', #49527, 2.799999999999999822 ) ;
#53266 = ADVANCED_FACE ( 'NONE', ( #45529 ), #36646, .F. ) ;
#53267 = DIRECTION ( 'NONE',  ( 0.000000000000000000, 1.000000000000000000, 0.000000000000000000 ) ) ;
#53268 = CARTESIAN_POINT ( 'NONE',  ( 7.942219812765999087, -79.63612155000399184, 7.984679643171000762 ) ) ;
#53269 = CARTESIAN_POINT ( 'NONE',  ( 10.75000000000000000, -77.35000000000000853, 0.000000000000000000 ) ) ;
#53270 = ORIENTED_EDGE ( 'NONE', *, *, #51262, .T. ) ;
#53271 = CARTESIAN_POINT ( 'NONE',  ( -0.06533073702471998978, -80.61372138577100088, -1.613397371670999947 ) ) ;
#53272 = ORIENTED_EDGE ( 'NONE', *, *, #43146, .F. ) ;
#53273 = DIRECTION ( 'NONE',  ( 4.079823248806000314E-14, 1.535319084990999808E-11, 1.000000000000000000 ) ) ;
#53274 = ORIENTED_EDGE ( 'NONE', *, *, #47411, .T. ) ;
#53275 = CARTESIAN_POINT ( 'NONE',  ( -10.98362417419999915, -18.84999999999999787, -0.5999999999999999778 ) ) ;
#53276 = CARTESIAN_POINT ( 'NONE',  ( 1.310679582531385279, -78.29166666666667140, 0.7554284705563519831 ) ) ;
#53277 = EDGE_CURVE ( 'NONE', #11044, #22044, #45822, .T. ) ;
#53278 = CARTESIAN_POINT ( 'NONE',  ( 10.63911585229000067, -78.84139468996799849, 2.446340097336999975 ) ) ;
#53279 = CARTESIAN_POINT ( 'NONE',  ( 0.006333666751365999749, -25.33262644299999877, -12.77652491955999992 ) ) ;
#53280 = CARTESIAN_POINT ( 'NONE',  ( -3.445809878667000170, -81.82057179202399766, 1.005057003444999930 ) ) ;
#53281 = CARTESIAN_POINT ( 'NONE',  ( -7.344791241739323517, -79.34486898742505900, 6.031409305879527949 ) ) ;
#53282 = ORIENTED_EDGE ( 'NONE', *, *, #41779, .F. ) ;
#53283 = CARTESIAN_POINT ( 'NONE',  ( 17.50000000000000000, -13.07071424677999971, 2.026616721661999859E-13 ) ) ;
#53284 = CARTESIAN_POINT ( 'NONE',  ( 9.965829256158000860, -78.80597494495999911, 7.308490088571999443 ) ) ;
#53285 = ORIENTED_EDGE ( 'NONE', *, *, #5550, .T. ) ;
#53286 = ORIENTED_EDGE ( 'NONE', *, *, #18886, .T. ) ;
#53287 = CARTESIAN_POINT ( 'NONE',  ( -1.302408693230432402, -77.79201247581434586, -0.7600488025388738578 ) ) ;
#53288 = CARTESIAN_POINT ( 'NONE',  ( -8.343860018000999190, -55.64999999967000122, 8.343860018000999190 ) ) ;
#53289 = CARTESIAN_POINT ( 'NONE',  ( -1.000649921775999873, -79.70818604951899999, 0.8816325131470000853 ) ) ;
#53290 = DIRECTION ( 'NONE',  ( 0.000000000000000000, -1.000000000000000000, 0.000000000000000000 ) ) ;
#53291 = CARTESIAN_POINT ( 'NONE',  ( -4.615324208696027775, -86.17851881763698429, -0.4418012292915585171 ) ) ;
#53293 = EDGE_CURVE ( 'NONE', #17043, #8334, #30281, .T. ) ;
#53292 = CARTESIAN_POINT ( 'NONE',  ( 3.572165910270233891, -85.80175210208024339, 0.8161875824647534250 ) ) ;
#53294 = CARTESIAN_POINT ( 'NONE',  ( -1.198731353186000215, -77.12333680668000113, -13.05866524906999970 ) ) ;
#53295 = CARTESIAN_POINT ( 'NONE',  ( 11.54974070075000014, -78.02769171769000423, 5.138670156068000594 ) ) ;
#53296 = ADVANCED_FACE ( 'NONE', ( #51414 ), #31560, .F. ) ;
#53297 = VECTOR ( 'NONE', #46688, 1000.000000000000114 ) ;
#53298 = CARTESIAN_POINT ( 'NONE',  ( 7.570062472618999116, -76.71279439517699927, -7.820779103414999156 ) ) ;
#53299 = CARTESIAN_POINT ( 'NONE',  ( -8.736253822433678096, -78.62667298105303360, -3.039731260859822370 ) ) ;
#53300 = CARTESIAN_POINT ( 'NONE',  ( 4.005932792494999894, -82.62224128856598782, -0.2640423048605999856 ) ) ;
#53301 = AXIS2_PLACEMENT_3D ( 'NONE', #23521, #1115, #36802 ) ;
#53302 = DIRECTION ( 'NONE',  ( 0.000000000000000000, -1.000000000000000000, 0.000000000000000000 ) ) ;
#53303 = CARTESIAN_POINT ( 'NONE',  ( -0.05688989330080245627, -2.976795852111999263, 3.249363959324195417 ) ) ;
#53304 = CARTESIAN_POINT ( 'NONE',  ( 3.380804078035000160, -82.41750264934799475, 0.3410251249121999950 ) ) ;
#53305 = CARTESIAN_POINT ( 'NONE',  ( -0.5668640726167896160, -24.91659694980447171, -12.50470739226977379 ) ) ;
#53306 = CARTESIAN_POINT ( 'NONE',  ( -7.960542989054001595, -80.83912993679970782, 7.971132368775000643 ) ) ;
#53307 = CARTESIAN_POINT ( 'NONE',  ( 3.190249742999000215, -1.952098507945999817, -2.075671974272999876 ) ) ;
#53308 = CARTESIAN_POINT ( 'NONE',  ( -1.085072108435533256, -80.29443781902547528, -0.6701691410297031526 ) ) ;
#53309 = ORIENTED_EDGE ( 'NONE', *, *, #14386, .T. ) ;
#53310 = DIRECTION ( 'NONE',  ( 0.000000000000000000, 1.000000000000000000, 0.000000000000000000 ) ) ;
#53311 = FACE_OUTER_BOUND ( 'NONE', #55385, .T. ) ;
#53312 = CARTESIAN_POINT ( 'NONE',  ( 1.221474390223999951, -81.43901740672500011, -0.5353283698298000326 ) ) ;
#53313 = CARTESIAN_POINT ( 'NONE',  ( -12.66737112516999986, -17.76697834132999887, -1.690666607834999891 ) ) ;
#53314 = CARTESIAN_POINT ( 'NONE',  ( 11.88928085110999966, -78.30064632562000781, 5.289737169833999886 ) ) ;
#53315 = CARTESIAN_POINT ( 'NONE',  ( 7.479111157460000214, -79.76976001420199225, -5.552063387031999753 ) ) ;
#53316 = CARTESIAN_POINT ( 'NONE',  ( 12.64500484465999897, -19.22847221992000044, -1.799490225533999732 ) ) ;
#53317 = ORIENTED_EDGE ( 'NONE', *, *, #8781, .T. ) ;
#53318 = CARTESIAN_POINT ( 'NONE',  ( -3.453171399369999950, -1.863032031399000088, -0.5706200895263999762 ) ) ;
#53319 = CARTESIAN_POINT ( 'NONE',  ( 9.322139347623476624, -76.97083333334067845, -1.984632901571217412 ) ) ;
#53320 = CARTESIAN_POINT ( 'NONE',  ( 0.5455113502570001494, -82.08278176514200197, 1.191738699715000127 ) ) ;
#53321 = CARTESIAN_POINT ( 'NONE',  ( -11.68767212001978706, -78.92083333333333428, -3.140974612311364655 ) ) ;
#53322 = CARTESIAN_POINT ( 'NONE',  ( 2.192362874646999860, -79.16451892421298453, -9.154492618432000128 ) ) ;
#53323 = CARTESIAN_POINT ( 'NONE',  ( 4.171966157921000118, -82.45880512652999528, -0.06563631418457001321 ) ) ;
#53324 = CARTESIAN_POINT ( 'NONE',  ( -1.215378159391584223, -79.98441448756166494, 10.68123553570516293 ) ) ;
#53325 = CARTESIAN_POINT ( 'NONE',  ( -0.3164422402712000482, -79.49559824363400651, 1.381999876370000102 ) ) ;
#53326 = ORIENTED_EDGE ( 'NONE', *, *, #54435, .F. ) ;
#53327 = CARTESIAN_POINT ( 'NONE',  ( 5.810395355999260936, -77.27055076788118981, -9.061764198440011242 ) ) ;
#53328 = CARTESIAN_POINT ( 'NONE',  ( 0.1738511560287839264, -82.16536458333123960, 1.334635416660091556 ) ) ;
#53329 = CARTESIAN_POINT ( 'NONE',  ( -3.407095545933028991, -78.77851879815550262, 6.814191091866018013 ) ) ;
#53330 = ORIENTED_EDGE ( 'NONE', *, *, #34578, .F. ) ;
#53331 = ORIENTED_EDGE ( 'NONE', *, *, #17231, .T. ) ;
#53332 = CARTESIAN_POINT ( 'NONE',  ( -9.937637090044999510, -79.77094125464398644, 4.829168387547000840 ) ) ;
#53333 = CARTESIAN_POINT ( 'NONE',  ( -8.140250184780514431, -55.34839576620330348, -7.398464061247827850 ) ) ;
#53334 = AXIS2_PLACEMENT_3D ( 'NONE', #27012, #40007, #26423 ) ;
#53335 = CARTESIAN_POINT ( 'NONE',  ( -10.52185994994999874, -79.89900688576899768, -3.892032218524000164 ) ) ;
#53336 = VERTEX_POINT ( 'NONE', #53720 ) ;
#53337 = ORIENTED_EDGE ( 'NONE', *, *, #45921, .F. ) ;
#53338 = CONICAL_SURFACE ( 'NONE', #55242, 10.84999999997999964, 0.7853981633972997312 ) ;
#53339 = ORIENTED_EDGE ( 'NONE', *, *, #27593, .T. ) ;
#53340 = CIRCLE ( 'NONE', #35405, 4.799999999999999822 ) ;
#53341 = B_SPLINE_SURFACE_WITH_KNOTS ( 'NONE', 3, 3, ( 
 ( #14973, #55130, #14675, #33265 ),
 ( #6122, #11155, #38284, #46883 ),
 ( #28246, #51883, #56305, #23540 ),
 ( #6414, #24427, #42443, #2010 ),
 ( #24718, #15859, #5825, #29129 ),
 ( #20009, #33845, #20289, #37991 ),
 ( #50725, #47177, #46300, #6708 ),
 ( #46009, #41554, #19124, #5531 ),
 ( #10267, #41848, #37406, #55427 ),
 ( #47752, #34423, #34995, #48323 ),
 ( #52172, #21438, #39448, #57161 ) ),
 .UNSPECIFIED., .F., .F., .F.,
 ( 4, 1, 1, 1, 1, 1, 1, 1, 4 ),
 ( 4, 4 ),
 ( -0.01994534136796000112, 0.000000000000000000, 0.1666666666667000196, 0.3333333333333000081, 0.5000000000000000000, 0.6666666666667000474, 0.8333333333333000637, 1.000000000000000000, 1.020519780480000138 ),
 ( -0.3582002740325999635, 1.358566136073000141 ),
 .UNSPECIFIED. ) ;
#53342 = EDGE_CURVE ( 'NONE', #36311, #35802, #29599, .T. ) ;
#53343 = CARTESIAN_POINT ( 'NONE',  ( 10.27275293713955584, -77.98886745049749436, 5.919664110522427691 ) ) ;
#53344 = DIRECTION ( 'NONE',  ( 1.000000000000000000, 0.000000000000000000, 0.000000000000000000 ) ) ;
#53345 = ORIENTED_EDGE ( 'NONE', *, *, #53777, .F. ) ;
#53346 = CARTESIAN_POINT ( 'NONE',  ( -1.199173895638943721, -81.84803276288215557, 0.9215510758497256205 ) ) ;
#53347 = ORIENTED_EDGE ( 'NONE', *, *, #14180, .T. ) ;
#53348 = CARTESIAN_POINT ( 'NONE',  ( -0.3055749384948234781, -80.54406969723000032, 1.237013315672344627 ) ) ;
#53349 = CARTESIAN_POINT ( 'NONE',  ( 2.103055900234938491, -78.99318692614359350, -3.641429946303727405 ) ) ;
#53350 = DIRECTION ( 'NONE',  ( 0.000000000000000000, -1.000000000000000000, 0.000000000000000000 ) ) ;
#53351 = CARTESIAN_POINT ( 'NONE',  ( 0.5999663639300889528, -18.81035107904150294, 10.98362601162691377 ) ) ;
#53352 = CARTESIAN_POINT ( 'NONE',  ( -9.599999999999999645, -87.29999999999999716, 0.000000000000000000 ) ) ;
#53353 = CARTESIAN_POINT ( 'NONE',  ( -1.708367912329182836, -80.96267845950610820, -11.07999331822880507 ) ) ;
#53354 = ADVANCED_FACE ( 'NONE', ( #26534 ), #45360, .F. ) ;
#53355 = CARTESIAN_POINT ( 'NONE',  ( 7.626500777218999438, -55.48415267986000288, -10.35747145890000098 ) ) ;
#53356 = CARTESIAN_POINT ( 'NONE',  ( 9.143727524999398781, -78.83803687086303569, -1.399743652968158836 ) ) ;
#53357 = DIRECTION ( 'NONE',  ( 0.000000000000000000, 1.000000000000000000, 0.000000000000000000 ) ) ;
#53358 = CARTESIAN_POINT ( 'NONE',  ( -4.170645326359000649, -80.13275264934799225, 0.1879290872891999920 ) ) ;
#53359 = CARTESIAN_POINT ( 'NONE',  ( -9.594333265089000307, -77.77168667140099956, -1.805238218963999941 ) ) ;
#53360 = CARTESIAN_POINT ( 'NONE',  ( -13.89999999994000035, -80.79999999994109317, -2.316526479204000061E-09 ) ) ;
#53361 = CARTESIAN_POINT ( 'NONE',  ( 0.000000000000000000, -5.000000000000000000, 0.000000000000000000 ) ) ;
#53362 = CARTESIAN_POINT ( 'NONE',  ( -1.698401934077000019, -24.22014045903999957, 12.66748707612999958 ) ) ;
#53363 = CARTESIAN_POINT ( 'NONE',  ( -8.084233020759592492, -80.04022715548097722, 7.554717540679545706 ) ) ;
#53364 = CARTESIAN_POINT ( 'NONE',  ( -10.74970698200568897, -78.10629880980414441, -0.8321373431320605585 ) ) ;
#53365 = CARTESIAN_POINT ( 'NONE',  ( 1.498260933585416455, -80.11042203568169384, 0.2089178497027620873 ) ) ;
#53366 = CARTESIAN_POINT ( 'NONE',  ( 12.66314513620999804, -61.97864743329000703, 0.04033065750138999789 ) ) ;
#53367 = CARTESIAN_POINT ( 'NONE',  ( -12.00000000000000000, -23.15000000000000213, 0.000000000000000000 ) ) ;
#53368 = CARTESIAN_POINT ( 'NONE',  ( 0.000000000000000000, -78.69999999999998863, 0.000000000000000000 ) ) ;
#53369 = EDGE_CURVE ( 'NONE', #37236, #41372, #4859, .T. ) ;
#53370 = CARTESIAN_POINT ( 'NONE',  ( -10.64055841416000092, -78.54452889900299795, -2.440058154124999934 ) ) ;
#53371 = CIRCLE ( 'NONE', #35450, 5.000000000000000000 ) ;
#53372 = CARTESIAN_POINT ( 'NONE',  ( 8.042137835475001495, -77.25865908154399619, 9.127242153301999394 ) ) ;
#53374 = CARTESIAN_POINT ( 'NONE',  ( -7.678655902612509188, -18.20623020282190296, 10.03844298039528127 ) ) ;
#53373 = CARTESIAN_POINT ( 'NONE',  ( 0.000000000000000000, -23.84999999976950136, -11.89999999977000122 ) ) ;
#53375 = CARTESIAN_POINT ( 'NONE',  ( -1.295013057735999951, -81.60307101349998504, -0.3858917059242000236 ) ) ;
#53376 = CARTESIAN_POINT ( 'NONE',  ( -7.492394017799830941, -79.53652907763523672, 7.710241490960848765 ) ) ;
#53377 = VECTOR ( 'NONE', #48320, 1000.000000000000114 ) ;
#53378 = ORIENTED_EDGE ( 'NONE', *, *, #29617, .F. ) ;
#53379 = VECTOR ( 'NONE', #45871, 1000.000000000000000 ) ;
#53380 = CARTESIAN_POINT ( 'NONE',  ( -10.38646360829000059, -22.77795407709999864, -7.655555357433999397 ) ) ;
#53381 = CARTESIAN_POINT ( 'NONE',  ( 12.06518374142000027, -79.49911536532098921, -1.485411366123999821 ) ) ;
#53382 = FACE_OUTER_BOUND ( 'NONE', #26188, .T. ) ;
#53383 = VECTOR ( 'NONE', #30782, 1000.000000000000000 ) ;
#53384 = DIRECTION ( 'NONE',  ( 0.000000000000000000, -1.000000000000000000, 0.000000000000000000 ) ) ;
#53385 = CARTESIAN_POINT ( 'NONE',  ( -9.934814764497000183, -61.42368287795999748, 7.968971842771999547 ) ) ;
#53386 = CARTESIAN_POINT ( 'NONE',  ( -1.160983053055000047, -1.445977233352999880, 3.343027787781999827 ) ) ;
#53387 = CARTESIAN_POINT ( 'NONE',  ( 9.354045381180000618, -79.98053041167199240, 2.857433141267999854 ) ) ;
#53388 = CARTESIAN_POINT ( 'NONE',  ( -2.597362135797363525, -3.152356596647883258, -1.996591761881967075 ) ) ;
#53389 = CARTESIAN_POINT ( 'NONE',  ( -1.931086388455000025, -55.50221404479999876, 12.71798280852999952 ) ) ;
#53390 = ORIENTED_EDGE ( 'NONE', *, *, #22230, .T. ) ;
#53391 = DIRECTION ( 'NONE',  ( 0.000000000000000000, 0.000000000000000000, -1.000000000000000000 ) ) ;
#53392 = CARTESIAN_POINT ( 'NONE',  ( -12.60356226362999976, -59.55077028856999988, 1.750000000000000000 ) ) ;
#53393 = CARTESIAN_POINT ( 'NONE',  ( 9.500000000000000000, -78.54999999999999716, 0.000000000000000000 ) ) ;
#53394 = CARTESIAN_POINT ( 'NONE',  ( 3.485499217011999828, -78.48547957940618858, 0.000000000000000000 ) ) ;
#53395 = CARTESIAN_POINT ( 'NONE',  ( 0.1745292062968000213, -85.79442953870898236, 3.543168428762999866 ) ) ;
#53396 = ORIENTED_EDGE ( 'NONE', *, *, #34578, .T. ) ;
#53397 = CARTESIAN_POINT ( 'NONE',  ( -12.50000000000000000, -18.75000000000000000, 0.000000000000000000 ) ) ;
#53398 = CARTESIAN_POINT ( 'NONE',  ( 11.37980319050488198, -77.92613131821927652, -3.047449828435636388 ) ) ;
#53399 = DIRECTION ( 'NONE',  ( 0.000000000000000000, 1.000000000000000000, 0.000000000000000000 ) ) ;
#53400 = ORIENTED_EDGE ( 'NONE', *, *, #50576, .T. ) ;
#53401 = CARTESIAN_POINT ( 'NONE',  ( 0.000000000000000000, -76.29999999999999716, 0.000000000000000000 ) ) ;
#53402 = ADVANCED_FACE ( 'NONE', ( #12109 ), #22636, .F. ) ;
#53403 = CARTESIAN_POINT ( 'NONE',  ( 8.249323304235000265, -79.97488639496098983, -5.229696851825000437 ) ) ;
#53404 = ORIENTED_EDGE ( 'NONE', *, *, #23023, .T. ) ;
#53405 = ORIENTED_EDGE ( 'NONE', *, *, #12045, .T. ) ;
#53406 = CARTESIAN_POINT ( 'NONE',  ( 0.03269534938340999675, -76.06591632114400170, 11.81851555469000026 ) ) ;
#53407 = CYLINDRICAL_SURFACE ( 'NONE', #23983, 12.00000000000000000 ) ;
#53408 = ADVANCED_FACE ( 'NONE', ( #38325 ), #29172, .T. ) ;
#53409 = CARTESIAN_POINT ( 'NONE',  ( 0.3914697351672000170, -79.41551968470000133, -1.482475952910999872 ) ) ;
#53410 = ORIENTED_EDGE ( 'NONE', *, *, #1537, .T. ) ;
#53411 = DIRECTION ( 'NONE',  ( 0.000000000000000000, -1.000000000000000000, 0.000000000000000000 ) ) ;
#53412 = AXIS2_PLACEMENT_3D ( 'NONE', #33353, #46680, #20655 ) ;
#53413 = CYLINDRICAL_SURFACE ( 'NONE', #881, 1.750000000000001332 ) ;
#53414 = PLANE ( 'NONE',  #51807 ) ;
#53415 = CARTESIAN_POINT ( 'NONE',  ( 0.004398891372963634194, -80.22583377693190698, -1.249663113230017997 ) ) ;
#53416 = CARTESIAN_POINT ( 'NONE',  ( 9.246161438659999732, -76.68655867677999538, -8.285323839175999794 ) ) ;
#53417 = PRODUCT_DEFINITION_CONTEXT ( 'detailed design', #45119, 'design' ) ;
#53418 = CIRCLE ( 'NONE', #54421, 12.50000000000000000 ) ;
#53419 = CARTESIAN_POINT ( 'NONE',  ( -8.500000000000000000, -5.000000000000000000, 0.000000000000000000 ) ) ;
#53420 = CARTESIAN_POINT ( 'NONE',  ( 0.000000000000000000, -26.30294702885999669, 12.53545825868000207 ) ) ;
#53421 = CARTESIAN_POINT ( 'NONE',  ( 4.268285239867531722, -86.40321104920798234, 0.4899302694419261917 ) ) ;
#53422 = CARTESIAN_POINT ( 'NONE',  ( 3.507155896972999898, -79.25137714550699286, 10.65448112794999957 ) ) ;
#53423 = CARTESIAN_POINT ( 'NONE',  ( -1.719802448987169274, -79.99009311709434655, 9.096255206201579568 ) ) ;
#53424 = EDGE_CURVE ( 'NONE', #39336, #5887, #45842, .T. ) ;
#53425 = CIRCLE ( 'NONE', #8179, 9.499999999999996447 ) ;
#53426 = CARTESIAN_POINT ( 'NONE',  ( 10.10448976475663407, -17.54884052604848677, 7.864761218169358692 ) ) ;
#53427 = ORIENTED_EDGE ( 'NONE', *, *, #48627, .F. ) ;
#53428 = CARTESIAN_POINT ( 'NONE',  ( 6.245083526999000156, -78.79256869612397907, -9.376985981987999708 ) ) ;
#53429 = CARTESIAN_POINT ( 'NONE',  ( 3.003484176522146054, -77.25148415549074343, -8.748772631339541306 ) ) ;
#53430 = CARTESIAN_POINT ( 'NONE',  ( -1.341023944040999893, -79.30986310998500244, -0.2092349045463000046 ) ) ;
#53431 = AXIS2_PLACEMENT_3D ( 'NONE', #47220, #11197, #38619 ) ;
#53432 = CARTESIAN_POINT ( 'NONE',  ( -1.281518013001000211, -77.67713930981540216, -0.3132342491214999969 ) ) ;
#53433 = CARTESIAN_POINT ( 'NONE',  ( -3.101110553533934944, -3.388432628819295633, -1.664369434271149473 ) ) ;
#53434 = CARTESIAN_POINT ( 'NONE',  ( -9.841113773978118928, -17.16371975942079686, 8.121706172286355496 ) ) ;
#53435 = B_SPLINE_CURVE_WITH_KNOTS ( 'NONE', 3,
 ( #21484, #17339, #53654, #21765, #3478, #4350 ),
 .UNSPECIFIED., .F., .F.,
 ( 4, 1, 1, 4 ),
 ( 0.000000000000000000, 0.3333333333333000081, 0.6666666666667000474, 1.000000000000000000 ),
 .UNSPECIFIED. ) ;
#53436 = DIRECTION ( 'NONE',  ( 0.000000000000000000, -1.000000000000000000, 0.000000000000000000 ) ) ;
#53437 = DIRECTION ( 'NONE',  ( -0.7071067811865470176, -0.7071067811865470176, -3.680441369915245526E-08 ) ) ;
#53438 = CARTESIAN_POINT ( 'NONE',  ( -7.632977269198000236, -79.12198591599799613, -8.138136006783000198 ) ) ;
#53439 = CARTESIAN_POINT ( 'NONE',  ( -9.539271075714001569, -76.93226332859899230, 1.308743492807000086 ) ) ;
#53440 = LINE ( 'NONE', #30411, #5554 ) ;
#53441 = CARTESIAN_POINT ( 'NONE',  ( -1.155567653434479647, -83.06898091192337574, 0.4764477841603429464 ) ) ;
#53442 = CARTESIAN_POINT ( 'NONE',  ( -6.206245474241998572, -79.67165790279912585, 9.343480492029000217 ) ) ;
#53443 = CARTESIAN_POINT ( 'NONE',  ( 10.47020627418438643, -77.77083333333334281, 2.813789756862283387 ) ) ;
#53444 = ORIENTED_EDGE ( 'NONE', *, *, #5485, .F. ) ;
#53445 = CARTESIAN_POINT ( 'NONE',  ( -0.6483708932059000229, -82.48482063826099875, -1.447070110047999902 ) ) ;
#53446 = CARTESIAN_POINT ( 'NONE',  ( -0.4789091134304000463, -81.55216508874998738, -1.232458658897999992 ) ) ;
#53447 = CYLINDRICAL_SURFACE ( 'NONE', #47439, 10.75000000000000000 ) ;
#53448 = CARTESIAN_POINT ( 'NONE',  ( -5.261498566940000288, -77.58713293807399225, -10.76255997729999869 ) ) ;
#53449 = CARTESIAN_POINT ( 'NONE',  ( -9.326074664721659246, -79.95762289869909978, 5.512178488021413969 ) ) ;
#53450 = CARTESIAN_POINT ( 'NONE',  ( 0.7735502751808678301, -78.92691180497098458, -1.012571407719350614 ) ) ;
#53451 = CARTESIAN_POINT ( 'NONE',  ( 6.420671964385999964, -77.74679431087899673, -10.06034164291999922 ) ) ;
#53452 = CARTESIAN_POINT ( 'NONE',  ( -7.401612602209000968, -79.06599415034600042, -6.305503003149000030 ) ) ;
#53453 = CARTESIAN_POINT ( 'NONE',  ( -9.628933692773001596, -78.70852403778498285, -0.1919528651714999812 ) ) ;
#53454 = CARTESIAN_POINT ( 'NONE',  ( -1.200170490674999924, -54.36594297968999712, -12.43444080546999864 ) ) ;
#53455 = CARTESIAN_POINT ( 'NONE',  ( 10.86825241270809173, -75.98052679898808037, 4.465012754454932953 ) ) ;
#53456 = CARTESIAN_POINT ( 'NONE',  ( 1.533375225219753890, -85.83735716284299144, 3.533266005812401023 ) ) ;
#53457 = ORIENTED_EDGE ( 'NONE', *, *, #27467, .T. ) ;
#53458 = CARTESIAN_POINT ( 'NONE',  ( -1.140226658635644874, -79.53775969004662727, -0.5918896188630813349 ) ) ;
#53459 = CARTESIAN_POINT ( 'NONE',  ( 1.460959015002472494, -79.17083333333334849, 0.3926218265389232465 ) ) ;
#53460 = CARTESIAN_POINT ( 'NONE',  ( -5.346699159600342810, -78.78725806292474942, -10.49909549695743749 ) ) ;
#53461 = CARTESIAN_POINT ( 'NONE',  ( -2.218416052576314801, -78.39678895079168797, -3.679255452198593179 ) ) ;
#53462 = CARTESIAN_POINT ( 'NONE',  ( 1.571434226476000173, -83.05267929568199747, -0.5530452149683998675 ) ) ;
#53463 = CARTESIAN_POINT ( 'NONE',  ( 10.34070037867000202, -78.05223280600100111, -4.346035695907999319 ) ) ;
#53464 = CARTESIAN_POINT ( 'NONE',  ( -10.79326785783000098, -79.44467717776498716, -1.992331681952000055 ) ) ;
#53465 = CARTESIAN_POINT ( 'NONE',  ( -6.634986530482820832, -80.40442708333218036, 8.632259101794380385 ) ) ;
#53466 = CARTESIAN_POINT ( 'NONE',  ( -1.041600863181999959, -76.62709993674098996, -12.22549076760999931 ) ) ;
#53467 = CARTESIAN_POINT ( 'NONE',  ( 3.768652233081607683, -78.54757323232175281, 11.12973672322252305 ) ) ;
#53468 = CARTESIAN_POINT ( 'NONE',  ( -8.485281374238999419, -60.04999999966999980, -8.485281374238999419 ) ) ;
#53469 = ORIENTED_EDGE ( 'NONE', *, *, #26612, .F. ) ;
#53470 = AXIS2_PLACEMENT_3D ( 'NONE', #37391, #28234, #51291 ) ;
#53471 = ADVANCED_FACE ( 'NONE', ( #1468 ), #15819, .T. ) ;
#53472 = CARTESIAN_POINT ( 'NONE',  ( -6.220196401501000061, -78.71846735336799838, -9.111031286755999048 ) ) ;
#53473 = CARTESIAN_POINT ( 'NONE',  ( 0.1339442445619486721, -79.96711704085768702, 1.244995031654752893 ) ) ;
#53474 = DIRECTION ( 'NONE',  ( -1.000000000000000000, 0.000000000000000000, 0.000000000000000000 ) ) ;
#53475 = CONICAL_SURFACE ( 'NONE', #8204, 9.649999999844000698, 0.7853981633972997312 ) ;
#53476 = TOROIDAL_SURFACE ( 'NONE', #51607, 17.50000000000000000, 5.000000000000000000 ) ;
#53477 = CARTESIAN_POINT ( 'NONE',  ( 6.722579162784999340, -79.56660374219698895, 8.904972230874999894 ) ) ;
#53478 = FACE_OUTER_BOUND ( 'NONE', #32603, .T. ) ;
#53479 = VECTOR ( 'NONE', #10484, 1000.000000000000000 ) ;
#53480 = CARTESIAN_POINT ( 'NONE',  ( -0.3340625910779762009, -81.45658993897731648, -1.473584088927320623 ) ) ;
#53481 = CARTESIAN_POINT ( 'NONE',  ( -12.26242965668000018, -78.32234609596400787, 0.6546740380507000134 ) ) ;
#53482 = LINE ( 'NONE', #13023, #32730 ) ;
#53483 = CARTESIAN_POINT ( 'NONE',  ( 8.251806177693529420, -17.19944067082483841, -9.431051272833316901 ) ) ;
#53484 = CARTESIAN_POINT ( 'NONE',  ( 10.75000000000000000, -78.25000000000000000, 1.005550720961999908E-14 ) ) ;
#53485 = CARTESIAN_POINT ( 'NONE',  ( -12.43356840162999966, -24.71269674488000234, 0.8410229959428999758 ) ) ;
#53486 = ORIENTED_EDGE ( 'NONE', *, *, #28500, .F. ) ;
#53487 = ORIENTED_EDGE ( 'NONE', *, *, #5166, .F. ) ;
#53488 = DIRECTION ( 'NONE',  ( 0.000000000000000000, 1.000000000000000000, 0.000000000000000000 ) ) ;
#53489 = ADVANCED_FACE ( 'NONE', ( #27644 ), #49522, .T. ) ;
#53490 = ORIENTED_EDGE ( 'NONE', *, *, #45774, .F. ) ;
#53491 = CARTESIAN_POINT ( 'NONE',  ( -1.777672186646999997, -78.93857582459999378, 12.13420648597999829 ) ) ;
#53492 = ORIENTED_EDGE ( 'NONE', *, *, #44468, .F. ) ;
#53493 = CARTESIAN_POINT ( 'NONE',  ( 8.950141054446001831, -25.20112627276999717, 8.958565985356999661 ) ) ;
#53494 = B_SPLINE_CURVE_WITH_KNOTS ( 'NONE', 3,
 ( #44241, #12368, #8811, #39800, #30645, #26803, #9112, #7934, #39518, #43961, #48680, #25935, #3511, #21512, #57523, #35066, #53103, #8224 ),
 .UNSPECIFIED., .F., .F.,
 ( 4, 2, 2, 2, 2, 2, 2, 2, 4 ),
 ( 0.000000000000000000, 0.1249999999999999445, 0.2499999999999998890, 0.3749999999999999445, 0.5000000000000000000, 0.6250000000000000000, 0.7500000000000001110, 0.8750000000000000000, 1.000000000000000000 ),
 .UNSPECIFIED. ) ;
#53495 = CARTESIAN_POINT ( 'NONE',  ( -8.838907858698000553, -78.66288998579800307, -3.964206742940000083 ) ) ;
#53496 = CARTESIAN_POINT ( 'NONE',  ( -12.50745077490000057, -24.99994448286999926, -2.662114616045000020E-09 ) ) ;
#53497 = CARTESIAN_POINT ( 'NONE',  ( -1.639962962630000076, -78.58499365464699338, 11.09633417262999977 ) ) ;
#53498 = CARTESIAN_POINT ( 'NONE',  ( -0.7617914920845411109, -79.52766219886571264, 0.9938330950829512567 ) ) ;
#53499 = ADVANCED_FACE ( 'NONE', ( #18808 ), #31191, .F. ) ;
#53500 = ORIENTED_EDGE ( 'NONE', *, *, #53021, .F. ) ;
#53501 = ORIENTED_EDGE ( 'NONE', *, *, #27937, .F. ) ;
#53502 = CARTESIAN_POINT ( 'NONE',  ( -1.866732844877771580, -77.49119273318581236, 9.060374038664914309 ) ) ;
#53503 = CARTESIAN_POINT ( 'NONE',  ( 10.71768947918000059, -78.04727784723098694, -1.656903943290000125 ) ) ;
#53504 = EDGE_CURVE ( 'NONE', #11048, #45504, #54817, .T. ) ;
#53505 = CARTESIAN_POINT ( 'NONE',  ( -4.784380313523539208, -77.48333333333332007, -8.300970689365453126 ) ) ;
#53506 = AXIS2_PLACEMENT_3D ( 'NONE', #6324, #28747, #24341 ) ;
#53507 = CARTESIAN_POINT ( 'NONE',  ( -7.707166124622999881, -77.38212234465098049, -5.896629607976000109 ) ) ;
#53508 = CARTESIAN_POINT ( 'NONE',  ( -12.80447607892999962, -76.33341425608999486, -0.3146157217153000007 ) ) ;
#53509 = CARTESIAN_POINT ( 'NONE',  ( -8.578468486503851409, -79.43533626687298010, -4.083052076949801545 ) ) ;
#53510 = LINE ( 'NONE', #30189, #2578 ) ;
#53511 = CARTESIAN_POINT ( 'NONE',  ( -4.017143116098000455, -80.33419522547698932, 10.51352533724000082 ) ) ;
#53512 = DIRECTION ( 'NONE',  ( 0.000000000000000000, -0.7071067811866525998, -0.7071067811864425456 ) ) ;
#53513 = CARTESIAN_POINT ( 'NONE',  ( 0.6295237254636258939, -78.16666666666665719, -1.092232985442821658 ) ) ;
#53514 = CARTESIAN_POINT ( 'NONE',  ( -1.210822168571057400, -78.61458333333332860, -9.250000000000001776 ) ) ;
#53515 = EDGE_LOOP ( 'NONE', ( #32779, #4320, #11125, #18229 ) ) ;
#53516 = CARTESIAN_POINT ( 'NONE',  ( -0.4732869866705000095, -79.06307788497599631, -12.30780274174999889 ) ) ;
#53517 = CARTESIAN_POINT ( 'NONE',  ( -7.753900686106000251, -54.51068035512000165, 10.31980286347000053 ) ) ;
#53518 = CARTESIAN_POINT ( 'NONE',  ( -4.118243260437115971, -78.00630453228950500, 9.929863582829632662 ) ) ;
#53519 = CARTESIAN_POINT ( 'NONE',  ( 3.925078296951999501, -78.48233087649200002, 11.31856107452000160 ) ) ;
#53520 = CARTESIAN_POINT ( 'NONE',  ( -12.76303204298000082, -60.06485150663000638, 1.980584515756000030 ) ) ;
#53522 = DIRECTION ( 'NONE',  ( 0.000000000000000000, -1.000000000000000000, 0.000000000000000000 ) ) ;
#53521 = LINE ( 'NONE', #20782, #24064 ) ;
#53523 = EDGE_CURVE ( 'NONE', #46987, #6045, #54786, .T. ) ;
#53524 = VECTOR ( 'NONE', #8232, 1000.000000000000000 ) ;
#53525 = CARTESIAN_POINT ( 'NONE',  ( 0.6454797251636636979, -53.91193487831556297, 12.50471521364905136 ) ) ;
#53526 = CARTESIAN_POINT ( 'NONE',  ( 10.38646360829000059, -56.02204592290999585, -7.655555357438999842 ) ) ;
#53527 = CARTESIAN_POINT ( 'NONE',  ( 8.485281374238999419, 0.000000000000000000, -8.485281374238999419 ) ) ;
#53528 = CARTESIAN_POINT ( 'NONE',  ( 11.24465069584000076, -78.06898427574600419, -0.6259355293341001270 ) ) ;
#53529 = DIRECTION ( 'NONE',  ( 0.000000000000000000, -0.1122098755727947705, -0.9936845293270585300 ) ) ;
#53530 = CARTESIAN_POINT ( 'NONE',  ( -9.248645349825999062, -80.77514956827684500, 6.415315719250000548 ) ) ;
#53531 = ORIENTED_EDGE ( 'NONE', *, *, #5120, .F. ) ;
#53532 = LINE ( 'NONE', #48820, #19729 ) ;
#53533 = CARTESIAN_POINT ( 'NONE',  ( -1.629367637664000057, -55.11736356569000606, 12.46114270824000059 ) ) ;
#53534 = CARTESIAN_POINT ( 'NONE',  ( 7.624341764926000131, -23.26485149464000202, -10.42531124853000080 ) ) ;
#53535 = CARTESIAN_POINT ( 'NONE',  ( -1.162378416399999947, -1.642324315393999923, -3.286269575089999950 ) ) ;
#53536 = B_SPLINE_CURVE_WITH_KNOTS ( 'NONE', 3,
 ( #9849, #23416, #41428, #1013, #14551, #50590 ),
 .UNSPECIFIED., .F., .F.,
 ( 4, 1, 1, 4 ),
 ( 0.000000000000000000, 0.3333333333333000081, 0.6666666666667000474, 1.000000000000000000 ),
 .UNSPECIFIED. ) ;
#53537 = CARTESIAN_POINT ( 'NONE',  ( -4.692196280270000130, -79.60434362032799527, -8.173708953481000350 ) ) ;
#53538 = CARTESIAN_POINT ( 'NONE',  ( -2.839805762151337731, -1.541666666666666519, -1.636761686205423949 ) ) ;
#53539 = DIRECTION ( 'NONE',  ( 0.000000000000000000, 0.000000000000000000, -1.000000000000000000 ) ) ;
#53540 = CARTESIAN_POINT ( 'NONE',  ( -1.798954018877999994, -60.01530973353999343, 12.61117007304000026 ) ) ;
#53541 = CARTESIAN_POINT ( 'NONE',  ( 12.68625206996000010, -18.23580249185999946, 1.886949102778999965 ) ) ;
#53542 = EDGE_CURVE ( 'NONE', #22144, #23718, #4936, .T. ) ;
#53543 = CARTESIAN_POINT ( 'NONE',  ( 3.635062440651000149, -85.62924735065199400, 2.053270061586999873 ) ) ;
#53544 = CARTESIAN_POINT ( 'NONE',  ( -6.100000000000000533, -80.79999999999999716, 0.000000000000000000 ) ) ;
#53545 = EDGE_CURVE ( 'NONE', #37205, #46203, #32645, .T. ) ;
#53546 = CARTESIAN_POINT ( 'NONE',  ( -11.81296717809978780, -76.93658351881686031, 2.479319390824800795 ) ) ;
#53547 = CARTESIAN_POINT ( 'NONE',  ( -3.734482694269000369, -78.39436234271001069, 11.50161222062999933 ) ) ;
#53548 = B_SPLINE_SURFACE_WITH_KNOTS ( 'NONE', 3, 3, ( 
 ( #24814, #43119, #51700, #30378, #34228, #48417, #29795, #47277, #47571, #42829, #30083, #56404, #2679, #16826, #3252, #38960, #33944, #52264, #43697, #20673, #42539, #47850, #7380, #25381, #21242, #43396, #2958, #20106, #34515, #34808, #56973, #16535, #52546, #31542, #35378 ),
 ( #49587, #54009, #35090, #53403, #57836, #17103, #44854, #12673, #44262, #35684, #58130, #17694, #26246, #49284, #4106, #22108, #13, #53124, #12951, #30664, #48701, #40117, #45159, #57544, #13842, #53712, #39822, #44554, #3817, #49883, #36284, #13249, #31242, #8244, #21819 ),
 ( #30949, #26527, #43978, #48988, #40421, #8533, #8835, #17393, #26824, #54306, #4406, #22408, #13550, #31840, #17992, #35984, #312, #9134, #40720, #27118, #4708, #39538, #25955, #22706, #3530, #18290, #21533, #54874, #18583, #37445, #4995, #50465, #42182, #28584, #46334 ),
 ( #15011, #18868, #14424, #1751, #5860, #37154, #10017, #27995, #32418, #46043, #55169, #55764, #55463, #14132, #33004, #51051, #50761, #5568, #10306, #10599, #46627, #36572, #27417, #6158, #9717, #24166, #37741, #19746, #14711, #45452, #23576, #32709, #27705, #41592, #15310 ),
 ( #9428, #1172, #41300, #19161, #28285, #23869, #41883, #33303, #22999, #1461, #19451, #41011, #603, #50172, #54596, #32131, #45751, #5284, #23292, #884, #36861, #11756, #38033, #11189, #2614, #25033, #43053, #51635, #16185, #29448, #47506, #25320, #42475, #38319, #2044 ),
 ( #34164, #56339, #7032, #20045, #52486, #29165, #15892, #16472, #29735, #56053, #12042, #43336, #38895, #38611, #20610, #52201, #56626, #47785, #7316, #15602, #33878, #56916, #3190, #21178, #48077, #2893, #20890, #10898, #34454, #33596, #47212, #28874, #25605, #30022, #7605 ),
 ( #6447, #39181, #43628, #57196, #16764, #6741, #51917, #24752, #51339, #46920, #11477, #24463, #42768, #2327, #20323, #30890, #22339, #44203, #22642, #35312, #12609, #3465, #40354, #17326, #30604, #45087, #26756, #13479, #39757, #53056, #4338, #58363, #3753, #9066, #17042 ) ),
 .UNSPECIFIED., .F., .F., .F.,
 ( 4, 3, 4 ),
 ( 4, 1, 1, 1, 1, 1, 1, 1, 1, 1, 1, 1, 1, 1, 1, 1, 1, 1, 1, 1, 1, 1, 1, 1, 1, 1, 1, 1, 1, 1, 1, 1, 4 ),
 ( -0.4045438850609999748, 1.404543885061000141, 5.000129188560400451 ),
 ( 0.4173531076193000011, 0.4359178370333999797, 0.4544825664474999583, 0.4730472958615999923, 0.4916120252757000264, 0.5101767546897999495, 0.5287414841038999835, 0.5473062135180000176, 0.5658709429320999407, 0.5844356723461999747, 0.6030004017601999777, 0.6215651311743000118, 0.6401298605884000459, 0.6586945900024999689, 0.6772593194166000030, 0.6958240488306999261, 0.7143887782447999601, 0.7329535076588999942, 0.7515182370730000283, 0.7700829664870000313, 0.7886476959010999543, 0.8072124253151999884, 0.8257771547292999115, 0.8443418841433999456, 0.8629066135575000906, 0.8814713429716000137, 0.9000360723857000478, 0.9186008017997999708, 0.9371655312139000049, 0.9557302606279000079, 0.9742949900419999310, 0.9928597194561000761, 1.011424448870000159 ),
 .UNSPECIFIED. ) ;
#53549 = CARTESIAN_POINT ( 'NONE',  ( -5.883052656872999719, -77.69532935296300025, 9.603314844095001135 ) ) ;
#53550 = CARTESIAN_POINT ( 'NONE',  ( 1.221746786348032687, -81.86707072010140962, 0.2639991584434943084 ) ) ;
#53551 = CARTESIAN_POINT ( 'NONE',  ( -0.1770758199222000062, -77.71431990869999140, 1.564455666405000001 ) ) ;
#53552 = DIRECTION ( 'NONE',  ( 0.000000000000000000, 1.000000000000000000, 0.000000000000000000 ) ) ;
#53553 = CARTESIAN_POINT ( 'NONE',  ( -0.6947239650216572304, -82.66294319288569170, 1.342880243175269550 ) ) ;
#53554 = CARTESIAN_POINT ( 'NONE',  ( -7.601397897754999633, -23.25000000000000000, -9.369164850722000892 ) ) ;
#53555 = CARTESIAN_POINT ( 'NONE',  ( 3.733146969192831843, -80.25324884369585732, -10.08725862556905994 ) ) ;
#53556 = CARTESIAN_POINT ( 'NONE',  ( 10.47020627418439531, -77.22916666666667140, -2.813789756862242974 ) ) ;
#53557 = CARTESIAN_POINT ( 'NONE',  ( -0.8908853506697682612, -77.71360592741159223, -0.9112983582399447613 ) ) ;
#53558 = B_SPLINE_CURVE_WITH_KNOTS ( 'NONE', 3,
 ( #46116, #18943, #31620, #32783, #41664, #32204, #36935, #1529, #19233, #18362, #37225, #55240, #54948, #19524, #50245, #37517, #54383, #22781, #49663, #10374, #13920, #27191, #41083, #23652, #31913, #49957, #14499, #45232, #9501, #383, #27487 ),
 .UNSPECIFIED., .F., .F.,
 ( 4, 1, 1, 1, 1, 1, 1, 1, 1, 1, 1, 1, 1, 1, 1, 1, 1, 1, 1, 1, 1, 1, 1, 1, 1, 1, 1, 1, 4 ),
 ( 0.000000000000000000, 0.01436125421998360463, 0.05169932518655311754, 0.08903739615315010847, 0.1263754671197221124, 0.1637135380862941303, 0.2010516090528911004, 0.2383896800194630905, 0.2757277509860102116, 0.3130658219525572772, 0.3504038929191043428, 0.3877419638859008200, 0.4250800348524479966, 0.4624181058189950622, 0.4997561767855421277, 0.5370942477520891378, 0.5744323187186362034, 0.6117703896851832690, 0.6491084606517303346, 0.6864465316185268673, 0.7237846025850739329, 0.7611226735516209985, 0.7984607445181682861, 0.8357988154847151296, 0.8731368864512621952, 0.9104749574178092608, 0.9478130283846057935, 0.9851510993511529701, 1.000000000000000000 ),
 .UNSPECIFIED. ) ;
#53559 = CARTESIAN_POINT ( 'NONE',  ( 0.6808670543330055391, -81.77126629245766765, -1.049018940644094400 ) ) ;
#53560 = CARTESIAN_POINT ( 'NONE',  ( -10.99999999999000089, -80.20000000002698926, -2.639066790267999940E-09 ) ) ;
#53561 = CARTESIAN_POINT ( 'NONE',  ( 2.026540639977999714, -80.03068473043869346, -10.96119216345999803 ) ) ;
#53562 = CARTESIAN_POINT ( 'NONE',  ( -0.1636246173744673738, -80.11458333333332860, -1.249999999999999778 ) ) ;
#53563 = ORIENTED_EDGE ( 'NONE', *, *, #22640, .F. ) ;
#53564 = ORIENTED_EDGE ( 'NONE', *, *, #38169, .F. ) ;
#53565 = FACE_OUTER_BOUND ( 'NONE', #42617, .T. ) ;
#53566 = B_SPLINE_CURVE_WITH_KNOTS ( 'NONE', 3,
 ( #23797, #28509, #46560, #14935, #32351, #10232 ),
 .UNSPECIFIED., .F., .F.,
 ( 4, 1, 1, 4 ),
 ( 0.000000000000000000, 0.3333333333333000081, 0.6666666666667000474, 1.000000000000000000 ),
 .UNSPECIFIED. ) ;
#53567 = ORIENTED_EDGE ( 'NONE', *, *, #13539, .F. ) ;
#53568 =( NAMED_UNIT ( * ) PLANE_ANGLE_UNIT ( ) SI_UNIT ( $, .RADIAN. ) );
#53569 = VERTEX_POINT ( 'NONE', #50696 ) ;
#53570 = CARTESIAN_POINT ( 'NONE',  ( 7.919595949288999570, -59.94999999040999938, -9.050966798898000931 ) ) ;
#53571 = CONICAL_SURFACE ( 'NONE', #26203, 9.649999999844000698, 0.7853981633972997312 ) ;
#53572 = CARTESIAN_POINT ( 'NONE',  ( -2.753094546102373918, -78.85416666326673862, -2.068686224605921442 ) ) ;
#53573 = CARTESIAN_POINT ( 'NONE',  ( -10.53927088184999938, -79.61726667242798783, 3.259678459687000096 ) ) ;
#53574 = B_SPLINE_CURVE_WITH_KNOTS ( 'NONE', 3,
 ( #17302, #48902, #48614, #9334 ),
 .UNSPECIFIED., .F., .F.,
 ( 4, 4 ),
 ( 0.000000000000000000, 1.000000000000000000 ),
 .UNSPECIFIED. ) ;
#53575 = CARTESIAN_POINT ( 'NONE',  ( 1.582498447119000229, -24.15086122477999808, -12.55493832972999968 ) ) ;
#53576 = CARTESIAN_POINT ( 'NONE',  ( -3.502956697134000041, -81.94082221650599251, -0.7829685155521000084 ) ) ;
#53577 = CARTESIAN_POINT ( 'NONE',  ( -7.649979009965352184, -79.34907697906386659, 5.632330841050999126 ) ) ;
#53578 = CARTESIAN_POINT ( 'NONE',  ( 5.341789944771998755, -77.68480993295618475, 9.661750877468000098 ) ) ;
#53579 = CARTESIAN_POINT ( 'NONE',  ( 9.846220907398999245, -78.71889409522999870, 7.220774715475999805 ) ) ;
#53580 = ORIENTED_EDGE ( 'NONE', *, *, #45970, .F. ) ;
#53581 = VERTEX_POINT ( 'NONE', #28219 ) ;
#53582 = CARTESIAN_POINT ( 'NONE',  ( -0.7999999997951999786, -18.85000000927000130, 11.99999999979999821 ) ) ;
#53583 = EDGE_CURVE ( 'NONE', #26401, #15817, #19390, .T. ) ;
#53584 = CARTESIAN_POINT ( 'NONE',  ( 0.6343572851480000496, -80.60121327037900585, 1.173101423079000005 ) ) ;
#53585 = CARTESIAN_POINT ( 'NONE',  ( 7.658860137760000519, -78.51216497498398894, 5.959242465009999989 ) ) ;
#53586 = FACE_BOUND ( 'NONE', #51631, .T. ) ;
#53587 = CARTESIAN_POINT ( 'NONE',  ( 1.992133063105471891, -85.88985440391550696, 2.860955247882542629 ) ) ;
#53588 = CARTESIAN_POINT ( 'NONE',  ( -9.306321164319999895, -77.06783216571999162, -9.238944841226000904 ) ) ;
#53589 = CARTESIAN_POINT ( 'NONE',  ( 5.420640129221999892, -77.08411282133998554, 11.42023903890000014 ) ) ;
#53590 = CARTESIAN_POINT ( 'NONE',  ( 4.772733260105000319, -76.68771245318799856, -9.782200613967999558 ) ) ;
#53591 = CARTESIAN_POINT ( 'NONE',  ( -9.119748668238788269, -78.61353292670899862, -1.546334858068346696 ) ) ;
#53592 = CARTESIAN_POINT ( 'NONE',  ( -2.796407410894000023, -81.81671231080099460, 2.808219311970999943 ) ) ;
#53593 = CARTESIAN_POINT ( 'NONE',  ( -10.07722254368999870, -57.05199022587000002, 7.718368845804999268 ) ) ;
#53594 = CARTESIAN_POINT ( 'NONE',  ( 1.100350654334843359, -2.948830382931522109, 3.057717532207668398 ) ) ;
#53595 = CARTESIAN_POINT ( 'NONE',  ( 3.438062426372999969, -82.37741931601499346, -0.2266141585933000024 ) ) ;
#53597 = ADVANCED_FACE ( 'NONE', ( #46567 ), #6706, .F. ) ;
#53596 = CIRCLE ( 'NONE', #28130, 11.75000000000000178 ) ;
#53598 = CARTESIAN_POINT ( 'NONE',  ( 0.000000000000000000, -26.93717104351999936, 0.000000000000000000 ) ) ;
#53599 = CARTESIAN_POINT ( 'NONE',  ( -9.578166812159000898, -80.35756696074160743, 5.930253639820000089 ) ) ;
#53600 = CARTESIAN_POINT ( 'NONE',  ( -2.707053224964000027, -2.685967474678999878, 2.675433656965999774 ) ) ;
#53601 = CARTESIAN_POINT ( 'NONE',  ( -1.149866947101319203, -79.78558583878638899, -0.5516533143361346259 ) ) ;
#53602 = ORIENTED_EDGE ( 'NONE', *, *, #9568, .T. ) ;
#53603 = CARTESIAN_POINT ( 'NONE',  ( -9.393203674808274783, -80.04166666666664298, -5.413904038987162437 ) ) ;
#53604 = EDGE_CURVE ( 'NONE', #9803, #39177, #21862, .T. ) ;
#53605 = B_SPLINE_CURVE_WITH_KNOTS ( 'NONE', 3,
 ( #12454, #7742, #20744, #33729, #47639, #51764 ),
 .UNSPECIFIED., .F., .F.,
 ( 4, 1, 1, 4 ),
 ( 0.000000000000000000, 0.3333333333333000081, 0.6666666666667000474, 1.000000000000000000 ),
 .UNSPECIFIED. ) ;
#53606 = LINE ( 'NONE', #57733, #49651 ) ;
#53607 = CARTESIAN_POINT ( 'NONE',  ( 0.8471236057751000414, -80.99834240209798963, 1.030027924806000028 ) ) ;
#53608 = CARTESIAN_POINT ( 'NONE',  ( -12.48375942317000131, -18.62730665102000316, -1.669542353227000175 ) ) ;
#53609 = CARTESIAN_POINT ( 'NONE',  ( -12.97861384075000046, -77.98845645414000671, -0.9459496016724999734 ) ) ;
#53610 = CARTESIAN_POINT ( 'NONE',  ( 6.454959760337000141, -79.25496001420199832, -6.996333296700000481 ) ) ;
#53611 = CARTESIAN_POINT ( 'NONE',  ( 12.49306752634999995, -18.71943307332999851, -1.667917367010000040 ) ) ;
#53612 = VERTEX_POINT ( 'NONE', #11988 ) ;
#53613 = EDGE_CURVE ( 'NONE', #456, #36279, #33106, .T. ) ;
#53614 = CARTESIAN_POINT ( 'NONE',  ( -0.7999999997951999786, -23.14999999072999870, -11.99999999979999821 ) ) ;
#53615 = CARTESIAN_POINT ( 'NONE',  ( 9.243145380909270514, -53.88347263105222851, -8.441178781369352180 ) ) ;
#53616 = CARTESIAN_POINT ( 'NONE',  ( 1.252904471488000215, -81.00955937516098970, -0.6434491202905999740 ) ) ;
#53617 = CARTESIAN_POINT ( 'NONE',  ( -1.667916687331000070, -23.29848884437999956, -12.49168451098999988 ) ) ;
#53618 = CARTESIAN_POINT ( 'NONE',  ( -9.446372167179999835, -78.44689511346298616, 1.198511206093999970 ) ) ;
#53620 = CARTESIAN_POINT ( 'NONE',  ( 3.981113306789000106, -0.9874747695768000266, -0.5296481109823999445 ) ) ;
#53619 = CARTESIAN_POINT ( 'NONE',  ( -0.7867051183105999712, -84.31375945333499544, 4.100085976432000123 ) ) ;
#53621 = CARTESIAN_POINT ( 'NONE',  ( -0.9995835529977281642, -82.44791666666662877, 0.7681833999686391579 ) ) ;
#53622 = CARTESIAN_POINT ( 'NONE',  ( 0.5499573741622000300, -79.44598562025299771, 1.306754138290999956 ) ) ;
#53623 = ORIENTED_EDGE ( 'NONE', *, *, #1322, .F. ) ;
#53624 = CARTESIAN_POINT ( 'NONE',  ( 5.363150622483991548, -77.26670457031288208, -9.329320527232589200 ) ) ;
#53625 = CARTESIAN_POINT ( 'NONE',  ( -1.230473908959625495, -82.23697916666547769, 0.3298056902639138754 ) ) ;
#53626 = CARTESIAN_POINT ( 'NONE',  ( 3.437187628289001040, -78.85171435493609238, 6.874375256578030502 ) ) ;
#53627 = EDGE_LOOP ( 'NONE', ( #880, #57354, #49319, #31170 ) ) ;
#53628 = ORIENTED_EDGE ( 'NONE', *, *, #43151, .F. ) ;
#53629 = CYLINDRICAL_SURFACE ( 'NONE', #49012, 10.14999999999999858 ) ;
#53630 = EDGE_CURVE ( 'NONE', #25746, #46308, #50758, .T. ) ;
#53631 = CYLINDRICAL_SURFACE ( 'NONE', #17046, 3.000000000000000000 ) ;
#53632 = DIRECTION ( 'NONE',  ( 0.000000000000000000, 1.000000000000000000, 0.000000000000000000 ) ) ;
#53633 = ORIENTED_EDGE ( 'NONE', *, *, #35296, .F. ) ;
#53634 = CARTESIAN_POINT ( 'NONE',  ( 7.897520336252998874, -77.37301250442499168, -9.100831677656000096 ) ) ;
#53635 = EDGE_LOOP ( 'NONE', ( #57696, #51048, #34990, #47500 ) ) ;
#53636 = VERTEX_POINT ( 'NONE', #34685 ) ;
#53637 = CARTESIAN_POINT ( 'NONE',  ( 0.000000000000000000, -0.8249999994726999741, 0.000000000000000000 ) ) ;
#53638 = AXIS2_PLACEMENT_3D ( 'NONE', #25056, #56936, #34475 ) ;
#53639 = CARTESIAN_POINT ( 'NONE',  ( 3.140974612311327796, -78.65416666666665435, 11.68767212001979594 ) ) ;
#53640 = DIRECTION ( 'NONE',  ( 0.000000000000000000, 1.000000000000000000, 3.788597347406000047E-11 ) ) ;
#53641 = ORIENTED_EDGE ( 'NONE', *, *, #26429, .T. ) ;
#53642 = B_SPLINE_CURVE_WITH_KNOTS ( 'NONE', 3,
 ( #16978, #57996, #34962, #53572, #52992, #17551, #30823, #30538, #44136, #17256, #48857, #8399, #35543, #49145, #26686, #14576, #50618, #55321, #1321, #55616, #23442, #14865, #42038, #9874, #23152, #32862, #10455, #14284, #5432, #18443, #4864, #36433, #9582, #41453, #5723, #464, #50907, #19315, #41157, #28442, #32280, #32570, #751, #22862, #23733, #1607, #41745, #1038, #50324, #46490, #18731, #46198, #19023, #37014, #36724, #6015, #24023, #40872, #54739, #27855, #54460, #28735, #10169, #51203, #37305, #15163, #28143, #19599, #33159, #13996, #37599 ),
 .UNSPECIFIED., .F., .F.,
 ( 4, 2, 2, 2, 1, 2, 2, 2, 2, 2, 2, 2, 2, 2, 2, 2, 2, 2, 1, 2, 2, 2, 2, 2, 2, 2, 2, 2, 2, 2, 2, 2, 1, 2, 2, 2, 4 ),
 ( 0.000000000000000000, 0.03124999999999998612, 0.06249999999999997224, 0.07812499999999995837, 0.09374999999999993061, 0.1093749999999999167, 0.1249999999999998890, 0.1562499999999999445, 0.1874999999999999445, 0.2187499999999999445, 0.2500000000000000000, 0.2812500000000000555, 0.3125000000000000555, 0.3437500000000001110, 0.3750000000000001665, 0.4062500000000001665, 0.4375000000000001110, 0.4687500000000001110, 0.5000000000000001110, 0.5312500000000001110, 0.5625000000000001110, 0.5937500000000001110, 0.6250000000000000000, 0.6562500000000000000, 0.6875000000000000000, 0.7187500000000000000, 0.7500000000000000000, 0.7812500000000000000, 0.8125000000000000000, 0.8437500000000000000, 0.8749999999999998890, 0.8906249999999998890, 0.9062499999999998890, 0.9218749999999998890, 0.9374999999999998890, 0.9687499999999998890, 1.000000000000000000 ),
 .UNSPECIFIED. ) ;
#53643 = ORIENTED_EDGE ( 'NONE', *, *, #1322, .T. ) ;
#53644 = CARTESIAN_POINT ( 'NONE',  ( 8.083247094228855900, -79.30839652358213243, -4.658693541334342214 ) ) ;
#53645 = EDGE_CURVE ( 'NONE', #2471, #7601, #30550, .T. ) ;
#53646 = CARTESIAN_POINT ( 'NONE',  ( -3.547719542586254882, -78.96264282632948550, 0.06688145936885296627 ) ) ;
#53647 = DIRECTION ( 'NONE',  ( 1.000000000000000000, 3.791713626542000006E-11, -3.791713626542000006E-11 ) ) ;
#53648 = CIRCLE ( 'NONE', #18767, 13.00000000000000000 ) ;
#53649 = CARTESIAN_POINT ( 'NONE',  ( -7.640030264154999529, -18.69283319134000010, -10.18491080493000212 ) ) ;
#53650 = CARTESIAN_POINT ( 'NONE',  ( 10.26578641119535007, -77.40555308739415352, -5.914033253227731990 ) ) ;
#53651 = CARTESIAN_POINT ( 'NONE',  ( -11.44417895085272008, -78.77916666666666856, 3.075537641221497420 ) ) ;
#53652 = CARTESIAN_POINT ( 'NONE',  ( -7.167604382869162905, -77.57604025214112653, 9.599037027053000770 ) ) ;
#53653 = B_SPLINE_CURVE_WITH_KNOTS ( 'NONE', 3,
 ( #20707, #38707, #40676, #29834, #38998, #31198, #57006, #18247 ),
 .UNSPECIFIED., .F., .F.,
 ( 4, 2, 2, 4 ),
 ( 0.000000000000000000, 0.5000000000000000000, 0.7500000000000000000, 1.000000000000000000 ),
 .UNSPECIFIED. ) ;
#53654 = CARTESIAN_POINT ( 'NONE',  ( -10.18496935386999880, -20.24935285395000051, -7.710095619721000659 ) ) ;
#53655 = CARTESIAN_POINT ( 'NONE',  ( 0.5999663639301143769, -23.18964892095651464, -10.98362601162690844 ) ) ;
#53656 = CARTESIAN_POINT ( 'NONE',  ( 1.460959015002474493, -80.12916666666669130, -0.3926218265389176953 ) ) ;
#53657 = CARTESIAN_POINT ( 'NONE',  ( 3.275410689762999983, -80.80305496681198463, -2.584907563698999766 ) ) ;
#53658 = CARTESIAN_POINT ( 'NONE',  ( -4.421234056401999624, -77.84448667140100042, -8.704183203973999028 ) ) ;
#53659 = CARTESIAN_POINT ( 'NONE',  ( -12.56594317823000040, -23.25000001387000026, 1.750000000000000000 ) ) ;
#53660 = EDGE_CURVE ( 'NONE', #5139, #34611, #16124, .T. ) ;
#53661 = DIRECTION ( 'NONE',  ( 0.000000000000000000, 1.000000000000000000, 0.000000000000000000 ) ) ;
#53662 = CARTESIAN_POINT ( 'NONE',  ( -1.930638663166000191, -23.22122063288999883, 12.72375916873000001 ) ) ;
#53663 = DIRECTION ( 'NONE',  ( 0.000000000000000000, 1.000000000000000000, 0.000000000000000000 ) ) ;
#53664 = CARTESIAN_POINT ( 'NONE',  ( -2.267046284475000117, -84.50932768054498467, 2.728563928855000320 ) ) ;
#53665 = CARTESIAN_POINT ( 'NONE',  ( 2.266888174815000045, -1.555016836958999837, -3.242122062176999719 ) ) ;
#53666 = CARTESIAN_POINT ( 'NONE',  ( 1.813979036993000227, -79.50980095943377535, 9.381055131006998948 ) ) ;
#53667 = CARTESIAN_POINT ( 'NONE',  ( 1.249290605349439254, -81.05175946334958326, -0.8518751653260581147 ) ) ;
#53668 = CARTESIAN_POINT ( 'NONE',  ( 12.54976804513999866, -61.84775476195000010, 0.05637402076003000112 ) ) ;
#53669 = CARTESIAN_POINT ( 'NONE',  ( -1.607511835558000035, -79.41551801124799681, -0.1512538100690999920 ) ) ;
#53670 = DIRECTION ( 'NONE',  ( 0.000000000000000000, -1.000000000000000000, 0.000000000000000000 ) ) ;
#53671 = CARTESIAN_POINT ( 'NONE',  ( 10.89235442234000040, -77.78191129495199618, 0.7293703643125000191 ) ) ;
#53672 = CARTESIAN_POINT ( 'NONE',  ( -4.187998665200000303, -78.27610463408198882, 11.54367560014000205 ) ) ;
#53673 = CARTESIAN_POINT ( 'NONE',  ( 0.7554284705563453217, -80.83333333333335702, 1.310679582531389276 ) ) ;
#53674 = VECTOR ( 'NONE', #11370, 1000.000000000000000 ) ;
#53675 = CARTESIAN_POINT ( 'NONE',  ( -10.75000000000000000, -79.00000000000000000, 0.000000000000000000 ) ) ;
#53677 = CARTESIAN_POINT ( 'NONE',  ( -1.040416939902000237, -78.41750647927929663, -1.102939138596999991 ) ) ;
#53676 = LINE ( 'NONE', #22378, #17565 ) ;
#53678 = CARTESIAN_POINT ( 'NONE',  ( 1.533821497824999991, -81.47706753059999585, 0.4022281561003999695 ) ) ;
#53679 = ORIENTED_EDGE ( 'NONE', *, *, #24009, .F. ) ;
#53680 = EDGE_CURVE ( 'NONE', #50158, #48229, #12339, .T. ) ;
#53681 = CARTESIAN_POINT ( 'NONE',  ( -1.560185313921000017, -83.23196544543098696, 3.417189128149000332 ) ) ;
#53682 = B_SPLINE_CURVE_WITH_KNOTS ( 'NONE', 3,
 ( #21739, #21164, #39745, #34439, #25879, #35597, #57755, #58049, #12594, #57181, #16746, #38881, #17312, #52469, #7593, #57468, #3451, #47771 ),
 .UNSPECIFIED., .F., .F.,
 ( 4, 2, 2, 2, 2, 2, 2, 2, 4 ),
 ( 0.000000000000000000, 0.1249999999999999722, 0.2499999999999999445, 0.3750000000000000000, 0.5000000000000001110, 0.6250000000000001110, 0.7500000000000000000, 0.8750000000000000000, 1.000000000000000000 ),
 .UNSPECIFIED. ) ;
#53683 = CARTESIAN_POINT ( 'NONE',  ( -11.23721025937000029, -79.15059218971499888, -3.995116809576999994 ) ) ;
#53684 = CARTESIAN_POINT ( 'NONE',  ( 6.760020157659999640, -80.81784931869341904, -8.895273066339001389 ) ) ;
#53685 = DIRECTION ( 'NONE',  ( 0.7071067811865475727, 0.000000000000000000, -0.7071067811865475727 ) ) ;
#53686 = FACE_OUTER_BOUND ( 'NONE', #14071, .T. ) ;
#53687 = CARTESIAN_POINT ( 'NONE',  ( -10.17713110909000029, -76.79936102791799613, 4.716330562529999604 ) ) ;
#53688 = CARTESIAN_POINT ( 'NONE',  ( -10.52693147742000157, -60.22153431716999705, 7.606024891127000309 ) ) ;
#53689 = CARTESIAN_POINT ( 'NONE',  ( -1.186507705731999929, -78.94446787273398058, -9.667052097962999468 ) ) ;
#53690 = AXIS2_PLACEMENT_3D ( 'NONE', #15205, #37051, #24063 ) ;
#53691 = CARTESIAN_POINT ( 'NONE',  ( 3.101351771310999705, -1.335516836959000031, -2.020112785969000235 ) ) ;
#53692 = CARTESIAN_POINT ( 'NONE',  ( 3.630949683904999947, -79.79999999999999716, -11.17491406647000041 ) ) ;
#53693 = CARTESIAN_POINT ( 'NONE',  ( 12.77297283014999962, -24.72822696531000020, -1.476112654659999857 ) ) ;
#53694 = CYLINDRICAL_SURFACE ( 'NONE', #30202, 1.750000000000000000 ) ;
#53695 = VERTEX_POINT ( 'NONE', #21696 ) ;
#53696 = CARTESIAN_POINT ( 'NONE',  ( -12.70451544420788537, -54.24534321881070298, 1.498804046722062022 ) ) ;
#53697 = CIRCLE ( 'NONE', #4695, 1.199999999999999956 ) ;
#53698 = CARTESIAN_POINT ( 'NONE',  ( 3.048335112825000248, -79.40808667140099431, -8.921746513659998712 ) ) ;
#53699 = CARTESIAN_POINT ( 'NONE',  ( -11.05000000000000071, -81.00000000000000000, 0.000000000000000000 ) ) ;
#53700 = ADVANCED_FACE ( 'NONE', ( #43865 ), #12267, .T. ) ;
#53701 = CARTESIAN_POINT ( 'NONE',  ( -10.38645071868999992, -56.02180874340999850, -7.655542440077000244 ) ) ;
#53702 = CARTESIAN_POINT ( 'NONE',  ( -1.387963714323000142, -79.84219163730999469, 0.9213108730841000904 ) ) ;
#53703 = EDGE_CURVE ( 'NONE', #57279, #33091, #48297, .T. ) ;
#53704 = LINE ( 'NONE', #58121, #2895 ) ;
#53705 = VERTEX_POINT ( 'NONE', #17267 ) ;
#53706 = FACE_OUTER_BOUND ( 'NONE', #21213, .T. ) ;
#53707 = CARTESIAN_POINT ( 'NONE',  ( 9.019414221601653736, -61.79291943934637032, -8.666941069242449558 ) ) ;
#53708 = CARTESIAN_POINT ( 'NONE',  ( -1.001315001699999874, -54.11477588220000001, -12.50000000000000000 ) ) ;
#53709 = ORIENTED_EDGE ( 'NONE', *, *, #3856, .T. ) ;
#53710 = VERTEX_POINT ( 'NONE', #3412 ) ;
#53711 = CARTESIAN_POINT ( 'NONE',  ( -8.541162059860999634, -53.79199348416999982, -9.205819316548000231 ) ) ;
#53712 = CARTESIAN_POINT ( 'NONE',  ( -9.699833017908000343, -79.26048791328599918, 1.146274062705999963 ) ) ;
#53713 = VERTEX_POINT ( 'NONE', #21412 ) ;
#53714 = ORIENTED_EDGE ( 'NONE', *, *, #18963, .T. ) ;
#53715 = CARTESIAN_POINT ( 'NONE',  ( -7.621235760192000441, -76.69489580791500316, -9.570988338631000403 ) ) ;
#53716 = DIRECTION ( 'NONE',  ( -1.000000000000000000, 0.000000000000000000, 0.000000000000000000 ) ) ;
#53717 = CARTESIAN_POINT ( 'NONE',  ( -1.397427047035999959, -78.31445671932998209, -0.8741189423671000824 ) ) ;
#53718 = VERTEX_POINT ( 'NONE', #39704 ) ;
#53719 = EDGE_CURVE ( 'NONE', #5420, #50457, #17058, .T. ) ;
#53720 = CARTESIAN_POINT ( 'NONE',  ( -10.42531124905999995, -23.26485148473999942, -7.624341765453999997 ) ) ;
#53721 = CARTESIAN_POINT ( 'NONE',  ( -9.346673348102125800, -77.82823394297724917, 2.610272996057591666 ) ) ;
#53722 = CARTESIAN_POINT ( 'NONE',  ( 1.231267358449230853, -80.33667723787161208, -0.2162300623809715050 ) ) ;
#53723 = CARTESIAN_POINT ( 'NONE',  ( 5.690325051763000630, -78.42027720837999993, 11.64023780191999968 ) ) ;
#53724 = CARTESIAN_POINT ( 'NONE',  ( 9.869466656387999137, -76.96059422246487713, -5.330266269891000164 ) ) ;
#53725 = CARTESIAN_POINT ( 'NONE',  ( 0.000000000000000000, -22.78578169018998878, 13.15643568216998638 ) ) ;
#53726 = CARTESIAN_POINT ( 'NONE',  ( -0.5084075448448571732, -86.36264282632899381, 4.088733110535507365 ) ) ;
#53727 = CARTESIAN_POINT ( 'NONE',  ( 11.14115696400000033, -79.14243177349999314, -1.301050381412999890 ) ) ;
#53728 = CARTESIAN_POINT ( 'NONE',  ( 7.033303429947452834, -79.90635737682303841, 6.007822180714758709 ) ) ;
#53729 = CARTESIAN_POINT ( 'NONE',  ( 9.175589925000075198, -16.77304466865986399, 8.792768277085899697 ) ) ;
#53730 = ORIENTED_EDGE ( 'NONE', *, *, #50998, .T. ) ;
#53731 = DIRECTION ( 'NONE',  ( 0.000000000000000000, 1.000000000000000000, 0.000000000000000000 ) ) ;
#53732 = CARTESIAN_POINT ( 'NONE',  ( 1.623944433304999935, -76.18752863036999656, -12.20239005717999881 ) ) ;
#53733 = CARTESIAN_POINT ( 'NONE',  ( 1.061497194196000082, -80.53940021773100000, -1.082666072229000020 ) ) ;
#53734 = VECTOR ( 'NONE', #24221, 1000.000000000000000 ) ;
#53735 = B_SPLINE_SURFACE_WITH_KNOTS ( 'NONE', 3, 3, ( 
 ( #37730, #11467, #46618, #5851, #6438, #23857, #15298, #41873, #20032, #33292, #51330, #19444, #55453, #10887, #28863, #24452, #42466, #2032, #34444 ),
 ( #56908, #44477, #43618, #58057, #17035, #25311, #53048, #22034, #12601, #40040, #3181, #20883, #30598, #48630, #26454, #21747, #48069, #52477, #8457 ),
 ( #12035, #30883, #52193, #48918, #39751, #35305, #7598, #57474, #47778, #34733, #4027, #12882, #11748, #8178, #25598, #2887, #21171, #17616, #52761 ),
 ( #12318, #29727, #7309, #53335, #43329, #44197, #38887, #57187, #30013, #57762, #17319, #39175, #16753, #16463, #30304, #48345, #25885, #7884, #43913 ) ),
 .UNSPECIFIED., .F., .F., .F.,
 ( 4, 4 ),
 ( 4, 1, 1, 1, 1, 1, 1, 1, 1, 1, 1, 1, 1, 1, 1, 1, 4 ),
 ( -0.1387574078320999993, 1.138757407831999968 ),
 ( -0.007432834721512999662, 0.01672387812341000202, 0.04088059096832000194, 0.06503730381324000775, 0.08919401665815999969, 0.1133507295031000034, 0.1375074423479999974, 0.1616641551929000054, 0.1858208680378000133, 0.2099775808827999968, 0.2341342937277000047, 0.2582910065726000126, 0.2824477194174999650, 0.3066044322623999729, 0.3307611451072999809, 0.3549178579523000199, 0.3790745707971999723 ),
 .UNSPECIFIED. ) ;
#53736 = CARTESIAN_POINT ( 'NONE',  ( 1.949429650119547164, -2.680776606104624094, 3.205215495301868334 ) ) ;
#53737 = AXIS2_PLACEMENT_3D ( 'NONE', #27854, #37303, #37889 ) ;
#53738 = CARTESIAN_POINT ( 'NONE',  ( 12.50000000000000000, -54.11640971901999819, -1.003652782195000093 ) ) ;
#53739 = CARTESIAN_POINT ( 'NONE',  ( 11.13784153760999907, -76.48629006631499294, 5.174080857020999957 ) ) ;
#53740 = DIRECTION ( 'NONE',  ( 0.000000000000000000, 1.000000000000000000, 0.000000000000000000 ) ) ;
#53741 = CARTESIAN_POINT ( 'NONE',  ( -5.068180973607000261, -78.64441589234299101, -9.940077528656999561 ) ) ;
#53742 = CARTESIAN_POINT ( 'NONE',  ( -1.206786224403999963, -77.32811332859900233, 9.552696603499001071 ) ) ;
#53743 = CARTESIAN_POINT ( 'NONE',  ( -7.710763962805349259, -76.98020946934893516, 9.280496569891228731 ) ) ;
#53744 = CYLINDRICAL_SURFACE ( 'NONE', #27927, 1.250000000000000000 ) ;
#53745 = DIRECTION ( 'NONE',  ( 1.776356839400000238E-14, -1.000000000000000000, 8.733754460384000171E-14 ) ) ;
#53746 = PLANE ( 'NONE',  #45110 ) ;
#53747 = ORIENTED_EDGE ( 'NONE', *, *, #55685, .T. ) ;
#53748 = CARTESIAN_POINT ( 'NONE',  ( -1.392304720662999928, -81.41111398138998823, -0.3162235598901000366 ) ) ;
#53749 = LINE ( 'NONE', #32162, #46671 ) ;
#53750 = CARTESIAN_POINT ( 'NONE',  ( 0.000000000000000000, -75.10000000284179578, -7.200000000000000178 ) ) ;
#53751 = CARTESIAN_POINT ( 'NONE',  ( 2.228685126279000173, -77.85842609231200129, 11.77068507108999995 ) ) ;
#53752 = CARTESIAN_POINT ( 'NONE',  ( 7.648026768019999366, -23.24999998419999869, 10.12290050217000115 ) ) ;
#53753 = CARTESIAN_POINT ( 'NONE',  ( 8.241770352740999783, -78.26225130393000029, -8.631843597936001089 ) ) ;
#53754 = CARTESIAN_POINT ( 'NONE',  ( 9.345760913908002010, -78.28209415034599772, 2.683384691900000174 ) ) ;
#53755 = CARTESIAN_POINT ( 'NONE',  ( 8.881263526186000234, -77.42242364445598923, 3.434171575746000293 ) ) ;
#53756 = CARTESIAN_POINT ( 'NONE',  ( -1.484804496640999893, -54.08130846584000295, -12.77261165604999960 ) ) ;
#53757 = CARTESIAN_POINT ( 'NONE',  ( 6.043427764450807871, -78.46666666666665435, -10.48543666025108934 ) ) ;
#53758 = CARTESIAN_POINT ( 'NONE',  ( -10.90697944550000109, -80.02995714425549068, -0.4616983494901999996 ) ) ;
#53759 = FACE_OUTER_BOUND ( 'NONE', #42034, .T. ) ;
#53760 = ORIENTED_EDGE ( 'NONE', *, *, #39447, .F. ) ;
#53761 = CARTESIAN_POINT ( 'NONE',  ( 12.56594317982999875, -55.55000000504000468, -1.750000000000000000 ) ) ;
#53762 = EDGE_CURVE ( 'NONE', #31986, #20195, #29320, .T. ) ;
#53763 = CARTESIAN_POINT ( 'NONE',  ( -1.500000000000000444, -79.38958333333333428, 0.1963495408493560745 ) ) ;
#53764 = CARTESIAN_POINT ( 'NONE',  ( 3.851650068367000301, -78.43735716284257364, -2.273141396972203854 ) ) ;
#53765 = EDGE_CURVE ( 'NONE', #54609, #57120, #51495, .T. ) ;
#53766 = B_SPLINE_CURVE_WITH_KNOTS ( 'NONE', 3,
 ( #32380, #1423, #45117, #22668, #271, #41260, #40679, #18830, #50424, #9974, #7502, #28542, #6409, #46590, #48252, #14968, #2006, #52952, #39374, #57087, #15267, #25789, #28831, #24424 ),
 .UNSPECIFIED., .F., .F.,
 ( 4, 2, 1, 2, 2, 2, 2, 2, 2, 2, 1, 2, 4 ),
 ( 0.000000000000000000, 0.06249999999999994449, 0.1249999999999999167, 0.1874999999999998890, 0.2499999999999998890, 0.3749999999999998890, 0.4999999999999998890, 0.6249999999999998890, 0.7499999999999998890, 0.8124999999999998890, 0.8750000000000000000, 0.9375000000000000000, 1.000000000000000000 ),
 .UNSPECIFIED. ) ;
#53767 = CARTESIAN_POINT ( 'NONE',  ( -9.813193589766999736, -78.96710715410898729, -4.915816122623000162 ) ) ;
#53768 = DIRECTION ( 'NONE',  ( 0.000000000000000000, -1.000000000000000000, 0.000000000000000000 ) ) ;
#53769 = CARTESIAN_POINT ( 'NONE',  ( 3.184503561814999717, -76.36297076860699917, 11.84932461738999976 ) ) ;
#53770 = CARTESIAN_POINT ( 'NONE',  ( -4.820688262674111435, -78.60634528047508240, 10.76661437165540747 ) ) ;
#53771 = CARTESIAN_POINT ( 'NONE',  ( 0.6694192215519998435, -76.87011569981827108, 10.80149589243966446 ) ) ;
#53772 = ORIENTED_EDGE ( 'NONE', *, *, #4707, .T. ) ;
#53773 = CARTESIAN_POINT ( 'NONE',  ( 10.53539001158999966, -79.99784788827008697, -3.979889026714000355 ) ) ;
#53774 = CARTESIAN_POINT ( 'NONE',  ( 9.278548426423457229, -77.24995839143393539, 0.001488306988104594027 ) ) ;
#53775 = CARTESIAN_POINT ( 'NONE',  ( 10.41874210216987073, -75.80000000000002558, -5.821609190279006363 ) ) ;
#53776 = CARTESIAN_POINT ( 'NONE',  ( 3.999999999999605649, -78.67389998729011324, -4.898587196588929651E-16 ) ) ;
#53777 = EDGE_CURVE ( 'NONE', #17469, #42116, #28078, .T. ) ;
#53778 = B_SPLINE_CURVE_WITH_KNOTS ( 'NONE', 3,
 ( #52, #921, #18903, #22446, #54908, #14460, #22741, #53752 ),
 .UNSPECIFIED., .F., .F.,
 ( 4, 2, 2, 4 ),
 ( 0.000000000000000000, 0.5000000000000007772, 0.7500000000000003331, 1.000000000000000000 ),
 .UNSPECIFIED. ) ;
#53779 = CARTESIAN_POINT ( 'NONE',  ( 11.12554012740000076, -78.49909427755598301, 0.8449594846185999319 ) ) ;
#53780 = DIRECTION ( 'NONE',  ( 0.000000000000000000, -1.000000000000000000, 0.000000000000000000 ) ) ;
#53781 = CARTESIAN_POINT ( 'NONE',  ( 7.601397897754999633, -55.55000000278000272, -10.07627163191000008 ) ) ;
#53782 = CARTESIAN_POINT ( 'NONE',  ( -8.353021825866999706, -78.89206171986300831, -9.001266886329000627 ) ) ;
#53783 = AXIS2_PLACEMENT_3D ( 'NONE', #33859, #24444, #56034 ) ;
#53784 = CARTESIAN_POINT ( 'NONE',  ( -13.89999999999999858, -80.79999999999999716, 0.000000000000000000 ) ) ;
#53785 = CARTESIAN_POINT ( 'NONE',  ( -1.750000000001000089, -60.04999998641999781, 12.56594318054000148 ) ) ;
#53786 = CARTESIAN_POINT ( 'NONE',  ( -12.70259419122151989, -61.53882758497012873, -1.314635108434076383 ) ) ;
#53787 = CARTESIAN_POINT ( 'NONE',  ( 12.00000000000000000, -77.04999999999999716, 0.000000000000000000 ) ) ;
#53788 = EDGE_LOOP ( 'NONE', ( #51148, #18213, #24393, #30085, #42654 ) ) ;
#53789 = VERTEX_POINT ( 'NONE', #23079 ) ;
#53790 = CARTESIAN_POINT ( 'NONE',  ( 10.24965171066401126, -78.82574021499290495, -3.245740100043394527 ) ) ;
#53791 = CARTESIAN_POINT ( 'NONE',  ( -7.634644595683999668, -77.68053998579799213, -5.724755653662000121 ) ) ;
#53792 = EDGE_LOOP ( 'NONE', ( #34438, #48921, #2045, #9481 ) ) ;
#53793 = CARTESIAN_POINT ( 'NONE',  ( -4.802691730569000228, -78.45956385665999733, 11.09149278351999968 ) ) ;
#53794 = ORIENTED_EDGE ( 'NONE', *, *, #57533, .F. ) ;
#53795 = CARTESIAN_POINT ( 'NONE',  ( 8.478749451758998745, -24.87812788920000173, 9.108222796172999125 ) ) ;
#53796 = CARTESIAN_POINT ( 'NONE',  ( -3.455491054688999863, -78.24078379918199744, -10.47670062235000010 ) ) ;
#53797 = CARTESIAN_POINT ( 'NONE',  ( -1.210822168571057400, -79.61458333333335702, -9.250000000000001776 ) ) ;
#53798 = CARTESIAN_POINT ( 'NONE',  ( -0.7677219301324074152, -82.52774397455820576, 0.9995942476885919525 ) ) ;
#53799 = CARTESIAN_POINT ( 'NONE',  ( -3.859218140372036032, -78.19092744093191527, -8.411749044435275380 ) ) ;
#53800 = CARTESIAN_POINT ( 'NONE',  ( -0.4146318973827000098, -79.32037491569599297, -11.20920117498000046 ) ) ;
#53801 = CARTESIAN_POINT ( 'NONE',  ( 1.224974234943492446, -79.36964605286109986, 0.3088754873210631802 ) ) ;
#53802 = ORIENTED_EDGE ( 'NONE', *, *, #40509, .F. ) ;
#53803 = VERTEX_POINT ( 'NONE', #54674 ) ;
#53804 = CARTESIAN_POINT ( 'NONE',  ( 2.848152166355370163, -77.45027005925211938, 8.800485350458805200 ) ) ;
#53805 = CARTESIAN_POINT ( 'NONE',  ( 10.71768947918000059, -78.16788369857198404, -1.656903943290000125 ) ) ;
#53806 = ADVANCED_FACE ( 'NONE', ( #41093 ), #969, .T. ) ;
#53807 = CARTESIAN_POINT ( 'NONE',  ( -1.182190922889000184, -79.00573587241498785, -9.631881180458998770 ) ) ;
#53808 = CARTESIAN_POINT ( 'NONE',  ( -2.113979906412999821, -75.85601843290000090, -12.47295230648999897 ) ) ;
#53809 = CARTESIAN_POINT ( 'NONE',  ( -9.030529600513531818, -79.42482680610650903, -2.948931173546283979 ) ) ;
#53810 = CARTESIAN_POINT ( 'NONE',  ( 1.341343219651000229, -78.91326760749998925, -0.9216622887798999741 ) ) ;
#53811 = DIRECTION ( 'NONE',  ( 0.7071067811865475727, 0.000000000000000000, -0.7071067811865475727 ) ) ;
#53812 = CARTESIAN_POINT ( 'NONE',  ( 12.43359548536000148, -17.29290601378000147, -0.8500179128024000219 ) ) ;
#53813 = CARTESIAN_POINT ( 'NONE',  ( -10.18948929998999908, -23.21532694344000092, -7.645397820736000050 ) ) ;
#53814 = CARTESIAN_POINT ( 'NONE',  ( 2.486903332704932801, -79.15440197946847434, 9.251043845573130753 ) ) ;
#53815 = CARTESIAN_POINT ( 'NONE',  ( 3.125201106736000156, -85.38443645448099062, 1.765463379168000113 ) ) ;
#53816 = VERTEX_POINT ( 'NONE', #41386 ) ;
#53817 = CARTESIAN_POINT ( 'NONE',  ( -5.635457317866999105, -79.02831925412799308, -10.95206051398000113 ) ) ;
#53818 = AXIS2_PLACEMENT_3D ( 'NONE', #8439, #504, #31740 ) ;
#53819 = CARTESIAN_POINT ( 'NONE',  ( -8.439750306821999004, -76.58265968624300513, 7.626226795102000189 ) ) ;
#53820 = CARTESIAN_POINT ( 'NONE',  ( -5.334928932963716619, -78.01642494921711091, 9.332864396458077749 ) ) ;
#53821 = CARTESIAN_POINT ( 'NONE',  ( 7.483561698776000526, -78.45520156106799448, 9.354804580292000793 ) ) ;
#53822 = CARTESIAN_POINT ( 'NONE',  ( -10.36289663187999999, -18.79893657682999830, 7.633501051924000080 ) ) ;
#53823 = AXIS2_PLACEMENT_3D ( 'NONE', #14076, #53350, #35620 ) ;
#53824 = LINE ( 'NONE', #49695, #48764 ) ;
#53825 = CARTESIAN_POINT ( 'NONE',  ( 3.184161977317999881, -86.31452042059399332, -1.417680250971000033 ) ) ;
#53826 = CARTESIAN_POINT ( 'NONE',  ( 10.01332852686999964, -55.51943464808999806, -7.654537165450999936 ) ) ;
#53827 = CARTESIAN_POINT ( 'NONE',  ( 1.568318300085000120E-14, -0.05000000003700048185, 0.000000000000000000 ) ) ;
#53828 = CARTESIAN_POINT ( 'NONE',  ( 9.807952262865001103, -77.10173030608999056, -5.297043796141999827 ) ) ;
#53829 = FACE_OUTER_BOUND ( 'NONE', #6313, .T. ) ;
#53830 = CARTESIAN_POINT ( 'NONE',  ( -11.00000000000000711, -80.18958333335920940, 1.439896632895276696 ) ) ;
#53831 = ORIENTED_EDGE ( 'NONE', *, *, #36575, .T. ) ;
#53832 = CARTESIAN_POINT ( 'NONE',  ( 3.168764867850674793, -1.372313138392203369, 0.8503644209021197220 ) ) ;
#53833 = CARTESIAN_POINT ( 'NONE',  ( 1.761265949711000145, -55.09141781180999686, 12.57448205041000122 ) ) ;
#53834 = B_SPLINE_CURVE_WITH_KNOTS ( 'NONE', 3,
 ( #54624, #26557, #44587, #31868, #57871, #27733, #35716, #13281, #32158, #4143, #50197, #45777, #18318, #21848, #17424, #35411, #53442, #49315, #12984, #4438, #22438, #36013, #54038, #13577, #31568, #19771, #32446, #41912, #51663, #6181, #15625, #10626, #14738, #37182, #54900, #24193, #10044, #2067, #33619, #32737, #56079, #38056, #46654, #6473, #1776, #11211, #914, #1197, #19476, #29189, #28025, #5314, #42210, #51078, #28608, #37767, #55788, #33032, #15338, #14451, #24484, #46070, #5592, #37469, #10330 ),
 .UNSPECIFIED., .F., .F.,
 ( 4, 1, 1, 1, 1, 1, 1, 1, 1, 1, 1, 1, 1, 1, 1, 1, 1, 1, 1, 1, 1, 1, 1, 1, 1, 1, 1, 1, 1, 1, 1, 1, 1, 1, 1, 1, 1, 1, 1, 1, 1, 1, 1, 1, 1, 1, 1, 1, 1, 1, 1, 1, 1, 1, 1, 1, 1, 1, 1, 1, 1, 1, 4 ),
 ( 0.000000000000000000, 0.01249977652363855676, 0.02874978397245062101, 0.04499979142126268872, 0.06124979887007475643, 0.07749980631888682414, 0.09374981376769889185, 0.1099998212165109596, 0.1262498286653230273, 0.1424998361141350811, 0.1587498435629471627, 0.1749998510117592165, 0.1912498584605712981, 0.2074998659093833520, 0.2237498733581954335, 0.2399998808070074596, 0.2562498882558195135, 0.2724998957046316228, 0.2887499031534436766, 0.3049999106022557305, 0.3212499180510677843, 0.3374999254998798937, 0.3537499329486919475, 0.3699999403975040013, 0.3862499478463160552, 0.4024999552951281645, 0.4187499627439402183, 0.4349999701927522722, 0.4512499776415643260, 0.4674999850903764353, 0.4837499925391884892, 0.4999999999880005430, 0.5162500074368124858, 0.5325000148856245952, 0.5487500223344365935, 0.5650000297832487028, 0.5812500372320608122, 0.5975000446808729215, 0.6137500521296849199, 0.6300000595784970292, 0.6462500670273090275, 0.6625000744761211369, 0.6787500819249331352, 0.6950000893737452445, 0.7112500968225573539, 0.7275001042713694632, 0.7437501117201814615, 0.7600001191689935709, 0.7762501266178055692, 0.7925001340666176786, 0.8087501415154296769, 0.8250001489642417862, 0.8412501564130538956, 0.8575001638618660049, 0.8737501713106780032, 0.8900001787594901126, 0.9062501862083021109, 0.9225001936571142203, 0.9387502011059262186, 0.9550002085547383279, 0.9712502160035503262, 0.9875002234523625466, 1.000000000000000000 ),
 .UNSPECIFIED. ) ;
#53835 = DIRECTION ( 'NONE',  ( -0.7071067811865475727, 0.000000000000000000, -0.7071067811865475727 ) ) ;
#53836 = CARTESIAN_POINT ( 'NONE',  ( -3.736288849819999758, -2.332852077435000115, -1.330886568031999895 ) ) ;
#53837 = EDGE_CURVE ( 'NONE', #15471, #35000, #26477, .T. ) ;
#53838 = CARTESIAN_POINT ( 'NONE',  ( -3.467202887606000150, -79.92579286116600201, 8.763830676697999422 ) ) ;
#53839 = CARTESIAN_POINT ( 'NONE',  ( -5.838193839761688153, -77.37291666666669698, -7.596835002782716728 ) ) ;
#53840 = DIRECTION ( 'NONE',  ( 0.000000000000000000, -1.000000000000000000, 0.000000000000000000 ) ) ;
#53841 = CARTESIAN_POINT ( 'NONE',  ( -1.698401934075999931, -61.02014045872000025, 12.66748707616000047 ) ) ;
#53842 = CARTESIAN_POINT ( 'NONE',  ( 0.000000000000000000, -60.04999999966999980, 12.50000000000000000 ) ) ;
#53843 = CARTESIAN_POINT ( 'NONE',  ( -4.134522458939999368, -83.15519503318799366, 0.5619488135074000024 ) ) ;
#53844 = DIRECTION ( 'NONE',  ( 0.000000000000000000, 1.000000000000000000, 0.000000000000000000 ) ) ;
#53845 = B_SPLINE_CURVE_WITH_KNOTS ( 'NONE', 3,
 ( #41532, #37092, #22942, #54245, #23810, #27648, #55109, #5229, #14654, #32649 ),
 .UNSPECIFIED., .F., .F.,
 ( 4, 2, 2, 2, 4 ),
 ( 0.000000000000000000, 0.2500000000000000000, 0.5000000000000000000, 0.7500000000000000000, 1.000000000000000000 ),
 .UNSPECIFIED. ) ;
#53846 = CARTESIAN_POINT ( 'NONE',  ( 6.162632954033368193, -76.78536682155184678, 10.39017533730111964 ) ) ;
#53847 = CARTESIAN_POINT ( 'NONE',  ( 12.43608888892000053, -79.01247494496000456, 1.073723900664999897 ) ) ;
#53848 = EDGE_CURVE ( 'NONE', #43630, #32566, #40800, .T. ) ;
#53849 = AXIS2_PLACEMENT_3D ( 'NONE', #15810, #42098, #32626 ) ;
#53850 = CARTESIAN_POINT ( 'NONE',  ( 10.94776161156000072, -76.97393005650599207, 2.097883759165000139 ) ) ;
#53851 = CARTESIAN_POINT ( 'NONE',  ( -0.6332123272625999055, -81.17642093709999074, 1.540853336418999797 ) ) ;
#53852 = CARTESIAN_POINT ( 'NONE',  ( 0.1056055121785000050, -79.32579514703000712, 1.430709028799999949 ) ) ;
#53853 = CARTESIAN_POINT ( 'NONE',  ( -0.2678032732400780769, -62.01432775263499764, 12.70526550773306340 ) ) ;
#53854 = CARTESIAN_POINT ( 'NONE',  ( 0.4262039658379053186, -82.60221317835673460, 1.450363779020775290 ) ) ;
#53855 = CARTESIAN_POINT ( 'NONE',  ( -12.61112459821999998, -60.01565178538000112, 1.798929298655999931 ) ) ;
#53856 = CARTESIAN_POINT ( 'NONE',  ( -2.075652906230024630, -80.20975560462747467, -10.54757134404949781 ) ) ;
#53857 = CARTESIAN_POINT ( 'NONE',  ( -9.500000000000000000, -77.79999999999999716, 0.000000000000000000 ) ) ;
#53858 = CARTESIAN_POINT ( 'NONE',  ( -1.249847342545643336, -77.66590148185295561, -0.2497756822732188076 ) ) ;
#53859 = EDGE_LOOP ( 'NONE', ( #15535, #29317, #51778, #55529, #34886 ) ) ;
#53860 = CARTESIAN_POINT ( 'NONE',  ( 8.872949061366725232, -53.78989818412265578, 8.813905827834215501 ) ) ;
#53861 = CARTESIAN_POINT ( 'NONE',  ( 5.539808784079903958, -79.43333333333332291, 9.611650271896833075 ) ) ;
#53862 = CARTESIAN_POINT ( 'NONE',  ( -1.769784341028000085, -80.00344838743689024, -11.00556513567000039 ) ) ;
#53863 = DIRECTION ( 'NONE',  ( 0.7071067811865475727, 0.000000000000000000, -0.7071067811865475727 ) ) ;
#53864 = EDGE_LOOP ( 'NONE', ( #44193, #4627, #34492, #9645 ) ) ;
#53865 = ORIENTED_EDGE ( 'NONE', *, *, #15642, .F. ) ;
#53866 = CARTESIAN_POINT ( 'NONE',  ( -1.599507418690000016, -82.00287484044099529, -0.2211225942084000251 ) ) ;
#53867 = AXIS2_PLACEMENT_3D ( 'NONE', #5652, #1254, #19241 ) ;
#53868 = ORIENTED_EDGE ( 'NONE', *, *, #55651, .T. ) ;
#53869 = DIRECTION ( 'NONE',  ( 0.000000000000000000, -1.000000000000000000, 0.000000000000000000 ) ) ;
#53870 = ORIENTED_EDGE ( 'NONE', *, *, #54792, .F. ) ;
#53871 = VECTOR ( 'NONE', #18282, 1000.000000000000114 ) ;
#53872 = CARTESIAN_POINT ( 'NONE',  ( -1.691611010928000036, -17.76917308770000048, 12.66722148969999928 ) ) ;
#53873 = FACE_BOUND ( 'NONE', #45978, .T. ) ;
#53874 = CARTESIAN_POINT ( 'NONE',  ( 0.9218200799623694763, -78.32291666666667140, 1.199500263597272465 ) ) ;
#53875 = CARTESIAN_POINT ( 'NONE',  ( 10.71899861749000138, -79.37213958541198622, -2.608601736514999825 ) ) ;
#53876 = CARTESIAN_POINT ( 'NONE',  ( 1.761265949708000100, -23.70858218785999938, -12.57448205042999945 ) ) ;
#53877 = CARTESIAN_POINT ( 'NONE',  ( -1.265088337640000171, -82.29771400872598974, -3.537080082236999878 ) ) ;
#53878 = CARTESIAN_POINT ( 'NONE',  ( -1.291158054771311958, -79.28560666305160964, 9.411828421188701554 ) ) ;
#53879 = ORIENTED_EDGE ( 'NONE', *, *, #23221, .F. ) ;
#53880 = CARTESIAN_POINT ( 'NONE',  ( -0.5413127449341000874, -77.97109731094417384, -11.02683867434999776 ) ) ;
#53881 = CARTESIAN_POINT ( 'NONE',  ( 12.10989215130000041, -79.17874558444999877, 1.561551467148000194 ) ) ;
#53882 = ORIENTED_EDGE ( 'NONE', *, *, #1068, .F. ) ;
#53883 = EDGE_LOOP ( 'NONE', ( #50320, #35974, #17684, #27965 ) ) ;
#53884 = DIRECTION ( 'NONE',  ( 0.000000000000000000, 0.000000000000000000, 1.000000000000000000 ) ) ;
#53885 = CARTESIAN_POINT ( 'NONE',  ( 1.250000000000000000, -60.04999999966999980, 12.00000000000000000 ) ) ;
#53886 = EDGE_CURVE ( 'NONE', #43107, #52954, #8473, .T. ) ;
#53887 = CARTESIAN_POINT ( 'NONE',  ( 0.6343572851480000496, -80.55743925279999473, 1.173101423079000005 ) ) ;
#53888 = CARTESIAN_POINT ( 'NONE',  ( -9.446433787353997857, -78.22792668369498870, -2.221620594898999990 ) ) ;
#53889 = CARTESIAN_POINT ( 'NONE',  ( -1.536715235503818278, -86.40321104920798234, -3.365784645892647919 ) ) ;
#53890 = CARTESIAN_POINT ( 'NONE',  ( 3.645504569144430551, -85.80231680694522822, 0.8496922539149652787 ) ) ;
#53891 = CARTESIAN_POINT ( 'NONE',  ( -12.92190527446000026, -77.92433021234000989, -0.9418163832602000074 ) ) ;
#53892 = EDGE_CURVE ( 'NONE', #17898, #43107, #18667, .T. ) ;
#53893 = CARTESIAN_POINT ( 'NONE',  ( 0.4719577028681999908, -80.73341720544999589, -1.266186157272999768 ) ) ;
#53894 = CARTESIAN_POINT ( 'NONE',  ( -9.673449916064999599, -76.98869575705799662, 4.989449158498000081 ) ) ;
#53895 = CYLINDRICAL_SURFACE ( 'NONE', #23725, 1.000000000000000000 ) ;
#53896 = STYLED_ITEM ( 'NONE', ( #34309 ), #44024 ) ;
#53897 = CARTESIAN_POINT ( 'NONE',  ( 3.645312667415999908, -82.65846528216999900, -1.554756671834999882 ) ) ;
#53898 = CARTESIAN_POINT ( 'NONE',  ( -10.24998526317999925, -57.04916621739000249, 7.705142895613999343 ) ) ;
#53899 = CARTESIAN_POINT ( 'NONE',  ( 5.629678282322556626, -76.86401920440739843, -10.39394257255064780 ) ) ;
#53900 = CARTESIAN_POINT ( 'NONE',  ( -2.026060677209999827, -80.37325264934800373, -2.908615120711000035 ) ) ;
#53901 = LINE ( 'NONE', #9024, #12722 ) ;
#53902 = DIRECTION ( 'NONE',  ( 1.000000000000000000, 0.000000000000000000, -0.000000000000000000 ) ) ;
#53903 = CARTESIAN_POINT ( 'NONE',  ( 9.755626371838998168, -81.11000911083239373, -5.633583086437000453 ) ) ;
#53904 = CARTESIAN_POINT ( 'NONE',  ( 1.068619641472000170, -1.930313715633000138, -3.652926003266999899 ) ) ;
#53905 = CARTESIAN_POINT ( 'NONE',  ( -0.9250595310797312676, -80.31033944340789787, -0.8763432897296752344 ) ) ;
#53906 = ORIENTED_EDGE ( 'NONE', *, *, #56872, .T. ) ;
#53907 = CARTESIAN_POINT ( 'NONE',  ( -0.5812841321855987120, -23.30416868476589798, 10.98463311464191605 ) ) ;
#53908 = CARTESIAN_POINT ( 'NONE',  ( 0.000000000000000000, 0.000000000000000000, 0.000000000000000000 ) ) ;
#53909 = CARTESIAN_POINT ( 'NONE',  ( -1.208084210770999922, -81.64330650605199935, 0.5648970606752000689 ) ) ;
#53910 = EDGE_CURVE ( 'NONE', #24152, #31999, #24710, .T. ) ;
#53911 = AXIS2_PLACEMENT_3D ( 'NONE', #33963, #11837, #29818 ) ;
#53912 = CARTESIAN_POINT ( 'NONE',  ( -12.54976795933000133, -16.95224500006000312, 0.05636009750358000198 ) ) ;
#53913 = CARTESIAN_POINT ( 'NONE',  ( 6.891227191158999510, -76.65634507106000228, -9.824000600561999974 ) ) ;
#53914 = AXIS2_PLACEMENT_3D ( 'NONE', #15811, #24082, #19961 ) ;
#53915 = CARTESIAN_POINT ( 'NONE',  ( -9.164385193292622134, -62.01567483102901690, -8.803702036947488097 ) ) ;
#53916 = CARTESIAN_POINT ( 'NONE',  ( 12.64502302235000109, -22.77129148951999937, -1.799490220168999954 ) ) ;
#53917 = ORIENTED_EDGE ( 'NONE', *, *, #25191, .T. ) ;
#53918 = CARTESIAN_POINT ( 'NONE',  ( 10.07627163191000008, -18.75000000310999937, 7.601397897754999633 ) ) ;
#53919 = CARTESIAN_POINT ( 'NONE',  ( -10.35570946080999910, -77.21152914414997781, -4.457041641201000104 ) ) ;
#53920 = ADVANCED_FACE ( 'NONE', ( #32500 ), #20858, .F. ) ;
#53921 = CARTESIAN_POINT ( 'NONE',  ( -0.2266931603661999917, -82.18517820610701108, 1.390102994847999929 ) ) ;
#53922 = CARTESIAN_POINT ( 'NONE',  ( -2.062503053667999797, -20.24263462181000151, -12.92177931909999877 ) ) ;
#53923 = CARTESIAN_POINT ( 'NONE',  ( 9.372653703366999878, -79.27821424072898537, 0.8742135494153999709 ) ) ;
#53924 = ADVANCED_FACE ( 'NONE', ( #50545 ), #14796, .T. ) ;
#53926 = CARTESIAN_POINT ( 'NONE',  ( 2.863963203921999767, -1.059821851618000021, 2.815564610575000071 ) ) ;
#53925 = CARTESIAN_POINT ( 'NONE',  ( -1.753665918641999832, -84.91501152966898758, -3.788702389557000227 ) ) ;
#53927 = CARTESIAN_POINT ( 'NONE',  ( -1.667961430005999945, -57.05111654290000445, -12.58335110165999993 ) ) ;
#53928 = CARTESIAN_POINT ( 'NONE',  ( -1.087531843820000121, -79.98596541309798624, 1.056511543117000018 ) ) ;
#53929 = ORIENTED_EDGE ( 'NONE', *, *, #30091, .T. ) ;
#53930 = CARTESIAN_POINT ( 'NONE',  ( -5.191308461407881047, -77.18497258547503748, -9.414107671153617574 ) ) ;
#53931 = CARTESIAN_POINT ( 'NONE',  ( 8.012523733906443013, -79.11708638852500997, 8.990154430766320814 ) ) ;
#53932 = ORIENTED_EDGE ( 'NONE', *, *, #25893, .F. ) ;
#53933 = VERTEX_POINT ( 'NONE', #30104 ) ;
#53934 = CARTESIAN_POINT ( 'NONE',  ( 7.520016693046000178, -79.88042186404709355, -9.389162645085001202 ) ) ;
#53935 = DIRECTION ( 'NONE',  ( 0.000000000000000000, -1.000000000000000000, 0.000000000000000000 ) ) ;
#53936 = DIRECTION ( 'NONE',  ( -0.7071067811865475727, 0.000000000000000000, 0.7071067811865475727 ) ) ;
#53937 = ORIENTED_EDGE ( 'NONE', *, *, #45605, .F. ) ;
#53938 =( GEOMETRIC_REPRESENTATION_CONTEXT ( 3 ) GLOBAL_UNCERTAINTY_ASSIGNED_CONTEXT ( ( #24836 ) ) GLOBAL_UNIT_ASSIGNED_CONTEXT ( ( #24962, #56267, #23291 ) ) REPRESENTATION_CONTEXT ( 'NONE', 'WORKASPACE' ) );
#53939 = CARTESIAN_POINT ( 'NONE',  ( 9.505630310840999186, -77.88846949747699000, -7.405319984134000499 ) ) ;
#53940 = ORIENTED_EDGE ( 'NONE', *, *, #11253, .T. ) ;
#53941 = ORIENTED_EDGE ( 'NONE', *, *, #17541, .F. ) ;
#53942 = CARTESIAN_POINT ( 'NONE',  ( -1.218029035538723992, -2.695274461392550780, -3.012586580984925710 ) ) ;
#53943 = EDGE_CURVE ( 'NONE', #10829, #24242, #9576, .T. ) ;
#53944 = CARTESIAN_POINT ( 'NONE',  ( -1.500000000000000000, -83.28333333333331723, 0.000000000000000000 ) ) ;
#53945 = CARTESIAN_POINT ( 'NONE',  ( -1.500000000000000000, -80.00000000000000000, 0.000000000000000000 ) ) ;
#53946 = ORIENTED_EDGE ( 'NONE', *, *, #43394, .F. ) ;
#53947 = CARTESIAN_POINT ( 'NONE',  ( -0.3925236660400593380, -81.79597738037770682, 1.460591605855642072 ) ) ;
#53948 = ORIENTED_EDGE ( 'NONE', *, *, #45223, .T. ) ;
#53949 = CARTESIAN_POINT ( 'NONE',  ( 1.169289758545334790, -80.43275932425954977, 0.5071859018191248181 ) ) ;
#53950 = CARTESIAN_POINT ( 'NONE',  ( -4.043785186575886925, -78.72610001270986402, -2.284879765406275354 ) ) ;
#53951 = DIRECTION ( 'NONE',  ( 0.000000000000000000, 0.000000000000000000, -1.000000000000000000 ) ) ;
#53952 = CARTESIAN_POINT ( 'NONE',  ( 0.1610657711504699108, -18.25053022707183459, 10.99997582743960400 ) ) ;
#53953 = EDGE_CURVE ( 'NONE', #54307, #33230, #43013, .T. ) ;
#53954 = AXIS2_PLACEMENT_3D ( 'NONE', #47186, #42451, #20017 ) ;
#53955 = CARTESIAN_POINT ( 'NONE',  ( 11.06835501100703034, -76.52189007101335960, -4.078077733570841801 ) ) ;
#53956 = CARTESIAN_POINT ( 'NONE',  ( 7.655555357447999754, -59.57795407677000554, -10.38646360829999971 ) ) ;
#53957 = CARTESIAN_POINT ( 'NONE',  ( 6.720086853208802502, -78.78986668635583612, -6.356536187194287812 ) ) ;
#53958 = CARTESIAN_POINT ( 'NONE',  ( -8.878335097414000288, -25.06963071744000260, 8.870344075630997693 ) ) ;
#53959 = CARTESIAN_POINT ( 'NONE',  ( 9.611650271896820641, -78.39166666666665151, 5.539808784079911952 ) ) ;
#53960 = CARTESIAN_POINT ( 'NONE',  ( -0.4361488465060999742, -80.56255496681198736, -4.149679081948000281 ) ) ;
#53961 = CARTESIAN_POINT ( 'NONE',  ( -9.702495711998999184, -77.83546001420199900, -1.825589709539000127 ) ) ;
#53962 = CARTESIAN_POINT ( 'NONE',  ( -12.57433760367000097, -18.28878254117000068, 1.760777649351999985 ) ) ;
#53963 = DIRECTION ( 'NONE',  ( 0.000000000000000000, -1.000000000000000000, 0.000000000000000000 ) ) ;
#53964 = CARTESIAN_POINT ( 'NONE',  ( 1.801750019963999971, -23.39007426722000105, 12.59656967653999970 ) ) ;
#53965 = CARTESIAN_POINT ( 'NONE',  ( 0.000000000000000000, -82.09999999999999432, 0.000000000000000000 ) ) ;
#53966 = CARTESIAN_POINT ( 'NONE',  ( 2.588476952076999904, -84.14857643474398685, 2.425767309192000454 ) ) ;
#53967 = CARTESIAN_POINT ( 'NONE',  ( -0.4739505115940000346, -1.178547659067000097, 4.095219728108999924 ) ) ;
#53968 = CARTESIAN_POINT ( 'NONE',  ( -9.554796630153999715, -79.65020095943376077, -0.02401403847836000235 ) ) ;
#53969 = CARTESIAN_POINT ( 'NONE',  ( -0.8705260234225306037, -80.27237256087059336, 1.278861286191462332 ) ) ;
#53970 = CARTESIAN_POINT ( 'NONE',  ( 12.54977961489000116, -61.84832888596000089, 0.03757501521674000422 ) ) ;
#53971 = CARTESIAN_POINT ( 'NONE',  ( -1.163821121499999833, -78.96900440081799388, -1.119256147183999905 ) ) ;
#53972 = CARTESIAN_POINT ( 'NONE',  ( 12.99510751537000353, -15.69705297113999443, -6.911973076623003642 ) ) ;
#53973 = CARTESIAN_POINT ( 'NONE',  ( 10.01578477942999967, -77.80914763795398414, 4.342743515613999961 ) ) ;
#53974 = CARTESIAN_POINT ( 'NONE',  ( -1.381217146163000065, -77.55708155120599656, -12.08613957309999876 ) ) ;
#53975 = CARTESIAN_POINT ( 'NONE',  ( 0.000000000000000000, -80.89999999999999147, 0.000000000000000000 ) ) ;
#53977 = CARTESIAN_POINT ( 'NONE',  ( 1.066951212256000092, -78.66556959618499434, 1.077291633113999891 ) ) ;
#53976 = CARTESIAN_POINT ( 'NONE',  ( 0.1963495408493571848, -79.76458333333334849, 1.500000000000000666 ) ) ;
#53978 = CARTESIAN_POINT ( 'NONE',  ( 1.463006681111000074, -81.47722500425999215, -0.8714086385761999898 ) ) ;
#53979 = ORIENTED_EDGE ( 'NONE', *, *, #22557, .T. ) ;
#53980 = CARTESIAN_POINT ( 'NONE',  ( 3.588900492731000202, -82.63457450217399014, -0.05646551414434999860 ) ) ;
#53981 = DIRECTION ( 'NONE',  ( 2.273770411328430080E-11, 5.530779797664840897E-21, -1.000000000000000000 ) ) ;
#53982 = CARTESIAN_POINT ( 'NONE',  ( -1.615886945735000024, -81.02768543471519536, 11.05491664572000232 ) ) ;
#53983 = FACE_OUTER_BOUND ( 'NONE', #10386, .T. ) ;
#53984 = LINE ( 'NONE', #31819, #32060 ) ;
#53985 = CARTESIAN_POINT ( 'NONE',  ( 7.155101792066000499, -78.58303919030899465, -8.354909834651998324 ) ) ;
#53986 = FACE_OUTER_BOUND ( 'NONE', #2395, .T. ) ;
#53987 = CARTESIAN_POINT ( 'NONE',  ( -9.190938788893999956, -78.80234872708999205, 3.222784492720999872 ) ) ;
#53988 = CIRCLE ( 'NONE', #3088, 13.94827586206999825 ) ;
#53989 = CARTESIAN_POINT ( 'NONE',  ( -3.246742581843999886, -0.7641268662769999942, -2.093162713580000389 ) ) ;
#53990 = CARTESIAN_POINT ( 'NONE',  ( 9.167980031031000010, -78.99867172123299497, -2.618862957269000091 ) ) ;
#53991 = CARTESIAN_POINT ( 'NONE',  ( 12.79895559715999909, -23.80469146265000191, -2.015913954444999767 ) ) ;
#53992 = CARTESIAN_POINT ( 'NONE',  ( -7.634645345446921638, -55.32415927443500436, -10.10912681045557449 ) ) ;
#53993 = ORIENTED_EDGE ( 'NONE', *, *, #26299, .T. ) ;
#53994 = CARTESIAN_POINT ( 'NONE',  ( -0.6484536763416249849, -53.67597017256773739, -12.70397497887333671 ) ) ;
#53995 = CARTESIAN_POINT ( 'NONE',  ( 9.397888517861000324, -79.43011332859899198, -1.549072035286999993 ) ) ;
#53996 = DIRECTION ( 'NONE',  ( 0.000000000000000000, 1.000000000000000000, 0.000000000000000000 ) ) ;
#53997 = CARTESIAN_POINT ( 'NONE',  ( 0.1963495408493637351, -81.53541666666667709, -1.499999999999999778 ) ) ;
#53998 = CARTESIAN_POINT ( 'NONE',  ( 3.235517742858999846, -82.34726287204199480, -1.192291943657000086 ) ) ;
#53999 = CIRCLE ( 'NONE', #14410, 0.5999999999999999778 ) ;
#54000 = ORIENTED_EDGE ( 'NONE', *, *, #31610, .F. ) ;
#54001 = CARTESIAN_POINT ( 'NONE',  ( 7.958776490642000212, -61.27699850017000216, -9.723157983989999309 ) ) ;
#54002 = CARTESIAN_POINT ( 'NONE',  ( -1.636761686205420396, -1.083333333333333703, -2.839805762151339508 ) ) ;
#54003 = ORIENTED_EDGE ( 'NONE', *, *, #27261, .F. ) ;
#54004 = ORIENTED_EDGE ( 'NONE', *, *, #1941, .F. ) ;
#54005 = CIRCLE ( 'NONE', #29503, 1.199999999999999956 ) ;
#54006 = EDGE_CURVE ( 'NONE', #14347, #4408, #38690, .T. ) ;
#54007 = CARTESIAN_POINT ( 'NONE',  ( -10.13695543446000080, -55.09168900617999753, -7.646071007854999380 ) ) ;
#54008 = AXIS2_PLACEMENT_3D ( 'NONE', #48541, #57392, #20517 ) ;
#54009 = CARTESIAN_POINT ( 'NONE',  ( 9.523132023602000729, -80.02900749205798547, 1.108936319727999997 ) ) ;
#54010 = EDGE_LOOP ( 'NONE', ( #17853, #17254, #27573, #2697 ) ) ;
#54011 = CARTESIAN_POINT ( 'NONE',  ( -12.34758422210000184, -76.18886453605900044, 0.3526192563760000009 ) ) ;
#54012 = CARTESIAN_POINT ( 'NONE',  ( -9.952579048958215324, -78.63104145445697668, -4.074197893549214911 ) ) ;
#54013 = CARTESIAN_POINT ( 'NONE',  ( -1.613562824561000086, -78.78634084733999998, -0.3366025691675999520 ) ) ;
#54014 = ORIENTED_EDGE ( 'NONE', *, *, #19352, .F. ) ;
#54015 = CARTESIAN_POINT ( 'NONE',  ( 9.136202122873999798, -77.34189805011500596, 2.585973524422000125 ) ) ;
#54016 = CARTESIAN_POINT ( 'NONE',  ( 1.195573974400984119, -80.32674014211457347, -0.3649524205962666468 ) ) ;
#54017 = CARTESIAN_POINT ( 'NONE',  ( 12.45567317068999991, -78.30926792646000933, -3.566394712320999805 ) ) ;
#54018 = CARTESIAN_POINT ( 'NONE',  ( -8.729704736440837110, -77.69597548351386251, 7.043462628994999974 ) ) ;
#54019 = EDGE_CURVE ( 'NONE', #4032, #24723, #20417, .T. ) ;
#54020 = CARTESIAN_POINT ( 'NONE',  ( 3.140027144888846156, -86.25171435493598437, -1.398030157552344832 ) ) ;
#54021 = CARTESIAN_POINT ( 'NONE',  ( -9.346518596363001308, -77.72832879406675488, 2.610229778083999808 ) ) ;
#54022 = CARTESIAN_POINT ( 'NONE',  ( 5.434563164594669260, -79.92550071562423852, 7.484833654678077153 ) ) ;
#54023 = CARTESIAN_POINT ( 'NONE',  ( 11.00000000000000000, -78.44999999999998863, 0.000000000000000000 ) ) ;
#54024 = VERTEX_POINT ( 'NONE', #15393 ) ;
#54025 = DIRECTION ( 'NONE',  ( -0.7071067811865475727, 0.000000000000000000, 0.7071067811865475727 ) ) ;
#54026 = CARTESIAN_POINT ( 'NONE',  ( -7.685416442687999172, -76.62334360383999865, -9.616126112745998711 ) ) ;
#54027 = CARTESIAN_POINT ( 'NONE',  ( 0.6554565090088000368, -80.19211185406399522, 1.367230381797000183 ) ) ;
#54028 = CIRCLE ( 'NONE', #40839, 0.5000000000000006661 ) ;
#54029 = CARTESIAN_POINT ( 'NONE',  ( -0.9319389680074999793, -79.21513063462899140, -0.8127712196805999545 ) ) ;
#54030 = CARTESIAN_POINT ( 'NONE',  ( 3.212974253443096728, -3.132653343500664711, 1.435077393723246386 ) ) ;
#54031 = CARTESIAN_POINT ( 'NONE',  ( 12.49168433579000137, -23.29849137228000444, 1.667916687244999974 ) ) ;
#54032 = EDGE_CURVE ( 'NONE', #3236, #17043, #2405, .T. ) ;
#54033 = CARTESIAN_POINT ( 'NONE',  ( 1.298131932841000147, -76.56825554292399261, 12.21218573294999921 ) ) ;
#54034 = FACE_OUTER_BOUND ( 'NONE', #47279, .T. ) ;
#54035 = CARTESIAN_POINT ( 'NONE',  ( 8.429898053969001381, -78.31499867246799340, -7.120476661986999467 ) ) ;
#54036 = CARTESIAN_POINT ( 'NONE',  ( 9.623577716457999642, -77.69568832859899032, 0.3115139696998999730 ) ) ;
#54037 = CARTESIAN_POINT ( 'NONE',  ( 1.083270717429015040, -76.91794464775904316, 12.16356161538060832 ) ) ;
#54038 = CARTESIAN_POINT ( 'NONE',  ( 11.15679540746000065, -79.50823984478810758, 1.159321710118000004 ) ) ;
#54039 = ADVANCED_FACE ( 'NONE', ( #15681 ), #51424, .F. ) ;
#54040 = B_SPLINE_SURFACE_WITH_KNOTS ( 'NONE', 3, 3, ( 
 ( #18314, #36305, #22730, #18607, #49906, #40448, #9740, #14446, #23021, #624, #18891, #27728, #45772, #32441, #26551, #54329, #31267, #4137, #22135, #58156, #17723, #54033, #35710, #53739, #49309, #49612, #44882, #22433, #39, #18015, #40741, #36007, #31864, #13573, #31564 ),
 ( #45182, #13870, #37464, #10622, #37763, #38339, #38053, #55191, #56076, #20065, #33324, #10326, #55784, #56363, #19766, #15334, #1772, #28603, #2064, #29186, #20344, #42785, #51361, #10037, #15033, #10917, #28306, #28897, #46357, #50486, #46944, #47234, #6469, #14732, #33616 ),
 ( #24480, #51074, #24187, #5881, #42495, #15621, #28020, #23889, #1481, #46065, #51660, #33028, #11208, #41908, #5587, #6762, #15913, #19471, #24772, #46650, #42205, #23600, #2349, #41612, #19183, #1193, #6177, #50781, #37178, #32732, #55485, #29470, #25054, #25627, #33898 ),
 ( #12062, #3485, #44222, #52504, #30042, #34184, #57792, #3771, #3209, #21199, #56650, #2637, #7626, #38916, #2915, #34473, #51941, #20913, #48374, #56934, #43650, #39200, #48095, #43936, #16783, #7339, #21491, #21774, #52790, #34764, #8202, #39497, #57501, #17063, #39778 ) ),
 .UNSPECIFIED., .F., .F., .F.,
 ( 4, 4 ),
 ( 4, 1, 1, 1, 1, 1, 1, 1, 1, 1, 1, 1, 1, 1, 1, 1, 1, 1, 1, 1, 1, 1, 1, 1, 1, 1, 1, 1, 1, 1, 1, 1, 4 ),
 ( -0.5168282991434000051, 1.516828299142999992 ),
 ( -0.01510644027126000107, 0.009441525169539000117, 0.03398949061033999797, 0.05853745605114000355, 0.08308542149195000115, 0.1076333869326999981, 0.1321813523735999862, 0.1567293178143999988, 0.1812772832552000113, 0.2058252486960000238, 0.2303732141367999808, 0.2549211795776000211, 0.2794691450183999781, 0.3040171104591999907, 0.3285650759000000032, 0.3531130413408000157, 0.3776610067816000282, 0.4022089722223999853, 0.4267569376631999978, 0.4513049031039999548, 0.4758528685447999673, 0.5004008339856000909, 0.5249487994264000479, 0.5494967648672000049, 0.5740447303079999619, 0.5985926957488000300, 0.6231406611895999870, 0.6476886266303999440, 0.6722365920712000120, 0.6967845575119999690, 0.7213325229527999261, 0.7458804883935999941, 0.7704284538343999511 ),
 .UNSPECIFIED. ) ;
#54041 = CARTESIAN_POINT ( 'NONE',  ( -1.500000000000000000, -77.50000000000000000, 0.000000000000000000 ) ) ;
#54042 = ORIENTED_EDGE ( 'NONE', *, *, #19264, .F. ) ;
#54043 = CARTESIAN_POINT ( 'NONE',  ( 0.6445170026176001432, -82.29550046658999918, 1.319487011787000119 ) ) ;
#54044 = CARTESIAN_POINT ( 'NONE',  ( 0.7658660592953000501, -79.84702375444000211, 1.113292320107999833 ) ) ;
#54045 = LINE ( 'NONE', #13582, #42744 ) ;
#54046 = DIRECTION ( 'NONE',  ( 0.000000000000000000, 1.000000000000000000, 0.000000000000000000 ) ) ;
#54047 = CARTESIAN_POINT ( 'NONE',  ( -10.07627163191000008, -60.04999999657000131, 7.601397897754999633 ) ) ;
#54048 = VECTOR ( 'NONE', #38439, 1000.000000000000000 ) ;
#54049 = CARTESIAN_POINT ( 'NONE',  ( 9.468750000004000356, -79.53124999999600675, -6.681056941828999630E-10 ) ) ;
#54050 = CARTESIAN_POINT ( 'NONE',  ( 7.920136950582000068, -77.80304415034599685, 4.778486233528999705 ) ) ;
#54051 = CARTESIAN_POINT ( 'NONE',  ( -0.4450739772406999695, -53.92186785164999918, -12.43586747591000119 ) ) ;
#54052 = CARTESIAN_POINT ( 'NONE',  ( 3.350051352536504545, -76.05149132198432937, 11.26355013934140104 ) ) ;
#54053 = CARTESIAN_POINT ( 'NONE',  ( 10.60715898610999908, -79.75759371423698951, -2.581384170113000032 ) ) ;
#54054 = CARTESIAN_POINT ( 'NONE',  ( 3.518657424384978416, -85.83735716284299144, -1.566607219110048188 ) ) ;
#54055 = ORIENTED_EDGE ( 'NONE', *, *, #52301, .F. ) ;
#54056 = CARTESIAN_POINT ( 'NONE',  ( -4.855043705795097253, -78.21750000000001535, 8.214633846514278304 ) ) ;
#54057 = CARTESIAN_POINT ( 'NONE',  ( 8.838834764832000701, -60.04999999966999980, 8.838834764832000701 ) ) ;
#54058 = CARTESIAN_POINT ( 'NONE',  ( -3.437217408589773093, -78.67390000031812747, -1.942147800595485974 ) ) ;
#54059 = CARTESIAN_POINT ( 'NONE',  ( -13.89248035986000041, -46.40840747658999277, -2.632528379792999703E-05 ) ) ;
#54060 = CARTESIAN_POINT ( 'NONE',  ( -10.65673661723999999, -78.91092244544400103, 2.626400817186000047 ) ) ;
#54061 = PLANE ( 'NONE',  #14735 ) ;
#54062 = EDGE_CURVE ( 'NONE', #14498, #26643, #10980, .T. ) ;
#54063 = CARTESIAN_POINT ( 'NONE',  ( 12.00000000000000000, -77.66041666666669130, 1.570796326794922093 ) ) ;
#54064 = DIRECTION ( 'NONE',  ( -0.7071067811865475727, 0.000000000000000000, 0.7071067811865475727 ) ) ;
#54065 = CARTESIAN_POINT ( 'NONE',  ( -4.249989987144469517, -76.90707437668547186, 9.952789594769198445 ) ) ;
#54066 = ORIENTED_EDGE ( 'NONE', *, *, #33501, .F. ) ;
#54067 = CARTESIAN_POINT ( 'NONE',  ( -1.788059198778999770, -79.88890251626278882, -11.11920900327000084 ) ) ;
#54068 = CARTESIAN_POINT ( 'NONE',  ( -7.582587422050910853, -77.44990485243668843, 5.494244969997139627 ) ) ;
#54069 = CARTESIAN_POINT ( 'NONE',  ( 0.000000000000000000, -76.75499999999999545, 0.000000000000000000 ) ) ;
#54070 = CARTESIAN_POINT ( 'NONE',  ( -2.347024351938371112, -78.48547955770030171, 3.892553724173937191 ) ) ;
#54071 = CARTESIAN_POINT ( 'NONE',  ( 11.74960618672723101, -76.44458049160198243, -0.7033066962385277066 ) ) ;
#54072 = CARTESIAN_POINT ( 'NONE',  ( -10.20553722967999910, -78.33823118367698157, -4.233781229625999565 ) ) ;
#54073 = CARTESIAN_POINT ( 'NONE',  ( 8.190859204290999784, -55.64999999967000122, 7.342331066867000544 ) ) ;
#54074 = CARTESIAN_POINT ( 'NONE',  ( -1.119262997622045175, -81.79061289717962779, 1.016493713523941578 ) ) ;
#54075 = CARTESIAN_POINT ( 'NONE',  ( -1.310679582531386611, -81.04166666666668561, -0.7554284705563495406 ) ) ;
#54076 = CARTESIAN_POINT ( 'NONE',  ( -12.50686284812396742, -54.49510763085821452, -1.423064270604161630 ) ) ;
#54077 = CARTESIAN_POINT ( 'NONE',  ( -6.606377239730371720, -78.42708333333332860, 8.596418555780411808 ) ) ;
#54078 = AXIS2_PLACEMENT_3D ( 'NONE', #37690, #23815, #32657 ) ;
#54079 = CARTESIAN_POINT ( 'NONE',  ( -12.66235429707000115, -25.13741783422999987, 0.4955846680317000374 ) ) ;
#54080 = ORIENTED_EDGE ( 'NONE', *, *, #8627, .F. ) ;
#54081 = VERTEX_POINT ( 'NONE', #47589 ) ;
#54082 = CARTESIAN_POINT ( 'NONE',  ( 0.000000000000000000, -0.5000000000000000000, 0.000000000000000000 ) ) ;
#54083 = ORIENTED_EDGE ( 'NONE', *, *, #52773, .F. ) ;
#54084 = CARTESIAN_POINT ( 'NONE',  ( -7.766269599678000013, -78.62242792576000738, -9.491266709826000181 ) ) ;
#54085 = VERTEX_POINT ( 'NONE', #20406 ) ;
#54086 = CARTESIAN_POINT ( 'NONE',  ( 7.761030428335000231, -24.08151201375000028, 9.835168816226000033 ) ) ;
#54087 = CARTESIAN_POINT ( 'NONE',  ( -8.507210620304000770, -77.69605693914598987, -7.023467935662000450 ) ) ;
#54088 = AXIS2_PLACEMENT_3D ( 'NONE', #39807, #34503, #38946 ) ;
#54089 = CARTESIAN_POINT ( 'NONE',  ( -12.50000000000000000, -13.07071424677999971, 0.000000000000000000 ) ) ;
#54091 = EDGE_CURVE ( 'NONE', #5785, #33530, #20692, .T. ) ;
#54090 = CARTESIAN_POINT ( 'NONE',  ( -0.8449659473473000171, -79.01128998579800111, 9.650246712936999316 ) ) ;
#54092 = CARTESIAN_POINT ( 'NONE',  ( -3.451502316031555662, -78.19470348729451814, -8.581920319061078217 ) ) ;
#54093 = CARTESIAN_POINT ( 'NONE',  ( 11.15679540746000065, -79.45655663070499486, 1.159321710118000004 ) ) ;
#54094 = CARTESIAN_POINT ( 'NONE',  ( 3.176273880393910787, -1.831745995345729128, -0.8078237210779479760 ) ) ;
#54095 = ORIENTED_EDGE ( 'NONE', *, *, #25472, .F. ) ;
#54096 = ORIENTED_EDGE ( 'NONE', *, *, #56593, .F. ) ;
#54097 = CARTESIAN_POINT ( 'NONE',  ( 0.8199666693160626574, -77.46800884939443677, 9.216836058761973760 ) ) ;
#54098 = CARTESIAN_POINT ( 'NONE',  ( -10.47078769031000078, -77.95581897413698869, -3.499536356729999742 ) ) ;
#54099 = CARTESIAN_POINT ( 'NONE',  ( -3.907230163516999699, -77.98247802377198923, -8.882807090995999744 ) ) ;
#54100 = CARTESIAN_POINT ( 'NONE',  ( 6.665976575492000400, -76.17302026400000159, -11.30427740477999876 ) ) ;
#54101 = CARTESIAN_POINT ( 'NONE',  ( -4.778511751969061194, -79.48269898195434280, -8.212683968085311648 ) ) ;
#54102 = CARTESIAN_POINT ( 'NONE',  ( 0.3877229342594999961, -77.91453410555999426, -1.580612325761999948 ) ) ;
#54103 = CARTESIAN_POINT ( 'NONE',  ( -11.00000000000000000, -78.19999999999998863, 0.000000000000000000 ) ) ;
#54104 = CARTESIAN_POINT ( 'NONE',  ( -9.062201444876000878, -78.88186501710097787, 6.128973919716999674 ) ) ;
#54105 = CARTESIAN_POINT ( 'NONE',  ( -0.1636246173744673738, -78.11458333333330017, -1.249999999999999778 ) ) ;
#54106 = EDGE_CURVE ( 'NONE', #48229, #12675, #11265, .T. ) ;
#54107 = CARTESIAN_POINT ( 'NONE',  ( -7.396918292183162436, -78.55208333333332860, -5.684557159767966716 ) ) ;
#54108 = CARTESIAN_POINT ( 'NONE',  ( 0.1764146904384000236, -85.62493728501499390, 3.585048402307000170 ) ) ;
#54109 = EDGE_LOOP ( 'NONE', ( #47651, #55986, #57251, #16345 ) ) ;
#54110 = CARTESIAN_POINT ( 'NONE',  ( -2.550058755020000234, -79.48197165242800111, -12.16911022628999994 ) ) ;
#54111 = CARTESIAN_POINT ( 'NONE',  ( 6.067686772785999771, -75.97136531054800912, 9.621429083000000659 ) ) ;
#54112 = CARTESIAN_POINT ( 'NONE',  ( -7.708860374575333907, -78.03865554921938497, 7.492616441312939912 ) ) ;
#54113 = CARTESIAN_POINT ( 'NONE',  ( -6.777984382448000389, -78.21103772225399098, -9.878005474088999094 ) ) ;
#54114 = CARTESIAN_POINT ( 'NONE',  ( -12.70556836326691474, -62.02772277412548618, 0.2597962962374435469 ) ) ;
#54115 = DIRECTION ( 'NONE',  ( -1.000000000000000000, 0.000000000000000000, 0.000000000000000000 ) ) ;
#54116 = LINE ( 'NONE', #8950, #21364 ) ;
#54117 = CARTESIAN_POINT ( 'NONE',  ( 2.661146832675047147, -80.95524119419135900, 10.42413934193408309 ) ) ;
#54118 = CARTESIAN_POINT ( 'NONE',  ( -5.148735870932999781, -80.20852921644699052, -10.17300617436000110 ) ) ;
#54119 = CARTESIAN_POINT ( 'NONE',  ( -4.784380313523538319, -78.38333333333332575, -8.300970689365453126 ) ) ;
#54120 = CARTESIAN_POINT ( 'NONE',  ( -8.675294248904002359, -77.83711156713900436, 6.999562148147999707 ) ) ;
#54121 = CARTESIAN_POINT ( 'NONE',  ( 1.636761686205415067, -1.833333333333333481, 2.839805762151342616 ) ) ;
#54122 = CARTESIAN_POINT ( 'NONE',  ( -3.046770093036999860, -80.56158377905549628, -10.59643116276000008 ) ) ;
#54123 = ORIENTED_EDGE ( 'NONE', *, *, #25472, .T. ) ;
#54124 = CARTESIAN_POINT ( 'NONE',  ( 2.065394024360999836, -55.37838567321000482, 12.82193048525000023 ) ) ;
#54125 = CARTESIAN_POINT ( 'NONE',  ( -4.802567994450000377, -77.23279903538302449, -8.191018798270000900 ) ) ;
#54126 = CARTESIAN_POINT ( 'NONE',  ( 3.651330038711999570, -2.087546241516999856, 1.548846843139000118 ) ) ;
#54127 = CARTESIAN_POINT ( 'NONE',  ( 10.79417609527999922, -77.42640152541599718, -3.050225076229999832 ) ) ;
#54128 = CARTESIAN_POINT ( 'NONE',  ( 10.97550047727999889, -78.05991538145298136, 0.05101033830554000531 ) ) ;
#54129 = CARTESIAN_POINT ( 'NONE',  ( 1.243547092045970581, -77.43541666666665435, -9.500000000000000000 ) ) ;
#54130 = CARTESIAN_POINT ( 'NONE',  ( 10.20000000000000107, -0.2000000000000000111, 0.000000000000000000 ) ) ;
#54131 = CLOSED_SHELL ( 'NONE', ( #37907, #42749, #47329, #5707, #8476, #26195, #30555, #53471, #41022, #35489, #16186, #48319 ) ) ;
#54132 = EDGE_CURVE ( 'NONE', #27512, #9574, #15970, .T. ) ;
#54133 = CARTESIAN_POINT ( 'NONE',  ( -2.062323307449999810, -60.02713153159000115, 12.83634826445999977 ) ) ;
#54134 = CARTESIAN_POINT ( 'NONE',  ( 12.66737112516999986, -17.76697834132999887, 1.690666607834999891 ) ) ;
#54135 = CARTESIAN_POINT ( 'NONE',  ( -1.813145781940000090, -86.12182450217399321, 3.710959265555000108 ) ) ;
#54136 = CYLINDRICAL_SURFACE ( 'NONE', #3706, 2.600000000000000089 ) ;
#54137 = CARTESIAN_POINT ( 'NONE',  ( 9.830798712606000578, -54.70910918491000530, -7.765013391389000041 ) ) ;
#54138 = CARTESIAN_POINT ( 'NONE',  ( 10.80251317621999974, -78.04940181198600158, 3.184285419974999698 ) ) ;
#54139 = CARTESIAN_POINT ( 'NONE',  ( -0.6332123272625999055, -81.11720461324000553, 1.540853336418999797 ) ) ;
#54140 = CARTESIAN_POINT ( 'NONE',  ( -1.485441059218000293, -77.87043921376999833, 0.4397084800123000070 ) ) ;
#54141 = CARTESIAN_POINT ( 'NONE',  ( 0.8804656547168402403, -61.82803394679353204, 12.70299681155804983 ) ) ;
#54142 = CARTESIAN_POINT ( 'NONE',  ( 1.009312198048121445, -83.06780995641257448, 1.154596580929102556 ) ) ;
#54143 = CARTESIAN_POINT ( 'NONE',  ( -12.66001556635999847, -61.43260856911000189, 1.381621105853999998 ) ) ;
#54144 = CARTESIAN_POINT ( 'NONE',  ( -2.169167664939000151, -78.24083109332160291, 10.75912301088999889 ) ) ;
#54145 = EDGE_CURVE ( 'NONE', #8940, #41814, #25609, .T. ) ;
#54146 = CARTESIAN_POINT ( 'NONE',  ( 8.596418555780450887, -77.19791666666668561, -6.606377239730321982 ) ) ;
#54147 = CARTESIAN_POINT ( 'NONE',  ( 0.5252637606625818467, -77.80901481852902180, -1.160894468899167364 ) ) ;
#54148 = ORIENTED_EDGE ( 'NONE', *, *, #16607, .T. ) ;
#54149 = CARTESIAN_POINT ( 'NONE',  ( 1.123730751682942453, -81.81383862517986927, -0.5490724999909163406 ) ) ;
#54150 = CARTESIAN_POINT ( 'NONE',  ( -8.796335266379998075, -79.54791666666665151, 6.760013919724039866 ) ) ;
#54151 = CARTESIAN_POINT ( 'NONE',  ( 9.395013887366999938, -79.18635809738199782, 5.999026139886999509 ) ) ;
#54152 = CIRCLE ( 'NONE', #15506, 1.250000000000000444 ) ;
#54153 = CARTESIAN_POINT ( 'NONE',  ( -1.980584515752000119, -55.53514853344000102, -12.76303204600000107 ) ) ;
#54154 = VERTEX_POINT ( 'NONE', #47868 ) ;
#54155 = ORIENTED_EDGE ( 'NONE', *, *, #39325, .T. ) ;
#54156 = CARTESIAN_POINT ( 'NONE',  ( -0.2218574163239999952, -81.60597385339299592, -1.599372756014999952 ) ) ;
#54157 = ORIENTED_EDGE ( 'NONE', *, *, #54826, .T. ) ;
#54158 = CIRCLE ( 'NONE', #26773, 1.499999999999999556 ) ;
#54159 = EDGE_LOOP ( 'NONE', ( #48702, #2680, #32790, #40645, #54422 ) ) ;
#54160 = PLANE ( 'NONE',  #24533 ) ;
#54161 = DIRECTION ( 'NONE',  ( -1.000000000000000000, 0.000000000000000000, 0.000000000000000000 ) ) ;
#54162 = CARTESIAN_POINT ( 'NONE',  ( 1.460959015002472494, -78.27083333333335702, 0.3926218265389233020 ) ) ;
#54164 = EDGE_CURVE ( 'NONE', #7174, #25733, #7028, .T. ) ;
#54163 = CARTESIAN_POINT ( 'NONE',  ( 0.005928781627658000382, -25.20113050262999721, -12.66336824419000173 ) ) ;
#54165 = AXIS2_PLACEMENT_3D ( 'NONE', #6140, #29149, #24147 ) ;
#54166 = CARTESIAN_POINT ( 'NONE',  ( -0.9905238183362000681, -81.58007094306199747, 3.450015621052000103 ) ) ;
#54167 = CARTESIAN_POINT ( 'NONE',  ( -9.472578462795231857, -79.39381934248991968, 0.7201139491716196384 ) ) ;
#54168 = CARTESIAN_POINT ( 'NONE',  ( -4.789974786805000662, -77.93928760227905173, -9.946872946892002076 ) ) ;
#54169 = CARTESIAN_POINT ( 'NONE',  ( 11.47679389412999917, -78.51599167770000065, 3.196029325000000032 ) ) ;
#54171 = EDGE_LOOP ( 'NONE', ( #53917, #234, #54083, #5191, #35126 ) ) ;
#54170 = APPLICATION_CONTEXT ( 'automotive_design' ) ;
#54173 = EDGE_LOOP ( 'NONE', ( #11553, #29995, #8333, #10717 ) ) ;
#54172 = EDGE_CURVE ( 'NONE', #8616, #45142, #35394, .T. ) ;
#54174 = LINE ( 'NONE', #40879, #30114 ) ;
#54175 = CARTESIAN_POINT ( 'NONE',  ( -7.223234266881706667, -76.97379502737749135, -9.635782272404652460 ) ) ;
#54176 = VECTOR ( 'NONE', #21400, 1000.000000000000000 ) ;
#54177 = CARTESIAN_POINT ( 'NONE',  ( 0.9336649615752000697, -80.40860138265699675, -0.9522845488933000535 ) ) ;
#54178 = CARTESIAN_POINT ( 'NONE',  ( 9.131029190779001325, -77.43205946808298279, -3.285576857342999979 ) ) ;
#54179 = CARTESIAN_POINT ( 'NONE',  ( 2.636417525263768713, -86.31452044229999387, -3.702674772290223348 ) ) ;
#54180 = CARTESIAN_POINT ( 'NONE',  ( 11.09875712452000052, -76.16149361465799927, 1.375294608629999971 ) ) ;
#54181 = CARTESIAN_POINT ( 'NONE',  ( 11.63291926114999875, -77.11568903011000486, 5.337072863433999892 ) ) ;
#54182 = CARTESIAN_POINT ( 'NONE',  ( -10.29607860738999925, -77.19512210326000456, 7.334573225905999472 ) ) ;
#54183 = CARTESIAN_POINT ( 'NONE',  ( -10.70541732380000077, -76.51213885926499358, 1.965825919828999790 ) ) ;
#54184 = EDGE_CURVE ( 'NONE', #4989, #27639, #24660, .T. ) ;
#54185 = DIRECTION ( 'NONE',  ( 1.000000000000000000, 0.000000000000000000, 0.000000000000000000 ) ) ;
#54186 = CARTESIAN_POINT ( 'NONE',  ( 4.161023627692999938, -79.45518468237709442, 0.3097663532143999920 ) ) ;
#54187 = CARTESIAN_POINT ( 'NONE',  ( -7.960542989054001595, -80.77134138352347748, 7.971132368775000643 ) ) ;
#54188 = CARTESIAN_POINT ( 'NONE',  ( 10.48543666025108401, -76.59166666666665435, 6.043427764450814976 ) ) ;
#54189 = CARTESIAN_POINT ( 'NONE',  ( -5.747123378374999980, -78.21567021303999923, 10.24856442990000005 ) ) ;
#54190 = CARTESIAN_POINT ( 'NONE',  ( -2.503181846702999813, -81.53082046129100036, 2.513689163497000223 ) ) ;
#54191 = CARTESIAN_POINT ( 'NONE',  ( -1.159125165887999964, -77.69135616363169561, 0.4678983327651999868 ) ) ;
#54192 = DIRECTION ( 'NONE',  ( 0.000000000000000000, -1.000000000000000000, 0.000000000000000000 ) ) ;
#54193 = CARTESIAN_POINT ( 'NONE',  ( 8.828526701892000617, -80.59834844877070736, -6.997593314318000246 ) ) ;
#54194 = CARTESIAN_POINT ( 'NONE',  ( -0.6295237254636235624, -79.08333333333332860, -1.092232985442822990 ) ) ;
#54195 = ORIENTED_EDGE ( 'NONE', *, *, #12093, .T. ) ;
#54196 = FACE_OUTER_BOUND ( 'NONE', #26603, .T. ) ;
#54197 = DIRECTION ( 'NONE',  ( 0.000000000000000000, 1.000000000000000000, 0.000000000000000000 ) ) ;
#54198 = AXIS2_PLACEMENT_3D ( 'NONE', #49560, #53981, #26798 ) ;
#54199 = CARTESIAN_POINT ( 'NONE',  ( -1.321095329625999959, -82.23281938082300258, -0.1826337427822999904 ) ) ;
#54200 = AXIS2_PLACEMENT_3D ( 'NONE', #36385, #45558, #46149 ) ;
#54201 = CARTESIAN_POINT ( 'NONE',  ( -1.882840341529000039, -79.93872424662198739, -9.567914882252001263 ) ) ;
#54203 = CARTESIAN_POINT ( 'NONE',  ( -12.97861384075000046, -78.02312312080999845, -0.9459496016724999734 ) ) ;
#54202 = B_SPLINE_CURVE_WITH_KNOTS ( 'NONE', 3,
 ( #9682, #27670, #45716, #43242, #19938, #6642, #7221, #20515, #10792, #2800, #34067, #25223, #29353, #47400, #24935, #38221, #38512, #15792, #24362 ),
 .UNSPECIFIED., .F., .F.,
 ( 4, 1, 1, 1, 1, 1, 1, 1, 1, 1, 1, 1, 1, 1, 1, 1, 4 ),
 ( 0.5000000000000000000, 0.5324999662279407131, 0.5649999184674565633, 0.5974998707067776804, 0.6299998229462931976, 0.6624997751858089368, 0.6949997274251300539, 0.7274996796646455710, 0.7599996319041613102, 0.7924995841434823163, 0.8249995363829980555, 0.8574994886225137947, 0.8899994408618348007, 0.9224993931013505399, 0.9549993453408660571, 0.9874992975801872852, 1.000000000000000000 ),
 .UNSPECIFIED. ) ;
#54204 = CARTESIAN_POINT ( 'NONE',  ( -2.309360228211999821, -79.67616001420199723, -9.234877421806000797 ) ) ;
#54205 = CARTESIAN_POINT ( 'NONE',  ( 10.09635500655283735, -18.47627834136018166, 7.644087038114626864 ) ) ;
#54206 = ORIENTED_EDGE ( 'NONE', *, *, #13019, .F. ) ;
#54207 = CIRCLE ( 'NONE', #50423, 0.5000000000000004441 ) ;
#54208 = CARTESIAN_POINT ( 'NONE',  ( -8.130811096542000627, -24.68523690389000080, -9.546858433121998999 ) ) ;
#54209 = CARTESIAN_POINT ( 'NONE',  ( 11.75000000000000000, -77.54999999999999716, 2.316376715183999699E-14 ) ) ;
#54210 = CARTESIAN_POINT ( 'NONE',  ( 1.362073333348000181, -81.52683166077699184, -0.3585378043983000196 ) ) ;
#54211 = DIRECTION ( 'NONE',  ( 1.000000000000000000, 0.000000000000000000, 0.000000000000000000 ) ) ;
#54212 = CARTESIAN_POINT ( 'NONE',  ( 7.267019124662000173, -77.65102789785198922, -6.153113788875000267 ) ) ;
#54214 = CARTESIAN_POINT ( 'NONE',  ( -1.180494763713999973, -0.6498550533857000433, 3.461421590595000097 ) ) ;
#54213 = CARTESIAN_POINT ( 'NONE',  ( -0.8079786370952000141, -83.47200654646700002, -4.095946834719000229 ) ) ;
#54215 = CARTESIAN_POINT ( 'NONE',  ( -1.217465845835396188, -82.47916666666667140, 0.3271848554490955907 ) ) ;
#54216 = CARTESIAN_POINT ( 'NONE',  ( 1.125436458607999901, -79.45174468460000128, 0.6884462015638999066 ) ) ;
#54217 = ORIENTED_EDGE ( 'NONE', *, *, #20617, .F. ) ;
#54218 = EDGE_CURVE ( 'NONE', #18403, #5025, #17121, .T. ) ;
#54219 = CARTESIAN_POINT ( 'NONE',  ( 7.162480479084130991, -77.28307999974209963, -8.040150979671629727 ) ) ;
#54220 = CARTESIAN_POINT ( 'NONE',  ( -10.98362417419999915, -23.15000000000000213, -0.5999999999999999778 ) ) ;
#54221 = VERTEX_POINT ( 'NONE', #12405 ) ;
#54222 = VERTEX_POINT ( 'NONE', #21833 ) ;
#54223 = CARTESIAN_POINT ( 'NONE',  ( -1.028867309006398445, -77.75000000000001421, 1.135838062686344241 ) ) ;
#54224 = CARTESIAN_POINT ( 'NONE',  ( -1.624989163556999141E-14, -74.59999999999999432, -11.00000000000000000 ) ) ;
#54225 = FACE_OUTER_BOUND ( 'NONE', #19519, .T. ) ;
#54226 = ORIENTED_EDGE ( 'NONE', *, *, #45602, .T. ) ;
#54227 = CARTESIAN_POINT ( 'NONE',  ( -12.03258451680999919, -78.18689196713800982, 0.6424029262030001020 ) ) ;
#54228 = VERTEX_POINT ( 'NONE', #13565 ) ;
#54229 = B_SPLINE_SURFACE_WITH_KNOTS ( 'NONE', 3, 3, ( 
 ( #33369, #15661, #10959, #28940 ),
 ( #2955, #52830, #44551, #8531 ),
 ( #48698, #25667, #48134, #57257 ),
 ( #12386, #43694, #30375, #22105 ),
 ( #26524, #40115, #3814, #4104 ),
 ( #3249, #17390, #58128, #16823 ),
 ( #17690, #48415, #35681, #3528 ),
 ( #29792, #47848, #34806, #7951 ) ),
 .UNSPECIFIED., .F., .F., .F.,
 ( 4, 1, 1, 1, 1, 4 ),
 ( 4, 4 ),
 ( -0.01200407345747999885, 0.000000000000000000, 0.3333333333333000081, 0.6666666666667000474, 1.000000000000000000, 1.011997855551999947 ),
 ( -0.3559705542741999906, 1.355970554273999928 ),
 .UNSPECIFIED. ) ;
#54230 = ORIENTED_EDGE ( 'NONE', *, *, #57145, .T. ) ;
#54231 = CARTESIAN_POINT ( 'NONE',  ( -7.919595949288999570, -55.65000000893999754, -9.050966798898000931 ) ) ;
#54232 = LINE ( 'NONE', #13769, #52151 ) ;
#54233 = LINE ( 'NONE', #19381, #4430 ) ;
#54234 = AXIS2_PLACEMENT_3D ( 'NONE', #19642, #46824, #1077 ) ;
#54235 = EDGE_LOOP ( 'NONE', ( #57352, #48721, #52549, #28869 ) ) ;
#54236 = CARTESIAN_POINT ( 'NONE',  ( -1.499529583595990090, -81.88967706888531950, 0.1963376940543553328 ) ) ;
#54238 = ADVANCED_FACE ( 'NONE', ( #30967 ), #31555, .F. ) ;
#54237 = ORIENTED_EDGE ( 'NONE', *, *, #12772, .T. ) ;
#54239 = CARTESIAN_POINT ( 'NONE',  ( -1.273668632959473745, -80.14653265090674950, 0.05892260551989451922 ) ) ;
#54240 = CIRCLE ( 'NONE', #41970, 3.600000000000000089 ) ;
#54241 = DIRECTION ( 'NONE',  ( -1.000000000000000000, 0.000000000000000000, 0.000000000000000000 ) ) ;
#54242 = CARTESIAN_POINT ( 'NONE',  ( 12.00000000000000000, -18.75000000000000000, 0.000000000000000000 ) ) ;
#54243 = TOROIDAL_SURFACE ( 'NONE', #36318, 13.50000000000000000, 0.5000000000000000000 ) ;
#54244 = CARTESIAN_POINT ( 'NONE',  ( -7.691916945430000041, -20.24634220924000161, -10.42274798266999980 ) ) ;
#54245 = CARTESIAN_POINT ( 'NONE',  ( -8.441176281571586060, -24.91652561798867183, 9.243148034848644556 ) ) ;
#54246 = CARTESIAN_POINT ( 'NONE',  ( 11.61175053437844795, -76.53594503550665706, -2.075198828568620701 ) ) ;
#54247 = CARTESIAN_POINT ( 'NONE',  ( -5.261498566940001176, -77.73881614468353973, -10.76255997729999869 ) ) ;
#54248 = EDGE_CURVE ( 'NONE', #24315, #8754, #35700, .T. ) ;
#54249 = CARTESIAN_POINT ( 'NONE',  ( 7.692184310832279159, -78.80316060324501848, -5.137369332712866665 ) ) ;
#54250 = CARTESIAN_POINT ( 'NONE',  ( 4.275783788279646558, -77.00602939643633249, -10.37011484984485676 ) ) ;
#54251 = CARTESIAN_POINT ( 'NONE',  ( 0.000000000000000000, -80.99999999999998579, 7.000000000000000000 ) ) ;
#54252 = CARTESIAN_POINT ( 'NONE',  ( -0.9218200799623714747, -79.97291666666667709, -1.199500263597270466 ) ) ;
#54253 = EDGE_CURVE ( 'NONE', #46629, #19319, #25317, .T. ) ;
#54254 = LINE ( 'NONE', #12417, #48760 ) ;
#54255 = CARTESIAN_POINT ( 'NONE',  ( -4.699224227394298126, -78.35979949309869141, 11.12336296093753596 ) ) ;
#54256 = CARTESIAN_POINT ( 'NONE',  ( -2.265188552264999711, -80.12503455456798918, -3.251907382878999719 ) ) ;
#54257 = CARTESIAN_POINT ( 'NONE',  ( 2.801992291048324812, -76.27265625000197247, 11.67810493544244999 ) ) ;
#54258 = CARTESIAN_POINT ( 'NONE',  ( 12.51072239526000196, -52.49705297114005020, -0.7871079366006996647 ) ) ;
#54259 = CARTESIAN_POINT ( 'NONE',  ( -1.814305421036000121, -24.28941969330999839, 12.78003582253000125 ) ) ;
#54260 = CARTESIAN_POINT ( 'NONE',  ( -1.250000000000000000, -82.25000000000000000, 8.279869130157999738E-11 ) ) ;
#54261 = DIRECTION ( 'NONE',  ( 1.000000000000000000, 0.000000000000000000, 0.000000000000000000 ) ) ;
#54262 = CARTESIAN_POINT ( 'NONE',  ( 2.588085340131999867, -1.699711001040999925, 2.991890042761000235 ) ) ;
#54263 = CARTESIAN_POINT ( 'NONE',  ( -1.217465845835396188, -80.97916666666667140, 0.3271848554490955907 ) ) ;
#54264 = CARTESIAN_POINT ( 'NONE',  ( 12.76303204294999993, -23.26485150694999859, -1.980584515756000030 ) ) ;
#54265 = CARTESIAN_POINT ( 'NONE',  ( -0.3900435134041961294, -80.45456690170814795, -1.498726833963420102 ) ) ;
#54266 = CARTESIAN_POINT ( 'NONE',  ( -0.8975083509913929225, -78.53903619159790139, 0.8699955927291534996 ) ) ;
#54267 = DIRECTION ( 'NONE',  ( 0.000000000000000000, -0.1961161351384349827, -0.9805806756908699295 ) ) ;
#54268 = LINE ( 'NONE', #30916, #35132 ) ;
#54269 = CARTESIAN_POINT ( 'NONE',  ( -10.66734455299000039, -77.50954786493399240, 2.320156498608999751 ) ) ;
#54270 = CARTESIAN_POINT ( 'NONE',  ( 1.735064171737695782, -77.31256701792597141, 10.69912951762188058 ) ) ;
#54271 = CARTESIAN_POINT ( 'NONE',  ( -10.75000000000000000, -76.50000000000000000, 0.000000000000000000 ) ) ;
#54272 = EDGE_CURVE ( 'NONE', #19448, #46033, #30222, .T. ) ;
#54274 = CARTESIAN_POINT ( 'NONE',  ( -0.6817061190079000133, -78.76479484294699773, 1.354333385606999896 ) ) ;
#54273 = DIRECTION ( 'NONE',  ( -1.000000000000000000, 0.000000000000000000, 0.000000000000000000 ) ) ;
#54275 = DIRECTION ( 'NONE',  ( 1.000000000000000000, 0.000000000000000000, 0.000000000000000000 ) ) ;
#54276 = EDGE_LOOP ( 'NONE', ( #29594, #47358, #5861, #23144 ) ) ;
#54277 = CARTESIAN_POINT ( 'NONE',  ( -3.377828507812000058, -86.23049735065200139, 0.3693357844676999902 ) ) ;
#54278 = CARTESIAN_POINT ( 'NONE',  ( 0.2367807722781999913, -79.49682939073299792, 11.92391661984999907 ) ) ;
#54279 = VECTOR ( 'NONE', #41869, 1000.000000000000114 ) ;
#54280 = CARTESIAN_POINT ( 'NONE',  ( 11.04613657998999976, -80.82006762628775220, -0.4641449021664000307 ) ) ;
#54281 = B_SPLINE_CURVE_WITH_KNOTS ( 'NONE', 3,
 ( #27620, #45660, #5203, #50672, #799, #18781, #36773, #32331, #19075, #24376, #52118, #11678, #29367, #33794, #24949, #38234, #33207, #29653 ),
 .UNSPECIFIED., .F., .F.,
 ( 4, 2, 2, 2, 2, 2, 2, 2, 4 ),
 ( 0.000000000000000000, 0.1250000000000000833, 0.2500000000000001665, 0.3750000000000001665, 0.5000000000000002220, 0.6250000000000002220, 0.7500000000000001110, 0.8750000000000001110, 1.000000000000000000 ),
 .UNSPECIFIED. ) ;
#54282 = CARTESIAN_POINT ( 'NONE',  ( -1.750000000000000000, -23.24999999758999536, -12.50000000000000000 ) ) ;
#54283 = CARTESIAN_POINT ( 'NONE',  ( 1.572508323189017787, -84.21145834493079008, 3.064032359733801503 ) ) ;
#54284 = CARTESIAN_POINT ( 'NONE',  ( 10.03846658012972703, -23.79367507167476248, -7.678639819101482189 ) ) ;
#54285 = CARTESIAN_POINT ( 'NONE',  ( -8.102939992022999860, -78.37599129015498534, -5.403892966383000207 ) ) ;
#54286 = CARTESIAN_POINT ( 'NONE',  ( 12.19230762942000013, -77.48434608859999173, -3.339585897562999950 ) ) ;
#54287 = CARTESIAN_POINT ( 'NONE',  ( 7.128677745341877703, -78.10833333333332007, 6.432089047655188629 ) ) ;
#54288 = CARTESIAN_POINT ( 'NONE',  ( -9.298485322486630622, -61.68812323674685416, 8.385852789354533598 ) ) ;
#54289 = CYLINDRICAL_SURFACE ( 'NONE', #35722, 9.250000000000000000 ) ;
#54290 = ORIENTED_EDGE ( 'NONE', *, *, #6837, .T. ) ;
#54291 = EDGE_CURVE ( 'NONE', #15053, #53225, #46473, .T. ) ;
#54292 = CARTESIAN_POINT ( 'NONE',  ( -0.7186926218484306350, -80.58590376313252079, -1.352462990148321831 ) ) ;
#54293 = CARTESIAN_POINT ( 'NONE',  ( -9.129633152678000130, -79.71611332859899335, -2.714724896223999817 ) ) ;
#54294 = CARTESIAN_POINT ( 'NONE',  ( 7.601397897754999633, -60.04999999725999515, -10.07627163191000008 ) ) ;
#54295 = ADVANCED_FACE ( 'NONE', ( #27134 ), #46350, .F. ) ;
#54296 = CARTESIAN_POINT ( 'NONE',  ( -12.71798280852999952, -55.50221404479999876, -1.931086388455000025 ) ) ;
#54297 = B_SPLINE_CURVE_WITH_KNOTS ( 'NONE', 3,
 ( #1874, #33427, #24872, #47334, #6863, #15433, #56462, #51754 ),
 .UNSPECIFIED., .F., .F.,
 ( 4, 2, 2, 4 ),
 ( 0.000000000000000000, 0.5000000000000046629, 0.7500000000000023315, 1.000000000000000000 ),
 .UNSPECIFIED. ) ;
#54298 = CARTESIAN_POINT ( 'NONE',  ( 9.468749999988999022, -76.98125000001098783, 2.084568677130999610E-09 ) ) ;
#54299 = ORIENTED_EDGE ( 'NONE', *, *, #2316, .F. ) ;
#54300 = CARTESIAN_POINT ( 'NONE',  ( -11.18554731360999988, -77.98760464090999278, 0.7683190734677000089 ) ) ;
#54301 = CARTESIAN_POINT ( 'NONE',  ( 10.25201842922365536, -60.92180395180004382, -7.730408553586130438 ) ) ;
#54302 = ORIENTED_EDGE ( 'NONE', *, *, #45602, .F. ) ;
#54303 = EDGE_LOOP ( 'NONE', ( #33883, #47065, #46916, #28136, #27624, #19089 ) ) ;
#54304 = CARTESIAN_POINT ( 'NONE',  ( -7.660431561264000599, -55.60820826791000115, -10.01749754193999919 ) ) ;
#54305 = PRESENTATION_STYLE_ASSIGNMENT (( #48700 ) ) ;
#54306 = CARTESIAN_POINT ( 'NONE',  ( -9.687172913667000174, -79.84035337108399233, -1.248753675804000096 ) ) ;
#54307 = VERTEX_POINT ( 'NONE', #9440 ) ;
#54308 = CARTESIAN_POINT ( 'NONE',  ( -12.01364710452999951, -77.17245025537799563, 2.874040219260999951 ) ) ;
#54309 = DIRECTION ( 'NONE',  ( 0.000000000000000000, 1.000000000000000000, 0.000000000000000000 ) ) ;
#54310 = CARTESIAN_POINT ( 'NONE',  ( 0.0006082099392775999975, -77.89500416108998593, -1.648286516476999974 ) ) ;
#54311 = EDGE_LOOP ( 'NONE', ( #28281, #22822, #39246 ) ) ;
#54312 = CARTESIAN_POINT ( 'NONE',  ( -2.712012240502000182, -77.46799805011498563, 9.099584490865000319 ) ) ;
#54313 = CARTESIAN_POINT ( 'NONE',  ( 0.2921935631638524211, -80.24396599101683591, -1.216359575293097350 ) ) ;
#54314 = CARTESIAN_POINT ( 'NONE',  ( -10.55245342185999924, -77.53220295299000497, 7.517205849611000801 ) ) ;
#54315 = CARTESIAN_POINT ( 'NONE',  ( 7.374560639698993114, -78.97708333333332575, -9.596002108778149520 ) ) ;
#54316 = B_SPLINE_CURVE_WITH_KNOTS ( 'NONE', 3,
 ( #44998, #53858, #35528, #53557, #8982, #13391, #13096, #54147, #8682, #31684, #49730, #27259, #45298, #4849, #18429, #22845, #40858, #449, #36418, #38955, #33364, #15373, #11814, #38666, #2100, #7375, #24808, #19805, #47563, #6799, #38375, #42531, #56685, #16243, #6211, #38089, #34223, #10954, #20667, #52257, #29789, #7091, #16530, #11531, #15657, #56111, #55820, #25089, #51401, #24518, #15947, #56396, #24226, #42821, #47269, #33652, #2385, #47844, #28935, #51692, #11242, #34509, #46980, #56969, #43113 ),
 .UNSPECIFIED., .F., .F.,
 ( 4, 2, 2, 2, 2, 2, 2, 2, 2, 2, 2, 2, 2, 2, 2, 2, 1, 2, 2, 2, 2, 2, 2, 2, 2, 2, 2, 2, 2, 2, 2, 2, 4 ),
 ( 0.000000000000000000, 0.03125000000000000694, 0.06250000000000001388, 0.09375000000000002776, 0.1250000000000000278, 0.1562500000000000000, 0.1874999999999999722, 0.2187500000000000000, 0.2500000000000000000, 0.2812500000000000000, 0.3125000000000000000, 0.3437500000000000000, 0.3750000000000000000, 0.4062500000000000555, 0.4375000000000000555, 0.4687500000000000555, 0.5000000000000000000, 0.5312500000000000000, 0.5625000000000000000, 0.5937500000000000000, 0.6250000000000000000, 0.6562500000000000000, 0.6875000000000000000, 0.7187500000000000000, 0.7500000000000000000, 0.7812500000000001110, 0.8125000000000001110, 0.8437500000000001110, 0.8750000000000001110, 0.9062500000000001110, 0.9375000000000001110, 0.9687500000000001110, 1.000000000000000000 ),
 .UNSPECIFIED. ) ;
#54317 = CARTESIAN_POINT ( 'NONE',  ( -8.073459667400001649, -78.29680537664623330, -5.384232384047000330 ) ) ;
#54318 = CARTESIAN_POINT ( 'NONE',  ( 5.432842449218323821, -79.92551948836533882, 7.486082547988446301 ) ) ;
#54319 = CARTESIAN_POINT ( 'NONE',  ( 10.41172548051542535, -18.47988211125808178, 7.610718780881719603 ) ) ;
#54320 = VERTEX_POINT ( 'NONE', #27431 ) ;
#54321 = DIRECTION ( 'NONE',  ( 1.000000000000000000, 0.000000000000000000, 0.000000000000000000 ) ) ;
#54322 = CARTESIAN_POINT ( 'NONE',  ( 11.65396969189999865, -75.78284329787000217, -2.860942225950000140 ) ) ;
#54323 = CARTESIAN_POINT ( 'NONE',  ( 1.504745031191999871, -80.09288660730200604, -0.1862378672923999945 ) ) ;
#54324 = TOROIDAL_SURFACE ( 'NONE', #28854, 9.000000000000000000, 0.5000000000000000000 ) ;
#54325 = CARTESIAN_POINT ( 'NONE',  ( -0.9052918118899000444, -78.22287816700719532, -0.9596938812619000281 ) ) ;
#54326 = CARTESIAN_POINT ( 'NONE',  ( 0.3501405267838854085, -3.482218366769342932, -3.504278122193990708 ) ) ;
#54327 = CARTESIAN_POINT ( 'NONE',  ( -8.200000000000001066, -80.99999999999998579, 0.000000000000000000 ) ) ;
#54328 = CARTESIAN_POINT ( 'NONE',  ( 10.82405698390000026, -79.30627921100000322, 5.765268246940999930 ) ) ;
#54329 = CARTESIAN_POINT ( 'NONE',  ( -1.925872869407999843, -76.81415197275400430, -12.12904120624999926 ) ) ;
#54330 = CARTESIAN_POINT ( 'NONE',  ( -5.407950800683633652, -80.45000000000000284, -9.358624512082498015 ) ) ;
#54331 = AXIS2_PLACEMENT_3D ( 'NONE', #31962, #31667, #49714 ) ;
#54332 = CARTESIAN_POINT ( 'NONE',  ( 8.730183855576999719, -77.15846332859899803, -4.061309546832000628 ) ) ;
#54333 = CARTESIAN_POINT ( 'NONE',  ( 10.35453599130000057, -76.75783510652000530, -6.064947188958000446 ) ) ;
#54334 = DIRECTION ( 'NONE',  ( 0.000000000000000000, 1.000000000000000000, 0.000000000000000000 ) ) ;
#54335 = CIRCLE ( 'NONE', #24288, 9.549999999999998934 ) ;
#54336 = ORIENTED_EDGE ( 'NONE', *, *, #39527, .T. ) ;
#54337 = CARTESIAN_POINT ( 'NONE',  ( -1.376471765390000046, -82.48497811192000029, -0.5116381728330999801 ) ) ;
#54338 = DIRECTION ( 'NONE',  ( -1.000000000000000000, 0.000000000000000000, 0.000000000000000000 ) ) ;
#54339 = CARTESIAN_POINT ( 'NONE',  ( 9.073558136264555429, -25.22808769493118319, 8.894842552359547128 ) ) ;
#54340 = CARTESIAN_POINT ( 'NONE',  ( -1.835125225091999823, -77.88555540773499786, 11.83842809849000055 ) ) ;
#54341 = CARTESIAN_POINT ( 'NONE',  ( -0.4877208950597860526, -82.24320891948377721, -1.155849057614090514 ) ) ;
#54342 = CARTESIAN_POINT ( 'NONE',  ( 7.455335830631999450, -78.39789788104899060, 9.319520915745998835 ) ) ;
#54343 = CARTESIAN_POINT ( 'NONE',  ( -7.603664017118000551, -78.51639805011500073, 6.060370778711000384 ) ) ;
#54344 = CARTESIAN_POINT ( 'NONE',  ( -9.737659524074000927, -78.77239977856800124, -0.1941203154314999901 ) ) ;
#54345 = EDGE_CURVE ( 'NONE', #35853, #16460, #32305, .T. ) ;
#54346 = CARTESIAN_POINT ( 'NONE',  ( 4.497237866730260158, -76.04321279041880643, 10.85494175940528372 ) ) ;
#54347 = CARTESIAN_POINT ( 'NONE',  ( -7.210617325615999995, -79.59417565622599966, -8.196484842528999337 ) ) ;
#54348 = CARTESIAN_POINT ( 'NONE',  ( -3.480234241935690864, -85.80681307243298761, 1.471539517285068932 ) ) ;
#54349 = ORIENTED_EDGE ( 'NONE', *, *, #15590, .F. ) ;
#54350 = CARTESIAN_POINT ( 'NONE',  ( 11.88049207238000093, -76.27891845887410227, -3.223263369271999856 ) ) ;
#54351 = ADVANCED_FACE ( 'NONE', ( #2906 ), #15906, .F. ) ;
#54352 = CARTESIAN_POINT ( 'NONE',  ( -3.399395987256420781, -78.70000000000000284, 0.06408526995191715647 ) ) ;
#54353 = CARTESIAN_POINT ( 'NONE',  ( -2.928603948516999900, -78.82664538244598873, 10.57767911662999971 ) ) ;
#54354 = LINE ( 'NONE', #36909, #29809 ) ;
#54355 = CARTESIAN_POINT ( 'NONE',  ( 6.043427764450763462, -77.73333333333330586, 10.48543666025111065 ) ) ;
#54356 = DIRECTION ( 'NONE',  ( 0.000000000000000000, -1.000000000000000000, 0.000000000000000000 ) ) ;
#54357 = CARTESIAN_POINT ( 'NONE',  ( 0.9316830647087891437, -77.94531250006815526, 0.9357750704700737998 ) ) ;
#54358 = EDGE_LOOP ( 'NONE', ( #12817, #49736, #24959, #4103, #46554, #18142 ) ) ;
#54359 = CARTESIAN_POINT ( 'NONE',  ( -6.231249681807000229, -79.69824811525000996, 9.381124237602000093 ) ) ;
#54360 = CARTESIAN_POINT ( 'NONE',  ( 12.70556836343000029, -53.57227722738999631, -1.774194422348999890E-09 ) ) ;
#54361 = CARTESIAN_POINT ( 'NONE',  ( -5.413904038987206846, -79.91666666666665719, 9.393203674808249914 ) ) ;
#54362 = CARTESIAN_POINT ( 'NONE',  ( -3.957349787215346471, -78.48547955770030171, 2.236041248680080251 ) ) ;
#54363 = B_SPLINE_CURVE_WITH_KNOTS ( 'NONE', 3,
 ( #14040, #5193, #27612, #40624, #40325, #22310, #45652, #18197, #8739, #54208 ),
 .UNSPECIFIED., .F., .F.,
 ( 4, 2, 2, 2, 4 ),
 ( 0.000000000000000000, 0.2500000000000000000, 0.5000000000000000000, 0.7500000000000000000, 1.000000000000000000 ),
 .UNSPECIFIED. ) ;
#54364 = EDGE_CURVE ( 'NONE', #55354, #49432, #31563, .T. ) ;
#54365 = CARTESIAN_POINT ( 'NONE',  ( 11.68671316441037789, -76.43942763544110619, -1.473703813607833091 ) ) ;
#54366 = CARTESIAN_POINT ( 'NONE',  ( -9.878709405926999310, -78.84389356166599327, -4.948635581693999974 ) ) ;
#54367 = CARTESIAN_POINT ( 'NONE',  ( 2.251292830498444086, -76.35833333333332007, 10.57172952794451959 ) ) ;
#54368 = CARTESIAN_POINT ( 'NONE',  ( 0.7772663842050028249, -81.51732138592326748, -1.296046382237271200 ) ) ;
#54369 = AXIS2_PLACEMENT_3D ( 'NONE', #58262, #30511, #3376 ) ;
#54370 = CARTESIAN_POINT ( 'NONE',  ( -1.199999995321999968, -75.00000000467838390, -7.200000027511999079 ) ) ;
#54371 = CARTESIAN_POINT ( 'NONE',  ( 4.658475568430798575, -79.83333333333332860, 8.082524092276898386 ) ) ;
#54372 = VECTOR ( 'NONE', #40376, 1000.000000000000114 ) ;
#54373 = CARTESIAN_POINT ( 'NONE',  ( 1.250000000000000000, -76.29999999999999716, -0.6999999999999999556 ) ) ;
#54374 = EDGE_CURVE ( 'NONE', #54392, #14174, #7619, .T. ) ;
#54375 = CARTESIAN_POINT ( 'NONE',  ( -12.54902678210999944, -25.00971938212000012, 0.4616712539286000339 ) ) ;
#54376 = VERTEX_POINT ( 'NONE', #44216 ) ;
#54377 = VECTOR ( 'NONE', #39370, 1000.000000000000114 ) ;
#54378 = ORIENTED_EDGE ( 'NONE', *, *, #35821, .F. ) ;
#54379 = CARTESIAN_POINT ( 'NONE',  ( 10.75000000000000000, -78.85000000000000853, 0.000000000000000000 ) ) ;
#54380 = CARTESIAN_POINT ( 'NONE',  ( -2.787231282280638656, -77.70418860435997033, -10.40622658089639607 ) ) ;
#54381 = CONICAL_SURFACE ( 'NONE', #57190, 9.649999999909001147, 0.7853981633972997312 ) ;
#54382 = ORIENTED_EDGE ( 'NONE', *, *, #51415, .F. ) ;
#54383 = CARTESIAN_POINT ( 'NONE',  ( -1.963210506780999953, -76.36095766513311389, -11.00998129987999974 ) ) ;
#54384 = CARTESIAN_POINT ( 'NONE',  ( 8.284635637485001425, -25.04861451557999885, 9.778492910169999774 ) ) ;
#54385 = CARTESIAN_POINT ( 'NONE',  ( 9.205846894779998735, -61.80798911315000055, 8.541134278117000989 ) ) ;
#54386 = CARTESIAN_POINT ( 'NONE',  ( -1.093189831540567036, -82.55899385228254062, 0.6295831063865356958 ) ) ;
#54387 = CARTESIAN_POINT ( 'NONE',  ( -5.852226986938722675, -78.17054011490029097, -7.163326417538566915 ) ) ;
#54388 = CARTESIAN_POINT ( 'NONE',  ( 11.21665020278000036, -78.51660049291498922, 0.06973997782872000395 ) ) ;
#54389 = CARTESIAN_POINT ( 'NONE',  ( 8.396442233597756655, -79.33930282387936472, 4.561172822325269216 ) ) ;
#54390 = VERTEX_POINT ( 'NONE', #34757 ) ;
#54391 = CARTESIAN_POINT ( 'NONE',  ( -10.27340958483875077, -24.06161210422248331, 7.712164009431025313 ) ) ;
#54392 = VERTEX_POINT ( 'NONE', #57208 ) ;
#54393 = CARTESIAN_POINT ( 'NONE',  ( 1.477687684953830294, -77.46224935051826321, 9.131248644580814755 ) ) ;
#54394 = CARTESIAN_POINT ( 'NONE',  ( -8.283402485401001769, -77.92732575713098697, -7.298588567667000149 ) ) ;
#54395 = CYLINDRICAL_SURFACE ( 'NONE', #17793, 11.05000000000000071 ) ;
#54396 = CARTESIAN_POINT ( 'NONE',  ( -5.681372509047000641, -78.46568311896498926, -7.867192369580999767 ) ) ;
#54397 = CARTESIAN_POINT ( 'NONE',  ( -10.04473064004999827, -75.94998313630999576, 8.446198957084000369 ) ) ;
#54398 = CARTESIAN_POINT ( 'NONE',  ( -12.00000000000000000, -78.39999999999999147, 0.000000000000000000 ) ) ;
#54399 = CARTESIAN_POINT ( 'NONE',  ( 0.4192948356380000186, -79.47715281348000360, -1.440205485619000081 ) ) ;
#54400 = DIRECTION ( 'NONE',  ( 0.000000000000000000, -1.000000000000000000, 0.000000000000000000 ) ) ;
#54401 = CARTESIAN_POINT ( 'NONE',  ( -5.736605348686000028, -78.34811028477999173, 9.315534093342000332 ) ) ;
#54402 = CARTESIAN_POINT ( 'NONE',  ( -10.15323304112999914, -24.23079616014999971, -7.760925857005999795 ) ) ;
#54403 = CARTESIAN_POINT ( 'NONE',  ( 12.71798280857999863, -60.09778595451999905, -1.931086388455000025 ) ) ;
#54404 = CARTESIAN_POINT ( 'NONE',  ( 3.588901577296000234, -82.25792565754399277, -0.05646313095269000354 ) ) ;
#54405 = EDGE_LOOP ( 'NONE', ( #17744, #45746, #41751, #33578 ) ) ;
#54406 = CARTESIAN_POINT ( 'NONE',  ( -5.660024744116999962, -78.92225316430300097, 10.80800494192000016 ) ) ;
#54407 = CARTESIAN_POINT ( 'NONE',  ( -4.602886058546999948, -76.30107567883000286, -10.53195524498000069 ) ) ;
#54408 = CARTESIAN_POINT ( 'NONE',  ( -6.498065648774645986, -78.02678715505997786, 8.565420681610083520 ) ) ;
#54409 = CARTESIAN_POINT ( 'NONE',  ( 11.70594025892000012, -78.40094293021999761, 2.546964289010999583 ) ) ;
#54410 = CARTESIAN_POINT ( 'NONE',  ( -1.250000000000000000, -23.25000000000000000, -12.50000000000000000 ) ) ;
#54411 = AXIS2_PLACEMENT_3D ( 'NONE', #21131, #21426, #16426 ) ;
#54413 = DIRECTION ( 'NONE',  ( 0.000000000000000000, 1.000000000000000000, 0.000000000000000000 ) ) ;
#54412 = LINE ( 'NONE', #9241, #9915 ) ;
#54414 = DIRECTION ( 'NONE',  ( 0.7071067811865475727, 0.000000000000000000, 0.7071067811865475727 ) ) ;
#54415 = CARTESIAN_POINT ( 'NONE',  ( 7.367079209569801002, -80.91505000046390705, 7.831813084430341299 ) ) ;
#54416 = CARTESIAN_POINT ( 'NONE',  ( -10.93228849373000067, -80.63166320050999047, -1.499812449630000044 ) ) ;
#54417 = CARTESIAN_POINT ( 'NONE',  ( 3.451879464910977191, -85.80681307243298761, -1.536875756006051752 ) ) ;
#54418 = CARTESIAN_POINT ( 'NONE',  ( 0.5439554104848000060, -77.02002127708399826, -11.13367472273999859 ) ) ;
#54419 = CARTESIAN_POINT ( 'NONE',  ( -9.596002108778193929, -78.24791666666664014, 7.374560639698935383 ) ) ;
#54420 = CARTESIAN_POINT ( 'NONE',  ( -5.285748055207999840, -80.37364997703009806, 9.676158635172999567 ) ) ;
#54421 = AXIS2_PLACEMENT_3D ( 'NONE', #30333, #58086, #35635 ) ;
#54422 = ORIENTED_EDGE ( 'NONE', *, *, #28885, .F. ) ;
#54423 = CARTESIAN_POINT ( 'NONE',  ( -2.455355393798975605, -77.07239583334455801, 9.133204103152696263 ) ) ;
#54424 = CARTESIAN_POINT ( 'NONE',  ( 2.962511214703000384, -77.80024903538301828, -9.021140561863999707 ) ) ;
#54425 = TOROIDAL_SURFACE ( 'NONE', #14781, 1.250000000000000000, 0.5000000000000000000 ) ;
#54426 = CARTESIAN_POINT ( 'NONE',  ( -10.12290050253000118, -23.24999997822999731, 7.648026768374000639 ) ) ;
#54427 = CARTESIAN_POINT ( 'NONE',  ( 9.668944085725000193, -76.99062003738698934, 5.685915129398999568 ) ) ;
#54428 = VECTOR ( 'NONE', #41437, 1000.000000000000000 ) ;
#54429 = LINE ( 'NONE', #39949, #13037 ) ;
#54430 = CARTESIAN_POINT ( 'NONE',  ( 10.57463602294768812, -77.20000000000000284, 2.242172298085619353 ) ) ;
#54431 = CARTESIAN_POINT ( 'NONE',  ( -10.75000000000000000, -78.50000000000000000, 0.000000000000000000 ) ) ;
#54432 = CARTESIAN_POINT ( 'NONE',  ( 12.43356773666999970, -17.28739071017999862, 0.8411682846947000636 ) ) ;
#54433 = CARTESIAN_POINT ( 'NONE',  ( -3.975696890031999331, -86.15517953870899248, 0.4347074241009999951 ) ) ;
#54434 = DIRECTION ( 'NONE',  ( 0.000000000000000000, 1.000000000000000000, 0.000000000000000000 ) ) ;
#54435 = EDGE_CURVE ( 'NONE', #19148, #4693, #8195, .T. ) ;
#54436 = B_SPLINE_CURVE_WITH_KNOTS ( 'NONE', 3,
 ( #10002, #1157, #41285, #868, #19145, #18854, #298, #54860, #31525, #18571, #10287, #5271, #14695, #9702, #13829, #36268, #53994, #23279, #9120, #40704, #32118, #18277, #27692, #17977, #31827, #5552, #14406, #37140, #35969, #49869 ),
 .UNSPECIFIED., .F., .F.,
 ( 4, 2, 2, 2, 2, 2, 2, 2, 2, 2, 2, 2, 2, 2, 4 ),
 ( 0.000000000000000000, 0.1250000000000045242, 0.1875000000000052458, 0.2500000000000059952, 0.3125000000000067724, 0.3750000000000074940, 0.5000000000000089928, 0.5625000000000097700, 0.6250000000000106581, 0.6875000000000113243, 0.7500000000000119904, 0.8125000000000127676, 0.8437500000000116573, 0.8750000000000105471, 1.000000000000000000 ),
 .UNSPECIFIED. ) ;
#54437 = CARTESIAN_POINT ( 'NONE',  ( 9.770419344647999438, -53.74469452534000169, -8.292776877908002220 ) ) ;
#54438 = CARTESIAN_POINT ( 'NONE',  ( 7.461283454533999659, -76.89222102750099452, -8.281536679888001018 ) ) ;
#54439 = CARTESIAN_POINT ( 'NONE',  ( -1.445929428138999828, -80.16981638657999554, 0.8273736140038000508 ) ) ;
#54440 = CARTESIAN_POINT ( 'NONE',  ( -0.9076773815622000141, -79.31816002803999766, 1.255319232249999972 ) ) ;
#54441 = CARTESIAN_POINT ( 'NONE',  ( -3.831287612370999796, -76.98242073713129230, -8.693171758988999187 ) ) ;
#54442 = CARTESIAN_POINT ( 'NONE',  ( -1.372670850766613659, -82.78440322194356327, -0.6347619962463861842 ) ) ;
#54443 = CARTESIAN_POINT ( 'NONE',  ( -12.43356840166999788, -61.51269674456000303, 0.8410229959425999935 ) ) ;
#54444 = DIRECTION ( 'NONE',  ( 0.000000000000000000, 0.000000000000000000, -1.000000000000000000 ) ) ;
#54445 = CARTESIAN_POINT ( 'NONE',  ( 10.75000000000000000, -77.25000000000000000, 0.000000000000000000 ) ) ;
#54446 = CARTESIAN_POINT ( 'NONE',  ( 8.645788266876911266, -78.65487569970177617, 7.146464437358057253 ) ) ;
#54447 = CARTESIAN_POINT ( 'NONE',  ( 1.226805910823643986, -81.83485757964179186, -0.2432299854603273970 ) ) ;
#54448 = PLANE ( 'NONE',  #41619 ) ;
#54449 = EDGE_CURVE ( 'NONE', #20659, #37664, #52783, .T. ) ;
#54450 = CARTESIAN_POINT ( 'NONE',  ( -2.830810333559000025, -78.99570369636998635, -10.78151721355999904 ) ) ;
#54451 = CARTESIAN_POINT ( 'NONE',  ( 7.997114030194825141, -55.11418618782499124, 7.553727747540665227 ) ) ;
#54452 = ORIENTED_EDGE ( 'NONE', *, *, #25141, .T. ) ;
#54453 = EDGE_LOOP ( 'NONE', ( #42407, #10752, #46202, #4918, #28505, #4341, #3807, #25608, #33851, #27480, #17921, #8104 ) ) ;
#54454 = CARTESIAN_POINT ( 'NONE',  ( -0.7881893378370999903, -81.40752335986800858, 1.409245008412000066 ) ) ;
#54455 = ORIENTED_EDGE ( 'NONE', *, *, #39188, .F. ) ;
#54456 = VECTOR ( 'NONE', #45548, 1000.000000000000000 ) ;
#54457 = ORIENTED_EDGE ( 'NONE', *, *, #52837, .F. ) ;
#54458 = CARTESIAN_POINT ( 'NONE',  ( -2.065550207748000133, -18.57434920668999823, 12.82162303854000029 ) ) ;
#54459 = CARTESIAN_POINT ( 'NONE',  ( -1.500000000000000000, -77.89999999999999147, 0.000000000000000000 ) ) ;
#54460 = CARTESIAN_POINT ( 'NONE',  ( -1.373083971518393565, -81.97604165108509733, -3.122541964024958094 ) ) ;
#54461 = CARTESIAN_POINT ( 'NONE',  ( 0.5154756746315999338, -25.13240599763000205, -12.66205448072999928 ) ) ;
#54462 = CARTESIAN_POINT ( 'NONE',  ( 3.582810207382000289, -82.77871570665098488, 0.3614056475548999559 ) ) ;
#54463 = CARTESIAN_POINT ( 'NONE',  ( -10.75000000000000000, -78.01041666666665719, -1.407171709420429018 ) ) ;
#54464 = CARTESIAN_POINT ( 'NONE',  ( -11.06142172674999991, -78.77465814038001213, -4.424517025895999822 ) ) ;
#54465 = VERTEX_POINT ( 'NONE', #3764 ) ;
#54466 = VERTEX_POINT ( 'NONE', #44798 ) ;
#54467 = CARTESIAN_POINT ( 'NONE',  ( 12.50000000000000000, -39.49523982883999906, 0.000000000000000000 ) ) ;
#54468 = CARTESIAN_POINT ( 'NONE',  ( -0.6295237254636286695, -81.41666666666667140, 1.092232985442819881 ) ) ;
#54469 = CIRCLE ( 'NONE', #28864, 14.00000000000000000 ) ;
#54470 = ADVANCED_FACE ( 'NONE', ( #8779 ), #17637, .F. ) ;
#54471 = CARTESIAN_POINT ( 'NONE',  ( -0.2976639488673999967, -79.65857342613799119, 1.299989344602000108 ) ) ;
#54472 = CARTESIAN_POINT ( 'NONE',  ( -1.182190922889000184, -78.82482709540299481, -9.631881180458998770 ) ) ;
#54473 = AXIS2_PLACEMENT_3D ( 'NONE', #40105, #13536, #3240 ) ;
#54474 = CARTESIAN_POINT ( 'NONE',  ( 3.654181830570633949, -86.09999999999978115, -1.626946572303283656 ) ) ;
#54475 = CARTESIAN_POINT ( 'NONE',  ( -2.381013104730116403, -86.03776559246422551, 3.227344833870573915 ) ) ;
#54476 = CARTESIAN_POINT ( 'NONE',  ( -1.258617752331000039, -77.53579772561000993, -12.89490358089000033 ) ) ;
#54477 = CARTESIAN_POINT ( 'NONE',  ( 1.399788002916999785, -80.41777860354999063, 0.4438937798904999954 ) ) ;
#54478 = CARTESIAN_POINT ( 'NONE',  ( -12.60413652831999975, -23.30716934606000024, -1.799502287743000029 ) ) ;
#54479 = FACE_OUTER_BOUND ( 'NONE', #1528, .T. ) ;
#54480 = CARTESIAN_POINT ( 'NONE',  ( -1.152093420842999816, -81.44824379153999416, 4.012765998397000544 ) ) ;
#54481 = CARTESIAN_POINT ( 'NONE',  ( -10.34138800174999950, -80.80143906952710608, 4.468208825537999473 ) ) ;
#54482 = CARTESIAN_POINT ( 'NONE',  ( -9.676327351641999641, -79.01948667140098337, -1.545051445613999874 ) ) ;
#54483 = CARTESIAN_POINT ( 'NONE',  ( -11.61175053437844262, -78.28594503550665706, 2.075198828568656673 ) ) ;
#54484 = CARTESIAN_POINT ( 'NONE',  ( -1.757625406357000042, -79.96757046129098967, 3.081445367595999407 ) ) ;
#54485 = CARTESIAN_POINT ( 'NONE',  ( -1.309352690804000074, -78.23709502082350298, -0.2533212985548999874 ) ) ;
#54486 = CARTESIAN_POINT ( 'NONE',  ( 0.000000000000000000, -86.09999999999999432, 0.000000000000000000 ) ) ;
#54487 = CARTESIAN_POINT ( 'NONE',  ( 5.620590082324000036, -80.56825076276699349, -9.763102121971000358 ) ) ;
#54488 = CARTESIAN_POINT ( 'NONE',  ( -3.448863046786000197, -1.852077464339999979, -1.608907009436000068 ) ) ;
#54489 = CARTESIAN_POINT ( 'NONE',  ( 7.177850223112891115, -77.20000000000000284, -8.156503725454280485 ) ) ;
#54490 = ORIENTED_EDGE ( 'NONE', *, *, #19452, .F. ) ;
#54491 = CARTESIAN_POINT ( 'NONE',  ( -0.5245219981451909597, -23.45160423345543421, 10.98753021428638554 ) ) ;
#54492 = CARTESIAN_POINT ( 'NONE',  ( 8.178338515874511216, -60.10416868444934835, -7.356278612544663531 ) ) ;
#54493 = CARTESIAN_POINT ( 'NONE',  ( 6.760013919724077169, -79.37708333333333144, -8.796335266379971429 ) ) ;
#54494 = CARTESIAN_POINT ( 'NONE',  ( 0.8962411872155999770, -81.58201667106600041, 0.9875868993909000526 ) ) ;
#54495 = CARTESIAN_POINT ( 'NONE',  ( 2.062597299672999540, -56.01514526721999943, 12.87022657272000004 ) ) ;
#54496 = CARTESIAN_POINT ( 'NONE',  ( 5.579996517577999526, -77.32240076259999739, 11.75597208960999929 ) ) ;
#54497 = CARTESIAN_POINT ( 'NONE',  ( -2.598793908247287732, -79.49442965258924687, 10.43132793576024220 ) ) ;
#54498 = CARTESIAN_POINT ( 'NONE',  ( -9.841120606655673342, -61.63627250027259663, -8.121699444612119123 ) ) ;
#54499 = CARTESIAN_POINT ( 'NONE',  ( 0.7942261439060999129, -76.36432412444001727, 12.48713564821000155 ) ) ;
#54500 = ORIENTED_EDGE ( 'NONE', *, *, #53159, .T. ) ;
#54501 = EDGE_CURVE ( 'NONE', #30023, #44757, #53435, .T. ) ;
#54502 = CARTESIAN_POINT ( 'NONE',  ( -11.17232872905999841, -77.66848448279598927, 1.511624848520999764 ) ) ;
#54503 = AXIS2_PLACEMENT_3D ( 'NONE', #14492, #19227, #953 ) ;
#54504 = EDGE_CURVE ( 'NONE', #28795, #10827, #22351, .T. ) ;
#54505 = B_SPLINE_CURVE_WITH_KNOTS ( 'NONE', 3,
 ( #17884, #21999, #5176, #36749, #32303, #22295, #40006, #8426, #58022, #58321 ),
 .UNSPECIFIED., .F., .F.,
 ( 4, 2, 2, 2, 4 ),
 ( 0.000000000000000000, 0.2499999999999998335, 0.4999999999999998890, 0.7499999999999998890, 1.000000000000000000 ),
 .UNSPECIFIED. ) ;
#54506 = CARTESIAN_POINT ( 'NONE',  ( -1.183389931723999977, -81.70658373923900797, 0.5633908112155999737 ) ) ;
#54507 = CARTESIAN_POINT ( 'NONE',  ( 7.691916945395000482, -21.75365779208000205, -10.42274798264000069 ) ) ;
#54508 = CARTESIAN_POINT ( 'NONE',  ( -7.233356275331999541, -78.96555212030999371, 6.024097567370000128 ) ) ;
#54510 = CARTESIAN_POINT ( 'NONE',  ( 2.028166799595999770, -0.9497943542025000241, -3.466423845304999585 ) ) ;
#54509 = CARTESIAN_POINT ( 'NONE',  ( 3.997213461646000443, -83.70093064074599454, -1.039614356706999976 ) ) ;
#54511 = CARTESIAN_POINT ( 'NONE',  ( -12.56594317823000040, -23.25000001387000026, 1.750000000000000000 ) ) ;
#54512 = DIRECTION ( 'NONE',  ( 0.000000000000000000, -1.000000000000000000, 0.000000000000000000 ) ) ;
#54513 = ORIENTED_EDGE ( 'NONE', *, *, #1839, .F. ) ;
#54514 = CARTESIAN_POINT ( 'NONE',  ( -4.625569715417624295, -77.18961895380674321, -9.703952514631545512 ) ) ;
#54515 = CARTESIAN_POINT ( 'NONE',  ( 11.87139580924463012, -79.06341727770498551, 2.023209039049198577 ) ) ;
#54516 = CARTESIAN_POINT ( 'NONE',  ( 3.962812355711000212, -78.85171438276199751, -4.853045467043058701E-16 ) ) ;
#54517 = EDGE_LOOP ( 'NONE', ( #33945, #55828, #21612, #3330, #45537 ) ) ;
#54518 = ORIENTED_EDGE ( 'NONE', *, *, #7335, .F. ) ;
#54519 = DIRECTION ( 'NONE',  ( 0.000000000000000000, 0.000000000000000000, -1.000000000000000000 ) ) ;
#54520 = LINE ( 'NONE', #36492, #34937 ) ;
#54521 = EDGE_CURVE ( 'NONE', #4702, #26583, #27460, .T. ) ;
#54522 = DIRECTION ( 'NONE',  ( 0.000000000000000000, 1.000000000000000000, 0.000000000000000000 ) ) ;
#54523 = ORIENTED_EDGE ( 'NONE', *, *, #26958, .T. ) ;
#54524 = CARTESIAN_POINT ( 'NONE',  ( 10.48586718643000104, -77.40014181984899722, -5.936521791247999502 ) ) ;
#54525 = ORIENTED_EDGE ( 'NONE', *, *, #33780, .F. ) ;
#54526 = EDGE_LOOP ( 'NONE', ( #8397, #35379, #36074, #33218 ) ) ;
#54527 = CARTESIAN_POINT ( 'NONE',  ( -2.805383591734468052, -2.643477393492342120, -1.642515783888874870 ) ) ;
#54528 = CARTESIAN_POINT ( 'NONE',  ( 1.570796326794857478, -78.66458333333331154, 12.00000000000000533 ) ) ;
#54529 = LINE ( 'NONE', #37080, #28908 ) ;
#54530 = B_SPLINE_SURFACE_WITH_KNOTS ( 'NONE', 3, 3, ( 
 ( #4519, #53822, #27517, #31650 ),
 ( #18101, #13358, #22521, #23103 ),
 ( #40530, #36097, #54693, #14236 ),
 ( #32234, #49693, #50276, #9824 ),
 ( #41407, #36966, #14528, #11575 ),
 ( #29265, #6257, #19266, #2142 ),
 ( #15997, #11286, #47313, #46737 ),
 ( #33984, #52021, #37844, #29555 ),
 ( #33111, #28982, #47610, #37547 ),
 ( #56154, #1855, #28391, #6553 ),
 ( #6842, #51153, #24271, #7134 ),
 ( #10407, #24853, #42288, #55565 ),
 ( #33697, #20429, #19850, #1558 ),
 ( #42869, #10708, #23971, #41696 ),
 ( #2426, #15415, #38423, #56442 ),
 ( #1273, #38131, #19549, #51737 ),
 ( #37257, #15113, #55864, #55269 ) ),
 .UNSPECIFIED., .F., .F., .F.,
 ( 4, 1, 1, 1, 1, 1, 1, 1, 1, 1, 1, 1, 1, 1, 4 ),
 ( 4, 4 ),
 ( -0.01011398171662000051, 0.000000000000000000, 0.08333333333333001192, 0.1666666666667000196, 0.2500000000000000000, 0.3333333333333000081, 0.4166666666666999919, 0.5000000000000000000, 0.5833333333333000637, 0.6666666666667000474, 0.7500000000000000000, 0.8333333333333000637, 0.9166666666667000474, 1.000000000000000000, 1.010365777941000021 ),
 ( -0.3559705546970999834, 1.357612346730000086 ),
 .UNSPECIFIED. ) ;
#54531 = EDGE_LOOP ( 'NONE', ( #38535, #21037, #49888, #45444 ) ) ;
#54532 = CARTESIAN_POINT ( 'NONE',  ( 1.165652817183006063, -82.82060152807378017, -0.4515180940258363695 ) ) ;
#54533 = VERTEX_POINT ( 'NONE', #44499 ) ;
#54534 = CARTESIAN_POINT ( 'NONE',  ( 2.322889840689335017, -78.69999999999998863, -4.022071228304438861 ) ) ;
#54535 = DIRECTION ( 'NONE',  ( 1.000000000000000000, 0.000000000000000000, 0.000000000000000000 ) ) ;
#54536 = VECTOR ( 'NONE', #29706, 1000.000000000000000 ) ;
#54537 = CARTESIAN_POINT ( 'NONE',  ( -10.85772169724999969, -76.75329282578898926, 1.763485056683000041 ) ) ;
#54538 = CARTESIAN_POINT ( 'NONE',  ( 0.5999999999999999778, -23.15000000000000213, 10.98362417419999915 ) ) ;
#54539 = DIRECTION ( 'NONE',  ( 0.000000000000000000, 0.000000000000000000, -1.000000000000000000 ) ) ;
#54540 = CARTESIAN_POINT ( 'NONE',  ( 7.640030139739999449, -55.49283065365000311, -10.18491068058999893 ) ) ;
#54541 = CARTESIAN_POINT ( 'NONE',  ( 7.984248283110355615, -78.80795658438964324, -4.671396296726914699 ) ) ;
#54542 = CARTESIAN_POINT ( 'NONE',  ( 1.980584515756000030, -18.73514849905999924, -12.76303204340999997 ) ) ;
#54543 = CARTESIAN_POINT ( 'NONE',  ( 0.000000000000000000, -39.49523982883999906, 0.000000000000000000 ) ) ;
#54544 = CARTESIAN_POINT ( 'NONE',  ( 0.000000000000000000, 0.000000000000000000, 0.000000000000000000 ) ) ;
#54545 = CARTESIAN_POINT ( 'NONE',  ( -9.683190293175545804, -78.00399549952769007, -7.215732957028438754 ) ) ;
#54546 = CARTESIAN_POINT ( 'NONE',  ( -3.867633442252000009, -81.44778455456800259, -0.8645186538081999217 ) ) ;
#54547 = EDGE_CURVE ( 'NONE', #36325, #40498, #1397, .T. ) ;
#54548 = CARTESIAN_POINT ( 'NONE',  ( -12.61117324689999997, -18.78448536116999890, 1.798979683802999885 ) ) ;
#54549 = CIRCLE ( 'NONE', #42291, 14.00000000000000000 ) ;
#54550 = DIRECTION ( 'NONE',  ( -0.7071067811864980568, -0.7071067811865969777, 1.752039988203994887E-09 ) ) ;
#54551 = CARTESIAN_POINT ( 'NONE',  ( -1.200170490671999879, -24.43405701997999913, 12.43444080551000042 ) ) ;
#54552 = CARTESIAN_POINT ( 'NONE',  ( -1.310962691340256780, -81.76182832648821375, -0.1935753109423370699 ) ) ;
#54553 = CARTESIAN_POINT ( 'NONE',  ( 9.489577027016325772, -79.99999999999998579, 0.7465672904055182801 ) ) ;
#54554 = CARTESIAN_POINT ( 'NONE',  ( -3.412382586387999961, -1.979717402877999799, -0.5131178166667998974 ) ) ;
#54555 = CARTESIAN_POINT ( 'NONE',  ( -1.087669557110363838, -82.13271128940070298, -0.8608145078121063332 ) ) ;
#54556 = DIRECTION ( 'NONE',  ( 0.000000000000000000, 0.000000000000000000, 1.000000000000000000 ) ) ;
#54557 = CARTESIAN_POINT ( 'NONE',  ( 12.70255466319078685, -24.74616562078519522, -1.306323829448696516 ) ) ;
#54558 = CARTESIAN_POINT ( 'NONE',  ( -1.758095523367999791, -23.72291663880000101, -12.57362173515999970 ) ) ;
#54559 = CARTESIAN_POINT ( 'NONE',  ( -0.01370464116672059050, -78.47610054924975032, 1.249783674205719786 ) ) ;
#54560 = CARTESIAN_POINT ( 'NONE',  ( 7.686918321215999939, -57.04439829094999936, -10.48771805383000100 ) ) ;
#54561 = CARTESIAN_POINT ( 'NONE',  ( -2.744117082525000306, -2.991506412944000104, 2.149193971933000213 ) ) ;
#54562 = DIRECTION ( 'NONE',  ( 0.000000000000000000, -1.000000000000000000, 0.000000000000000000 ) ) ;
#54563 = PRODUCT_DEFINITION_SHAPE ( 'NONE', 'NONE',  #58414 ) ;
#54564 = CARTESIAN_POINT ( 'NONE',  ( -12.22643784615999962, -77.38083722509800566, -1.144550905343000080 ) ) ;
#54565 = FACE_OUTER_BOUND ( 'NONE', #598, .T. ) ;
#54567 = CARTESIAN_POINT ( 'NONE',  ( -0.9855275769405000830, -77.92138024546849806, -1.152289182367999931 ) ) ;
#54566 = LINE ( 'NONE', #36831, #1530 ) ;
#54568 = CARTESIAN_POINT ( 'NONE',  ( -1.308644393797000038, -81.24548374185999933, -0.6845726736234999388 ) ) ;
#54569 = EDGE_LOOP ( 'NONE', ( #31447, #52126, #34034 ) ) ;
#54570 = CARTESIAN_POINT ( 'NONE',  ( 3.161565914092999918, -85.52057450217398582, -1.699481856679999847 ) ) ;
#54571 = CARTESIAN_POINT ( 'NONE',  ( 6.273262642061999905, -80.40039539424418535, 9.103776903494001260 ) ) ;
#54572 = ADVANCED_FACE ( 'NONE', ( #39137 ), #52724, .F. ) ;
#54573 = CARTESIAN_POINT ( 'NONE',  ( 1.028703311283999754E-14, 0.000000000000000000, 0.000000000000000000 ) ) ;
#54574 = CARTESIAN_POINT ( 'NONE',  ( 1.017700374863836688, -85.75312500679751793, 3.277910159453279348 ) ) ;
#54575 = CARTESIAN_POINT ( 'NONE',  ( 9.869466656387999137, -77.04448811493399774, -5.330266269891000164 ) ) ;
#54576 = CARTESIAN_POINT ( 'NONE',  ( 10.20942848027640792, -76.56032164449479183, -5.979968601052592092 ) ) ;
#54577 = DIRECTION ( 'NONE',  ( 0.000000000000000000, -1.000000000000000000, 1.998401444324999992E-14 ) ) ;
#54578 = CARTESIAN_POINT ( 'NONE',  ( 0.009013724458761000410, -1.180443126209999916, 4.026554455433999813 ) ) ;
#54579 = CARTESIAN_POINT ( 'NONE',  ( 7.811513588403999897, -79.07336703774899433, 6.067673790570999870 ) ) ;
#54580 = CARTESIAN_POINT ( 'NONE',  ( 5.522795323340943696, -76.07083333333035569, 9.558450660443439162 ) ) ;
#54581 = VERTEX_POINT ( 'NONE', #39431 ) ;
#54582 = DIRECTION ( 'NONE',  ( -1.000000000000000000, 0.000000000000000000, 0.000000000000000000 ) ) ;
#54583 = CARTESIAN_POINT ( 'NONE',  ( -9.025535990598001490, -79.65233998579800812, -2.683771280366999523 ) ) ;
#54584 = DIRECTION ( 'NONE',  ( 0.000000000000000000, -1.000000000000000000, 0.000000000000000000 ) ) ;
#54585 = CARTESIAN_POINT ( 'NONE',  ( 0.3926218265389221362, -81.54583333333334849, -1.460959015002473160 ) ) ;
#54586 = CARTESIAN_POINT ( 'NONE',  ( -12.80900240956999880, -57.04634220890999785, -1.930989144707000005 ) ) ;
#54587 = EDGE_CURVE ( 'NONE', #51909, #17562, #22492, .T. ) ;
#54588 = CARTESIAN_POINT ( 'NONE',  ( 10.99999999999999645, -23.74999999999999289, 0.1603812274922369330 ) ) ;
#54589 = ORIENTED_EDGE ( 'NONE', *, *, #22079, .T. ) ;
#54590 = CARTESIAN_POINT ( 'NONE',  ( -2.062503053667999797, -21.75736537952000305, 12.92177931904999966 ) ) ;
#54591 = ADVANCED_FACE ( 'NONE', ( #2845 ), #36906, .T. ) ;
#54592 = ORIENTED_EDGE ( 'NONE', *, *, #47173, .T. ) ;
#54593 = VERTEX_POINT ( 'NONE', #26137 ) ;
#54594 = DIRECTION ( 'NONE',  ( 0.7071067811865475727, 0.000000000000000000, 0.7071067811865475727 ) ) ;
#54595 =( NAMED_UNIT ( * ) SI_UNIT ( $, .STERADIAN. ) SOLID_ANGLE_UNIT ( ) );
#54596 = CARTESIAN_POINT ( 'NONE',  ( 3.269429986698999979, -79.85814584891350876, 9.203886808668999109 ) ) ;
#54597 = VERTEX_POINT ( 'NONE', #11997 ) ;
#54598 = CARTESIAN_POINT ( 'NONE',  ( 12.72554264789000023, -55.59839278072999491, 1.930240062458999928 ) ) ;
#54599 = CARTESIAN_POINT ( 'NONE',  ( 9.848022987176388909, -24.82869493595770649, -8.114799025119214804 ) ) ;
#54600 = CARTESIAN_POINT ( 'NONE',  ( -0.07808091635396000041, -78.89120398689999547, -1.646447584893999894 ) ) ;
#54601 = ORIENTED_EDGE ( 'NONE', *, *, #42905, .T. ) ;
#54602 = CARTESIAN_POINT ( 'NONE',  ( -7.591316436381999821, -77.12122305011499179, -5.703451837412999659 ) ) ;
#54603 = PRODUCT_DEFINITION ( 'UNKNOWN', '', #9353, #16836 ) ;
#54604 = CARTESIAN_POINT ( 'NONE',  ( -1.039294407854003843, -80.14744977795547243, -0.6948369225764182699 ) ) ;
#54605 = CARTESIAN_POINT ( 'NONE',  ( 7.255994938323000021, -78.25376328549999982, -10.73374472359000009 ) ) ;
#54606 = CARTESIAN_POINT ( 'NONE',  ( 0.000000000000000000, -86.29999999996098836, -10.04999999996000071 ) ) ;
#54607 = CARTESIAN_POINT ( 'NONE',  ( 8.240801834864576847, -79.88798849990462259, 4.200746768372105144 ) ) ;
#54608 = CARTESIAN_POINT ( 'NONE',  ( 2.551980763918843653, -79.23958331830202440, -3.097208638987810403 ) ) ;
#54609 = VERTEX_POINT ( 'NONE', #44158 ) ;
#54610 = CARTESIAN_POINT ( 'NONE',  ( 5.838193839761673054, -77.62291666666669698, 7.596835002782728274 ) ) ;
#54611 = CARTESIAN_POINT ( 'NONE',  ( 3.295079792876999925, -76.37076945043999388, 11.86077433336000020 ) ) ;
#54612 = CARTESIAN_POINT ( 'NONE',  ( -0.7062052416310000691, -80.93630120477999412, -1.233256579520999763 ) ) ;
#54613 = ADVANCED_FACE ( 'NONE', ( #57148 ), #3904, .T. ) ;
#54614 = CARTESIAN_POINT ( 'NONE',  ( -3.428559295506383275, -2.331211582835436946, 0.7930039989315531557 ) ) ;
#54615 = AXIS2_PLACEMENT_3D ( 'NONE', #3411, #30256, #43566 ) ;
#54616 = CARTESIAN_POINT ( 'NONE',  ( 8.194866293469999619, -61.51043252617999713, -9.389192598819999347 ) ) ;
#54617 = CARTESIAN_POINT ( 'NONE',  ( 7.914613980750001332, -79.33501992907000044, 9.019916049260999102 ) ) ;
#54618 = CARTESIAN_POINT ( 'NONE',  ( -1.750000000001000089, -18.74999999009000007, 12.56594317857000043 ) ) ;
#54619 = CARTESIAN_POINT ( 'NONE',  ( 12.70610308058891569, -17.54479009143859969, -1.580620443400405861 ) ) ;
#54620 = ADVANCED_FACE ( 'NONE', ( #25846 ), #35267, .F. ) ;
#54621 = CARTESIAN_POINT ( 'NONE',  ( 6.722579162784999340, -79.88047948297999312, 8.904972230874999894 ) ) ;
#54622 = CARTESIAN_POINT ( 'NONE',  ( 9.705941689622999746, -77.12296498579800641, -0.7792165775660999660 ) ) ;
#54623 = DIRECTION ( 'NONE',  ( -0.7071067811865475727, 0.000000000000000000, -0.7071067811865475727 ) ) ;
#54624 = CARTESIAN_POINT ( 'NONE',  ( 6.586108526242999694, -80.07391735373440156, 8.810401493720998900 ) ) ;
#54625 = ORIENTED_EDGE ( 'NONE', *, *, #3254, .T. ) ;
#54626 = CARTESIAN_POINT ( 'NONE',  ( -0.4497554808884999811, -82.42197637046800196, 1.274241432965000032 ) ) ;
#54627 = CARTESIAN_POINT ( 'NONE',  ( 1.100531998921000065, -79.72070532422000610, -0.7842560430284000184 ) ) ;
#54628 = CARTESIAN_POINT ( 'NONE',  ( 9.689272046653734094, -24.97888144173617775, 8.274769670417640555 ) ) ;
#54629 = CARTESIAN_POINT ( 'NONE',  ( 7.919842512018000491, -77.31583978383599742, 8.988445846368000147 ) ) ;
#54630 = CARTESIAN_POINT ( 'NONE',  ( -0.5849236359613864122, -82.23641784656102516, -1.109830192218287825 ) ) ;
#54631 = CARTESIAN_POINT ( 'NONE',  ( 0.7076411874954000591, -82.93030375670298326, -1.508144869335000138 ) ) ;
#54632 = VECTOR ( 'NONE', #8481, 1000.000000000000000 ) ;
#54633 = CARTESIAN_POINT ( 'NONE',  ( -4.109499447189000065, -78.41155876290798687, 11.32730267836999971 ) ) ;
#54634 = CARTESIAN_POINT ( 'NONE',  ( 8.381176496771999496, -77.99792830956099010, 4.744374615790000860 ) ) ;
#54635 = CARTESIAN_POINT ( 'NONE',  ( 2.306676788976210979, -76.05906975059716046, 11.52121794999999871 ) ) ;
#54636 = CARTESIAN_POINT ( 'NONE',  ( 10.35105862822000056, -80.30232057427369341, 3.468557695829999954 ) ) ;
#54637 = CARTESIAN_POINT ( 'NONE',  ( -3.138103972814559217, -86.02148120184399716, 1.326877354891812244 ) ) ;
#54638 = ORIENTED_EDGE ( 'NONE', *, *, #2858, .T. ) ;
#54639 = CARTESIAN_POINT ( 'NONE',  ( -1.476182556143999403, -76.43456666368409458, 12.22114576030999800 ) ) ;
#54640 = CARTESIAN_POINT ( 'NONE',  ( 2.194290298650410698, -78.40681307243319509, -3.799401814995372995 ) ) ;
#54641 = CARTESIAN_POINT ( 'NONE',  ( -10.79326785783000098, -79.50498010343598310, -1.992331681952000055 ) ) ;
#54642 = DIRECTION ( 'NONE',  ( 1.000000000000000000, 0.000000000000000000, 0.000000000000000000 ) ) ;
#54643 = CARTESIAN_POINT ( 'NONE',  ( -7.845158543477998236, -76.94443866757499961, -9.736889158655001708 ) ) ;
#54644 = CARTESIAN_POINT ( 'NONE',  ( -12.00000000000000000, -55.54999999966999980, 1.250000000000000000 ) ) ;
#54645 = CARTESIAN_POINT ( 'NONE',  ( 10.36221646773000060, -18.77876216379999974, -7.631895822745999425 ) ) ;
#54646 = CARTESIAN_POINT ( 'NONE',  ( 9.546815224142999767, -17.31472046677999899, 8.130854305520999858 ) ) ;
#54647 = ORIENTED_EDGE ( 'NONE', *, *, #21295, .T. ) ;
#54648 = CARTESIAN_POINT ( 'NONE',  ( 10.52346617262000095, -78.43212195875699422, -3.675769182893000142 ) ) ;
#54649 = CARTESIAN_POINT ( 'NONE',  ( 12.71107039382469850, -17.74871969254651205, 1.717622521802969704 ) ) ;
#54650 = CARTESIAN_POINT ( 'NONE',  ( 6.724037440004856592, -79.72330751359039880, -9.661915242757062927 ) ) ;
#54651 = CARTESIAN_POINT ( 'NONE',  ( -1.179862061259663086, -81.57352980150935196, 0.4123850943632001442 ) ) ;
#54652 = ADVANCED_FACE ( 'NONE', ( #13722 ), #53895, .F. ) ;
#54653 = CARTESIAN_POINT ( 'NONE',  ( -4.681555824253774922, -76.99999999999998579, -8.244243791166322666 ) ) ;
#54654 = CARTESIAN_POINT ( 'NONE',  ( -1.750000000000000000, -18.75000000000000000, 12.00000000000000000 ) ) ;
#54655 = EDGE_CURVE ( 'NONE', #21736, #37515, #4882, .T. ) ;
#54656 = FACE_OUTER_BOUND ( 'NONE', #40717, .T. ) ;
#54657 = CARTESIAN_POINT ( 'NONE',  ( 0.000000000000000000, -26.10094976978000147, 0.000000000000000000 ) ) ;
#54658 = CARTESIAN_POINT ( 'NONE',  ( 5.330257171412455364, -78.28474862486109487, 9.594590749055214474 ) ) ;
#54659 = CARTESIAN_POINT ( 'NONE',  ( -3.781264912327570116, -79.74479166666647245, -8.502894493265863218 ) ) ;
#54660 = ORIENTED_EDGE ( 'NONE', *, *, #38891, .T. ) ;
#54661 = VERTEX_POINT ( 'NONE', #14301 ) ;
#54662 = CARTESIAN_POINT ( 'NONE',  ( 9.800312463269442276, -78.81625363457253286, -4.431906745122180524 ) ) ;
#54663 = VERTEX_POINT ( 'NONE', #480 ) ;
#54664 = FACE_OUTER_BOUND ( 'NONE', #18841, .T. ) ;
#54665 = CARTESIAN_POINT ( 'NONE',  ( 9.310177428684999867, -25.13531023636999961, 8.596745825432000387 ) ) ;
#54666 = CIRCLE ( 'NONE', #24492, 11.05000000000000071 ) ;
#54667 = ADVANCED_FACE ( 'NONE', ( #5169 ), #18747, .F. ) ;
#54668 = CARTESIAN_POINT ( 'NONE',  ( 9.516272955320999927, -61.62538765589000178, 8.227498559456998706 ) ) ;
#54669 = CARTESIAN_POINT ( 'NONE',  ( 7.624341764923000753, -18.73514850530999709, 10.42531124853000080 ) ) ;
#54670 = CARTESIAN_POINT ( 'NONE',  ( 6.233047529871999615, -78.88050366622999832, 9.960502923565000444 ) ) ;
#54671 = CARTESIAN_POINT ( 'NONE',  ( -0.2721098858049000313, -79.14303638195599433, 11.21356619464000026 ) ) ;
#54672 = CARTESIAN_POINT ( 'NONE',  ( -2.527424140845015543, -80.99999999999998579, 10.49288982607049192 ) ) ;
#54673 = ORIENTED_EDGE ( 'NONE', *, *, #23149, .F. ) ;
#54674 = CARTESIAN_POINT ( 'NONE',  ( -0.5999999999999999778, -5.200000000000000178, -4.000000000000000000 ) ) ;
#54675 = ORIENTED_EDGE ( 'NONE', *, *, #6993, .F. ) ;
#54676 = CARTESIAN_POINT ( 'NONE',  ( -0.01106553558703762298, -77.47524953867433339, 9.249901033550106177 ) ) ;
#54677 = CARTESIAN_POINT ( 'NONE',  ( 10.71768947918000059, -78.10758077290198287, -1.656903943290000125 ) ) ;
#54678 = CARTESIAN_POINT ( 'NONE',  ( 1.199500263597268246, -77.80208333333335702, 0.9218200799623752495 ) ) ;
#54679 = CARTESIAN_POINT ( 'NONE',  ( -1.107979503908000041, -78.05676310382339977, -1.174561767264999945 ) ) ;
#54680 = CARTESIAN_POINT ( 'NONE',  ( -9.867655926066998262, -76.19057412444000477, 7.916616500084998620 ) ) ;
#54681 = CARTESIAN_POINT ( 'NONE',  ( 9.596002108778174389, -78.59791666666667709, -7.374560639698961140 ) ) ;
#54682 = CARTESIAN_POINT ( 'NONE',  ( 0.4192948356380000186, -79.41793648960999974, -1.440205485619000081 ) ) ;
#54683 = DIRECTION ( 'NONE',  ( 0.000000000000000000, 1.000000000000000000, 0.000000000000000000 ) ) ;
#54684 = EDGE_CURVE ( 'NONE', #35302, #11183, #49469, .T. ) ;
#54685 = CARTESIAN_POINT ( 'NONE',  ( -10.75843888410000027, -79.44371210375499004, -1.985902594052000092 ) ) ;
#54686 = CARTESIAN_POINT ( 'NONE',  ( 12.71759155194729374, -60.86493881539610840, 1.809604648260254134 ) ) ;
#54687 = CARTESIAN_POINT ( 'NONE',  ( 12.83044027758000105, -55.49360215019999742, -2.062670899361999766 ) ) ;
#54688 = CARTESIAN_POINT ( 'NONE',  ( -3.306587955628999875, -83.23150571593299674, -1.277281160637999902 ) ) ;
#54689 = EDGE_LOOP ( 'NONE', ( #1389, #9633, #24928, #22320, #26180, #58005, #51131 ) ) ;
#54690 = CARTESIAN_POINT ( 'NONE',  ( -12.03384906095000062, -78.92404336158600131, 2.625351077966999735 ) ) ;
#54691 = CARTESIAN_POINT ( 'NONE',  ( 6.130995657900000673, -76.03909237496100104, 9.721816919625998921 ) ) ;
#54692 = CARTESIAN_POINT ( 'NONE',  ( 8.547764506834246490, -77.90230234131951192, 6.557723838816148287 ) ) ;
#54693 = CARTESIAN_POINT ( 'NONE',  ( -10.18114972182000066, -18.60990354280999881, 7.633087078986000584 ) ) ;
#54695 = DIRECTION ( 'NONE',  ( 1.000000000000000000, 0.000000000000000000, 0.000000000000000000 ) ) ;
#54694 = CARTESIAN_POINT ( 'NONE',  ( 8.838834764832000701, -18.75000000000000000, 8.838834764832000701 ) ) ;
#54696 = CARTESIAN_POINT ( 'NONE',  ( -3.461458192032003556, -3.264785587585083970, -0.6488018207460357623 ) ) ;
#54697 = CARTESIAN_POINT ( 'NONE',  ( -3.790141024232000166, -77.67121002409098196, -8.616613344227999960 ) ) ;
#54698 = CARTESIAN_POINT ( 'NONE',  ( 0.3488014753759141051, -85.88547957940599531, -7.786004205606935180 ) ) ;
#54699 = CARTESIAN_POINT ( 'NONE',  ( -3.455491054688999863, -78.55851086359500357, -10.47670062235000010 ) ) ;
#54700 = CARTESIAN_POINT ( 'NONE',  ( 5.137083998358000336, -77.31100733245999379, -10.56753840748999984 ) ) ;
#54701 = CARTESIAN_POINT ( 'NONE',  ( -10.62901853172999900, -80.93745138310640641, 2.931062299181000252 ) ) ;
#54702 = VERTEX_POINT ( 'NONE', #50341 ) ;
#54703 = CARTESIAN_POINT ( 'NONE',  ( -4.342561293556999935, -77.73719903538301423, -8.443909622126001935 ) ) ;
#54704 = CARTESIAN_POINT ( 'NONE',  ( -3.282727429393999863, -1.693833096892000123, 1.053290761329999770 ) ) ;
#54705 = CARTESIAN_POINT ( 'NONE',  ( -8.649885944100999424, -77.75323764143800531, -7.141259254888000285 ) ) ;
#54706 = CARTESIAN_POINT ( 'NONE',  ( -7.604423127187000198, -79.74545664141298573, 7.914351627518998455 ) ) ;
#54707 = DIRECTION ( 'NONE',  ( 0.000000000000000000, 0.000000000000000000, 1.000000000000000000 ) ) ;
#54708 = DIRECTION ( 'NONE',  ( 0.000000000000000000, 1.000000000000000000, 0.000000000000000000 ) ) ;
#54709 = DIRECTION ( 'NONE',  ( 0.000000000000000000, 1.000000000000000000, 1.125025998287000022E-13 ) ) ;
#54710 = DIRECTION ( 'NONE',  ( 1.000000000000000000, 0.000000000000000000, 0.000000000000000000 ) ) ;
#54711 = VECTOR ( 'NONE', #28061, 1000.000000000000114 ) ;
#54712 = CIRCLE ( 'NONE', #9450, 0.5000000000000004441 ) ;
#54713 = CARTESIAN_POINT ( 'NONE',  ( 1.268460950069999926, -83.62992953870899271, -3.974613432138999869 ) ) ;
#54714 = AXIS2_PLACEMENT_3D ( 'NONE', #11233, #6791, #30360 ) ;
#54715 = CARTESIAN_POINT ( 'NONE',  ( 1.500000000000000000, -80.25000000000000000, 0.000000000000000000 ) ) ;
#54716 = CARTESIAN_POINT ( 'NONE',  ( 8.790679651930998872, -53.86186536156999694, -8.797972003268000663 ) ) ;
#54717 = CARTESIAN_POINT ( 'NONE',  ( 3.911191660715999774, -77.12336614992500472, 10.56108632439999973 ) ) ;
#54718 = CARTESIAN_POINT ( 'NONE',  ( 0.4771943503223999850, -80.41851035578000051, -1.596102929133000004 ) ) ;
#54719 = CARTESIAN_POINT ( 'NONE',  ( -0.5511083744702001130, -79.11070398689999195, -1.199565526491999989 ) ) ;
#54720 = CARTESIAN_POINT ( 'NONE',  ( 12.00000000000000000, -77.54999999999999716, 0.000000000000000000 ) ) ;
#54721 = CARTESIAN_POINT ( 'NONE',  ( -1.064217634024700043, -81.81272298947914123, -1.071786072975686066 ) ) ;
#54722 = CARTESIAN_POINT ( 'NONE',  ( 0.6756574613765372606, -83.18743617693904469, 1.353690879101595801 ) ) ;
#54723 = CARTESIAN_POINT ( 'NONE',  ( -7.443611313279832054, -80.16459463203885605, -7.755757990568101334 ) ) ;
#54724 = CARTESIAN_POINT ( 'NONE',  ( -9.499999999999998224, -77.81041666666665435, -1.243547092045960367 ) ) ;
#54725 = EDGE_LOOP ( 'NONE', ( #34441, #56991, #14797, #56769 ) ) ;
#54726 = CARTESIAN_POINT ( 'NONE',  ( -1.163712929666468110, -81.62986445498971477, -0.4567824189295925930 ) ) ;
#54727 = DIRECTION ( 'NONE',  ( 0.000000000000000000, -1.000000000000000000, 0.000000000000000000 ) ) ;
#54728 = CARTESIAN_POINT ( 'NONE',  ( 11.14495853502000067, -80.13963010244600582, -0.2109943715695999922 ) ) ;
#54729 = CARTESIAN_POINT ( 'NONE',  ( -7.648026766733999615, -18.74999999413999774, -10.12290050089000104 ) ) ;
#54730 = EDGE_LOOP ( 'NONE', ( #37252, #19815, #32922, #48137, #3461, #39118 ) ) ;
#54731 = ORIENTED_EDGE ( 'NONE', *, *, #34403, .T. ) ;
#54732 = AXIS2_PLACEMENT_3D ( 'NONE', #5265, #44833, #32113 ) ;
#54733 = CARTESIAN_POINT ( 'NONE',  ( 0.9005648571752999931, -80.92291525475098979, 1.095007794218000097 ) ) ;
#54734 = EDGE_LOOP ( 'NONE', ( #25187, #4009, #42392, #24087 ) ) ;
#54735 = ORIENTED_EDGE ( 'NONE', *, *, #39358, .F. ) ;
#54736 = CARTESIAN_POINT ( 'NONE',  ( -2.015551294784000191, -18.19652295155999866, 12.79857978895000059 ) ) ;
#54737 = DIRECTION ( 'NONE',  ( 0.000000000000000000, -1.000000000000000000, 0.000000000000000000 ) ) ;
#54738 = ADVANCED_FACE ( 'NONE', ( #9307 ), #18461, .F. ) ;
#54739 = CARTESIAN_POINT ( 'NONE',  ( -2.311705299946139380, -81.89895831805255000, -2.551961939471520946 ) ) ;
#54740 = CARTESIAN_POINT ( 'NONE',  ( 2.424019779656216400, -78.24625956200173960, -8.927873433679032189 ) ) ;
#54741 = LINE ( 'NONE', #31997, #25344 ) ;
#54742 = CARTESIAN_POINT ( 'NONE',  ( -10.31585246991000027, -78.28606593309000061, -5.959411202814999697 ) ) ;
#54743 = ORIENTED_EDGE ( 'NONE', *, *, #29021, .T. ) ;
#54745 = ORIENTED_EDGE ( 'NONE', *, *, #21135, .F. ) ;
#54744 = B_SPLINE_CURVE_WITH_KNOTS ( 'NONE', 3,
 ( #49713, #4238, #57965, #13964 ),
 .UNSPECIFIED., .F., .F.,
 ( 4, 4 ),
 ( 0.000000000000000000, 1.000000000000000000 ),
 .UNSPECIFIED. ) ;
#54746 = CIRCLE ( 'NONE', #31283, 3.249999999999999556 ) ;
#54747 = DIRECTION ( 'NONE',  ( 0.000000000000000000, 1.000000000000000000, 0.000000000000000000 ) ) ;
#54748 = FACE_OUTER_BOUND ( 'NONE', #43774, .T. ) ;
#54749 = CARTESIAN_POINT ( 'NONE',  ( -1.500000000000000000, -78.39999999999999147, 0.000000000000000000 ) ) ;
#54750 = CARTESIAN_POINT ( 'NONE',  ( -4.814859605045999302, -78.62586029149998978, 8.425427962446999430 ) ) ;
#54751 = DIRECTION ( 'NONE',  ( 0.000000000000000000, 1.000000000000000000, 0.000000000000000000 ) ) ;
#54752 = CARTESIAN_POINT ( 'NONE',  ( 3.528139790557236477, -85.82128727395084411, 1.440633993175003402 ) ) ;
#54753 = CARTESIAN_POINT ( 'NONE',  ( -9.650487694675000228, -78.36836734003000515, 7.043610823269999877 ) ) ;
#54754 = B_SPLINE_SURFACE_WITH_KNOTS ( 'NONE', 3, 3, ( 
 ( #26960, #27251, #5699, #18420, #54139, #44990, #5412, #442, #13679, #28123, #9853, #55007, #22837, #36123, #45880, #23420, #45291, #152, #46173, #54439, #41432, #9559, #14555, #32548, #4841, #1018, #23710, #41720, #50597, #49424, #36411, #40559, #17834, #18128, #31677 ),
 ( #10146, #35822, #40850, #31970, #53851, #8974, #45587, #4546, #5132, #22548, #23129, #49723, #9266, #729, #18709, #36703, #54718, #14261, #32257, #50303, #27834, #10736, #48409, #1883, #37575, #28417, #48126, #42315, #55592, #12378, #52538, #39238, #6286, #19576, #30076 ),
 ( #30366, #19877, #16817, #5992, #10432, #19291, #25658, #1586, #57250, #7945, #52823, #47842, #24301, #46764, #7659, #43388, #15141, #2947, #28712, #38663, #33136, #3243, #56683, #14845, #20947, #16240, #34219, #51179, #12095, #43689, #1298, #52254, #21235, #23998, #16528 ),
 ( #11812, #55299, #34801, #46464, #25948, #37283, #32839, #29787, #50886, #42016, #7373, #25373, #38952, #56965, #34507, #4, #31232, #13540, #21523, #3806, #26516, #9124, #30656, #49577, #49274, #40107, #17682, #53702, #8826, #58120, #35671, #35077, #17982, #26813, #22397 ) ),
 .UNSPECIFIED., .F., .F., .F.,
 ( 4, 4 ),
 ( 4, 1, 1, 1, 1, 1, 1, 1, 1, 1, 1, 1, 1, 1, 1, 1, 1, 1, 1, 1, 1, 1, 1, 1, 1, 1, 1, 1, 1, 1, 1, 1, 4 ),
 ( -0.3882448580381000491, 1.388244858038000018 ),
 ( -0.02000000000000000042, 0.01250000000000000069, 0.04499999999999999833, 0.07749999999999999944, 0.1100000000000000006, 0.1424999999999999878, 0.1749999999999999889, 0.2074999999999999900, 0.2399999999999999911, 0.2725000000000000200, 0.3049999999999999933, 0.3375000000000000222, 0.3699999999999999956, 0.4025000000000000244, 0.4349999999999999978, 0.4675000000000000266, 0.5000000000000000000, 0.5324999999999999734, 0.5649999999999999467, 0.5975000000000000311, 0.6300000000000000044, 0.6624999999999999778, 0.6949999999999999512, 0.7275000000000000355, 0.7600000000000000089, 0.7924999999999999822, 0.8249999999999999556, 0.8575000000000000400, 0.8900000000000000133, 0.9224999999999999867, 0.9549999999999999600, 0.9875000000000000444, 1.020000000000000018 ),
 .UNSPECIFIED. ) ;
#54755 = EDGE_CURVE ( 'NONE', #13712, #46203, #13339, .T. ) ;
#54756 = CARTESIAN_POINT ( 'NONE',  ( -1.456085397364999867, -81.23900587363999648, -0.6271128268704999620 ) ) ;
#54757 = CARTESIAN_POINT ( 'NONE',  ( -7.731096697273209806, -77.00347157156862465, 5.096092861886030612 ) ) ;
#54758 = DIRECTION ( 'NONE',  ( 0.000000000000000000, 1.000000000000000000, 0.000000000000000000 ) ) ;
#54759 = CARTESIAN_POINT ( 'NONE',  ( 0.7554157024156027411, -76.56982309619165505, 11.72738829954458595 ) ) ;
#54760 = CARTESIAN_POINT ( 'NONE',  ( 0.6660276224462000627, -82.16974633842799847, -4.121401291365000219 ) ) ;
#54761 = CARTESIAN_POINT ( 'NONE',  ( 7.496935112050000072, -80.65095063950900567, 8.408636027568000770 ) ) ;
#54762 = CARTESIAN_POINT ( 'NONE',  ( 2.006136628026000235, -78.21226001420198770, -9.477164255927000625 ) ) ;
#54763 = CARTESIAN_POINT ( 'NONE',  ( 3.162225869758173324, -2.869653500654393063, 0.7815842452000089091 ) ) ;
#54764 = CARTESIAN_POINT ( 'NONE',  ( 2.359885590755999907, -81.17007046129099024, 2.648677523046000015 ) ) ;
#54765 = CARTESIAN_POINT ( 'NONE',  ( -1.150888948972000003, -79.13596084748500914, 0.6738713386821000295 ) ) ;
#54766 = PLANE ( 'NONE',  #15815 ) ;
#54767 = CARTESIAN_POINT ( 'NONE',  ( 12.50240633875000107, -54.11762602111000575, 1.005381409374000112 ) ) ;
#54768 = EDGE_CURVE ( 'NONE', #33739, #43690, #28302, .T. ) ;
#54769 = CARTESIAN_POINT ( 'NONE',  ( 3.542727183245000244, -3.037558102910000279, -1.391102635753999950 ) ) ;
#54770 = CARTESIAN_POINT ( 'NONE',  ( 6.848120951879766771, -77.19999999999998863, -8.441927890790847044 ) ) ;
#54771 = ORIENTED_EDGE ( 'NONE', *, *, #8142, .T. ) ;
#54772 = CARTESIAN_POINT ( 'NONE',  ( 5.539808784079907511, -78.36666666666667425, -9.611650271896827746 ) ) ;
#54773 = CARTESIAN_POINT ( 'NONE',  ( 7.666647577129663382, -60.55042584425824259, -7.889735440113329723 ) ) ;
#54774 = EDGE_CURVE ( 'NONE', #34958, #52197, #31719, .T. ) ;
#54775 = CARTESIAN_POINT ( 'NONE',  ( 9.722718241315000398, -23.25000000000000000, 7.954951288349001004 ) ) ;
#54776 = CARTESIAN_POINT ( 'NONE',  ( 6.165970644978999715, -79.14971247365699014, 7.554510225358000319 ) ) ;
#54777 = CARTESIAN_POINT ( 'NONE',  ( 5.715297388934000189, -78.28681763324999565, 11.69132169264999987 ) ) ;
#54778 = CARTESIAN_POINT ( 'NONE',  ( -8.941925947373027483, -79.55322172220051868, 5.966891831842909610 ) ) ;
#54779 = LINE ( 'NONE', #14322, #28218 ) ;
#54780 = CARTESIAN_POINT ( 'NONE',  ( 11.23304052927915642, -78.47249383617504748, 3.444503982574532497 ) ) ;
#54781 = EDGE_LOOP ( 'NONE', ( #33346, #38241, #47662, #51779 ) ) ;
#54782 = CARTESIAN_POINT ( 'NONE',  ( 0.5999999999999999778, -5.000000000000000000, -0.5999999999999999778 ) ) ;
#54783 = CARTESIAN_POINT ( 'NONE',  ( 10.91664470761000061, -77.98939760156699208, -0.5030651442900000436 ) ) ;
#54784 = CARTESIAN_POINT ( 'NONE',  ( -1.096457908046999830, -82.34294633480099890, 1.170898023252000097 ) ) ;
#54785 = CARTESIAN_POINT ( 'NONE',  ( 7.612971540276999960, -23.32452273707999879, -10.53003236233000095 ) ) ;
#54786 = CIRCLE ( 'NONE', #16149, 5.000000000000000000 ) ;
#54787 = CARTESIAN_POINT ( 'NONE',  ( 8.191903123214999027, -78.31180405034399428, 4.637231687908999866 ) ) ;
#54789 = CARTESIAN_POINT ( 'NONE',  ( -3.858199361241999803, -0.8051001901206000788, -1.117275487237999965 ) ) ;
#54788 = CARTESIAN_POINT ( 'NONE',  ( -0.7993309613926999901, -83.34017939494499672, -4.052108522299000093 ) ) ;
#54790 = CARTESIAN_POINT ( 'NONE',  ( -1.931087888240000217, -55.48415267986000288, -12.71658872082999814 ) ) ;
#54791 = CARTESIAN_POINT ( 'NONE',  ( 1.187026915874999755, -80.44399715222199632, 0.5757885860275999690 ) ) ;
#54792 = EDGE_CURVE ( 'NONE', #1603, #39698, #4836, .T. ) ;
#54793 = ORIENTED_EDGE ( 'NONE', *, *, #12169, .F. ) ;
#54794 = CARTESIAN_POINT ( 'NONE',  ( 0.000000000000000000, -75.00000000000000000, 7.200000000000000178 ) ) ;
#54795 = CARTESIAN_POINT ( 'NONE',  ( 0.9218200799623741393, -79.07708333333334849, -1.199500263597268690 ) ) ;
#54796 = AXIS2_PLACEMENT_3D ( 'NONE', #2241, #6652, #33507 ) ;
#54797 = CARTESIAN_POINT ( 'NONE',  ( -3.962812355711033074, -78.85171438276199751, 7.925624711422019075 ) ) ;
#54798 = ORIENTED_EDGE ( 'NONE', *, *, #5058, .F. ) ;
#54799 = ORIENTED_EDGE ( 'NONE', *, *, #36578, .T. ) ;
#54800 = CARTESIAN_POINT ( 'NONE',  ( 11.90415444617999974, -79.94018912574220792, -1.731350929957999885 ) ) ;
#54801 = DIRECTION ( 'NONE',  ( -1.000000000000000000, 0.000000000000000000, 0.000000000000000000 ) ) ;
#54802 = DIRECTION ( 'NONE',  ( 3.675130213670998824E-09, -0.9999999999999997780, -2.168720875627999536E-08 ) ) ;
#54803 = EDGE_LOOP ( 'NONE', ( #33448, #42804 ) ) ;
#54804 = CARTESIAN_POINT ( 'NONE',  ( -11.80948866808000020, -78.67521964476598839, 2.394107155543000243 ) ) ;
#54805 = ORIENTED_EDGE ( 'NONE', *, *, #48250, .T. ) ;
#54806 = EDGE_LOOP ( 'NONE', ( #41954, #22627, #38546, #15230 ) ) ;
#54807 = CARTESIAN_POINT ( 'NONE',  ( -2.225834838116822034, -2.665714381188136972, -2.367851236585388541 ) ) ;
#54808 = ORIENTED_EDGE ( 'NONE', *, *, #54978, .T. ) ;
#54809 = CARTESIAN_POINT ( 'NONE',  ( -5.318190277593210169, -76.48798860270505884, -10.78586198116576256 ) ) ;
#54810 = DIRECTION ( 'NONE',  ( 3.788556036780999566E-11, -1.000000000000000000, 0.000000000000000000 ) ) ;
#54811 = ORIENTED_EDGE ( 'NONE', *, *, #22017, .T. ) ;
#54812 = CARTESIAN_POINT ( 'NONE',  ( -9.546815223803999828, -54.11472046612000497, -8.130854305859001485 ) ) ;
#54813 = CIRCLE ( 'NONE', #15237, 11.70000000000000107 ) ;
#54814 = ORIENTED_EDGE ( 'NONE', *, *, #23876, .T. ) ;
#54815 = CARTESIAN_POINT ( 'NONE',  ( -10.47020627418439354, -80.52083333333331439, -2.813789756862263847 ) ) ;
#54816 = CARTESIAN_POINT ( 'NONE',  ( 2.867595730404614240, -77.99877691775095911, -9.270961250973028811 ) ) ;
#54817 = LINE ( 'NONE', #26763, #45403 ) ;
#54818 = CARTESIAN_POINT ( 'NONE',  ( 1.247385798810000113, -54.32277743478999810, -12.50301438874000048 ) ) ;
#54819 = CARTESIAN_POINT ( 'NONE',  ( -10.99972769911000015, -76.18386543273099676, 2.019869862886000345 ) ) ;
#54820 = DIRECTION ( 'NONE',  ( -0.7071067811865474617, 0.7071067811865474617, 6.547106584528433984E-10 ) ) ;
#54821 = EDGE_CURVE ( 'NONE', #53612, #35878, #50046, .T. ) ;
#54822 = CARTESIAN_POINT ( 'NONE',  ( -5.917523019358107206, -78.71666666666666856, 10.26699006316250795 ) ) ;
#54823 = CARTESIAN_POINT ( 'NONE',  ( -7.682344222575999915, -56.03537109808000594, -10.04116292115999975 ) ) ;
#54824 = CARTESIAN_POINT ( 'NONE',  ( 5.208840937792781567, -78.77265696413414275, -7.682242898499267447 ) ) ;
#54825 = CARTESIAN_POINT ( 'NONE',  ( 4.693089899494290229, -76.54199774624609631, 10.77217413037992699 ) ) ;
#54826 = EDGE_CURVE ( 'NONE', #42686, #54392, #1010, .T. ) ;
#54827 = CARTESIAN_POINT ( 'NONE',  ( -8.296701268784000050, -77.03153501420199234, 4.443109075551999965 ) ) ;
#54828 = CARTESIAN_POINT ( 'NONE',  ( -1.185397549814999785, -80.17221547735599074, -0.6110718436566999756 ) ) ;
#54829 = CARTESIAN_POINT ( 'NONE',  ( -8.735356708122031577, -80.15212943903959797, -6.698788252584580327 ) ) ;
#54830 = CARTESIAN_POINT ( 'NONE',  ( 9.760317337979069308, -78.25305829502794097, 7.105173469063493563 ) ) ;
#54831 = CARTESIAN_POINT ( 'NONE',  ( 0.9178498446945000389, -81.08317549782599087, 4.026916334423999544 ) ) ;
#54832 = CARTESIAN_POINT ( 'NONE',  ( 1.856358691897999957, -77.05271332859899758, 9.472443054301999510 ) ) ;
#54833 = FACE_OUTER_BOUND ( 'NONE', #21890, .T. ) ;
#54834 = CARTESIAN_POINT ( 'NONE',  ( -10.75000000000000000, -79.51041666666668561, -1.407171709420429018 ) ) ;
#54835 = CARTESIAN_POINT ( 'NONE',  ( 13.63885489310999510, -59.58578169018998949, 7.254376133916000668 ) ) ;
#54836 = CARTESIAN_POINT ( 'NONE',  ( 6.108123033638238830, -80.00000000000000000, 7.128822434192190194 ) ) ;
#54837 = CARTESIAN_POINT ( 'NONE',  ( -3.385193567608999476, -1.931486014851000022, 1.699696520826999846 ) ) ;
#54838 = CARTESIAN_POINT ( 'NONE',  ( 10.55911395187000146, -59.58461666436000570, 7.642160924878999673 ) ) ;
#54839 = CARTESIAN_POINT ( 'NONE',  ( -1.691611010928000036, -24.23082691229999952, -12.66722148969999928 ) ) ;
#54840 = DIRECTION ( 'NONE',  ( -0.07798810297990073359, -0.04890180925223042846, 0.9957542211035085300 ) ) ;
#54841 = CARTESIAN_POINT ( 'NONE',  ( 2.612650524949999831, -3.236812248861999919, -2.307222756693999788 ) ) ;
#54842 = CARTESIAN_POINT ( 'NONE',  ( 3.102135221549690236, -77.30237053728062335, 10.38336816366492243 ) ) ;
#54843 = LINE ( 'NONE', #18257, #6219 ) ;
#54845 = CARTESIAN_POINT ( 'NONE',  ( -0.9215294167384999735, -77.86600855774059937, -1.077461862040000051 ) ) ;
#54844 = CARTESIAN_POINT ( 'NONE',  ( 1.499999999999999778, -79.66041666666667709, 0.1963495408493654004 ) ) ;
#54846 = CARTESIAN_POINT ( 'NONE',  ( 0.6196687357644999894, -82.42461323090898873, -1.586136063883000213 ) ) ;
#54847 = ORIENTED_EDGE ( 'NONE', *, *, #40495, .T. ) ;
#54848 = CARTESIAN_POINT ( 'NONE',  ( 1.091293945889000083, -83.83707450217399071, -3.419475842359000151 ) ) ;
#54849 = CARTESIAN_POINT ( 'NONE',  ( -4.459146134027999864, -80.11617729102648866, 10.37101146982000088 ) ) ;
#54850 = CARTESIAN_POINT ( 'NONE',  ( -12.76303204522000101, -23.26485147686999966, -1.980584515753000208 ) ) ;
#54851 = FACE_OUTER_BOUND ( 'NONE', #41800, .T. ) ;
#54852 = CARTESIAN_POINT ( 'NONE',  ( 9.144378690012999300, -77.53474228896699572, -6.496033325431000094 ) ) ;
#54853 = DIRECTION ( 'NONE',  ( -1.000000000000000000, 0.000000000000000000, 0.000000000000000000 ) ) ;
#54854 = DIRECTION ( 'NONE',  ( 0.000000000000000000, -1.000000000000000000, 0.000000000000000000 ) ) ;
#54855 = CARTESIAN_POINT ( 'NONE',  ( -3.575925901623000058, -0.7202288115830999260, -0.05194511807925000085 ) ) ;
#54856 = CARTESIAN_POINT ( 'NONE',  ( -4.721094452241000106, -79.18541001252299338, 8.691768742354998523 ) ) ;
#54857 = CARTESIAN_POINT ( 'NONE',  ( -9.490437400528026757, -76.14895833332546715, 5.483493355980267658 ) ) ;
#54858 = EDGE_CURVE ( 'NONE', #16988, #21964, #4591, .T. ) ;
#54859 = ORIENTED_EDGE ( 'NONE', *, *, #46191, .F. ) ;
#54860 = CARTESIAN_POINT ( 'NONE',  ( 1.308715794772571828, -54.05595500774170858, -12.70256747352388338 ) ) ;
#54861 = CARTESIAN_POINT ( 'NONE',  ( 7.624341766656999475, -60.06485146221000093, 10.42531125026000005 ) ) ;
#54862 = FACE_OUTER_BOUND ( 'NONE', #30417, .T. ) ;
#54863 = LINE ( 'NONE', #50454, #34587 ) ;
#54864 = FACE_OUTER_BOUND ( 'NONE', #18770, .T. ) ;
#54865 = DIRECTION ( 'NONE',  ( -0.7071067811865475727, 0.000000000000000000, 0.7071067811865475727 ) ) ;
#54866 = ORIENTED_EDGE ( 'NONE', *, *, #4869, .T. ) ;
#54867 = CARTESIAN_POINT ( 'NONE',  ( 1.675539995062999887, -79.19048418952499446, 11.92720225554999836 ) ) ;
#54868 = CARTESIAN_POINT ( 'NONE',  ( 8.064399500920000463, -77.80418109758298328, 7.789238951990999915 ) ) ;
#54869 = DIRECTION ( 'NONE',  ( 1.000000000000000000, 0.000000000000000000, 0.000000000000000000 ) ) ;
#54870 = CIRCLE ( 'NONE', #5856, 1.250000000000000000 ) ;
#54871 = EDGE_CURVE ( 'NONE', #31838, #10296, #50971, .T. ) ;
#54872 = ORIENTED_EDGE ( 'NONE', *, *, #13474, .T. ) ;
#54873 = CARTESIAN_POINT ( 'NONE',  ( 12.50240681834000078, -24.68234730741999883, -1.005418943851999813 ) ) ;
#54874 = CARTESIAN_POINT ( 'NONE',  ( -5.809791519574999619, -79.25584552244097836, 7.851562197947999699 ) ) ;
#54875 = ORIENTED_EDGE ( 'NONE', *, *, #38273, .F. ) ;
#54876 = CARTESIAN_POINT ( 'NONE',  ( -7.709154088362966561, -54.87253195859281618, 9.998702477015426027 ) ) ;
#54877 = CARTESIAN_POINT ( 'NONE',  ( 9.355938762748150950, -25.17483711029779414, -8.610912454445188047 ) ) ;
#54878 = CARTESIAN_POINT ( 'NONE',  ( -12.54980660768000078, -25.04777352165000082, 0.05651102257796999928 ) ) ;
#54879 = VERTEX_POINT ( 'NONE', #27296 ) ;
#54880 = CARTESIAN_POINT ( 'NONE',  ( 8.979348251287998295, -77.84629805011500991, 3.086914251890999772 ) ) ;
#54881 = CARTESIAN_POINT ( 'NONE',  ( 10.21026245503029450, -17.74392421793578833, -7.764236519581510620 ) ) ;
#54882 = CARTESIAN_POINT ( 'NONE',  ( -1.722320549991694039, -17.76336311174892657, -12.71171904436490685 ) ) ;
#54883 = CARTESIAN_POINT ( 'NONE',  ( -3.621447497675000182, -78.40681307390448751, -1.372262476832999913E-09 ) ) ;
#54884 = ADVANCED_FACE ( 'NONE', ( #54479 ), #14014, .T. ) ;
#54885 = CARTESIAN_POINT ( 'NONE',  ( 1.500000000000000000, -78.64999999999999147, 0.000000000000000000 ) ) ;
#54886 = CARTESIAN_POINT ( 'NONE',  ( -0.4639630351240068284, -78.24932064131154164, 1.464561517630637910 ) ) ;
#54887 = CARTESIAN_POINT ( 'NONE',  ( -4.008544904492841177, -80.16458332861317615, 0.5932793604889254890 ) ) ;
#54888 = EDGE_LOOP ( 'NONE', ( #16799, #19087, #25895, #8109 ) ) ;
#54889 = FACE_OUTER_BOUND ( 'NONE', #3082, .T. ) ;
#54890 = EDGE_CURVE ( 'NONE', #38477, #45960, #44331, .T. ) ;
#54891 = CARTESIAN_POINT ( 'NONE',  ( -1.771468677314999907, -75.86915816935000123, 12.18184739844999953 ) ) ;
#54892 = CARTESIAN_POINT ( 'NONE',  ( -0.5899402231854000700, -79.50329419107600870, -1.503093382721999882 ) ) ;
#54893 = CARTESIAN_POINT ( 'NONE',  ( 1.576369461341504019, -2.510257082558531749, -3.216291020494079334 ) ) ;
#54894 = CARTESIAN_POINT ( 'NONE',  ( 4.000000000000000000, -5.200000000000000178, 0.5999999999999999778 ) ) ;
#54895 = CARTESIAN_POINT ( 'NONE',  ( 3.086017585447000222, -79.19724228728000526, -11.86910201801999953 ) ) ;
#54896 = CARTESIAN_POINT ( 'NONE',  ( -13.94827586207000003, -45.69638659094999866, -8.082388077679998639E-06 ) ) ;
#54897 = CARTESIAN_POINT ( 'NONE',  ( 12.70556836329126149, -16.77227722666621190, -0.2641978056567622635 ) ) ;
#54898 = CARTESIAN_POINT ( 'NONE',  ( 10.09635298639789625, -60.32373519955886820, -7.644087781989472141 ) ) ;
#54899 = CARTESIAN_POINT ( 'NONE',  ( 7.954951288349001004, -55.54999999966999980, 9.722718241315000398 ) ) ;
#54900 = CARTESIAN_POINT ( 'NONE',  ( -7.301194973305000779, -79.18140372876651156, 8.515319286630999684 ) ) ;
#54901 = EDGE_CURVE ( 'NONE', #37657, #40036, #49356, .T. ) ;
#54902 = VERTEX_POINT ( 'NONE', #25747 ) ;
#54903 = FACE_OUTER_BOUND ( 'NONE', #40032, .T. ) ;
#54904 = CARTESIAN_POINT ( 'NONE',  ( -1.217840012802438698, -78.62105508162261458, -0.3270303979875727740 ) ) ;
#54905 = CARTESIAN_POINT ( 'NONE',  ( 7.864802647417423742, -24.45123893519480163, 10.10444599041134417 ) ) ;
#54906 = AXIS2_PLACEMENT_3D ( 'NONE', #51359, #56074, #42783 ) ;
#54907 = CARTESIAN_POINT ( 'NONE',  ( -12.00000000000000000, -18.84999999997999964, 0.7999999999999001243 ) ) ;
#54908 = CARTESIAN_POINT ( 'NONE',  ( 7.678657038172564064, -23.79377623515379270, 10.03844138475566261 ) ) ;
#54909 = CARTESIAN_POINT ( 'NONE',  ( -1.561527218546999940, -82.29871160559999055, -0.5804237711334999661 ) ) ;
#54910 = CARTESIAN_POINT ( 'NONE',  ( 4.441925970415999458, -77.42124252579399979, 11.07721969470000190 ) ) ;
#54911 = CARTESIAN_POINT ( 'NONE',  ( 1.251117773441000169, -77.57157087262599759, 9.549236319306000809 ) ) ;
#54912 = CARTESIAN_POINT ( 'NONE',  ( 4.496864984682853894, -76.04321546014720923, 10.85509615260737348 ) ) ;
#54913 = CARTESIAN_POINT ( 'NONE',  ( 2.343379474233999726, -80.38402960327920255, 10.44606179296999926 ) ) ;
#54914 = CARTESIAN_POINT ( 'NONE',  ( 3.241578942234978999, -85.83735717367099483, -1.443243930775044870 ) ) ;
#54915 = ORIENTED_EDGE ( 'NONE', *, *, #53, .F. ) ;
#54916 = CARTESIAN_POINT ( 'NONE',  ( 1.750000000000000000, -18.75000000310999937, 12.50000000000000000 ) ) ;
#54917 = CONICAL_SURFACE ( 'NONE', #44543, 0.6999999997695030007, 0.7853981633972997312 ) ;
#54918 = CARTESIAN_POINT ( 'NONE',  ( 8.082760247877876836, -77.89183626726020293, 4.658660117716662441 ) ) ;
#54919 = CARTESIAN_POINT ( 'NONE',  ( -10.86848958346127247, -76.18151041669857193, -1.423534178637803960 ) ) ;
#54920 = CARTESIAN_POINT ( 'NONE',  ( 12.00000000000000000, -55.54999999966999980, -1.250000000000000000 ) ) ;
#54921 = CARTESIAN_POINT ( 'NONE',  ( -5.327124403004999564, -75.96338747164598715, -11.31261546482999947 ) ) ;
#54922 = CARTESIAN_POINT ( 'NONE',  ( 0.000000000000000000, -2.900000000000000355, -12.80000000000000071 ) ) ;
#54923 = CARTESIAN_POINT ( 'NONE',  ( 7.969034948596000589, -17.37623147815000024, -9.934750886910000744 ) ) ;
#54924 = CARTESIAN_POINT ( 'NONE',  ( -5.869402599192000025, -78.36567021304000491, 10.46661899222999992 ) ) ;
#54925 = VERTEX_POINT ( 'NONE', #57049 ) ;
#54927 = AXIS2_PLACEMENT_3D ( 'NONE', #29221, #30079, #33938 ) ;
#54926 = CARTESIAN_POINT ( 'NONE',  ( -2.830810333559000025, -78.81343076078299248, -10.78151721355999904 ) ) ;
#54928 = CARTESIAN_POINT ( 'NONE',  ( -9.249803168447471080, -77.49364314078148652, 0.7265176776316289997 ) ) ;
#54929 = CARTESIAN_POINT ( 'NONE',  ( -10.75000000000000000, -80.00000000000000000, 0.000000000000000000 ) ) ;
#54930 = CARTESIAN_POINT ( 'NONE',  ( 3.621447497675000182, -78.40681307385639798, -4.434994086307880463E-16 ) ) ;
#54931 = CARTESIAN_POINT ( 'NONE',  ( 10.35453599130000057, -76.65783510652001098, -6.064947188958000446 ) ) ;
#54932 = CONICAL_SURFACE ( 'NONE', #37016, 3.471875000818999801, 0.7853981633972997312 ) ;
#54933 = DIRECTION ( 'NONE',  ( 1.000000000000000000, 0.000000000000000000, 0.000000000000000000 ) ) ;
#54934 = CARTESIAN_POINT ( 'NONE',  ( -9.295554138914937425, -76.99999999999998579, -1.018217055612035127 ) ) ;
#54935 = CARTESIAN_POINT ( 'NONE',  ( -8.441163348734360028, -17.08348045813886529, -9.243160721213708797 ) ) ;
#54936 = EDGE_CURVE ( 'NONE', #9760, #45077, #25492, .T. ) ;
#54937 = DIRECTION ( 'NONE',  ( 0.000000000000000000, -1.000000000000000000, 0.000000000000000000 ) ) ;
#54938 = CARTESIAN_POINT ( 'NONE',  ( -1.165746613897999928E-14, -72.79999999999999716, 0.000000000000000000 ) ) ;
#54939 = EDGE_CURVE ( 'NONE', #14936, #12183, #39327, .T. ) ;
#54940 = CARTESIAN_POINT ( 'NONE',  ( -3.548359637466153238, -79.54890456983206093, -10.38638352587388169 ) ) ;
#54941 = CYLINDRICAL_SURFACE ( 'NONE', #52605, 0.6000000000000008660 ) ;
#54942 = EDGE_LOOP ( 'NONE', ( #37442, #35906, #42282, #41108 ) ) ;
#54943 = VERTEX_POINT ( 'NONE', #43771 ) ;
#54944 = CARTESIAN_POINT ( 'NONE',  ( 8.072669757012000957, -77.73631332859899601, 4.870514429535999668 ) ) ;
#54945 = CARTESIAN_POINT ( 'NONE',  ( 6.822280249786099482, -78.77980337427507607, -8.307691429770278191 ) ) ;
#54946 = VECTOR ( 'NONE', #11573, 1000.000000000000114 ) ;
#54947 = ORIENTED_EDGE ( 'NONE', *, *, #43314, .F. ) ;
#54948 = CARTESIAN_POINT ( 'NONE',  ( 9.886069181790999139, -76.46128543308955727, -5.228720670581999741 ) ) ;
#54949 = CARTESIAN_POINT ( 'NONE',  ( -2.278711097333574465, -83.40208334745025809, -2.582645949866041235 ) ) ;
#54950 = CARTESIAN_POINT ( 'NONE',  ( 10.07616267223999884, -61.52631138996999738, 7.986947465035998839 ) ) ;
#54951 = CARTESIAN_POINT ( 'NONE',  ( 3.166308453645628074, -76.40348697233208952, 11.78162183767860682 ) ) ;
#54952 = CARTESIAN_POINT ( 'NONE',  ( 11.20814727018469981, -77.82862452491039562, 4.230534968287241959 ) ) ;
#54953 = CARTESIAN_POINT ( 'NONE',  ( -4.152600241220000044, -79.36092712597098853, -10.41988588363999924 ) ) ;
#54954 = CARTESIAN_POINT ( 'NONE',  ( 2.443158415888972090, -1.792198805145689633, -2.251047301635219267 ) ) ;
#54955 = VERTEX_POINT ( 'NONE', #3321 ) ;
#54956 = CARTESIAN_POINT ( 'NONE',  ( 10.44963345251333919, -78.02857427158255632, -2.857245842109498835 ) ) ;
#54957 = ORIENTED_EDGE ( 'NONE', *, *, #15251, .T. ) ;
#54959 = EDGE_CURVE ( 'NONE', #33527, #28360, #42902, .T. ) ;
#54958 = B_SPLINE_CURVE_WITH_KNOTS ( 'NONE', 3,
 ( #50481, #6464, #41903, #55480 ),
 .UNSPECIFIED., .F., .F.,
 ( 4, 4 ),
 ( 0.000000000000000000, 1.000000000000000000 ),
 .UNSPECIFIED. ) ;
#54960 = CARTESIAN_POINT ( 'NONE',  ( 9.246497739354760270, -77.35225292060245295, 0.2614339155388125113 ) ) ;
#54961 = CARTESIAN_POINT ( 'NONE',  ( -7.062685404271999978, -77.80008692246998692, 8.485436034813998774 ) ) ;
#54962 = FACE_OUTER_BOUND ( 'NONE', #39858, .T. ) ;
#54963 = CARTESIAN_POINT ( 'NONE',  ( 9.703485699160999900, -77.64139207422398670, 0.1143444355825999903 ) ) ;
#54964 = CARTESIAN_POINT ( 'NONE',  ( -2.438596655773999977, -76.13481484252000087, 12.41356352284000053 ) ) ;
#54965 = CARTESIAN_POINT ( 'NONE',  ( 10.35396498619769190, -76.69116843985601406, -6.064612950829414650 ) ) ;
#54966 = CARTESIAN_POINT ( 'NONE',  ( 0.3877229342594999961, -77.85531778169000461, -1.580612325761999948 ) ) ;
#54967 = CARTESIAN_POINT ( 'NONE',  ( -1.456717367586000012E-14, -79.29999999999999716, 0.000000000000000000 ) ) ;
#54968 = AXIS2_PLACEMENT_3D ( 'NONE', #45359, #45065, #41790 ) ;
#54969 = CARTESIAN_POINT ( 'NONE',  ( -1.293339008660999934, -78.54475676510898552, -10.86347506762000137 ) ) ;
#54970 = CARTESIAN_POINT ( 'NONE',  ( -8.588902834690999910, -25.13240111580999780, -9.317946123639000433 ) ) ;
#54971 = CARTESIAN_POINT ( 'NONE',  ( -7.555116226634104315, -60.48684619743404056, 7.995796640818095824 ) ) ;
#54972 = EDGE_CURVE ( 'NONE', #53581, #29780, #34914, .T. ) ;
#54973 = CARTESIAN_POINT ( 'NONE',  ( 2.573844042005999810, -83.71250737700098909, -2.437272650364000093 ) ) ;
#54974 = VERTEX_POINT ( 'NONE', #52624 ) ;
#54975 = CARTESIAN_POINT ( 'NONE',  ( 6.043427764450807871, -79.56666666666666288, -10.48543666025108756 ) ) ;
#54976 = CARTESIAN_POINT ( 'NONE',  ( -3.290092089285999499, -76.67444993108999540, 11.13683286123999849 ) ) ;
#54977 = PLANE ( 'NONE',  #20072 ) ;
#54978 = EDGE_CURVE ( 'NONE', #17731, #9942, #16852, .T. ) ;
#54979 = CARTESIAN_POINT ( 'NONE',  ( -11.96278216175999987, -78.06186122270700878, 0.6386762756999999624 ) ) ;
#54980 = CARTESIAN_POINT ( 'NONE',  ( -3.250000000000000000, -2.000000000000000000, 0.000000000000000000 ) ) ;
#54982 = CARTESIAN_POINT ( 'NONE',  ( 0.000000000000000000, -18.84999999999999787, -11.79999999999999893 ) ) ;
#54981 = CARTESIAN_POINT ( 'NONE',  ( -1.704789469357325560, -60.50346161385032673, -12.53199752970037473 ) ) ;
#54983 = CARTESIAN_POINT ( 'NONE',  ( -2.641758692652436125, -3.192411922226876531, 2.330954230004774086 ) ) ;
#54984 = CARTESIAN_POINT ( 'NONE',  ( 4.081313924463877640, -80.94422573434229662, 9.944984660275112631 ) ) ;
#54985 = CARTESIAN_POINT ( 'NONE',  ( 5.254748191175000471, -78.75131553099198811, -7.810174947890000219 ) ) ;
#54986 = CARTESIAN_POINT ( 'NONE',  ( -6.254307708149989153, -85.80681307385599155, -5.143738424904902296 ) ) ;
#54987 = CARTESIAN_POINT ( 'NONE',  ( -11.05562587724999979, -77.40133007910999652, -1.423986317748999975 ) ) ;
#54988 = CARTESIAN_POINT ( 'NONE',  ( 0.000000000000000000, -74.64999999999999147, 0.000000000000000000 ) ) ;
#54989 = CARTESIAN_POINT ( 'NONE',  ( -8.190711764258001182, -80.40049766303370404, 7.381016022845000357 ) ) ;
#54990 = ORIENTED_EDGE ( 'NONE', *, *, #24918, .T. ) ;
#54991 = CARTESIAN_POINT ( 'NONE',  ( -9.061228178001998756, -77.67414903538301019, -2.837532765875999896 ) ) ;
#54992 = CARTESIAN_POINT ( 'NONE',  ( -3.122542015344999644, -3.252748962127999910, 2.445576582436999935 ) ) ;
#54993 = CARTESIAN_POINT ( 'NONE',  ( 0.5473670387515998659, -76.82720197937599949, -11.20350390113000039 ) ) ;
#54994 = CARTESIAN_POINT ( 'NONE',  ( 3.915498778898000687, -79.15551720042698491, 10.25343288338999947 ) ) ;
#54995 = AXIS2_PLACEMENT_3D ( 'NONE', #8653, #45270, #26068 ) ;
#54996 = CARTESIAN_POINT ( 'NONE',  ( 9.108250977391000092, -24.87811334491999915, -8.478720681740998799 ) ) ;
#54997 = CARTESIAN_POINT ( 'NONE',  ( -1.513914364619621393E-14, -80.70000000000000284, 13.99999999999935874 ) ) ;
#54998 = FACE_OUTER_BOUND ( 'NONE', #17561, .T. ) ;
#54999 = CARTESIAN_POINT ( 'NONE',  ( -8.620934061362914846, -53.63470696640088420, -9.346030177741987188 ) ) ;
#55000 = CARTESIAN_POINT ( 'NONE',  ( 1.268589096840999852, -83.63619503318798820, -3.975014969037000689 ) ) ;
#55001 = EDGE_CURVE ( 'NONE', #56632, #36279, #8497, .T. ) ;
#55002 = CYLINDRICAL_SURFACE ( 'NONE', #11316, 9.500000000000000000 ) ;
#55003 = VECTOR ( 'NONE', #56499, 1000.000000000000000 ) ;
#55004 = CARTESIAN_POINT ( 'NONE',  ( -9.128070454880999662, -79.05712101268998993, -9.183783075634998738 ) ) ;
#55005 = B_SPLINE_SURFACE_WITH_KNOTS ( 'NONE', 3, 3, ( 
 ( #40604, #48593, #35567, #27302 ),
 ( #9021, #8422, #22883, #45335 ),
 ( #58019, #40003, #18176, #35869 ),
 ( #49769, #26139, #22292, #26419 ),
 ( #13133, #8139, #53898, #53593 ),
 ( #44441, #45041, #36169, #53012 ),
 ( #3993, #44160, #27007, #17580 ),
 ( #21995, #3707, #9310, #39716 ) ),
 .UNSPECIFIED., .F., .F., .F.,
 ( 4, 1, 1, 1, 1, 4 ),
 ( 4, 4 ),
 ( -0.01200407347463999970, 0.000000000000000000, 0.3333333333333000081, 0.6666666666667000474, 1.000000000000000000, 1.011997855551999947 ),
 ( -0.3559705542741999906, 1.355970554273999928 ),
 .UNSPECIFIED. ) ;
#55006 = CARTESIAN_POINT ( 'NONE',  ( 10.83613785003000096, -78.40712618243998122, -3.083350589994000135 ) ) ;
#55007 = CARTESIAN_POINT ( 'NONE',  ( -1.497546582071999977, -80.67509010745999376, 0.7298035716741000378 ) ) ;
#55008 = CARTESIAN_POINT ( 'NONE',  ( 0.9487295532135000542, -78.33116200998999545, 0.9179270638336999300 ) ) ;
#55009 = CARTESIAN_POINT ( 'NONE',  ( -1.570796326794885012, -79.41458333333333997, -12.00000000000000178 ) ) ;
#55010 = CARTESIAN_POINT ( 'NONE',  ( -1.388199995259592479, -81.78235798221467689, -0.5980877822880301675 ) ) ;
#55011 = DIRECTION ( 'NONE',  ( -0.6489586447330936148, -0.04890182338522946343, -0.7592504784955924624 ) ) ;
#55012 = CARTESIAN_POINT ( 'NONE',  ( -10.31421052434999908, -76.72175206120299151, 3.823226550887000030 ) ) ;
#55013 = CYLINDRICAL_SURFACE ( 'NONE', #14578, 0.5000000000000004441 ) ;
#55014 = EDGE_CURVE ( 'NONE', #30887, #9420, #26896, .T. ) ;
#55015 = CIRCLE ( 'NONE', #16377, 1.750000000000001332 ) ;
#55016 = ORIENTED_EDGE ( 'NONE', *, *, #29887, .T. ) ;
#55017 = ADVANCED_FACE ( 'NONE', ( #52909 ), #3037, .F. ) ;
#55018 = VECTOR ( 'NONE', #41067, 1000.000000000000000 ) ;
#55019 = CARTESIAN_POINT ( 'NONE',  ( 14.00000000000000000, -45.91785611817000046, 0.000000000000000000 ) ) ;
#55020 = CARTESIAN_POINT ( 'NONE',  ( -10.22609403765000025, -79.98946642284438724, -4.138687607718999573 ) ) ;
#55021 = DIRECTION ( 'NONE',  ( 0.7071067811865475727, 0.000000000000000000, -0.7071067811865475727 ) ) ;
#55022 = ORIENTED_EDGE ( 'NONE', *, *, #44348, .T. ) ;
#55023 = VERTEX_POINT ( 'NONE', #48487 ) ;
#55024 = CARTESIAN_POINT ( 'NONE',  ( -0.1948004972424999814, -81.71671722884900646, -1.404319104179999833 ) ) ;
#55025 = ORIENTED_EDGE ( 'NONE', *, *, #13441, .T. ) ;
#55026 = ORIENTED_EDGE ( 'NONE', *, *, #22404, .F. ) ;
#55027 = CARTESIAN_POINT ( 'NONE',  ( 1.200170490671999879, -17.56594298002000087, 12.43444080551000042 ) ) ;
#55028 = DIRECTION ( 'NONE',  ( 0.000000000000000000, 1.000000000000000000, 0.000000000000000000 ) ) ;
#55029 = APPLICATION_PROTOCOL_DEFINITION ( 'draft international standard', 'automotive_design', 1998, #58302 ) ;
#55030 = CARTESIAN_POINT ( 'NONE',  ( -10.25000000000000000, -87.20000000000000284, 0.000000000000000000 ) ) ;
#55031 = CARTESIAN_POINT ( 'NONE',  ( -9.943323471430000282, -78.81066001420198575, 1.256133873833999992 ) ) ;
#55032 = CARTESIAN_POINT ( 'NONE',  ( 2.003558085140010547, -78.24252397767638456, -9.030659044987556783 ) ) ;
#55033 = DIRECTION ( 'NONE',  ( -0.7071067811865475727, 0.000000000000000000, 0.7071067811865475727 ) ) ;
#55034 = ORIENTED_EDGE ( 'NONE', *, *, #6635, .T. ) ;
#55035 = ORIENTED_EDGE ( 'NONE', *, *, #21547, .T. ) ;
#55036 = CARTESIAN_POINT ( 'NONE',  ( -9.164162942852110305, -77.58929706276954619, 1.258628486501499610 ) ) ;
#55037 = CARTESIAN_POINT ( 'NONE',  ( 0.000000000000000000, -79.79999999999999716, 0.000000000000000000 ) ) ;
#55038 = CARTESIAN_POINT ( 'NONE',  ( 0.000000000000000000, -46.09579702914000165, 0.000000000000000000 ) ) ;
#55039 = CARTESIAN_POINT ( 'NONE',  ( -0.2584144828367441193, -62.02845396889886587, -12.70558781492531431 ) ) ;
#55040 = CARTESIAN_POINT ( 'NONE',  ( -7.456816947376000648, -78.71458704629999659, 6.210200510404999541 ) ) ;
#55041 = CARTESIAN_POINT ( 'NONE',  ( 0.000000000000000000, -2.949999999935999817, 0.000000000000000000 ) ) ;
#55042 = CARTESIAN_POINT ( 'NONE',  ( 3.554131759373959643, -85.81848765646206800, 1.355124311572487139 ) ) ;
#55043 = CARTESIAN_POINT ( 'NONE',  ( -3.116139353062999717, -78.31286269907000985, 12.57467468523999976 ) ) ;
#55044 = CARTESIAN_POINT ( 'NONE',  ( -0.5171309048475001280, -81.30216508874998738, -1.330821326197000110 ) ) ;
#55045 = AXIS2_PLACEMENT_3D ( 'NONE', #22086, #35662, #26807 ) ;
#55046 = CARTESIAN_POINT ( 'NONE',  ( -12.80900240957999969, -20.24634220924000161, -1.930989144707000005 ) ) ;
#55047 = CARTESIAN_POINT ( 'NONE',  ( -8.299831609958628675, -76.63730787009656353, 8.317058589932315726 ) ) ;
#55048 = CARTESIAN_POINT ( 'NONE',  ( -3.198370537365000210, -78.85393255997098549, -2.679685760545999607 ) ) ;
#55049 = CARTESIAN_POINT ( 'NONE',  ( -5.059370734576000395, -80.85404126026540439, -10.06538451635999998 ) ) ;
#55050 = CARTESIAN_POINT ( 'NONE',  ( -7.374560639699022424, -76.72708333333333997, 9.596002108778135309 ) ) ;
#55051 = AXIS2_PLACEMENT_3D ( 'NONE', #44417, #22570, #58294 ) ;
#55052 = CARTESIAN_POINT ( 'NONE',  ( -10.71846391861806858, -76.73410648036755788, -4.978960265409741126 ) ) ;
#55053 = CARTESIAN_POINT ( 'NONE',  ( -3.238543791219999690, -78.64482046129089099, 1.037289224933999998 ) ) ;
#55054 = VECTOR ( 'NONE', #12777, 1000.000000000000000 ) ;
#55055 = CARTESIAN_POINT ( 'NONE',  ( -1.182296476285000120, -78.68360863125299431, 0.6170503964917000150 ) ) ;
#55056 = CARTESIAN_POINT ( 'NONE',  ( -3.999999999993000266, -77.30000000000720206, 8.632643823722999667E-11 ) ) ;
#55057 = CARTESIAN_POINT ( 'NONE',  ( 9.345049821197974893, -79.99999999999998579, -1.982164977907467041 ) ) ;
#55058 = CARTESIAN_POINT ( 'NONE',  ( 3.171758640500000226, -3.636739359372000102, 1.479846994257000059 ) ) ;
#55059 = CARTESIAN_POINT ( 'NONE',  ( -5.869402599192000025, -78.46567021303999923, 10.46661899222999992 ) ) ;
#55060 = ORIENTED_EDGE ( 'NONE', *, *, #32602, .T. ) ;
#55061 = CARTESIAN_POINT ( 'NONE',  ( 8.666912951930401121, -61.79291380851744719, 9.019442092634875507 ) ) ;
#55062 = CARTESIAN_POINT ( 'NONE',  ( 0.5392637480172763897, -18.58467666638075855, -10.98678411023717416 ) ) ;
#55063 = CARTESIAN_POINT ( 'NONE',  ( -11.74610588145644208, -77.68890476463809591, 1.536422268980871308 ) ) ;
#55064 = CARTESIAN_POINT ( 'NONE',  ( 1.799501877793999949, -55.51082276539999327, 12.60552511008000032 ) ) ;
#55065 = CARTESIAN_POINT ( 'NONE',  ( -9.692839446179998930, -78.39782691517000046, 7.074522137259999788 ) ) ;
#55066 = CARTESIAN_POINT ( 'NONE',  ( -0.9930572065396647830, -79.48254699571987203, 10.70474299318766853 ) ) ;
#55067 = EDGE_CURVE ( 'NONE', #29230, #31908, #57551, .T. ) ;
#55068 = DIRECTION ( 'NONE',  ( 0.000000000000000000, 1.000000000000000000, 0.000000000000000000 ) ) ;
#55069 = CARTESIAN_POINT ( 'NONE',  ( 0.000000000000000000, -78.00000000000000000, 7.200000000000000178 ) ) ;
#55070 = EDGE_CURVE ( 'NONE', #55197, #40109, #37968, .T. ) ;
#55071 = CARTESIAN_POINT ( 'NONE',  ( 5.571808657063000325, -77.07548692427589287, 9.401125172057000157 ) ) ;
#55072 = AXIS2_PLACEMENT_3D ( 'NONE', #11990, #34399, #34104 ) ;
#55073 = CARTESIAN_POINT ( 'NONE',  ( -3.264115890327925484, -76.30205353464953077, -11.28874797633254090 ) ) ;
#55074 = CARTESIAN_POINT ( 'NONE',  ( -1.328207365693999886, -82.38162415354899792, -0.5054827672177999442 ) ) ;
#55075 = CARTESIAN_POINT ( 'NONE',  ( -1.480597980168999888E-14, -80.60000000000000853, 0.000000000000000000 ) ) ;
#55076 = CARTESIAN_POINT ( 'NONE',  ( 9.227078657215999513, -78.25495639208598675, -1.863387764540999969 ) ) ;
#55078 = CARTESIAN_POINT ( 'NONE',  ( -3.370206795150183510, -1.714299274284970309, -0.5568820970875701937 ) ) ;
#55077 = CARTESIAN_POINT ( 'NONE',  ( 3.640419752155000133, -83.70479011275499204, 0.9266684177237000108 ) ) ;
#55079 = FACE_OUTER_BOUND ( 'NONE', #17454, .T. ) ;
#55080 = CARTESIAN_POINT ( 'NONE',  ( 0.000000000000000000, -80.70000000003399521, 0.000000000000000000 ) ) ;
#55081 = CARTESIAN_POINT ( 'NONE',  ( 1.010832202629999843, -79.35251943783799788, -0.8478131160371998876 ) ) ;
#55082 = DIRECTION ( 'NONE',  ( 9.148990415650000800E-11, 1.000000000000000000, -8.583837524864000176E-10 ) ) ;
#55083 = CARTESIAN_POINT ( 'NONE',  ( 5.838193839761669501, -77.22291666666666288, 7.596835002782726498 ) ) ;
#55084 = CARTESIAN_POINT ( 'NONE',  ( 3.778552491321002016, -78.99318692756679638, 7.557104982642034230 ) ) ;
#55086 = EDGE_CURVE ( 'NONE', #40996, #15146, #9491, .T. ) ;
#55085 = EDGE_LOOP ( 'NONE', ( #44428, #31543, #11836, #50903 ) ) ;
#55087 = CARTESIAN_POINT ( 'NONE',  ( 7.652056849482000267, -79.52181829387700418, 9.281873293285000770 ) ) ;
#55088 = AXIS2_PLACEMENT_3D ( 'NONE', #42186, #1754, #49886 ) ;
#55089 = DIRECTION ( 'NONE',  ( 0.000000000000000000, -1.000000000000000000, 0.000000000000000000 ) ) ;
#55090 = CARTESIAN_POINT ( 'NONE',  ( 7.601397897754999633, -23.24999999688999708, 10.07627163191000008 ) ) ;
#55091 = ORIENTED_EDGE ( 'NONE', *, *, #13017, .F. ) ;
#55092 = CARTESIAN_POINT ( 'NONE',  ( 7.970414252720421366, -61.32292089011284730, 9.713036876910342343 ) ) ;
#55093 = ORIENTED_EDGE ( 'NONE', *, *, #43595, .F. ) ;
#55094 = ORIENTED_EDGE ( 'NONE', *, *, #5550, .F. ) ;
#55095 = EDGE_CURVE ( 'NONE', #9508, #27850, #29484, .T. ) ;
#55096 = VERTEX_POINT ( 'NONE', #19224 ) ;
#55097 = CARTESIAN_POINT ( 'NONE',  ( -2.503149587979999868, -81.49317640407899432, 2.513722780998999706 ) ) ;
#55098 = CARTESIAN_POINT ( 'NONE',  ( 9.500000000000000000, -79.14999999999999147, 0.000000000000000000 ) ) ;
#55099 = EDGE_CURVE ( 'NONE', #35536, #57897, #14197, .T. ) ;
#55100 = EDGE_LOOP ( 'NONE', ( #41810, #31645, #52547, #25887, #49704 ) ) ;
#55101 = CARTESIAN_POINT ( 'NONE',  ( -8.441163350029313506, -53.88348045720209001, -9.243160719890433086 ) ) ;
#55102 = ORIENTED_EDGE ( 'NONE', *, *, #52693, .F. ) ;
#55103 = DIRECTION ( 'NONE',  ( 0.000000000000000000, 1.000000000000000000, 0.000000000000000000 ) ) ;
#55104 = CARTESIAN_POINT ( 'NONE',  ( -6.766501570400897059, -77.91350543036399756, -6.956168793800119765 ) ) ;
#55105 = CARTESIAN_POINT ( 'NONE',  ( -2.398287624620532910, -78.69999999999998863, -3.977573462190750142 ) ) ;
#55106 = CARTESIAN_POINT ( 'NONE',  ( -5.051502324002999760E-14, -80.79999999999999716, 0.000000000000000000 ) ) ;
#55107 = CARTESIAN_POINT ( 'NONE',  ( -9.042832678091775378, -79.00923211523392808, -8.284631484192345852 ) ) ;
#55108 = CARTESIAN_POINT ( 'NONE',  ( -9.831705185582000794, -76.15878349074199605, 5.330239850318999828 ) ) ;
#55109 = CARTESIAN_POINT ( 'NONE',  ( -9.019414222042072993, -24.99291943955542550, 8.666941068750990240 ) ) ;
#55110 = AXIS2_PLACEMENT_3D ( 'NONE', #10628, #46364, #19478 ) ;
#55111 = CARTESIAN_POINT ( 'NONE',  ( -7.627487606591000002, -55.50221404479999876, -10.35845616725999996 ) ) ;
#55112 = CARTESIAN_POINT ( 'NONE',  ( 7.284053360365863483, -78.79718121070038706, -5.701434584557759422 ) ) ;
#55113 = CARTESIAN_POINT ( 'NONE',  ( 8.713488674121839139, -76.50807972678794044, 7.883309514286040987 ) ) ;
#55114 = CARTESIAN_POINT ( 'NONE',  ( -4.747522457205999302, -77.65358501420199389, -8.126364432035000362 ) ) ;
#55115 = CARTESIAN_POINT ( 'NONE',  ( -0.9102058945833000347, -80.56911646440499908, 0.9747214924314999696 ) ) ;
#55117 = EDGE_CURVE ( 'NONE', #54943, #31523, #16127, .T. ) ;
#55116 = CARTESIAN_POINT ( 'NONE',  ( -10.06640125953788889, -80.13353945426578662, -4.440637828395845865 ) ) ;
#55118 = CARTESIAN_POINT ( 'NONE',  ( 8.196558852201880185, -78.13742199711396097, -8.869913710989646205 ) ) ;
#55119 = CARTESIAN_POINT ( 'NONE',  ( -0.4142543683532000087, -80.24528455456798781, -3.941367037266000573 ) ) ;
#55120 = FACE_OUTER_BOUND ( 'NONE', #18881, .T. ) ;
#55121 = CARTESIAN_POINT ( 'NONE',  ( -0.1192998693168455110, -82.98315628367254249, 1.244397729618985871 ) ) ;
#55122 = CARTESIAN_POINT ( 'NONE',  ( 8.125826840328944201, -77.10625000000000284, -4.977714890814727511 ) ) ;
#55123 = CARTESIAN_POINT ( 'NONE',  ( 1.750000000000000000, -55.55000000278000272, 12.50000000000000000 ) ) ;
#55124 = CARTESIAN_POINT ( 'NONE',  ( 4.262694164919158091, -79.99999999999998579, 8.335102471465946294 ) ) ;
#55125 = CARTESIAN_POINT ( 'NONE',  ( -0.1086647425368000019, -0.9333606339641999927, 3.155427364003000168 ) ) ;
#55126 = CONICAL_SURFACE ( 'NONE', #29657, 0.6999999997694995590, 0.7853981633972997312 ) ;
#55127 = CARTESIAN_POINT ( 'NONE',  ( -1.065760231334440311, -79.78652098530383796, 1.072882827548660156 ) ) ;
#55128 = CARTESIAN_POINT ( 'NONE',  ( 7.651160336708000109, -59.56232686183999903, -10.45205658995999976 ) ) ;
#55129 = CARTESIAN_POINT ( 'NONE',  ( -2.229182494176999985, -3.114159330903000011, -2.679543090139000050 ) ) ;
#55130 = CARTESIAN_POINT ( 'NONE',  ( 12.66315196848000113, -25.17802884708999756, -0.06065366946593000325 ) ) ;
#55131 = CARTESIAN_POINT ( 'NONE',  ( 9.687205842286999768, -77.57074243306399808, -7.546775612817000045 ) ) ;
#55132 = CARTESIAN_POINT ( 'NONE',  ( -9.500000000000000000, -77.89999999999999147, 0.000000000000000000 ) ) ;
#55134 = CARTESIAN_POINT ( 'NONE',  ( -9.091539081997000338, -78.80267817997544455, 6.148815634104000338 ) ) ;
#55133 = CARTESIAN_POINT ( 'NONE',  ( 0.000000000000000000, -78.69999999999998863, 0.000000000000000000 ) ) ;
#55135 = CARTESIAN_POINT ( 'NONE',  ( -6.217012876707000757, -76.33752954592999629, -10.33620136625999919 ) ) ;
#55136 = ORIENTED_EDGE ( 'NONE', *, *, #19452, .T. ) ;
#55137 = CARTESIAN_POINT ( 'NONE',  ( -0.7466828201185000680, -84.67496544543098480, 3.892100405984999956 ) ) ;
#55138 = CARTESIAN_POINT ( 'NONE',  ( 8.646305450917001423, -80.01125923301559340, 6.688629566474999955 ) ) ;
#55139 = CARTESIAN_POINT ( 'NONE',  ( 8.331241633165971550, -78.31425648247298454, -4.019023800633488186 ) ) ;
#55140 = LINE ( 'NONE', #9992, #29910 ) ;
#55141 = CARTESIAN_POINT ( 'NONE',  ( 9.869466656387999137, -77.11227666821000071, -5.330266269891000164 ) ) ;
#55142 = CARTESIAN_POINT ( 'NONE',  ( 9.249483092228999226, -78.85084128437098627, 0.09778817195952001218 ) ) ;
#55143 = CARTESIAN_POINT ( 'NONE',  ( -7.735308924444000311, -77.38115727064098337, -5.918161214274000770 ) ) ;
#55144 = CARTESIAN_POINT ( 'NONE',  ( -4.013075295723000480, -1.312137290291999880, -0.3293376867898999971 ) ) ;
#55145 = CARTESIAN_POINT ( 'NONE',  ( 3.548349909811000291, -78.96264282632948550, 0.000000000000000000 ) ) ;
#55146 = CARTESIAN_POINT ( 'NONE',  ( 10.93439773960121641, -81.00000000000000000, -1.422938603756783049 ) ) ;
#55147 = VERTEX_POINT ( 'NONE', #36925 ) ;
#55148 = DIRECTION ( 'NONE',  ( 0.000000000000000000, -1.000000000000000000, 0.000000000000000000 ) ) ;
#55149 = FACE_OUTER_BOUND ( 'NONE', #50329, .T. ) ;
#55150 = CARTESIAN_POINT ( 'NONE',  ( -10.34138800174999950, -80.66586196297468803, 4.468208825537999473 ) ) ;
#55151 = FACE_OUTER_BOUND ( 'NONE', #48900, .T. ) ;
#55152 = ORIENTED_EDGE ( 'NONE', *, *, #8253, .T. ) ;
#55153 = EDGE_CURVE ( 'NONE', #470, #49572, #41656, .T. ) ;
#55154 = CARTESIAN_POINT ( 'NONE',  ( 0.9218200799623741393, -78.57708333333334849, -1.199500263597268690 ) ) ;
#55155 = CARTESIAN_POINT ( 'NONE',  ( -1.104817622806009147, -77.61549472473473088, -9.262197383512390303 ) ) ;
#55156 = CIRCLE ( 'NONE', #31569, 12.50000000000000000 ) ;
#55157 = DIRECTION ( 'NONE',  ( 0.9999999999999694689, -2.469235736007923508E-07, -1.232399279922961038E-12 ) ) ;
#55158 = VERTEX_POINT ( 'NONE', #86 ) ;
#55159 = CARTESIAN_POINT ( 'NONE',  ( -1.381217146163000065, -77.87480861561799372, -12.08613957309999876 ) ) ;
#55160 = CARTESIAN_POINT ( 'NONE',  ( 7.925900958036001143, -77.18054105027188427, -7.930104832517999469 ) ) ;
#55161 = AXIS2_PLACEMENT_3D ( 'NONE', #29743, #47222, #20056 ) ;
#55162 = CARTESIAN_POINT ( 'NONE',  ( 8.620921568006147950, -61.96528830388066922, -9.346042573999042702 ) ) ;
#55164 = EDGE_LOOP ( 'NONE', ( #39266, #15918, #50762, #25188 ) ) ;
#55163 = B_SPLINE_CURVE_WITH_KNOTS ( 'NONE', 3,
 ( #27208, #10102, #23380, #41390, #973, #18957 ),
 .UNSPECIFIED., .F., .F.,
 ( 4, 2, 4 ),
 ( 0.000000000000000000, 0.5000000000000001110, 1.000000000000000000 ),
 .UNSPECIFIED. ) ;
#55165 = ORIENTED_EDGE ( 'NONE', *, *, #28980, .F. ) ;
#55166 = CARTESIAN_POINT ( 'NONE',  ( -1.247931803916645821, -80.59581569326661565, 0.07626238930717134379 ) ) ;
#55167 = AXIS2_PLACEMENT_3D ( 'NONE', #19207, #28628, #19791 ) ;
#55168 = FILL_AREA_STYLE ('',( #19160 ) ) ;
#55169 = CARTESIAN_POINT ( 'NONE',  ( -9.387315177295000979, -79.86818363849698699, 2.697965643110000311 ) ) ;
#55170 = EDGE_CURVE ( 'NONE', #36279, #56632, #35858, .T. ) ;
#55171 = ORIENTED_EDGE ( 'NONE', *, *, #47117, .T. ) ;
#55172 = CARTESIAN_POINT ( 'NONE',  ( 12.77297374709000088, -54.07184670079000455, 1.476174539902000094 ) ) ;
#55173 = CARTESIAN_POINT ( 'NONE',  ( 8.274772993773998664, -24.97888614414509334, -9.689268730326240586 ) ) ;
#55174 = ORIENTED_EDGE ( 'NONE', *, *, #28890, .F. ) ;
#55175 = CARTESIAN_POINT ( 'NONE',  ( 10.46888361534042566, -80.82922105002511159, -2.813437968995440741 ) ) ;
#55176 = CARTESIAN_POINT ( 'NONE',  ( 4.001451577097999923, -77.90934805011499975, 8.339717337904000161 ) ) ;
#55177 = CARTESIAN_POINT ( 'NONE',  ( -1.099011084613188860, -80.13991461626227419, -0.5953293180670605755 ) ) ;
#55178 = CARTESIAN_POINT ( 'NONE',  ( 1.321783848197346511, -77.89322916679840603, -0.3543445508106254915 ) ) ;
#55179 = FACE_OUTER_BOUND ( 'NONE', #57772, .T. ) ;
#55180 = CARTESIAN_POINT ( 'NONE',  ( 3.751322949195571077, -86.17851881763701272, 2.724698623987952928 ) ) ;
#55181 = CARTESIAN_POINT ( 'NONE',  ( 8.281063756823000332, -76.97785287111209129, -4.978728297554999571 ) ) ;
#55182 = CARTESIAN_POINT ( 'NONE',  ( -1.330154178996141967, -78.89180944238322013, -0.7730572632364612895 ) ) ;
#55183 = CARTESIAN_POINT ( 'NONE',  ( -3.823662190920919635, -80.28020832990246447, -1.341411907055170660 ) ) ;
#55184 = ORIENTED_EDGE ( 'NONE', *, *, #23986, .F. ) ;
#55185 = CARTESIAN_POINT ( 'NONE',  ( -9.844172144369998989, -75.96608411793999949, 7.391061701651999272 ) ) ;
#55186 = CARTESIAN_POINT ( 'NONE',  ( -5.413904038987160661, -77.58333333333332860, -9.393203674808278336 ) ) ;
#55187 = EDGE_CURVE ( 'NONE', #47200, #21690, #20781, .T. ) ;
#55188 = CARTESIAN_POINT ( 'NONE',  ( -3.449594485955520984, -2.365315487544573436, -0.7067013086087599039 ) ) ;
#55189 = CARTESIAN_POINT ( 'NONE',  ( 12.49168451098999988, -18.70151115557999688, 1.667916687331000070 ) ) ;
#55190 = CARTESIAN_POINT ( 'NONE',  ( -7.766269599678000013, -78.55309459242000969, -9.491266709826000181 ) ) ;
#55191 = CARTESIAN_POINT ( 'NONE',  ( -8.987350104473000201, -77.07422532591699849, 8.369597699504998545 ) ) ;
#55192 = CYLINDRICAL_SURFACE ( 'NONE', #25161, 9.199999999999999289 ) ;
#55193 = CARTESIAN_POINT ( 'NONE',  ( 1.476721224666196930, -2.763797600519179110, -2.894638992734555938 ) ) ;
#55194 = CARTESIAN_POINT ( 'NONE',  ( -2.382985193727138462, -77.94086671676463141, 11.78025155718290229 ) ) ;
#55195 = CYLINDRICAL_SURFACE ( 'NONE', #37973, 11.75000000000000000 ) ;
#55196 = AXIS2_PLACEMENT_3D ( 'NONE', #23467, #42365, #28174 ) ;
#55197 = VERTEX_POINT ( 'NONE', #45518 ) ;
#55198 = CARTESIAN_POINT ( 'NONE',  ( -0.5525270872808000222, -82.61145401579800307, -1.233160589678000019 ) ) ;
#55199 = DIRECTION ( 'NONE',  ( 0.9936845293270585300, -0.1122098755727947705, 0.000000000000000000 ) ) ;
#55200 = CARTESIAN_POINT ( 'NONE',  ( 8.611000705966242563, -25.17488119224633536, 9.355851007297125932 ) ) ;
#55201 = CARTESIAN_POINT ( 'NONE',  ( -12.50000000000000000, -55.55000000209000177, -1.750000000000000000 ) ) ;
#55202 = CARTESIAN_POINT ( 'NONE',  ( 2.383991792491000350, -3.477118084780000284, -2.687767044859000087 ) ) ;
#55203 = CARTESIAN_POINT ( 'NONE',  ( -8.524893907337000698, -77.63827704918399775, -8.352346156331998728 ) ) ;
#55204 = CARTESIAN_POINT ( 'NONE',  ( -0.1527179957142000277, -78.08319979694698532, 9.629635879864999026 ) ) ;
#55205 = CARTESIAN_POINT ( 'NONE',  ( -9.750154851953961810, -76.15233773468979450, 6.556588445750800354 ) ) ;
#55206 = CARTESIAN_POINT ( 'NONE',  ( 1.274651354540000003, -82.80309610059499903, -0.4485964608026000167 ) ) ;
#55207 = CARTESIAN_POINT ( 'NONE',  ( -2.452652587122547523, -85.83735717367099483, 3.310696598561351234 ) ) ;
#55208 = ORIENTED_EDGE ( 'NONE', *, *, #53195, .T. ) ;
#55209 = DIRECTION ( 'NONE',  ( 0.000000000000000000, -1.000000000000000000, 0.000000000000000000 ) ) ;
#55210 = LINE ( 'NONE', #15356, #23902 ) ;
#55211 = CARTESIAN_POINT ( 'NONE',  ( -11.44417895085270942, -76.82083333333335418, -3.075537641221545826 ) ) ;
#55212 = CARTESIAN_POINT ( 'NONE',  ( 9.304500756975000897, -79.19596420577599361, -5.821536072646999571 ) ) ;
#55213 = CARTESIAN_POINT ( 'NONE',  ( -6.713100897100000353, -76.79350771435500178, 10.54932473490999989 ) ) ;
#55214 = CARTESIAN_POINT ( 'NONE',  ( 7.000000000000000000, -80.99999999999998579, 0.000000000000000000 ) ) ;
#55215 = CARTESIAN_POINT ( 'NONE',  ( 9.414496040451998837, -16.73736394015000073, -8.652369398714998994 ) ) ;
#55216 = DIRECTION ( 'NONE',  ( 2.678937178693000147E-11, -1.000000000000000000, 2.678911359553000079E-11 ) ) ;
#55217 = ORIENTED_EDGE ( 'NONE', *, *, #35119, .T. ) ;
#55218 = CARTESIAN_POINT ( 'NONE',  ( 7.840078887343000069, -78.96286685420099616, -8.084993976410000727 ) ) ;
#55219 = CYLINDRICAL_SURFACE ( 'NONE', #19204, 11.00000000000000000 ) ;
#55220 = CARTESIAN_POINT ( 'NONE',  ( 0.000000000000000000, -81.99999999999998579, 0.000000000000000000 ) ) ;
#55221 = CARTESIAN_POINT ( 'NONE',  ( -3.893811115504242970, -78.43735716284257364, 2.200139673516985361 ) ) ;
#55222 = CARTESIAN_POINT ( 'NONE',  ( 11.72872471648087966, -77.68377190531555243, -2.898477863863423654 ) ) ;
#55223 = ADVANCED_FACE ( 'NONE', ( #41074 ), #55681, .F. ) ;
#55224 = CARTESIAN_POINT ( 'NONE',  ( 11.75000000000000000, -76.45000000000000284, 0.000000000000000000 ) ) ;
#55225 = EDGE_CURVE ( 'NONE', #25256, #10013, #15135, .T. ) ;
#55226 = CARTESIAN_POINT ( 'NONE',  ( -5.638272052137092594, -76.99999999999998579, -7.602424392853662560 ) ) ;
#55227 = CARTESIAN_POINT ( 'NONE',  ( -3.804208684430999909, -3.250482064474000232, -0.1186911049137999996 ) ) ;
#55228 = CARTESIAN_POINT ( 'NONE',  ( -0.8004101649314999678, -77.65262252499999818, -1.034513833287000084 ) ) ;
#55229 = CARTESIAN_POINT ( 'NONE',  ( 1.407171709420391936, -79.36458333333331439, 10.75000000000000178 ) ) ;
#55230 = B_SPLINE_SURFACE_WITH_KNOTS ( 'NONE', 3, 3, ( 
 ( #19136, #45430, #18562, #1151 ),
 ( #27396, #36841, #863, #5264 ),
 ( #23845, #4971, #18848, #32398 ),
 ( #22980, #36554, #50442, #41862 ),
 ( #48055, #51893, #51611, #38003 ),
 ( #11451, #29430, #6425, #10876 ),
 ( #47189, #11168, #42742, #1728 ),
 ( #56603, #29143, #7008, #15283 ),
 ( #12020, #42454, #29714, #6721 ),
 ( #2592, #43031, #16451, #11736 ),
 ( #24729, #2305, #34432, #52462 ) ),
 .UNSPECIFIED., .F., .F., .F.,
 ( 4, 1, 1, 1, 1, 1, 1, 1, 4 ),
 ( 4, 4 ),
 ( -0.01994574723506000249, 0.000000000000000000, 0.1666666666667000196, 0.3333333333333000081, 0.5000000000000000000, 0.6666666666667000474, 0.8333333333333000637, 1.000000000000000000, 1.020511277925000071 ),
 ( -0.3582002740308999900, 1.358574366093000085 ),
 .UNSPECIFIED. ) ;
#55231 = CARTESIAN_POINT ( 'NONE',  ( -4.277805800101380562, -79.04324219184334765, -10.10782847103924631 ) ) ;
#55232 = AXIS2_PLACEMENT_3D ( 'NONE', #46887, #6124, #33848 ) ;
#55233 = CARTESIAN_POINT ( 'NONE',  ( 8.485281374238999419, -59.94999999967000548, 8.485281374238999419 ) ) ;
#55234 = ORIENTED_EDGE ( 'NONE', *, *, #40266, .F. ) ;
#55235 = EDGE_CURVE ( 'NONE', #57298, #52316, #36638, .T. ) ;
#55236 = ORIENTED_EDGE ( 'NONE', *, *, #34450, .T. ) ;
#55237 = CARTESIAN_POINT ( 'NONE',  ( 2.078959492154019095, -77.75750000000002160, 9.312872062229846648 ) ) ;
#55238 = CARTESIAN_POINT ( 'NONE',  ( 6.023077783880060210, -78.77250036845040881, -8.904115691191277548 ) ) ;
#55239 = ORIENTED_EDGE ( 'NONE', *, *, #33110, .T. ) ;
#55240 = CARTESIAN_POINT ( 'NONE',  ( 11.01994305158000209, -76.48636737507854377, -1.906499110313000234 ) ) ;
#55241 = CARTESIAN_POINT ( 'NONE',  ( -0.2605555034656120705, -82.84322918252360068, 3.400557700907242520 ) ) ;
#55242 = AXIS2_PLACEMENT_3D ( 'NONE', #1274, #18395, #13657 ) ;
#55243 = CARTESIAN_POINT ( 'NONE',  ( -1.199500263597274241, -80.34791666666667709, 0.9218200799623669228 ) ) ;
#55244 = VECTOR ( 'NONE', #27180, 1000.000000000000000 ) ;
#55245 = CARTESIAN_POINT ( 'NONE',  ( 7.645391636782999711, -60.01530450324999322, 10.18949673577000148 ) ) ;
#55246 = DIRECTION ( 'NONE',  ( 0.000000000000000000, 0.000000000000000000, -1.000000000000000000 ) ) ;
#55247 = CARTESIAN_POINT ( 'NONE',  ( -6.778077112046531738, -78.12704699457141544, -9.878140615074055830 ) ) ;
#55248 = CARTESIAN_POINT ( 'NONE',  ( 4.782478426736999744, -79.60605421298700435, 10.14623135401999932 ) ) ;
#55249 = ORIENTED_EDGE ( 'NONE', *, *, #4266, .F. ) ;
#55250 = CARTESIAN_POINT ( 'NONE',  ( 0.000000000000000000, -74.70999999999999375, 0.000000000000000000 ) ) ;
#55251 = ORIENTED_EDGE ( 'NONE', *, *, #20760, .F. ) ;
#55252 = CARTESIAN_POINT ( 'NONE',  ( 8.234955035280039581, -77.38774562065144380, 4.212665045149399212 ) ) ;
#55253 = DIRECTION ( 'NONE',  ( -0.7071067811865474617, 0.000000000000000000, -0.7071067811865474617 ) ) ;
#55254 = CARTESIAN_POINT ( 'NONE',  ( 1.136236858042999787, -78.30482622072879906, 1.147248764840999913 ) ) ;
#55255 = CARTESIAN_POINT ( 'NONE',  ( -10.09635500655283735, -18.47627834136018166, -7.644087038114626864 ) ) ;
#55256 = CARTESIAN_POINT ( 'NONE',  ( 10.35453599130000057, -76.75783510652000530, -6.064947188958000446 ) ) ;
#55257 = CARTESIAN_POINT ( 'NONE',  ( 0.4102083068199999794, -78.41566823357999283, -1.574926093281000083 ) ) ;
#55258 = CARTESIAN_POINT ( 'NONE',  ( -1.405028834994999976, -82.01182046129099490, -3.928416441703999507 ) ) ;
#55259 = CARTESIAN_POINT ( 'NONE',  ( -0.8591865374099513231, -79.16499716410996257, -0.9081973555077933469 ) ) ;
#55260 = CARTESIAN_POINT ( 'NONE',  ( -0.5177219211888000050, -79.05041914309698825, -10.92793577709999830 ) ) ;
#55261 = CARTESIAN_POINT ( 'NONE',  ( -9.029867227896000159, -25.33262194290999858, -9.038867509618000895 ) ) ;
#55262 = CARTESIAN_POINT ( 'NONE',  ( 12.49306752631999906, -55.51943307300000185, -1.667917367010000040 ) ) ;
#55263 = CARTESIAN_POINT ( 'NONE',  ( 1.941413306027000019, -82.70557145154198508, 2.969078086012999940 ) ) ;
#55264 = ORIENTED_EDGE ( 'NONE', *, *, #1014, .F. ) ;
#55265 = CARTESIAN_POINT ( 'NONE',  ( 3.140974612311376646, -79.54583333333333428, -11.68767212001978706 ) ) ;
#55266 = CARTESIAN_POINT ( 'NONE',  ( -0.5171309048475001280, -81.48884839998999041, -1.330821326197000110 ) ) ;
#55267 = CARTESIAN_POINT ( 'NONE',  ( 5.679944191426311129, -77.93085335426356153, 9.133896504759128732 ) ) ;
#55268 = CARTESIAN_POINT ( 'NONE',  ( 6.917788961650999546, -78.74009410830100819, -9.780606322222999083 ) ) ;
#55269 = CARTESIAN_POINT ( 'NONE',  ( -7.660411364622000008, -18.80826384815000196, 10.01752038683000023 ) ) ;
#55270 = B_SPLINE_CURVE_WITH_KNOTS ( 'NONE', 3,
 ( #20589, #17021, #7584, #7295, #3729, #53038, #30584, #16449, #25297, #12585 ),
 .UNSPECIFIED., .F., .F.,
 ( 4, 2, 2, 2, 4 ),
 ( 0.000000000000000000, 0.5000000000000012212, 0.6250000000000035527, 0.7500000000000057732, 1.000000000000000000 ),
 .UNSPECIFIED. ) ;
#55271 = EDGE_CURVE ( 'NONE', #31290, #47045, #12310, .T. ) ;
#55272 = CARTESIAN_POINT ( 'NONE',  ( 1.201075292024272434, -77.97281434202166395, -0.4271495449073431372 ) ) ;
#55273 = CARTESIAN_POINT ( 'NONE',  ( -0.07478521273582763862, -3.373346085622628276, -3.521909467481564082 ) ) ;
#55274 = CARTESIAN_POINT ( 'NONE',  ( 10.44390837562477969, -80.86943310474272550, 2.545984649820042023 ) ) ;
#55275 = CARTESIAN_POINT ( 'NONE',  ( 0.000000000000000000, -92.13603921945998820, 0.000000000000000000 ) ) ;
#55276 = CARTESIAN_POINT ( 'NONE',  ( -6.843851216451987796, -85.94828561723799965, -5.628597459398892333 ) ) ;
#55277 = CARTESIAN_POINT ( 'NONE',  ( -10.98551332331999930, -76.95156662648800250, 1.010146990136999934 ) ) ;
#55278 = CARTESIAN_POINT ( 'NONE',  ( -9.801255020792000394, -76.59853460670321113, 7.399866681860999940 ) ) ;
#55279 = CARTESIAN_POINT ( 'NONE',  ( 5.459723135333999444, -80.22537985460630239, 9.711247138783999588 ) ) ;
#55280 = ORIENTED_EDGE ( 'NONE', *, *, #38805, .F. ) ;
#55281 = CARTESIAN_POINT ( 'NONE',  ( -7.264520526674997924, -77.70567403538302642, -6.114261184555999762 ) ) ;
#55282 = CARTESIAN_POINT ( 'NONE',  ( -8.090910852015777976, -55.25278097498932084, 7.452378523309688418 ) ) ;
#55283 = APPLICATION_CONTEXT ( 'automotive_design' ) ;
#55284 = CARTESIAN_POINT ( 'NONE',  ( -11.12496554189999998, -77.27629933467800072, -1.432917402686000097 ) ) ;
#55285 = CARTESIAN_POINT ( 'NONE',  ( 4.038786804788999873, -79.46453309808698862, -10.20549938643999965 ) ) ;
#55286 = CARTESIAN_POINT ( 'NONE',  ( 6.536160117426359051, -80.22377045582020116, 8.743586084475110098 ) ) ;
#55287 = CARTESIAN_POINT ( 'NONE',  ( -14.00000000000000000, -32.88214388149999934, 1.168298652233000123E-11 ) ) ;
#55288 = CARTESIAN_POINT ( 'NONE',  ( -9.238576773750232007, -78.54311845634511258, -5.559101997765075964 ) ) ;
#55289 = DIRECTION ( 'NONE',  ( 0.000000000000000000, -1.000000000000000000, 0.000000000000000000 ) ) ;
#55290 = AXIS2_PLACEMENT_3D ( 'NONE', #55573, #47617, #33992 ) ;
#55291 = CARTESIAN_POINT ( 'NONE',  ( 3.471920961466000044, -82.30717953870899350, -1.985170305869999874 ) ) ;
#55292 = CARTESIAN_POINT ( 'NONE',  ( 1.460959015002474048, -79.72916666666668561, -0.3926218265389178064 ) ) ;
#55293 = AXIS2_PLACEMENT_3D ( 'NONE', #12854, #54197, #36181 ) ;
#55294 = VECTOR ( 'NONE', #53768, 1000.000000000000000 ) ;
#55295 = CARTESIAN_POINT ( 'NONE',  ( 10.13402152808999901, -55.07694524364999467, -7.647754144006999155 ) ) ;
#55296 = CIRCLE ( 'NONE', #10085, 1.250000000000000444 ) ;
#55297 = CARTESIAN_POINT ( 'NONE',  ( 8.538884422081000736, -77.98574086744999079, 7.349585687664999867 ) ) ;
#55298 = EDGE_CURVE ( 'NONE', #56133, #1101, #49270, .T. ) ;
#55299 = CARTESIAN_POINT ( 'NONE',  ( -0.9131908197385000259, -81.46327815847000409, -1.254418330386999791 ) ) ;
#55300 = CARTESIAN_POINT ( 'NONE',  ( 0.000000000000000000, -76.29999999999999716, 0.000000000000000000 ) ) ;
#55301 = CARTESIAN_POINT ( 'NONE',  ( -1.980610890454873374, -60.32073889447752890, 12.74374574610012800 ) ) ;
#55302 = CARTESIAN_POINT ( 'NONE',  ( 1.270052417142802925, -81.95442635671317078, -0.8198608233724109517 ) ) ;
#55303 = LINE ( 'NONE', #14849, #43126 ) ;
#55304 = CARTESIAN_POINT ( 'NONE',  ( -10.72781790777320765, -80.10681046886573142, -0.8882985175872072370 ) ) ;
#55305 = CARTESIAN_POINT ( 'NONE',  ( 4.784380313523556083, -77.96666666666666856, -8.300970689365444244 ) ) ;
#55306 = CARTESIAN_POINT ( 'NONE',  ( 1.500000000000000000, -78.14999999999999147, 0.000000000000000000 ) ) ;
#55307 = ORIENTED_EDGE ( 'NONE', *, *, #18223, .F. ) ;
#55308 = CARTESIAN_POINT ( 'NONE',  ( -0.4780979534308362200, -81.69389049006093728, -1.154869708129174111 ) ) ;
#55309 = CARTESIAN_POINT ( 'NONE',  ( 3.315825420378000210, -79.60815762081898583, -10.52174111842000137 ) ) ;
#55310 = CARTESIAN_POINT ( 'NONE',  ( 2.799999998984000094, -78.69999999898398357, -6.819611318389000073E-10 ) ) ;
#55311 = ORIENTED_EDGE ( 'NONE', *, *, #35956, .F. ) ;
#55312 = ADVANCED_FACE ( 'NONE', ( #38670 ), #19871, .T. ) ;
#55313 = ORIENTED_EDGE ( 'NONE', *, *, #48488, .T. ) ;
#55314 = CARTESIAN_POINT ( 'NONE',  ( -0.8736801639325000313, -80.67485213784600262, -1.116492654993999967 ) ) ;
#55315 = EDGE_CURVE ( 'NONE', #37657, #49174, #48144, .T. ) ;
#55316 = ORIENTED_EDGE ( 'NONE', *, *, #16724, .T. ) ;
#55317 = EDGE_LOOP ( 'NONE', ( #45343, #2545, #37945, #6419 ) ) ;
#55318 = CARTESIAN_POINT ( 'NONE',  ( -1.477284502223000118, -17.27368499703000282, 12.77254812468999923 ) ) ;
#55319 = CARTESIAN_POINT ( 'NONE',  ( -9.998734510692901978, -54.87263061026161637, -7.709128441167184320 ) ) ;
#55320 = APPLICATION_PROTOCOL_DEFINITION ( 'draft international standard', 'automotive_design', 1998, #34138 ) ;
#55321 = CARTESIAN_POINT ( 'NONE',  ( 3.430463647390288529, -79.47083332752710305, 0.3047064478928679931 ) ) ;
#55322 = CARTESIAN_POINT ( 'NONE',  ( -7.837473280028000033, -78.76711001420200375, 6.246724465767999668 ) ) ;
#55323 = CARTESIAN_POINT ( 'NONE',  ( 3.667343776274157197, -78.25747830790810156, -8.492070081455974417 ) ) ;
#55324 = CARTESIAN_POINT ( 'NONE',  ( -9.369164850722000892, -18.75000000000000000, -7.601397897754999633 ) ) ;
#55325 = ORIENTED_EDGE ( 'NONE', *, *, #21861, .T. ) ;
#55326 = VERTEX_POINT ( 'NONE', #56401 ) ;
#55327 = CARTESIAN_POINT ( 'NONE',  ( -9.249917423436453845, -77.59781344625758948, 0.2701611356223029836 ) ) ;
#55328 = CARTESIAN_POINT ( 'NONE',  ( -9.404538367151713985, -76.95366911081998751, -7.521839627126676753 ) ) ;
#55329 = CARTESIAN_POINT ( 'NONE',  ( 10.36935812844000004, -78.17876026662598576, -2.835297515976000327 ) ) ;
#55330 = AXIS2_PLACEMENT_3D ( 'NONE', #57391, #21941, #34931 ) ;
#55331 = CARTESIAN_POINT ( 'NONE',  ( -0.3664097479087854992, -17.02809982499438135, 12.50575740043635697 ) ) ;
#55332 = CARTESIAN_POINT ( 'NONE',  ( 9.367484565636001292, -78.99882533758999159, -2.533990228858999938 ) ) ;
#55333 = EDGE_CURVE ( 'NONE', #3745, #30361, #34226, .T. ) ;
#55334 = CARTESIAN_POINT ( 'NONE',  ( -8.190859204290999784, -55.64999999967000122, 7.342331066867000544 ) ) ;
#55335 = CARTESIAN_POINT ( 'NONE',  ( 2.736345944437820421, -85.86944366957823149, 2.769272514814725028 ) ) ;
#55336 = AXIS2_PLACEMENT_3D ( 'NONE', #7785, #7496, #21925 ) ;
#55337 = CARTESIAN_POINT ( 'NONE',  ( -5.508096857961803927, -77.38721230508248539, -10.70907476296403793 ) ) ;
#55338 = CARTESIAN_POINT ( 'NONE',  ( -0.7224186015757000368, -79.15443682768999167, -0.9790252285018000711 ) ) ;
#55339 = CARTESIAN_POINT ( 'NONE',  ( -7.931488639841374422, -77.09554693750341414, -5.131895770657950884 ) ) ;
#55340 = CIRCLE ( 'NONE', #38385, 3.399999999999999911 ) ;
#55341 = CARTESIAN_POINT ( 'NONE',  ( 0.5577297053749999955, -79.16348572639719805, -4.137458692512000269 ) ) ;
#55342 = VECTOR ( 'NONE', #40047, 1000.000000000000114 ) ;
#55343 = CARTESIAN_POINT ( 'NONE',  ( 8.828526701892000617, -80.46277134221820404, -6.997593314318000246 ) ) ;
#55344 = CARTESIAN_POINT ( 'NONE',  ( 6.458817137649000450, -79.25746001420199605, -6.573457973844999636 ) ) ;
#55345 = CARTESIAN_POINT ( 'NONE',  ( -5.413682991573638859, -76.68346113739394809, -9.392790915597688084 ) ) ;
#55346 = CARTESIAN_POINT ( 'NONE',  ( -3.481077770090000190, -78.76507046129088963, -0.6828731366740999897 ) ) ;
#55347 = EDGE_CURVE ( 'NONE', #31098, #353, #26656, .T. ) ;
#55349 = CARTESIAN_POINT ( 'NONE',  ( -0.5409299486741000473, -79.08634822410400034, 1.218996123443000013 ) ) ;
#55348 = CARTESIAN_POINT ( 'NONE',  ( -1.250000000000000000, -55.54999999966999980, 12.50000000000000000 ) ) ;
#55350 = LINE ( 'NONE', #55056, #27003 ) ;
#55351 = CARTESIAN_POINT ( 'NONE',  ( 0.000000000000000000, -74.70999999999999375, 0.000000000000000000 ) ) ;
#55352 = CARTESIAN_POINT ( 'NONE',  ( 0.000000000000000000, -13.07071424677999971, 0.000000000000000000 ) ) ;
#55353 = ADVANCED_FACE ( 'NONE', ( #33657, #42250 ), #6804, .T. ) ;
#55354 = VERTEX_POINT ( 'NONE', #41950 ) ;
#55355 = CARTESIAN_POINT ( 'NONE',  ( -1.148784730228095574, -3.499999999999998668, -3.235125723717343860 ) ) ;
#55356 = CARTESIAN_POINT ( 'NONE',  ( -6.267465111053000193, -78.04198670514499270, 9.561428071649999083 ) ) ;
#55357 = CARTESIAN_POINT ( 'NONE',  ( -3.047192285975917070, -77.59416509716808719, 11.37765756762788349 ) ) ;
#55358 = B_SPLINE_CURVE_WITH_KNOTS ( 'NONE', 3,
 ( #52863, #49230, #36521, #22658, #45105, #26772, #44802, #8782, #4354, #40667, #32083, #49829, #39277, #9377, #13785, #258, #14086, #36229, #552, #57287 ),
 .UNSPECIFIED., .F., .F.,
 ( 4, 2, 2, 2, 2, 2, 2, 2, 2, 4 ),
 ( 0.000000000000000000, 0.06250000000000004163, 0.1250000000000000833, 0.2500000000000001110, 0.3750000000000001665, 0.5000000000000002220, 0.6250000000000002220, 0.7500000000000001110, 0.8750000000000001110, 1.000000000000000000 ),
 .UNSPECIFIED. ) ;
#55359 = CARTESIAN_POINT ( 'NONE',  ( 1.799490220168999954, -59.57129148919000272, 12.64502302236999931 ) ) ;
#55360 = CARTESIAN_POINT ( 'NONE',  ( -3.129814719915999799, -78.34232227420999095, 12.62985940900000159 ) ) ;
#55361 = CARTESIAN_POINT ( 'NONE',  ( 9.898445906460613841, -79.38214623308790863, 4.225145221008577145 ) ) ;
#55362 = DIRECTION ( 'NONE',  ( -1.000000000000000000, 0.000000000000000000, 0.000000000000000000 ) ) ;
#55363 = LINE ( 'NONE', #54782, #11797 ) ;
#55364 = CARTESIAN_POINT ( 'NONE',  ( -9.409947959002000317, -77.72560390012598930, -6.209574706611999950 ) ) ;
#55365 = CARTESIAN_POINT ( 'NONE',  ( -4.499009195832593733, -76.29327141761633868, -10.85425454283228319 ) ) ;
#55366 = CARTESIAN_POINT ( 'NONE',  ( -0.7686600910219999472, -81.77030236145701281, 1.295400560101000131 ) ) ;
#55367 = CARTESIAN_POINT ( 'NONE',  ( -4.799999999999999822, -74.99999999999998579, 0.000000000000000000 ) ) ;
#55368 = CARTESIAN_POINT ( 'NONE',  ( 4.061470846528000500, -78.68131382901999871, -8.492093326754000415 ) ) ;
#55370 = CARTESIAN_POINT ( 'NONE',  ( -3.249661007175000282, -0.8020864414130000064, 2.357191814219000037 ) ) ;
#55369 = CARTESIAN_POINT ( 'NONE',  ( 1.160729942571000040, -83.94529094328899532, 3.572684750812999965 ) ) ;
#55371 = CARTESIAN_POINT ( 'NONE',  ( -8.630067035710000667, -79.60524805011499438, -4.100810385846999750 ) ) ;
#55372 = CARTESIAN_POINT ( 'NONE',  ( -0.1636246173744673738, -82.61458333333330017, -1.249999999999999778 ) ) ;
#55373 = PLANE ( 'NONE',  #15137 ) ;
#55374 = DIRECTION ( 'NONE',  ( -1.205798306660979359E-11, 1.868137356545963916E-07, 0.9999999999999824585 ) ) ;
#55375 = CARTESIAN_POINT ( 'NONE',  ( -8.300970689365467337, -77.35833333333330586, 4.784380313523513450 ) ) ;
#55376 = ORIENTED_EDGE ( 'NONE', *, *, #18928, .F. ) ;
#55377 = CARTESIAN_POINT ( 'NONE',  ( -6.309004353333000026, -79.21496069382000371, -10.24224633278999796 ) ) ;
#55378 = DIRECTION ( 'NONE',  ( 1.000000000000000000, 0.000000000000000000, 0.000000000000000000 ) ) ;
#55379 = DIRECTION ( 'NONE',  ( 0.000000000000000000, -1.000000000000000000, 0.000000000000000000 ) ) ;
#55380 = AXIS2_PLACEMENT_3D ( 'NONE', #1597, #55021, #55606 ) ;
#55381 = ORIENTED_EDGE ( 'NONE', *, *, #47049, .T. ) ;
#55382 = CARTESIAN_POINT ( 'NONE',  ( 11.83900414546000057, -78.36332874153899297, -1.507807444711000144 ) ) ;
#55383 = CIRCLE ( 'NONE', #44050, 1.000000000000000000 ) ;
#55384 = EDGE_CURVE ( 'NONE', #13401, #52629, #16022, .T. ) ;
#55385 = EDGE_LOOP ( 'NONE', ( #27043, #56974, #24863, #4577 ) ) ;
#55386 = VERTEX_POINT ( 'NONE', #28647 ) ;
#55387 = ORIENTED_EDGE ( 'NONE', *, *, #25293, .T. ) ;
#55388 = CARTESIAN_POINT ( 'NONE',  ( -0.3708642736603999790, -80.53743850270798532, -3.527609609179999772 ) ) ;
#55389 = CARTESIAN_POINT ( 'NONE',  ( -12.76303204294000082, -18.73514849292999784, -1.980584515756000030 ) ) ;
#55390 = ORIENTED_EDGE ( 'NONE', *, *, #27165, .F. ) ;
#55391 = CARTESIAN_POINT ( 'NONE',  ( 1.155591953334705657, -82.81890755821275718, -0.4764985287334481123 ) ) ;
#55392 = CARTESIAN_POINT ( 'NONE',  ( 0.9406238316005999245, -2.408324159475999870, 3.268731539939000008 ) ) ;
#55393 = ORIENTED_EDGE ( 'NONE', *, *, #20325, .F. ) ;
#55394 = CARTESIAN_POINT ( 'NONE',  ( 10.75000000000000355, -80.73958333333332860, -1.407171709420407035 ) ) ;
#55395 = CARTESIAN_POINT ( 'NONE',  ( -7.707293733352901022, -77.40187650604293879, -5.896727239374860652 ) ) ;
#55396 = CARTESIAN_POINT ( 'NONE',  ( -7.679961486493839473, -79.79999999999998295, -9.071626512970588863 ) ) ;
#55397 = DIRECTION ( 'NONE',  ( -1.000000000000000000, 0.000000000000000000, 0.000000000000000000 ) ) ;
#55398 = CARTESIAN_POINT ( 'NONE',  ( -7.766498253946735097, -78.52063990793401160, -9.491546151406783594 ) ) ;
#55399 = EDGE_CURVE ( 'NONE', #35908, #27991, #37120, .T. ) ;
#55400 = CARTESIAN_POINT ( 'NONE',  ( 7.405962610586998451, -77.44409050277675988, -6.270759699041999369 ) ) ;
#55401 = CARTESIAN_POINT ( 'NONE',  ( -1.963210506780999953, -76.30927514267598610, -11.00998129987999974 ) ) ;
#55402 = CARTESIAN_POINT ( 'NONE',  ( 8.624362245272223504, -79.63790916909928796, 4.474991579895456262 ) ) ;
#55403 = ADVANCED_FACE ( 'NONE', ( #55526 ), #42537, .T. ) ;
#55404 = CARTESIAN_POINT ( 'NONE',  ( 1.250000000000000000, -81.24999999999998579, 0.000000000000000000 ) ) ;
#55405 = B_SPLINE_CURVE_WITH_KNOTS ( 'NONE', 3,
 ( #45560, #36678, #54981, #44669, #45856, #22220 ),
 .UNSPECIFIED., .F., .F.,
 ( 4, 2, 4 ),
 ( 0.000000000000000000, 0.5000000000000000000, 1.000000000000000000 ),
 .UNSPECIFIED. ) ;
#55406 = CARTESIAN_POINT ( 'NONE',  ( -7.668949790007999923, -56.02870851050000311, -10.21381326472999795 ) ) ;
#55407 = CARTESIAN_POINT ( 'NONE',  ( -7.804500157903205171, -78.64526517801122907, -4.965041426151914905 ) ) ;
#55408 = CARTESIAN_POINT ( 'NONE',  ( -8.899304630592000720, -77.59703501420199245, -3.062539053741000217 ) ) ;
#55409 = CARTESIAN_POINT ( 'NONE',  ( 1.021809889922000059, -79.32880087987798845, -0.8570204080543000202 ) ) ;
#55410 = CARTESIAN_POINT ( 'NONE',  ( -3.399186938124999724, -80.19999999999998863, -10.46162167925000119 ) ) ;
#55411 = CARTESIAN_POINT ( 'NONE',  ( -12.65375411750999923, -57.05022861049000227, -1.750000000000000000 ) ) ;
#55412 = CARTESIAN_POINT ( 'NONE',  ( 3.110986529608999795, -80.48578455456799929, -2.455146353428000250 ) ) ;
#55413 = CARTESIAN_POINT ( 'NONE',  ( -10.24862125074130859, -78.07571521542081427, 3.248992843890492033 ) ) ;
#55414 = CARTESIAN_POINT ( 'NONE',  ( 1.030642090993115989, -82.89809790103859655, 0.7070660955623684352 ) ) ;
#55415 = CARTESIAN_POINT ( 'NONE',  ( -1.980584515752000119, -60.06485146591000301, 12.76303204605000197 ) ) ;
#55416 = CARTESIAN_POINT ( 'NONE',  ( -12.79999999996999982, -0.1000000000339999751, 4.310442092940000344E-10 ) ) ;
#55417 = CARTESIAN_POINT ( 'NONE',  ( -0.9058031679606026731, -82.18505110562824711, 0.9672994567659488618 ) ) ;
#55418 = CARTESIAN_POINT ( 'NONE',  ( -10.07979664880000037, -76.97175206120299151, 3.736335038366999761 ) ) ;
#55419 = ADVANCED_FACE ( 'NONE', ( #6216 ), #19811, .T. ) ;
#55420 = FACE_OUTER_BOUND ( 'NONE', #42025, .T. ) ;
#55421 = CARTESIAN_POINT ( 'NONE',  ( 12.55433072264032823, -23.38725213725910024, 1.749897784985354532 ) ) ;
#55422 = AXIS2_PLACEMENT_3D ( 'NONE', #46699, #6513, #15075 ) ;
#55423 = CARTESIAN_POINT ( 'NONE',  ( 12.71466317164898285, -24.13795986741620325, -1.778778223976646755 ) ) ;
#55424 = CARTESIAN_POINT ( 'NONE',  ( -1.288488638074000159, -24.53564939367999997, -12.54709296483000003 ) ) ;
#55425 = DIRECTION ( 'NONE',  ( 0.000000000000000000, -0.7071067811865475727, -0.7071067811865475727 ) ) ;
#55426 = CARTESIAN_POINT ( 'NONE',  ( 4.598371993787000456, -78.67404415034599197, -8.567308531191999421 ) ) ;
#55427 = CARTESIAN_POINT ( 'NONE',  ( 12.48409101788000086, -23.36970703835000052, 1.669510252625999946 ) ) ;
#55428 = CARTESIAN_POINT ( 'NONE',  ( -1.249999999999999778, -80.51041666666664298, -0.1636246173744686228 ) ) ;
#55429 = CARTESIAN_POINT ( 'NONE',  ( 8.118221194901000359, -77.19093201713099006, 9.213591238522999660 ) ) ;
#55430 = CARTESIAN_POINT ( 'NONE',  ( 0.000000000000000000, -74.64999999999999147, 0.000000000000000000 ) ) ;
#55431 = B_SPLINE_CURVE_WITH_KNOTS ( 'NONE', 3,
 ( #28793, #55674, #19371, #24383, #46255, #14634 ),
 .UNSPECIFIED., .F., .F.,
 ( 4, 2, 4 ),
 ( 0.000000000000000000, 0.5000000000000000000, 1.000000000000000000 ),
 .UNSPECIFIED. ) ;
#55432 = CARTESIAN_POINT ( 'NONE',  ( -6.405050160242000246, -78.77458582564257483, 8.912875463421000788 ) ) ;
#55433 = CARTESIAN_POINT ( 'NONE',  ( -1.086153235740000111, -76.28645333715999755, -12.16362709103000128 ) ) ;
#55434 = ORIENTED_EDGE ( 'NONE', *, *, #42254, .T. ) ;
#55435 = CARTESIAN_POINT ( 'NONE',  ( 3.997189897728999686, -84.07757450217398798, -1.039700163341999994 ) ) ;
#55436 = ADVANCED_FACE ( 'NONE', ( #15376 ), #54229, .F. ) ;
#55437 = CARTESIAN_POINT ( 'NONE',  ( 7.587302191891999392, -79.95518973060389101, 7.873108652756999781 ) ) ;
#55438 = B_SPLINE_CURVE_WITH_KNOTS ( 'NONE', 3,
 ( #21079, #16658, #15788, #34351 ),
 .UNSPECIFIED., .F., .F.,
 ( 4, 4 ),
 ( 0.000000000000000000, 1.000000000000000000 ),
 .UNSPECIFIED. ) ;
#55439 = CARTESIAN_POINT ( 'NONE',  ( 8.998106893723814892, -78.33155866549604696, -2.144391086070803532 ) ) ;
#55440 = CARTESIAN_POINT ( 'NONE',  ( 0.1963495408493638184, -81.63541666666668561, -1.499999999999999778 ) ) ;
#55441 = CARTESIAN_POINT ( 'NONE',  ( -11.12496554189999998, -77.41187644123000666, -1.432917402686000097 ) ) ;
#55442 = DIRECTION ( 'NONE',  ( 0.7071067811865475727, 0.000000000000000000, -0.7071067811865475727 ) ) ;
#55443 = CARTESIAN_POINT ( 'NONE',  ( 5.376158796547000129, -79.06519127177598705, -7.990628517496999983 ) ) ;
#55444 = CARTESIAN_POINT ( 'NONE',  ( -0.7572724432162000197, -83.30137326488198823, 1.483977110291999857 ) ) ;
#55445 = DIRECTION ( 'NONE',  ( -1.000000000000000000, 0.000000000000000000, 0.000000000000000000 ) ) ;
#55446 = CARTESIAN_POINT ( 'NONE',  ( -1.799502287691000069, -55.49283319101999723, 12.60413670417000098 ) ) ;
#55447 = ORIENTED_EDGE ( 'NONE', *, *, #6663, .F. ) ;
#55448 = DIRECTION ( 'NONE',  ( 0.000000000000000000, -1.000000000000000000, 0.000000000000000000 ) ) ;
#55449 = CARTESIAN_POINT ( 'NONE',  ( -4.454457568640999732, -80.60566659096738817, 10.34731867136000005 ) ) ;
#55450 = CARTESIAN_POINT ( 'NONE',  ( 14.00000000000000000, -45.91785611817000046, 0.000000000000000000 ) ) ;
#55451 = ORIENTED_EDGE ( 'NONE', *, *, #40173, .T. ) ;
#55452 = CARTESIAN_POINT ( 'NONE',  ( -0.1120320062231000002, -77.79642001619639302, -1.328911429676000067 ) ) ;
#55453 = CARTESIAN_POINT ( 'NONE',  ( -4.123528034279000387, -80.08323015146697799, 10.79195219444999942 ) ) ;
#55454 = ORIENTED_EDGE ( 'NONE', *, *, #21481, .T. ) ;
#55455 = CARTESIAN_POINT ( 'NONE',  ( 8.048377923311001325, -77.50846663325098973, -9.274674788995000085 ) ) ;
#55456 = CARTESIAN_POINT ( 'NONE',  ( 5.324680568677000458, -77.65744226292098062, -9.866841419866000606 ) ) ;
#55457 = CARTESIAN_POINT ( 'NONE',  ( 12.50000000000000000, -28.92928575306000383, 0.000000000000000000 ) ) ;
#55458 = VERTEX_POINT ( 'NONE', #21530 ) ;
#55459 = ORIENTED_EDGE ( 'NONE', *, *, #21089, .T. ) ;
#55460 = DIRECTION ( 'NONE',  ( 0.7071067811865470176, -0.7071067811865470176, 3.680441446989245012E-08 ) ) ;
#55461 = AXIS2_PLACEMENT_3D ( 'NONE', #9680, #4672, #5823 ) ;
#55462 = CARTESIAN_POINT ( 'NONE',  ( -7.374560639699022424, -79.72708333333335418, 9.596002108778135309 ) ) ;
#55463 = CARTESIAN_POINT ( 'NONE',  ( -4.465297566879000257, -79.80323832198099865, 8.686876450551999085 ) ) ;
#55464 = EDGE_LOOP ( 'NONE', ( #48356, #34536, #12538 ) ) ;
#55465 = CARTESIAN_POINT ( 'NONE',  ( 12.83836748059999877, -55.59372227128000077, 2.062147040909000140 ) ) ;
#55466 = DIRECTION ( 'NONE',  ( -1.000000000000000000, 0.000000000000000000, 0.000000000000000000 ) ) ;
#55467 = ORIENTED_EDGE ( 'NONE', *, *, #36242, .T. ) ;
#55468 = CARTESIAN_POINT ( 'NONE',  ( 10.75068688215930379, -80.83963933037178151, -1.406941906430807521 ) ) ;
#55469 = CARTESIAN_POINT ( 'NONE',  ( -2.712012240502000182, -77.40789415034599585, 9.099584490865000319 ) ) ;
#55470 = DIRECTION ( 'NONE',  ( 0.000000000000000000, -0.7071067811866525998, -0.7071067811864425456 ) ) ;
#55471 = AXIS2_PLACEMENT_3D ( 'NONE', #14220, #398, #18376 ) ;
#55472 = EDGE_CURVE ( 'NONE', #42112, #1538, #28017, .T. ) ;
#55473 = CARTESIAN_POINT ( 'NONE',  ( -1.063570462605010869, -80.14457819395771310, -0.6576264011075878546 ) ) ;
#55474 = CARTESIAN_POINT ( 'NONE',  ( 1.208267226925118898, -17.17409317848484918, -12.70228502423913497 ) ) ;
#55475 = CARTESIAN_POINT ( 'NONE',  ( -12.00000000000000178, -78.81041666666666856, -1.570796326794897890 ) ) ;
#55476 = CARTESIAN_POINT ( 'NONE',  ( -12.71107039382202508, -17.74871969248833636, -1.717622521776180466 ) ) ;
#55477 = CARTESIAN_POINT ( 'NONE',  ( 1.095260562757544687, -78.16008608560689197, 1.039742534048890832 ) ) ;
#55478 = CARTESIAN_POINT ( 'NONE',  ( -1.750000000001000089, -23.24999998674999802, 12.56594318051000059 ) ) ;
#55479 = CARTESIAN_POINT ( 'NONE',  ( 11.05577208806000122, -76.73394859499998688, -4.921212746988999243 ) ) ;
#55480 = CARTESIAN_POINT ( 'NONE',  ( -0.6747260877994001316, -82.25000000000000000, -1.052256958371999840 ) ) ;
#55481 = B_SPLINE_CURVE_WITH_KNOTS ( 'NONE', 3,
 ( #6212, #41072, #37503, #41365, #28057, #28643 ),
 .UNSPECIFIED., .F., .F.,
 ( 4, 2, 4 ),
 ( 0.000000000000000000, 0.5000000000000000000, 1.000000000000000000 ),
 .UNSPECIFIED. ) ;
#55482 = DIRECTION ( 'NONE',  ( 0.000000000000000000, -1.000000000000000000, 0.000000000000000000 ) ) ;
#55483 = CARTESIAN_POINT ( 'NONE',  ( 0.000000000000000000, -65.72928575305999743, 0.000000000000000000 ) ) ;
#55484 = CARTESIAN_POINT ( 'NONE',  ( 7.081057523560999378, -79.19131633868998676, -10.01287680343000019 ) ) ;
#55485 = CARTESIAN_POINT ( 'NONE',  ( -12.27595451887999900, -76.06383379162799940, 0.3505736730271999391 ) ) ;
#55486 = CARTESIAN_POINT ( 'NONE',  ( -3.106054555984679499, -86.07390000031791999, 1.382904586457438967 ) ) ;
#55487 = ADVANCED_FACE ( 'NONE', ( #49444 ), #27273, .T. ) ;
#55488 = CARTESIAN_POINT ( 'NONE',  ( -8.583774432395999909, -76.84021498579799925, 4.596844558760999178 ) ) ;
#55489 = CARTESIAN_POINT ( 'NONE',  ( 2.256045313337027292, -78.18992600313380592, -11.85249000648438411 ) ) ;
#55490 = CYLINDRICAL_SURFACE ( 'NONE', #24791, 10.75000000000000000 ) ;
#55491 = VERTEX_POINT ( 'NONE', #8396 ) ;
#55492 = CARTESIAN_POINT ( 'NONE',  ( -1.074445222347000017, -83.55884224245099290, -0.5709172427956999973 ) ) ;
#55493 = CARTESIAN_POINT ( 'NONE',  ( -3.605088315526999487, -77.23446514106798588, 9.013044129564001139 ) ) ;
#55494 = CARTESIAN_POINT ( 'NONE',  ( -1.750000000000000000, -58.54977139303999678, -12.65375411740000011 ) ) ;
#55495 = CARTESIAN_POINT ( 'NONE',  ( -0.9995835529977281642, -78.94791666666662877, 0.7681833999686391579 ) ) ;
#55496 = CARTESIAN_POINT ( 'NONE',  ( 3.854927634485999732, -3.051506412944000157, 0.3462089483260999967 ) ) ;
#55497 = CARTESIAN_POINT ( 'NONE',  ( -0.7974440169908999509, -78.62859328629799904, -12.02330465019000094 ) ) ;
#55498 = CARTESIAN_POINT ( 'NONE',  ( 3.223804565277000211, -78.05477596781798866, 9.075257246486000184 ) ) ;
#55499 = AXIS2_PLACEMENT_3D ( 'NONE', #57215, #12345, #35044 ) ;
#55500 = EDGE_CURVE ( 'NONE', #28651, #41885, #31402, .T. ) ;
#55502 = CARTESIAN_POINT ( 'NONE',  ( -6.364729966985085419, -77.77625342220865434, -9.067865724216227719 ) ) ;
#55501 = CARTESIAN_POINT ( 'NONE',  ( -10.72149750877111707, -76.16622351037557337, 4.807460443398728245 ) ) ;
#55503 = CARTESIAN_POINT ( 'NONE',  ( 7.599690325503999588, -79.21286685420099616, -7.837095951096998192 ) ) ;
#55504 = CARTESIAN_POINT ( 'NONE',  ( -3.407883501311117946, -85.79678895079199208, 1.440947618426057009 ) ) ;
#55505 = VERTEX_POINT ( 'NONE', #52989 ) ;
#55506 = CARTESIAN_POINT ( 'NONE',  ( 12.70228857838913505, -24.82190589608148201, 1.213561371330137861 ) ) ;
#55507 = EDGE_CURVE ( 'NONE', #22633, #35536, #45310, .T. ) ;
#55508 = DIRECTION ( 'NONE',  ( -0.7071067811865474617, -0.7071067811865474617, -8.139044558222544110E-11 ) ) ;
#55509 = CARTESIAN_POINT ( 'NONE',  ( -7.220923959705244144, -76.87291666666665435, -9.396085398178621872 ) ) ;
#55510 = CARTESIAN_POINT ( 'NONE',  ( -8.058638732054999920, -78.54984005612499232, -7.451332657186999775 ) ) ;
#55511 = CARTESIAN_POINT ( 'NONE',  ( -10.50034262194430568, -80.07607525657526537, 3.277372812034037075 ) ) ;
#55512 = CARTESIAN_POINT ( 'NONE',  ( -9.084942557926000362, -79.55399766404198658, 2.975715551223999888 ) ) ;
#55513 = CARTESIAN_POINT ( 'NONE',  ( 9.963464501286001251, -18.31723479381000175, -7.659241807038999816 ) ) ;
#55514 = CARTESIAN_POINT ( 'NONE',  ( -1.199999995295999877, -81.00000000470399186, 6.999999972240000368 ) ) ;
#55515 = EDGE_LOOP ( 'NONE', ( #15222, #50186, #53929, #4681 ) ) ;
#55516 = CARTESIAN_POINT ( 'NONE',  ( -8.075863243196769403, -76.41068158389745690, -7.736832730023080806 ) ) ;
#55517 = CARTESIAN_POINT ( 'NONE',  ( 7.833999859145873934, -79.73288990288156697, -8.785953829483144517 ) ) ;
#55518 = CARTESIAN_POINT ( 'NONE',  ( 3.399999999999980815, -78.70000000000000284, -4.163799117100976893E-16 ) ) ;
#55519 = CARTESIAN_POINT ( 'NONE',  ( 10.11262422264428196, -77.65708660579868194, -6.589681015037502476 ) ) ;
#55520 = CARTESIAN_POINT ( 'NONE',  ( 1.045473607267330740, -81.39676167661833972, 0.6855302019354867493 ) ) ;
#55521 = CARTESIAN_POINT ( 'NONE',  ( -5.269052519453173211, -78.76382107170879010, 9.902459013403186461 ) ) ;
#55522 = CARTESIAN_POINT ( 'NONE',  ( -11.75000000000000000, -77.70000000000000284, 0.000000000000000000 ) ) ;
#55523 = CARTESIAN_POINT ( 'NONE',  ( -8.583665412789912352, -17.02814425026586420, -9.102144266520932447 ) ) ;
#55524 = ADVANCED_FACE ( 'NONE', ( #26683 ), #41517, .T. ) ;
#55525 = CARTESIAN_POINT ( 'NONE',  ( -0.5791533927176000240, -78.49152764148000472, 1.172759083288000159 ) ) ;
#55526 = FACE_OUTER_BOUND ( 'NONE', #4203, .T. ) ;
#55527 = CARTESIAN_POINT ( 'NONE',  ( -10.65690479855507000, -78.93087277451306250, 2.626442266231765021 ) ) ;
#55528 = DIRECTION ( 'NONE',  ( -1.000000000000000000, 0.000000000000000000, 0.000000000000000000 ) ) ;
#55529 = ORIENTED_EDGE ( 'NONE', *, *, #33603, .F. ) ;
#55530 = ORIENTED_EDGE ( 'NONE', *, *, #31916, .T. ) ;
#55531 = CARTESIAN_POINT ( 'NONE',  ( -7.629208874607999569, -78.93548998579800013, -6.499394396314999156 ) ) ;
#55532 = CARTESIAN_POINT ( 'NONE',  ( 8.747355858532181117, -78.80079676788167831, -6.250980141072946417 ) ) ;
#55533 = ORIENTED_EDGE ( 'NONE', *, *, #32602, .F. ) ;
#55534 = DIRECTION ( 'NONE',  ( 1.000000000000000000, 0.000000000000000000, 0.000000000000000000 ) ) ;
#55535 = AXIS2_PLACEMENT_3D ( 'NONE', #39283, #30980, #48170 ) ;
#55536 = CARTESIAN_POINT ( 'NONE',  ( 0.7554284705563452107, -80.23333333333330586, 1.310679582531388609 ) ) ;
#55537 = CARTESIAN_POINT ( 'NONE',  ( 7.758655887927999650, -60.95078616210999911, 9.996711281005000060 ) ) ;
#55538 = CARTESIAN_POINT ( 'NONE',  ( -9.663535141866287148, -76.10162506589206544, -7.446444224017321645 ) ) ;
#55539 = CARTESIAN_POINT ( 'NONE',  ( 3.249543687795219959, -78.69676261847072851, -11.53084807003014056 ) ) ;
#55540 = CARTESIAN_POINT ( 'NONE',  ( 6.766402264611000028, -79.44263615497600028, -8.946167390840999545 ) ) ;
#55541 = ORIENTED_EDGE ( 'NONE', *, *, #23548, .T. ) ;
#55542 = CARTESIAN_POINT ( 'NONE',  ( -8.274772993773998664, -24.97888614414509334, 9.689268730326240586 ) ) ;
#55543 = ORIENTED_EDGE ( 'NONE', *, *, #42332, .F. ) ;
#55544 = CARTESIAN_POINT ( 'NONE',  ( 7.483246165179296305, -77.40010939284451297, 5.437107557591821738 ) ) ;
#55545 = CARTESIAN_POINT ( 'NONE',  ( 1.010832202629999843, -79.43640437465400339, -0.8478131160371998876 ) ) ;
#55546 = LINE ( 'NONE', #23952, #48897 ) ;
#55547 = CARTESIAN_POINT ( 'NONE',  ( -7.707166124622999881, -77.44242527032199064, -5.896629607976000109 ) ) ;
#55548 = CARTESIAN_POINT ( 'NONE',  ( -9.243145382174642322, -17.08347263195844334, 8.441178780136395332 ) ) ;
#55549 = AXIS2_PLACEMENT_3D ( 'NONE', #28591, #23299, #46636 ) ;
#55550 = CARTESIAN_POINT ( 'NONE',  ( 3.140974612311376646, -78.54583333333332007, -11.68767212001978706 ) ) ;
#55551 = CARTESIAN_POINT ( 'NONE',  ( 0.4192948356380000186, -79.53636913735000746, -1.440205485619000081 ) ) ;
#55552 = CARTESIAN_POINT ( 'NONE',  ( 7.840491480036000382, -78.80527898622098348, 7.784894796889999746 ) ) ;
#55553 = EDGE_CURVE ( 'NONE', #23504, #50397, #11116, .T. ) ;
#55554 = DIRECTION ( 'NONE',  ( 0.000000000000000000, 0.7071067811866525998, -0.7071067811864425456 ) ) ;
#55555 = CARTESIAN_POINT ( 'NONE',  ( -8.533826143225001104, -25.00526450249999755, -9.213084459905999779 ) ) ;
#55556 = CARTESIAN_POINT ( 'NONE',  ( 5.836375128730250772, -79.12308539666503293, 7.594790468097947667 ) ) ;
#55557 = CARTESIAN_POINT ( 'NONE',  ( 3.437433312124999585, -84.02206052499799682, 0.8749982434006999821 ) ) ;
#55558 = ORIENTED_EDGE ( 'NONE', *, *, #7318, .F. ) ;
#55559 = EDGE_CURVE ( 'NONE', #47356, #51133, #26408, .T. ) ;
#55560 = CARTESIAN_POINT ( 'NONE',  ( -10.84960119849321281, -77.20000000000000284, 1.688458811413132699 ) ) ;
#55561 = CARTESIAN_POINT ( 'NONE',  ( -1.530783851654999861, -80.79393956010999034, 0.7460011833842999929 ) ) ;
#55562 = CARTESIAN_POINT ( 'NONE',  ( 10.45296947248102803, -77.86878944864642449, 2.509422360510712213 ) ) ;
#55563 = CARTESIAN_POINT ( 'NONE',  ( 11.70594025892000012, -78.33315437694399463, 2.546964289010999583 ) ) ;
#55564 = MANIFOLD_SOLID_BREP ( 'Stock-MAS-694-1', #31467 ) ;
#55565 = CARTESIAN_POINT ( 'NONE',  ( -7.943801774166999508, -17.56598212471000053, 9.641153612788999183 ) ) ;
#55566 = CARTESIAN_POINT ( 'NONE',  ( 1.750000000000000000, -23.24999999688999708, -12.50000000000000000 ) ) ;
#55567 = CARTESIAN_POINT ( 'NONE',  ( 1.925972852894063836, -2.921010677132802602, -2.948710677374434486 ) ) ;
#55568 = LINE ( 'NONE', #15418, #27364 ) ;
#55569 = CARTESIAN_POINT ( 'NONE',  ( 7.429344776774999382, -78.38180575231598368, 5.780660057059999524 ) ) ;
#55570 = CARTESIAN_POINT ( 'NONE',  ( 3.620209227049975720, -85.94828561723799965, -1.611820994701054222 ) ) ;
#55571 = CARTESIAN_POINT ( 'NONE',  ( -9.833855776131001036, -77.49629348652399585, -4.999701486664000605 ) ) ;
#55572 = CARTESIAN_POINT ( 'NONE',  ( 0.000000000000000000, -2.660000000000000142, 0.000000000000000000 ) ) ;
#55573 = CARTESIAN_POINT ( 'NONE',  ( 0.000000000000000000, -77.29999999999999716, 0.000000000000000000 ) ) ;
#55574 = EDGE_LOOP ( 'NONE', ( #6439, #14681, #15314, #39743, #35701 ) ) ;
#55575 = CARTESIAN_POINT ( 'NONE',  ( 0.2153359604882000011, -82.08398151067899562, 1.316133176457000120 ) ) ;
#55576 = CARTESIAN_POINT ( 'NONE',  ( -0.7707251311569810470, -77.07827341652770770, 11.74748571488081517 ) ) ;
#55577 = CARTESIAN_POINT ( 'NONE',  ( 0.005119011380000999985, -61.73813862155999743, -12.43705489347999915 ) ) ;
#55578 = ADVANCED_FACE ( 'NONE', ( #30536 ), #48569, .F. ) ;
#55579 = LINE ( 'NONE', #15716, #54048 ) ;
#55580 = CARTESIAN_POINT ( 'NONE',  ( 2.854969924326999919, -78.12062596773400003, 10.84745395576000071 ) ) ;
#55581 = CARTESIAN_POINT ( 'NONE',  ( -8.631379868284000167, -78.31686478745199054, 6.779623747090999686 ) ) ;
#55582 = CARTESIAN_POINT ( 'NONE',  ( 6.436424241555000592, -80.32391735373440156, 8.610165096135999008 ) ) ;
#55583 = CARTESIAN_POINT ( 'NONE',  ( -3.355836315903201417, -86.06145835254793042, 2.200893284374637826 ) ) ;
#55584 = CARTESIAN_POINT ( 'NONE',  ( -1.750000000001000089, -23.25000000990999993, -12.56594317857000043 ) ) ;
#55585 = CARTESIAN_POINT ( 'NONE',  ( -10.18249594442533024, -54.50907903246198316, -7.792385963363297030 ) ) ;
#55586 = CARTESIAN_POINT ( 'NONE',  ( 2.265192278225999889, -85.19944503318799889, -3.504135580763000135 ) ) ;
#55587 = AXIS2_PLACEMENT_3D ( 'NONE', #3931, #49108, #21651 ) ;
#55588 = CARTESIAN_POINT ( 'NONE',  ( -7.624341764943999955, -60.06485149430999826, 10.42531124854999902 ) ) ;
#55589 = CARTESIAN_POINT ( 'NONE',  ( 7.756275637014999447, -54.57995361804000112, -10.15825999914999933 ) ) ;
#55590 = CARTESIAN_POINT ( 'NONE',  ( 10.33259770149999923, -77.55914763795398414, 4.480110411294999651 ) ) ;
#55591 = B_SPLINE_CURVE_WITH_KNOTS ( 'NONE', 3,
 ( #39108, #34664, #35233, #53264, #8388, #53860, #45597, #31981, #49732, #8683 ),
 .UNSPECIFIED., .F., .F.,
 ( 4, 2, 2, 2, 4 ),
 ( 0.000000000000000000, 0.2500000000000000000, 0.5000000000000000000, 0.7500000000000000000, 1.000000000000000000 ),
 .UNSPECIFIED. ) ;
#55592 = CARTESIAN_POINT ( 'NONE',  ( -0.3164372427141999844, -79.66059977445999607, 1.635583079321000000 ) ) ;
#55593 = CARTESIAN_POINT ( 'NONE',  ( 0.1413472186869999814, -77.88570945174998883, 1.208470106255999932 ) ) ;
#55594 = CARTESIAN_POINT ( 'NONE',  ( -12.00000000000000355, -77.78958333333331154, 1.570796326794848596 ) ) ;
#55595 = DIRECTION ( 'NONE',  ( -0.9999999999999997780, 0.000000000000000000, 2.125172267659999677E-08 ) ) ;
#55596 = TOROIDAL_SURFACE ( 'NONE', #40547, 1.250000000000000000, 0.5000000000000000000 ) ;
#55597 = DIRECTION ( 'NONE',  ( 0.000000000000000000, -1.000000000000000000, 0.000000000000000000 ) ) ;
#55598 = ORIENTED_EDGE ( 'NONE', *, *, #11996, .F. ) ;
#55599 = B_SPLINE_CURVE_WITH_KNOTS ( 'NONE', 3,
 ( #26850, #9158, #12977, #12416, #52862, #57863 ),
 .UNSPECIFIED., .F., .F.,
 ( 4, 2, 4 ),
 ( 0.000000000000000000, 0.5000000000000000000, 1.000000000000000000 ),
 .UNSPECIFIED. ) ;
#55600 = CARTESIAN_POINT ( 'NONE',  ( 1.212634435040167658, -79.83097499881669989, -0.3047410518862661011 ) ) ;
#55601 = CARTESIAN_POINT ( 'NONE',  ( 1.250000000000000000, -80.84999999999999432, 0.000000000000000000 ) ) ;
#55602 = ORIENTED_EDGE ( 'NONE', *, *, #15874, .F. ) ;
#55603 = CARTESIAN_POINT ( 'NONE',  ( 0.004852466274130710043, -81.72588911470774065, -1.249646052481410141 ) ) ;
#55604 = PRESENTATION_STYLE_ASSIGNMENT (( #37586 ) ) ;
#55605 = CARTESIAN_POINT ( 'NONE',  ( -9.575027280576000166, -79.41750321980599381, 5.479104576271000226 ) ) ;
#55606 = DIRECTION ( 'NONE',  ( 0.000000000000000000, -1.000000000000000000, 0.000000000000000000 ) ) ;
#55607 = VERTEX_POINT ( 'NONE', #173 ) ;
#55608 = ORIENTED_EDGE ( 'NONE', *, *, #19106, .F. ) ;
#55609 = CARTESIAN_POINT ( 'NONE',  ( -0.7514556209146998622, -81.02214050151400215, 1.202236998062000239 ) ) ;
#55610 = EDGE_LOOP ( 'NONE', ( #44824, #28176, #58325, #33964, #58027 ) ) ;
#55612 = EDGE_CURVE ( 'NONE', #53199, #21248, #17937, .T. ) ;
#55611 = ORIENTED_EDGE ( 'NONE', *, *, #12268, .T. ) ;
#55613 = CARTESIAN_POINT ( 'NONE',  ( 0.9887300587123999396, -17.06589942230999668, 12.65963207090000076 ) ) ;
#55614 = CARTESIAN_POINT ( 'NONE',  ( -8.744140569414998510, -80.29580545329308450, 7.086030162020000134 ) ) ;
#55615 = PRODUCT_CONTEXT ( 'NONE', #48140, 'mechanical' ) ;
#55616 = CARTESIAN_POINT ( 'NONE',  ( 2.894124890898986280, -79.58645832707598800, 1.867041973107900210 ) ) ;
#55617 = CARTESIAN_POINT ( 'NONE',  ( 5.882476073987271015, -78.27997737893470287, -7.138446288670057704 ) ) ;
#55618 = CYLINDRICAL_SURFACE ( 'NONE', #7454, 1.750000000000000000 ) ;
#55619 = VERTEX_POINT ( 'NONE', #49140 ) ;
#55620 = ORIENTED_EDGE ( 'NONE', *, *, #52709, .F. ) ;
#55621 = CARTESIAN_POINT ( 'NONE',  ( -9.175128499341100863, -77.59002790297775221, 1.175099295633919017 ) ) ;
#55622 = CARTESIAN_POINT ( 'NONE',  ( -1.417334032777999964, -79.02654225787900089, -0.4910847579886000736 ) ) ;
#55623 = CARTESIAN_POINT ( 'NONE',  ( 0.000000000000000000, -23.25000000000000000, -12.50000000000000000 ) ) ;
#55624 = CARTESIAN_POINT ( 'NONE',  ( 11.00000000000000000, -76.04999999999999716, -1.235097113410999977E-09 ) ) ;
#55625 = CARTESIAN_POINT ( 'NONE',  ( 9.045658679128999680, -79.04619838613798777, 3.115350657311999782 ) ) ;
#55626 = DIRECTION ( 'NONE',  ( 1.000000000000000000, 0.000000000000000000, 0.000000000000000000 ) ) ;
#55627 = CARTESIAN_POINT ( 'NONE',  ( 2.546818232473923249, -85.87759057800617768, 2.955671346788312892 ) ) ;
#55628 = CARTESIAN_POINT ( 'NONE',  ( -8.254612054926999676, -79.75421655541097721, 6.886499823760000361 ) ) ;
#55629 = CARTESIAN_POINT ( 'NONE',  ( 1.100531998921000065, -79.28075525790998768, -0.7842560430285000495 ) ) ;
#55630 = CARTESIAN_POINT ( 'NONE',  ( 1.780723875404367718, -76.56267306090380487, 11.62581106263551156 ) ) ;
#55631 = B_SPLINE_CURVE_WITH_KNOTS ( 'NONE', 3,
 ( #33133, #36988, #46170, #41132, #27539, #726 ),
 .UNSPECIFIED., .F., .F.,
 ( 4, 1, 1, 4 ),
 ( 0.000000000000000000, 0.3333333333333000081, 0.6666666666667000474, 1.000000000000000000 ),
 .UNSPECIFIED. ) ;
#55632 = EDGE_CURVE ( 'NONE', #29156, #25767, #4751, .T. ) ;
#55633 = DIRECTION ( 'NONE',  ( -1.000000000000000000, 0.000000000000000000, 0.000000000000000000 ) ) ;
#55635 = VECTOR ( 'NONE', #12453, 1000.000000000000000 ) ;
#55634 = CARTESIAN_POINT ( 'NONE',  ( 0.5368854727554398520, -79.59607745916922283, 1.411883060306194926 ) ) ;
#55636 = CARTESIAN_POINT ( 'NONE',  ( -0.6447613848864999220, -77.95096001420199627, 9.665783406873000416 ) ) ;
#55637 = DIRECTION ( 'NONE',  ( 2.011932846957000032E-11, -1.000000000000000000, -1.337053924462999991E-10 ) ) ;
#55638 = CARTESIAN_POINT ( 'NONE',  ( 1.548297770046941357, -76.13463541594487083, -11.83463544049746652 ) ) ;
#55639 = CIRCLE ( 'NONE', #21661, 11.70000000000000107 ) ;
#55641 = CARTESIAN_POINT ( 'NONE',  ( 0.4356486348716999690, -17.11935044189999999, -12.43591427121000237 ) ) ;
#55640 = CARTESIAN_POINT ( 'NONE',  ( 0.000000000000000000, -2.660000000000000142, 0.000000000000000000 ) ) ;
#55642 = CARTESIAN_POINT ( 'NONE',  ( 0.000000000000000000, -74.70999999999999375, 0.000000000000000000 ) ) ;
#55643 = CARTESIAN_POINT ( 'NONE',  ( 9.499999794217913518, -79.99999999999998579, -1.003825360198642880 ) ) ;
#55644 = CARTESIAN_POINT ( 'NONE',  ( -7.919595949288999570, -59.94999999969999749, -9.050966799188000067 ) ) ;
#55645 = CARTESIAN_POINT ( 'NONE',  ( -3.320509146851418958, -1.277620849617314702, -1.203439844071006126 ) ) ;
#55646 = ORIENTED_EDGE ( 'NONE', *, *, #6448, .T. ) ;
#55647 = CARTESIAN_POINT ( 'NONE',  ( 8.796335266379992746, -78.39791666666666003, -6.760013919724047859 ) ) ;
#55648 = CARTESIAN_POINT ( 'NONE',  ( 0.4764073897346013386, -18.48308356130117502, -10.98970030907996431 ) ) ;
#55649 = DIRECTION ( 'NONE',  ( 0.7071067811865475727, 0.000000000000000000, 0.7071067811865475727 ) ) ;
#55650 = CARTESIAN_POINT ( 'NONE',  ( -6.184040273379711294, -77.17951720182109909, -6.972051400811474231 ) ) ;
#55651 = EDGE_CURVE ( 'NONE', #20090, #20675, #16050, .T. ) ;
#55652 = CARTESIAN_POINT ( 'NONE',  ( 9.457014981167999323, -79.13566112575199440, -0.8878631254947999540 ) ) ;
#55653 = CARTESIAN_POINT ( 'NONE',  ( 1.750000000001000089, -23.24999998674999802, -12.56594318051000059 ) ) ;
#55654 = LINE ( 'NONE', #20795, #42199 ) ;
#55655 = CARTESIAN_POINT ( 'NONE',  ( 10.34395135506634311, -79.37222233871651156, 2.957440531220869140 ) ) ;
#55656 = CARTESIAN_POINT ( 'NONE',  ( 9.129467682721999822, -79.09873998579800514, -3.694451172265999617 ) ) ;
#55657 = FACE_OUTER_BOUND ( 'NONE', #57545, .T. ) ;
#55658 = CARTESIAN_POINT ( 'NONE',  ( 3.913900004701999613, -77.58956168025198963, 10.45689208369000056 ) ) ;
#55659 = CIRCLE ( 'NONE', #45258, 1.000000000000000000 ) ;
#55660 = CARTESIAN_POINT ( 'NONE',  ( -0.5022895558335001009, -81.30840176356799986, 1.523433483890000106 ) ) ;
#55661 = CARTESIAN_POINT ( 'NONE',  ( -8.871933854994999535, -78.68354514476064310, -3.979018739998999354 ) ) ;
#55662 = DIRECTION ( 'NONE',  ( 1.000000000000000000, 0.000000000000000000, 0.000000000000000000 ) ) ;
#55664 = CARTESIAN_POINT ( 'NONE',  ( 3.250000000000000000, -2.750000000000000000, 0.000000000000000000 ) ) ;
#55663 = CARTESIAN_POINT ( 'NONE',  ( 2.055812863559000281, -82.38203554481998481, 3.144033732121000124 ) ) ;
#55665 = DIRECTION ( 'NONE',  ( 0.000000000000000000, 0.000000000000000000, -1.000000000000000000 ) ) ;
#55666 = CARTESIAN_POINT ( 'NONE',  ( -1.310679582531389276, -80.85833333333332007, 0.7554284705563443225 ) ) ;
#55667 = CARTESIAN_POINT ( 'NONE',  ( 7.601957635810941305, -80.28750185634191894, -7.600825067425311055 ) ) ;
#55668 = LINE ( 'NONE', #10215, #32430 ) ;
#55669 = CARTESIAN_POINT ( 'NONE',  ( 2.905710065331635228, -79.62500000110051701, -8.943793168028266294 ) ) ;
#55670 = PRODUCT_DEFINITION ( 'UNKNOWN', '', #24436, #25680 ) ;
#55671 = CARTESIAN_POINT ( 'NONE',  ( 0.000000000000000000, -81.99999999999998579, -4.299999999999968736 ) ) ;
#55672 = EDGE_LOOP ( 'NONE', ( #33868, #36353, #18503, #16686 ) ) ;
#55673 = CARTESIAN_POINT ( 'NONE',  ( -11.22206352833000054, -79.66321515653298491, -4.332716936452000844 ) ) ;
#55674 = CARTESIAN_POINT ( 'NONE',  ( -12.50728321921983799, -61.79975184134815436, -0.1774118161306304509 ) ) ;
#55675 = CARTESIAN_POINT ( 'NONE',  ( 7.850068285611341956, -17.68530314558086047, 9.837745660714951157 ) ) ;
#55676 = VERTEX_POINT ( 'NONE', #28436 ) ;
#55677 = CARTESIAN_POINT ( 'NONE',  ( -1.828203654226000063, -78.01064764102999050, 11.79377691179999843 ) ) ;
#55678 = ORIENTED_EDGE ( 'NONE', *, *, #31687, .T. ) ;
#55680 = EDGE_CURVE ( 'NONE', #43667, #54465, #40575, .T. ) ;
#55679 = ORIENTED_EDGE ( 'NONE', *, *, #46918, .F. ) ;
#55681 = CONICAL_SURFACE ( 'NONE', #29235, 8.749999999256001360, 0.7853981633972997312 ) ;
#55682 = CARTESIAN_POINT ( 'NONE',  ( 10.47020627418438643, -78.77083333333334281, 2.813789756862283387 ) ) ;
#55683 = AXIS2_PLACEMENT_3D ( 'NONE', #18568, #586, #14988 ) ;
#55684 = ORIENTED_EDGE ( 'NONE', *, *, #41247, .T. ) ;
#55685 = EDGE_CURVE ( 'NONE', #47619, #1538, #51198, .T. ) ;
#55686 = CARTESIAN_POINT ( 'NONE',  ( -3.405161111042999789, -81.61969232303898991, 0.9932007693457001185 ) ) ;
#55687 = CARTESIAN_POINT ( 'NONE',  ( 7.735842139137476536, -79.19900585853359587, 5.514108658314483158 ) ) ;
#55688 = EDGE_LOOP ( 'NONE', ( #91, #40568, #30462, #54123 ) ) ;
#55689 = CARTESIAN_POINT ( 'NONE',  ( 1.156359412676422282, -82.81903375624176533, -0.4746362260554010670 ) ) ;
#55690 = CARTESIAN_POINT ( 'NONE',  ( -7.613962827198000660, -60.10639625617000092, 10.53101998748999968 ) ) ;
#55691 = ORIENTED_EDGE ( 'NONE', *, *, #44884, .T. ) ;
#55692 = CARTESIAN_POINT ( 'NONE',  ( -1.191119343893799920, -79.57605893021457177, 0.3784560293714495649 ) ) ;
#55693 = CARTESIAN_POINT ( 'NONE',  ( 1.528777005363244568, -78.99356928323743432, -0.1184073789878865995 ) ) ;
#55694 = CARTESIAN_POINT ( 'NONE',  ( -9.949999999959999286, -86.19999999995999929, -1.488372002482999864E-09 ) ) ;
#55695 = CARTESIAN_POINT ( 'NONE',  ( -12.50657384684486573, -17.02752586736362872, 0.3552647087867685238 ) ) ;
#55696 = CARTESIAN_POINT ( 'NONE',  ( -0.5211966972079136173, -0.9921874999512605431, 3.256119704917901370 ) ) ;
#55697 = CARTESIAN_POINT ( 'NONE',  ( 3.089703999423501379, -78.54774383309995756, -10.47025070535708835 ) ) ;
#55698 = CARTESIAN_POINT ( 'NONE',  ( 7.486068761172999686, -75.88288212886199346, -8.059700645992000645 ) ) ;
#55699 = CARTESIAN_POINT ( 'NONE',  ( -11.75000000000000711, -77.28958333333332575, 1.538071403319954955 ) ) ;
#55700 = B_SPLINE_CURVE_WITH_KNOTS ( 'NONE', 3,
 ( #12241, #47702, #52404, #11958, #57681, #47989, #7525, #25522, #51833, #11388, #47413, #6943, #43539, #21098, #57111, #30232, #45294, #22840 ),
 .UNSPECIFIED., .F., .F.,
 ( 4, 2, 2, 2, 2, 2, 2, 2, 4 ),
 ( 0.000000000000000000, 0.1250000000000000000, 0.2500000000000000000, 0.3750000000000000000, 0.5000000000000000000, 0.6250000000000000000, 0.7500000000000000000, 0.8750000000000000000, 1.000000000000000000 ),
 .UNSPECIFIED. ) ;
#55701 = CARTESIAN_POINT ( 'NONE',  ( 0.6295237254636258939, -81.16666666666665719, -1.092232985442821658 ) ) ;
#55702 = CARTESIAN_POINT ( 'NONE',  ( 11.06434106074000034, -76.55977708591699127, -1.914180163160999815 ) ) ;
#55703 = CARTESIAN_POINT ( 'NONE',  ( -7.868794148055054727, -78.64422463589345114, -4.862493407595640527 ) ) ;
#55704 = CARTESIAN_POINT ( 'NONE',  ( 7.037839055072352856, -76.52353836542157239, 9.409452059956553427 ) ) ;
#55705 = AXIS2_PLACEMENT_3D ( 'NONE', #11605, #4097, #48207 ) ;
#55706 = CARTESIAN_POINT ( 'NONE',  ( -6.984884556549999957, -77.51221001420199741, 6.307785355753999568 ) ) ;
#55708 = EDGE_CURVE ( 'NONE', #15167, #57774, #44313, .T. ) ;
#55707 = B_SPLINE_CURVE_WITH_KNOTS ( 'NONE', 3,
 ( #49409, #26942, #4531, #17219 ),
 .UNSPECIFIED., .F., .F.,
 ( 4, 4 ),
 ( 0.000000000000000000, 1.000000000000000000 ),
 .UNSPECIFIED. ) ;
#55709 = CARTESIAN_POINT ( 'NONE',  ( 0.000000000000000000, -80.79999999999999716, 0.000000000000000000 ) ) ;
#55710 = CARTESIAN_POINT ( 'NONE',  ( -7.774388101806787077, -80.16288445207561608, -7.781834858813881262 ) ) ;
#55711 = CARTESIAN_POINT ( 'NONE',  ( -3.002885140990844359, -3.070088000970283115, 1.241022100456280919 ) ) ;
#55712 = CARTESIAN_POINT ( 'NONE',  ( 3.542352713837999989, -80.72628455456799657, 1.250239712736999964 ) ) ;
#55713 = CARTESIAN_POINT ( 'NONE',  ( -10.76103485090999889, -79.54790851955898745, -5.748848539142999314 ) ) ;
#55714 = CARTESIAN_POINT ( 'NONE',  ( -9.129079589776326387, -78.05585660196875608, 5.676768158082784232 ) ) ;
#55715 = CARTESIAN_POINT ( 'NONE',  ( -0.5008228193151907925, -83.00788715391320238, 1.145400540283604496 ) ) ;
#55716 = CYLINDRICAL_SURFACE ( 'NONE', #8524, 1.500000000000000000 ) ;
#55717 = CARTESIAN_POINT ( 'NONE',  ( -8.246370918359055224, -76.26250308826989510, -8.370124202908149513 ) ) ;
#55718 = CARTESIAN_POINT ( 'NONE',  ( 5.674932013357969041, -79.99999999999998579, 7.468275051675760778 ) ) ;
#55719 = CARTESIAN_POINT ( 'NONE',  ( -0.2494208068355079355, -24.99288960762974909, 12.50614183112980626 ) ) ;
#55720 = CARTESIAN_POINT ( 'NONE',  ( 0.2561524587948984522, -3.499999999999999112, 3.291991744369633377 ) ) ;
#55721 = EDGE_CURVE ( 'NONE', #16901, #45372, #47175, .T. ) ;
#55722 = CARTESIAN_POINT ( 'NONE',  ( 0.6791306551168999617, -81.30185674818700647, -1.147762040996999966 ) ) ;
#55723 = CONICAL_SURFACE ( 'NONE', #40628, 1.099999997158000120, 0.7853981633972997312 ) ;
#55724 = CARTESIAN_POINT ( 'NONE',  ( 0.000000000000000000, -76.39999999999999147, 0.5999999999999999778 ) ) ;
#55726 = EDGE_CURVE ( 'NONE', #15959, #6548, #2635, .T. ) ;
#55725 = DIRECTION ( 'NONE',  ( 0.000000000000000000, -1.000000000000000000, 0.000000000000000000 ) ) ;
#55727 = FACE_OUTER_BOUND ( 'NONE', #47934, .T. ) ;
#55728 = CIRCLE ( 'NONE', #4813, 1.250000000000000444 ) ;
#55729 = CARTESIAN_POINT ( 'NONE',  ( 1.674065321307220300, -77.58787199535142065, -10.64115275760022605 ) ) ;
#55730 = CARTESIAN_POINT ( 'NONE',  ( 3.074539145570156951, -78.34369197868522861, -11.43814598833678708 ) ) ;
#55731 = CARTESIAN_POINT ( 'NONE',  ( -9.505686244346000180, -79.30834055796346149, 5.486888517706000279 ) ) ;
#55732 = CARTESIAN_POINT ( 'NONE',  ( 4.340686961497000063, -76.32245797811999921, -11.41455165844999975 ) ) ;
#55733 = EDGE_LOOP ( 'NONE', ( #55459, #41191, #21979, #32137 ) ) ;
#55734 = CARTESIAN_POINT ( 'NONE',  ( -2.655941862454000102, -83.59657450217399344, -3.162985355011000088 ) ) ;
#55735 = CARTESIAN_POINT ( 'NONE',  ( 10.40890440584000132, -80.99049444111729201, 4.369998498427999145 ) ) ;
#55736 = DIRECTION ( 'NONE',  ( 0.000000000000000000, -1.000000000000000000, 0.000000000000000000 ) ) ;
#55737 = DIRECTION ( 'NONE',  ( -1.000000000000000000, 0.000000000000000000, 0.000000000000000000 ) ) ;
#55738 = CARTESIAN_POINT ( 'NONE',  ( 9.668944085725000193, -77.19398569721599301, 5.685915129398999568 ) ) ;
#55739 = CARTESIAN_POINT ( 'NONE',  ( -12.76303204522000101, -23.26485147686999966, -1.980584515753000208 ) ) ;
#55740 = CARTESIAN_POINT ( 'NONE',  ( -5.370832524224000259, -77.75066704931698780, 8.124890996387998499 ) ) ;
#55741 = CARTESIAN_POINT ( 'NONE',  ( 4.037784781204999618, -83.90807560421097833, -1.050166339152999839 ) ) ;
#55742 = CARTESIAN_POINT ( 'NONE',  ( 0.5999999999999999778, -5.000000000000000000, 4.000000000000000000 ) ) ;
#55743 = FACE_OUTER_BOUND ( 'NONE', #5976, .T. ) ;
#55744 = ORIENTED_EDGE ( 'NONE', *, *, #7707, .F. ) ;
#55745 = FACE_OUTER_BOUND ( 'NONE', #15958, .T. ) ;
#55746 = CARTESIAN_POINT ( 'NONE',  ( -5.059370734576000395, -80.78625270698918825, -10.06538451635999998 ) ) ;
#55747 = ADVANCED_FACE ( 'NONE', ( #8325 ), #22655, .F. ) ;
#55748 = CARTESIAN_POINT ( 'NONE',  ( 2.604727510204928986, -78.97720587346522336, -2.786836471777216495 ) ) ;
#55749 = EDGE_LOOP ( 'NONE', ( #4403, #49511, #46520, #48641 ) ) ;
#55750 = CARTESIAN_POINT ( 'NONE',  ( -0.2406813341972999787, -78.78867248381800437, -1.311734976874999958 ) ) ;
#55751 = CARTESIAN_POINT ( 'NONE',  ( 11.01715842067999951, -78.56297001833898719, 0.8367281403419999375 ) ) ;
#55752 = CARTESIAN_POINT ( 'NONE',  ( 4.714910253073366420, -77.66722752291366305, -8.048511890795102985 ) ) ;
#55753 = CARTESIAN_POINT ( 'NONE',  ( 6.321312781113044288, -78.78005093995929542, 10.10155803323563894 ) ) ;
#55754 = ORIENTED_EDGE ( 'NONE', *, *, #14682, .F. ) ;
#55755 = CIRCLE ( 'NONE', #2034, 3.400000000000000799 ) ;
#55756 = CARTESIAN_POINT ( 'NONE',  ( -10.77989530031999976, -78.79720534002599663, -5.637054895855999170 ) ) ;
#55757 = CARTESIAN_POINT ( 'NONE',  ( 10.79265454957999992, -77.83137212970099483, 3.422111395643999909 ) ) ;
#55758 = CARTESIAN_POINT ( 'NONE',  ( 9.298780387958270666, -78.70743112811207709, -5.515246406192360062 ) ) ;
#55759 = ORIENTED_EDGE ( 'NONE', *, *, #28870, .T. ) ;
#55760 = ORIENTED_EDGE ( 'NONE', *, *, #31865, .F. ) ;
#55761 = CARTESIAN_POINT ( 'NONE',  ( 0.6783686788296603432, -80.42946718699170106, 1.049845246189362147 ) ) ;
#55762 = EDGE_CURVE ( 'NONE', #46115, #1066, #33008, .T. ) ;
#55763 = CARTESIAN_POINT ( 'NONE',  ( -10.75007815099182551, -77.61041948879531560, -1.407065427747188568 ) ) ;
#55764 = CARTESIAN_POINT ( 'NONE',  ( -7.545891804452000251, -79.83571098023898571, 6.201630566990999682 ) ) ;
#55765 = ORIENTED_EDGE ( 'NONE', *, *, #21561, .F. ) ;
#55766 = DIRECTION ( 'NONE',  ( 0.000000000000000000, 0.000000000000000000, 1.000000000000000000 ) ) ;
#55767 = CARTESIAN_POINT ( 'NONE',  ( -8.824204240651999598, -78.62350394595299008, -6.427191105727000142 ) ) ;
#55768 = EDGE_LOOP ( 'NONE', ( #52348, #38747, #5503, #21172 ) ) ;
#55769 = CARTESIAN_POINT ( 'NONE',  ( 7.103614071024587417, -80.78233878846501170, -8.098765007180103837 ) ) ;
#55770 = CARTESIAN_POINT ( 'NONE',  ( 7.430757984336000099, -77.31331915034598978, 5.911115298933000695 ) ) ;
#55771 = CIRCLE ( 'NONE', #45407, 4.299999999999999822 ) ;
#55772 = CARTESIAN_POINT ( 'NONE',  ( -0.4778988054446937639, -80.19393997919249273, -1.154928669624085691 ) ) ;
#55773 = DIRECTION ( 'NONE',  ( 0.0001230612157847738313, 0.000000000000000000, -0.9999999924279686647 ) ) ;
#55774 = CARTESIAN_POINT ( 'NONE',  ( -0.5313338453197881117, -78.66977913613844464, -9.710363398104801647 ) ) ;
#55775 = DIRECTION ( 'NONE',  ( 1.000000000000000000, 0.000000000000000000, 0.000000000000000000 ) ) ;
#55776 = CARTESIAN_POINT ( 'NONE',  ( -0.7609899864356860499, -79.26659457633572003, 1.304350159878486570 ) ) ;
#55777 = CARTESIAN_POINT ( 'NONE',  ( 4.029970506843416622, -80.97395833763627593, 0.4115634813596021901 ) ) ;
#55778 = CARTESIAN_POINT ( 'NONE',  ( -12.22985280536000019, -76.49175098858000865, -1.402219185755000153 ) ) ;
#55779 = CARTESIAN_POINT ( 'NONE',  ( -7.624341766656999475, -60.06485146221000093, -10.42531125026000005 ) ) ;
#55780 = B_SPLINE_CURVE_WITH_KNOTS ( 'NONE', 3,
 ( #39329, #16330, #47645, #3603, #16900, #30460, #38751, #52058, #34884, #48491, #43196, #8031, #16037, #34598, #34020, #7463, #26029, #21607 ),
 .UNSPECIFIED., .F., .F.,
 ( 4, 2, 2, 2, 2, 2, 2, 2, 4 ),
 ( 0.000000000000000000, 0.1250000000000000833, 0.2500000000000001665, 0.3750000000000001110, 0.5000000000000001110, 0.6250000000000001110, 0.7500000000000000000, 0.8750000000000000000, 1.000000000000000000 ),
 .UNSPECIFIED. ) ;
#55781 = CARTESIAN_POINT ( 'NONE',  ( -12.50000000000000000, -23.24999999688999708, -1.750000000000000000 ) ) ;
#55782 = LINE ( 'NONE', #29184, #25693 ) ;
#55783 = CARTESIAN_POINT ( 'NONE',  ( -1.307210027570999911, -79.06450156920999461, -12.19386267984000050 ) ) ;
#55784 = CARTESIAN_POINT ( 'NONE',  ( 12.07535958108000074, -76.86931163439298587, -2.237927141218000404 ) ) ;
#55785 = CYLINDRICAL_SURFACE ( 'NONE', #48714, 11.75000000000000000 ) ;
#55786 = CARTESIAN_POINT ( 'NONE',  ( 3.224895395523625474, -2.840360689075250189, -0.4480854406879138940 ) ) ;
#55787 = CARTESIAN_POINT ( 'NONE',  ( 11.81350916550069563, -77.81633707358489005, 2.468257657043821496 ) ) ;
#55788 = CARTESIAN_POINT ( 'NONE',  ( 5.745747329289001115, -78.58220418272651386, 9.633509135241000720 ) ) ;
#55789 = AXIS2_PLACEMENT_3D ( 'NONE', #44406, #54727, #26675 ) ;
#55790 = EDGE_LOOP ( 'NONE', ( #46387, #32403, #33813, #28569 ) ) ;
#55791 = CYLINDRICAL_SURFACE ( 'NONE', #16473, 1.750000000000000000 ) ;
#55792 = CARTESIAN_POINT ( 'NONE',  ( -2.858782626228999924, -76.99373160055630194, -9.043346509775000541 ) ) ;
#55793 = DIRECTION ( 'NONE',  ( -1.000000000000000000, 0.000000000000000000, 0.000000000000000000 ) ) ;
#55794 = CARTESIAN_POINT ( 'NONE',  ( -1.217465845835396188, -82.97916666666668561, 0.3271848554490955907 ) ) ;
#55795 = CARTESIAN_POINT ( 'NONE',  ( 2.287685435952000024, -3.564198934507999628, -2.579189048856000088 ) ) ;
#55796 = CARTESIAN_POINT ( 'NONE',  ( 9.846943056836000352, -78.70998123256900669, -6.945033154232000072 ) ) ;
#55797 = CARTESIAN_POINT ( 'NONE',  ( 0.000000000000000000, -87.70000000000000284, 0.000000000000000000 ) ) ;
#55799 = CARTESIAN_POINT ( 'NONE',  ( 10.12290050124000018, -18.75000000007999645, -7.648026767085999822 ) ) ;
#55798 = CARTESIAN_POINT ( 'NONE',  ( -8.194277599536388124, -76.13640838913404707, 8.421365530498844620 ) ) ;
#55800 = CARTESIAN_POINT ( 'NONE',  ( -0.4497554808884999811, -81.98202630415998726, 1.274241432965000032 ) ) ;
#55801 = CARTESIAN_POINT ( 'NONE',  ( -10.54473782110994584, -79.58454813932776517, 2.090270118525876075 ) ) ;
#55802 = ORIENTED_EDGE ( 'NONE', *, *, #17079, .T. ) ;
#55803 = CARTESIAN_POINT ( 'NONE',  ( 1.092232985442823212, -82.20833333333331439, -0.6295237254636224522 ) ) ;
#55804 = CARTESIAN_POINT ( 'NONE',  ( -0.03204405817076169671, -78.70000000000000284, -3.399848993460711899 ) ) ;
#55805 = CARTESIAN_POINT ( 'NONE',  ( -2.839805762151343949, -2.458333333333332593, 1.636761686205412181 ) ) ;
#55806 = CARTESIAN_POINT ( 'NONE',  ( -6.920341278396000106, -79.56116481210098357, -8.518972542050999408 ) ) ;
#55807 = CARTESIAN_POINT ( 'NONE',  ( 7.954951288349001004, -18.55321828668999729, -9.722718241315000398 ) ) ;
#55808 = CARTESIAN_POINT ( 'NONE',  ( -0.2701109549781999797, -78.95643513191498641, 9.556054066276999492 ) ) ;
#55809 = CARTESIAN_POINT ( 'NONE',  ( 9.783235115942000348, -17.46434390394999880, -7.961033122320000821 ) ) ;
#55810 = CARTESIAN_POINT ( 'NONE',  ( 0.000000000000000000, -28.92928575306000383, 0.000000000000000000 ) ) ;
#55811 = EDGE_LOOP ( 'NONE', ( #24266, #39752, #18666, #42253, #11698 ) ) ;
#55812 = CARTESIAN_POINT ( 'NONE',  ( 2.325232682335999890, -78.41813999416500280, -11.01938817673000059 ) ) ;
#55813 = CARTESIAN_POINT ( 'NONE',  ( 10.02302243881105248, -76.06467930920804577, -4.754755962258590429 ) ) ;
#55814 = CARTESIAN_POINT ( 'NONE',  ( -7.104039980509410768, -78.97588114887535937, 9.465219502475884283 ) ) ;
#55815 = CARTESIAN_POINT ( 'NONE',  ( -0.03204386105641461591, -78.70000000000000284, 3.399848995318537348 ) ) ;
#55816 = ADVANCED_FACE ( 'NONE', ( #34889 ), #30747, .T. ) ;
#55817 = CARTESIAN_POINT ( 'NONE',  ( 7.386320950128953733, -77.63040130628132829, -9.560526057520540633 ) ) ;
#55818 = CARTESIAN_POINT ( 'NONE',  ( 1.154165937183204926, -81.38156932103548513, 0.4796374930683212634 ) ) ;
#55819 = B_SPLINE_CURVE_WITH_KNOTS ( 'NONE', 3,
 ( #38404, #31190, #44801, #4353 ),
 .UNSPECIFIED., .F., .F.,
 ( 4, 4 ),
 ( 0.000000000000000000, 1.000000000000000000 ),
 .UNSPECIFIED. ) ;
#55820 = CARTESIAN_POINT ( 'NONE',  ( -0.1930468007397637131, -78.76310372970323215, -1.260176113982175217 ) ) ;
#55821 = CARTESIAN_POINT ( 'NONE',  ( -9.098835018745974779, -77.00000000000000000, -2.252957314591238269 ) ) ;
#55822 = CARTESIAN_POINT ( 'NONE',  ( 1.781953555039999859, -2.911773310596999842, -3.363141973650999983 ) ) ;
#55823 = CARTESIAN_POINT ( 'NONE',  ( -0.1495270637475999975, -79.02672845825999559, 1.413525301447999816 ) ) ;
#55824 = DIRECTION ( 'NONE',  ( -1.000000000000000000, 0.000000000000000000, 0.000000000000000000 ) ) ;
#55825 = CARTESIAN_POINT ( 'NONE',  ( -10.81666588859962275, -79.43653515250106523, 1.862137996412334795 ) ) ;
#55826 = ADVANCED_FACE ( 'NONE', ( #22189 ), #2647, .F. ) ;
#55827 = CARTESIAN_POINT ( 'NONE',  ( -9.000000000000000000, -4.000000000000000000, 0.000000000000000000 ) ) ;
#55828 = ORIENTED_EDGE ( 'NONE', *, *, #15972, .T. ) ;
#55829 = ORIENTED_EDGE ( 'NONE', *, *, #7574, .F. ) ;
#55830 = CARTESIAN_POINT ( 'NONE',  ( -8.500869906239362450, -77.86249999999999716, 4.334382246026820873 ) ) ;
#55831 = CARTESIAN_POINT ( 'NONE',  ( 8.956105305515906778, -78.80351547480260876, -5.945488880285457967 ) ) ;
#55832 = EDGE_LOOP ( 'NONE', ( #5000, #23437, #19489, #50164, #19012, #33293 ) ) ;
#55833 = CARTESIAN_POINT ( 'NONE',  ( 10.15833271782000047, -17.78011549213000109, 7.756208840363000512 ) ) ;
#55834 = CARTESIAN_POINT ( 'NONE',  ( -9.128193891305592444, -79.37730585991548082, 2.631818823965640597 ) ) ;
#55835 = EDGE_CURVE ( 'NONE', #2377, #18636, #32036, .T. ) ;
#55836 = CARTESIAN_POINT ( 'NONE',  ( 0.4354618354436000649, -78.37228808732000118, -11.90553545880999842 ) ) ;
#55837 = CYLINDRICAL_SURFACE ( 'NONE', #47649, 11.65000000000000036 ) ;
#55838 = DIRECTION ( 'NONE',  ( 1.000000000000000000, 0.000000000000000000, 0.000000000000000000 ) ) ;
#55839 = CARTESIAN_POINT ( 'NONE',  ( 10.99434377831019560, -78.83240919558934934, 4.758605572679748263 ) ) ;
#55840 = CARTESIAN_POINT ( 'NONE',  ( 8.554126827399000987, -80.09570377856319112, -7.255689219360999864 ) ) ;
#55841 = EDGE_CURVE ( 'NONE', #9701, #37791, #34183, .T. ) ;
#55842 = VERTEX_POINT ( 'NONE', #51940 ) ;
#55843 = ORIENTED_EDGE ( 'NONE', *, *, #15855, .F. ) ;
#55844 = CARTESIAN_POINT ( 'NONE',  ( 7.475510798934743129, -77.40022076363275971, 5.447743833593036378 ) ) ;
#55845 = CARTESIAN_POINT ( 'NONE',  ( 9.507661145905998978, -77.69802481315399234, -5.611464101879999333 ) ) ;
#55846 = AXIS2_PLACEMENT_3D ( 'NONE', #8413, #18454, #49464 ) ;
#55847 = CARTESIAN_POINT ( 'NONE',  ( 5.263204982374492857, -78.01377408750333586, -9.905568246058097159 ) ) ;
#55848 = CARTESIAN_POINT ( 'NONE',  ( -0.6549273519428999712, -78.90017770130199892, 1.475891481164999908 ) ) ;
#55849 = DIRECTION ( 'NONE',  ( -1.996944831318000060E-10, 1.000000000000000000, 5.653829486504999768E-11 ) ) ;
#55850 = CARTESIAN_POINT ( 'NONE',  ( 0.000000000000000000, -76.75499999999999545, 0.000000000000000000 ) ) ;
#55851 = CARTESIAN_POINT ( 'NONE',  ( -0.9536002873971000104, -79.31364285822999705, 1.318830682536000110 ) ) ;
#55852 = CARTESIAN_POINT ( 'NONE',  ( -10.72788417900999924, -78.97383311221699387, 2.643935454766999982 ) ) ;
#55853 = CARTESIAN_POINT ( 'NONE',  ( 1.931087888240000217, -60.11584731951999316, -12.71658872087999903 ) ) ;
#55854 = AXIS2_PLACEMENT_3D ( 'NONE', #42273, #19834, #23954 ) ;
#55855 = DIRECTION ( 'NONE',  ( 1.000000000000000000, 0.000000000000000000, 0.000000000000000000 ) ) ;
#55856 = CARTESIAN_POINT ( 'NONE',  ( -3.380079031964000169, -86.18656799980000471, 0.3693951276397000050 ) ) ;
#55857 = ORIENTED_EDGE ( 'NONE', *, *, #26817, .F. ) ;
#55858 = B_SPLINE_CURVE_WITH_KNOTS ( 'NONE', 3,
 ( #44676, #40238, #11567, #25702, #2710, #24554 ),
 .UNSPECIFIED., .F., .F.,
 ( 4, 1, 1, 4 ),
 ( 0.000000000000000000, 0.3333333333333000081, 0.6666666666667000474, 1.000000000000000000 ),
 .UNSPECIFIED. ) ;
#55859 = CARTESIAN_POINT ( 'NONE',  ( -10.80118587004463393, -77.19999999999998863, 1.952987246723529413 ) ) ;
#55860 = CARTESIAN_POINT ( 'NONE',  ( -9.517692138466999907, -76.32513885926499597, -6.653162853725000048 ) ) ;
#55861 = CARTESIAN_POINT ( 'NONE',  ( -0.2771659042208530210, -77.97711776262842420, 10.74664504278661781 ) ) ;
#55862 = CARTESIAN_POINT ( 'NONE',  ( 4.374544387491000386, -77.28864099784598807, -11.15253550093999912 ) ) ;
#55863 = EDGE_CURVE ( 'NONE', #21570, #2251, #35013, .T. ) ;
#55864 = CARTESIAN_POINT ( 'NONE',  ( -7.646944981223999349, -18.80364172516999943, 10.19022195330999914 ) ) ;
#55865 = VECTOR ( 'NONE', #35899, 1000.000000000000000 ) ;
#55866 = CARTESIAN_POINT ( 'NONE',  ( 0.03840548688684078393, -77.87740459572674467, -1.273959412799388291 ) ) ;
#55867 = CARTESIAN_POINT ( 'NONE',  ( -2.995811057868809524, -2.703889681057667360, 1.977980227838953775 ) ) ;
#55868 = CARTESIAN_POINT ( 'NONE',  ( 10.45021209859945799, -80.86923990539705187, 2.519930479213339680 ) ) ;
#55869 = CARTESIAN_POINT ( 'NONE',  ( -8.985695946343000173, -78.61622446787298202, 3.150816496261000133 ) ) ;
#55870 = CARTESIAN_POINT ( 'NONE',  ( -10.07979664880000037, -76.57175206120300004, 3.736335038366999761 ) ) ;
#55871 = CARTESIAN_POINT ( 'NONE',  ( 8.993546968190999635, -77.65971154453498571, -6.388884668894999841 ) ) ;
#55872 = CARTESIAN_POINT ( 'NONE',  ( 9.406806676749999596, -76.84443103653305229, -7.895227358184000899 ) ) ;
#55873 = CARTESIAN_POINT ( 'NONE',  ( 0.6259563484655999988, -80.65615852947209419, -10.89273910470000040 ) ) ;
#55874 = ORIENTED_EDGE ( 'NONE', *, *, #51400, .F. ) ;
#55875 = AXIS2_PLACEMENT_3D ( 'NONE', #30512, #11949, #42959 ) ;
#55876 = CARTESIAN_POINT ( 'NONE',  ( -0.9657971644277000278, -82.28243200420399717, -0.9195906491977999808 ) ) ;
#55877 = CARTESIAN_POINT ( 'NONE',  ( 1.930638663164000235, -60.02122063256000217, -12.72375916875000179 ) ) ;
#55878 = CARTESIAN_POINT ( 'NONE',  ( -7.710118476742000126, -20.25022860572000027, -10.18499221090000084 ) ) ;
#55879 = CARTESIAN_POINT ( 'NONE',  ( -3.513443458492000016, -78.43354160802699937, -10.65240647004999985 ) ) ;
#55880 = CARTESIAN_POINT ( 'NONE',  ( 10.71556987377000070, -79.57690251541698956, 2.374990294079000197 ) ) ;
#55881 = CARTESIAN_POINT ( 'NONE',  ( 8.541150802303999257, -25.00800189280999675, -9.205830468593999782 ) ) ;
#55882 = CARTESIAN_POINT ( 'NONE',  ( -2.680836717414254444, -83.40208332392113277, -3.038406753995844145 ) ) ;
#55883 = CARTESIAN_POINT ( 'NONE',  ( -1.123220714122999953, -76.95895616928899585, 12.10057525372000065 ) ) ;
#55884 = CARTESIAN_POINT ( 'NONE',  ( 7.974576219238914021, -78.51319164874669809, 8.644719456487203857 ) ) ;
#55885 = DIRECTION ( 'NONE',  ( -1.044282756598000039E-09, -1.000000000000000000, 6.141137129051000072E-09 ) ) ;
#55886 = ORIENTED_EDGE ( 'NONE', *, *, #15164, .T. ) ;
#55887 = CARTESIAN_POINT ( 'NONE',  ( -0.8890245797214872958, -80.03847917517971666, 0.8782872498970755171 ) ) ;
#55888 = CARTESIAN_POINT ( 'NONE',  ( -1.199500263597274685, -80.44791666666668561, 0.9218200799623673669 ) ) ;
#55889 = CARTESIAN_POINT ( 'NONE',  ( 7.633403241802001027, -55.41350283619000550, -10.18127013546999926 ) ) ;
#55890 = CARTESIAN_POINT ( 'NONE',  ( -5.907589619820999616, -78.09811028477999173, 9.593191298321000815 ) ) ;
#55891 = CARTESIAN_POINT ( 'NONE',  ( 0.3417741717619000030, -78.10080061187998979, -1.393295110451999941 ) ) ;
#55892 = CARTESIAN_POINT ( 'NONE',  ( 10.48543666025108401, -77.59166666666668277, 6.043427764450814976 ) ) ;
#55893 = CARTESIAN_POINT ( 'NONE',  ( 0.5361682633709462520, -81.90381801127249162, -1.413805704914858241 ) ) ;
#55894 = VECTOR ( 'NONE', #12908, 1000.000000000000114 ) ;
#55895 = DIRECTION ( 'NONE',  ( 0.7071067811864981678, 0.000000000000000000, -0.7071067811865970887 ) ) ;
#55896 = CARTESIAN_POINT ( 'NONE',  ( 7.596835002782722057, -77.99791666666666856, -5.838193839761678383 ) ) ;
#55897 = CARTESIAN_POINT ( 'NONE',  ( 1.093259379017939681, -80.89232953274604654, 0.6295269788946473710 ) ) ;
#55898 = VERTEX_POINT ( 'NONE', #3484 ) ;
#55899 = CARTESIAN_POINT ( 'NONE',  ( -0.8383438467763877355, -81.66698421707488365, -0.9271207089584655447 ) ) ;
#55900 = EDGE_CURVE ( 'NONE', #11974, #26900, #39936, .T. ) ;
#55901 = CIRCLE ( 'NONE', #29492, 1.000000000000000000 ) ;
#55902 = CARTESIAN_POINT ( 'NONE',  ( -1.629741404508999958, -78.77781295235500636, 11.02717296151999982 ) ) ;
#55903 = CARTESIAN_POINT ( 'NONE',  ( 0.000000000000000000, -76.75499999999999545, 0.000000000000000000 ) ) ;
#55904 = ORIENTED_EDGE ( 'NONE', *, *, #27610, .T. ) ;
#55905 = EDGE_LOOP ( 'NONE', ( #32856, #5211, #18482, #3258 ) ) ;
#55906 = CARTESIAN_POINT ( 'NONE',  ( 1.018949564034999922, -81.36366980083398914, 1.122801824928000070 ) ) ;
#55907 = VERTEX_POINT ( 'NONE', #52789 ) ;
#55908 = DIRECTION ( 'NONE',  ( 1.000000000000000000, 0.000000000000000000, 0.000000000000000000 ) ) ;
#55909 = VERTEX_POINT ( 'NONE', #57500 ) ;
#55910 = CARTESIAN_POINT ( 'NONE',  ( 1.389926494651000155, -17.37618663744999736, 12.65988803923000106 ) ) ;
#55911 = CIRCLE ( 'NONE', #53065, 6.100000000000000533 ) ;
#55912 = DIRECTION ( 'NONE',  ( 1.000000000000000000, 0.000000000000000000, 0.000000000000000000 ) ) ;
#55913 = DIRECTION ( 'NONE',  ( 1.000000000000000000, 0.000000000000000000, 0.000000000000000000 ) ) ;
#55914 = CARTESIAN_POINT ( 'NONE',  ( -13.13047446164998711, -56.01421830981000483, 0.8260994316375004365 ) ) ;
#55915 = AXIS2_PLACEMENT_3D ( 'NONE', #32981, #36261, #19430 ) ;
#55916 = CARTESIAN_POINT ( 'NONE',  ( -5.941820572504999731, -79.24616001420199041, 8.071079272148001138 ) ) ;
#55917 = CARTESIAN_POINT ( 'NONE',  ( 5.414928535605519677, -78.27494612867262447, -7.499721313425219194 ) ) ;
#55918 = CARTESIAN_POINT ( 'NONE',  ( -2.460623815919318336, -79.39618386848788134, 8.998003677019603685 ) ) ;
#55919 = ADVANCED_FACE ( 'NONE', ( #8487 ), #30179, .T. ) ;
#55920 = ORIENTED_EDGE ( 'NONE', *, *, #22628, .T. ) ;
#55921 = VERTEX_POINT ( 'NONE', #17944 ) ;
#55922 = CARTESIAN_POINT ( 'NONE',  ( 12.65375411750999923, -57.05022861049000227, 1.750000000000000000 ) ) ;
#55923 = CARTESIAN_POINT ( 'NONE',  ( -12.80000000000000071, -0.1000000000000002554, 0.000000000000000000 ) ) ;
#55924 = CARTESIAN_POINT ( 'NONE',  ( 1.980584515752000119, -60.06485146591000301, -12.76303204605000197 ) ) ;
#55925 = CARTESIAN_POINT ( 'NONE',  ( 9.259046916275000427, -78.54404407152598822, 2.905298533503999803 ) ) ;
#55926 = FACE_OUTER_BOUND ( 'NONE', #54781, .T. ) ;
#55927 = DIRECTION ( 'NONE',  ( 1.000000000000000000, 0.000000000000000000, 0.000000000000000000 ) ) ;
#55928 = CARTESIAN_POINT ( 'NONE',  ( 11.81567892624999949, -79.00458388498999796, 1.523613136442999894 ) ) ;
#55929 = CARTESIAN_POINT ( 'NONE',  ( -1.530783851654999861, -80.73388962642000877, 0.7460011833842999929 ) ) ;
#55930 = B_SPLINE_CURVE_WITH_KNOTS ( 'NONE', 3,
 ( #38894, #16763, #30889, #34163, #7031, #17041, #48352, #25032, #38610, #7892, #56625, #34741, #11755, #29734, #52769 ),
 .UNSPECIFIED., .F., .F.,
 ( 4, 1, 1, 1, 1, 1, 1, 1, 1, 1, 1, 1, 4 ),
 ( 0.000000000000000000, 0.08333611588665000569, 0.1666676715620999949, 0.2500039875833999781, 0.3333306964953999807, 0.4166666792817999565, 0.4999999999924999994, 0.5833333197091999933, 0.6666692694150000431, 0.7499959719902999922, 0.8333323089881000678, 0.9166638425153998959, 1.000000000000000000 ),
 .UNSPECIFIED. ) ;
#55931 = CARTESIAN_POINT ( 'NONE',  ( -8.247965593175072385, -76.63679069186150628, 8.368539974147305216 ) ) ;
#55932 = DIRECTION ( 'NONE',  ( 0.000000000000000000, -1.000000000000000000, 0.000000000000000000 ) ) ;
#55934 = VECTOR ( 'NONE', #21282, 1000.000000000000227 ) ;
#55933 = CARTESIAN_POINT ( 'NONE',  ( -0.03127831795120067371, -79.37340073922844397, -1.510815432793727986 ) ) ;
#55935 = CARTESIAN_POINT ( 'NONE',  ( -5.548464554217999556, -78.58398667140099292, -8.076689350464999251 ) ) ;
#55936 = CARTESIAN_POINT ( 'NONE',  ( -1.750000000001000089, -19.24899163674999869, -12.60354432393000046 ) ) ;
#55937 = CARTESIAN_POINT ( 'NONE',  ( 0.000000000000000000, -0.2000000000000000111, -9.000000000000271783 ) ) ;
#55939 = CARTESIAN_POINT ( 'NONE',  ( 1.629367637659999923, -18.31736356602000271, -12.46114270826000059 ) ) ;
#55938 = DIRECTION ( 'NONE',  ( 0.000000000000000000, 1.000000000000000000, 0.000000000000000000 ) ) ;
#55940 = FACE_OUTER_BOUND ( 'NONE', #3047, .T. ) ;
#55941 = CARTESIAN_POINT ( 'NONE',  ( 8.724294832244513742, -79.99999999999995737, -3.890814657221138173 ) ) ;
#55942 = CARTESIAN_POINT ( 'NONE',  ( 0.000000000000000000, -75.10000000284179578, 7.200000000000000178 ) ) ;
#55943 = CARTESIAN_POINT ( 'NONE',  ( 3.530886011689700510, -1.499221606517874061, -0.03292542109241022863 ) ) ;
#55944 = VERTEX_POINT ( 'NONE', #49235 ) ;
#55945 = CARTESIAN_POINT ( 'NONE',  ( 1.750000000000000000, -55.55000000209000177, -12.50000000000000000 ) ) ;
#55946 = CARTESIAN_POINT ( 'NONE',  ( 7.342377162853137129, -60.03019609282338109, -8.190817883596540838 ) ) ;
#55947 = CARTESIAN_POINT ( 'NONE',  ( -8.852886909552351469, -77.64153493090338998, 7.764045341703079472 ) ) ;
#55948 = CARTESIAN_POINT ( 'NONE',  ( 1.179985190145098173, -78.37701668321712134, 0.4119397061850897934 ) ) ;
#55949 = CARTESIAN_POINT ( 'NONE',  ( -8.641832836834998588, -79.85648669611498462, 4.277501108045999700 ) ) ;
#55950 = CARTESIAN_POINT ( 'NONE',  ( 7.287838312904000304, -78.12030371036000531, -10.78085041437000058 ) ) ;
#55951 = LINE ( 'NONE', #33495, #14834 ) ;
#55952 = CARTESIAN_POINT ( 'NONE',  ( -2.002768801220407013, -79.48993535946543432, 10.56433384562239475 ) ) ;
#55953 = AXIS2_PLACEMENT_3D ( 'NONE', #3728, #13744, #45062 ) ;
#55954 = CARTESIAN_POINT ( 'NONE',  ( 2.854995274860000265, -79.02853998579799111, -9.096945719287999665 ) ) ;
#55955 = DIRECTION ( 'NONE',  ( 0.9999548435846228323, 0.000000000000000000, 0.009503199022040118363 ) ) ;
#55956 = CARTESIAN_POINT ( 'NONE',  ( 4.360500596435000098, -77.21275830873099721, 9.871531364361999294 ) ) ;
#55957 = CARTESIAN_POINT ( 'NONE',  ( -1.448341597990999929, -81.87269880242300246, 0.6895295675035000293 ) ) ;
#55958 = DIRECTION ( 'NONE',  ( 1.000000000000000000, 0.000000000000000000, 0.000000000000000000 ) ) ;
#55960 = CARTESIAN_POINT ( 'NONE',  ( 2.028166799595999770, -1.019127687536000026, -3.466423845304999585 ) ) ;
#55959 = CARTESIAN_POINT ( 'NONE',  ( -3.689388438892000188, -84.30604218908899838, 1.447205210676999920 ) ) ;
#55961 = CARTESIAN_POINT ( 'NONE',  ( 8.150225256662000817, -79.84085194988499268, -4.374508917085999649 ) ) ;
#55962 = CARTESIAN_POINT ( 'NONE',  ( -8.485281374238999419, -60.04999999966999980, 8.485281374238999419 ) ) ;
#55963 = CARTESIAN_POINT ( 'NONE',  ( 4.585445119925699586, -80.26028109100353447, -9.723566880156193193 ) ) ;
#55964 = CARTESIAN_POINT ( 'NONE',  ( -7.100359491673154722, -77.16761677373057182, -8.072272176001158428 ) ) ;
#55965 = CARTESIAN_POINT ( 'NONE',  ( 14.00000000000000000, -91.29999999999999716, -8.151435677387999117E-14 ) ) ;
#55966 = ORIENTED_EDGE ( 'NONE', *, *, #48048, .T. ) ;
#55967 = ORIENTED_EDGE ( 'NONE', *, *, #46836, .F. ) ;
#55968 = CARTESIAN_POINT ( 'NONE',  ( 0.4713521909880000194, -79.00577527788799159, 12.02020425643999957 ) ) ;
#55969 = EDGE_CURVE ( 'NONE', #38447, #55909, #5448, .T. ) ;
#55970 = CARTESIAN_POINT ( 'NONE',  ( 1.115616509574796078, -78.30837352953511754, -0.6527249703762391109 ) ) ;
#55971 = LINE ( 'NONE', #29090, #1124 ) ;
#55972 = ORIENTED_EDGE ( 'NONE', *, *, #42483, .F. ) ;
#55973 = EDGE_CURVE ( 'NONE', #4702, #27444, #12628, .T. ) ;
#55974 = CARTESIAN_POINT ( 'NONE',  ( -7.140570215937000143, -77.54944927882600325, 9.562832187120999805 ) ) ;
#55975 = ORIENTED_EDGE ( 'NONE', *, *, #36496, .T. ) ;
#55976 = ORIENTED_EDGE ( 'NONE', *, *, #44919, .T. ) ;
#55977 = CARTESIAN_POINT ( 'NONE',  ( 2.813789756862229652, -78.85416666666665719, 10.47020627418440064 ) ) ;
#55978 = ORIENTED_EDGE ( 'NONE', *, *, #50580, .F. ) ;
#55979 = AXIS2_PLACEMENT_3D ( 'NONE', #40177, #36332, #26305 ) ;
#55980 = CARTESIAN_POINT ( 'NONE',  ( -0.3709083427993999926, -80.53117300822900404, -3.528028788725999565 ) ) ;
#55981 = CARTESIAN_POINT ( 'NONE',  ( 6.183015154944156322, -79.21846095476607275, 7.212400455461417614 ) ) ;
#55982 = ORIENTED_EDGE ( 'NONE', *, *, #52097, .F. ) ;
#55984 = EDGE_CURVE ( 'NONE', #35168, #40044, #41493, .T. ) ;
#55983 = CARTESIAN_POINT ( 'NONE',  ( 0.3045730287770247458, -82.74492401537455066, -1.212283547811195739 ) ) ;
#55985 = B_SPLINE_CURVE_WITH_KNOTS ( 'NONE', 3,
 ( #38774, #25483, #15478, #33758, #11064, #3063 ),
 .UNSPECIFIED., .F., .F.,
 ( 4, 1, 1, 4 ),
 ( 0.000000000000000000, 0.3333333333333000081, 0.6666666666667000474, 1.000000000000000000 ),
 .UNSPECIFIED. ) ;
#55986 = ORIENTED_EDGE ( 'NONE', *, *, #33671, .T. ) ;
#55987 = CARTESIAN_POINT ( 'NONE',  ( -7.641012386057000505, -60.08917565288000162, 10.18589234709999936 ) ) ;
#55988 = EDGE_LOOP ( 'NONE', ( #25753, #12884, #42756, #42467 ) ) ;
#55989 = CARTESIAN_POINT ( 'NONE',  ( -5.413904038987160661, -80.58333333333332860, -9.393203674808278336 ) ) ;
#55990 = CARTESIAN_POINT ( 'NONE',  ( 1.507222751313145093, -77.98526986442249154, -0.2769236843535003434 ) ) ;
#55991 = DIRECTION ( 'NONE',  ( -0.7071067811865969777, -0.7071067811864980568, 1.236220812569996176E-09 ) ) ;
#55992 = AXIS2_PLACEMENT_3D ( 'NONE', #51371, #2075, #50203 ) ;
#55993 = FACE_OUTER_BOUND ( 'NONE', #51267, .T. ) ;
#55994 = CARTESIAN_POINT ( 'NONE',  ( 9.512131559252001267, -77.98414325622765375, -1.920953556448999899 ) ) ;
#55995 = CARTESIAN_POINT ( 'NONE',  ( -1.963210506780999953, -76.51264080250500399, -11.00998129987999974 ) ) ;
#55996 = CARTESIAN_POINT ( 'NONE',  ( 10.14846770183394931, -76.32381270956288688, -3.633859120905852613 ) ) ;
#55997 = CARTESIAN_POINT ( 'NONE',  ( -2.879226727952121312, -78.59583333333331723, 10.71369944335146052 ) ) ;
#55998 = CARTESIAN_POINT ( 'NONE',  ( 1.857189518626999991, -76.68518679586200903, 11.07404950498000140 ) ) ;
#55999 = CARTESIAN_POINT ( 'NONE',  ( -8.158649804916262127, -78.63917908708265259, -4.359350819807166211 ) ) ;
#56000 = CARTESIAN_POINT ( 'NONE',  ( 8.381245741137949068, -76.51127116153249119, 8.234743652916119316 ) ) ;
#56001 = CARTESIAN_POINT ( 'NONE',  ( -0.8465867926663999121, -80.70141679342098939, -0.9556525628790000226 ) ) ;
#56002 = CARTESIAN_POINT ( 'NONE',  ( -9.038121182379606822, -80.14837150988061865, -6.270795222358383825 ) ) ;
#56003 = CARTESIAN_POINT ( 'NONE',  ( 5.838193839761673054, -77.12291666666669698, 7.596835002782728274 ) ) ;
#56004 = CARTESIAN_POINT ( 'NONE',  ( 3.582810602826999702, -82.16928455456799441, 0.3614017272707000239 ) ) ;
#56005 = CARTESIAN_POINT ( 'NONE',  ( 10.14252871893000041, -79.37232516803899784, 6.568753285854999291 ) ) ;
#56006 = CARTESIAN_POINT ( 'NONE',  ( -10.10146701087682963, -78.07232890951112836, 3.678169913406422520 ) ) ;
#56007 = CARTESIAN_POINT ( 'NONE',  ( 0.4362293792333048481, -82.94664917577976837, 1.171447771671162652 ) ) ;
#56008 = CARTESIAN_POINT ( 'NONE',  ( 0.000000000000000000, -59.58578169018999660, 13.15643568216998638 ) ) ;
#56009 = CARTESIAN_POINT ( 'NONE',  ( -3.399999999999999911, -78.69999997992952956, 5.715921273723000819E-07 ) ) ;
#56010 = CARTESIAN_POINT ( 'NONE',  ( -6.589344923537027832, -76.27752133694943382, -9.728425524022272342 ) ) ;
#56011 = CARTESIAN_POINT ( 'NONE',  ( 10.01234990228999955, -18.70150862776000267, 7.653559502277999194 ) ) ;
#56012 = DIRECTION ( 'NONE',  ( 0.000000000000000000, -1.000000000000000000, -6.735284179502000863E-11 ) ) ;
#56013 = VECTOR ( 'NONE', #36513, 1000.000000000000000 ) ;
#56014 = CARTESIAN_POINT ( 'NONE',  ( 1.199500263597271799, -77.69791666666667140, -0.9218200799623701425 ) ) ;
#56015 = DIRECTION ( 'NONE',  ( 0.000000000000000000, 0.000000000000000000, -1.000000000000000000 ) ) ;
#56016 = CARTESIAN_POINT ( 'NONE',  ( -7.624341766639000539, -23.26485146254000114, -10.42531125024000005 ) ) ;
#56017 = EDGE_CURVE ( 'NONE', #17378, #47194, #52784, .T. ) ;
#56018 = CARTESIAN_POINT ( 'NONE',  ( 9.943037443271171227, -78.16907139213840594, -4.146583387419329192 ) ) ;
#56019 =( LENGTH_UNIT ( ) NAMED_UNIT ( * ) SI_UNIT ( .MILLI., .METRE. ) );
#56020 = CARTESIAN_POINT ( 'NONE',  ( -10.79326785783000098, -79.36452526662860407, -1.992331681952000055 ) ) ;
#56021 = CARTESIAN_POINT ( 'NONE',  ( 12.00296638904000091, -76.01348777726998662, 1.190414638386999790 ) ) ;
#56022 = ORIENTED_EDGE ( 'NONE', *, *, #11328, .F. ) ;
#56023 = CARTESIAN_POINT ( 'NONE',  ( -3.707169433487000454, -86.43863211209799147, 1.047003938644999854 ) ) ;
#56024 = CIRCLE ( 'NONE', #34335, 9.000000000000000000 ) ;
#56025 = CARTESIAN_POINT ( 'NONE',  ( -6.032763990770999563, -81.13038518513180009, 9.116036532382999269 ) ) ;
#56026 = CARTESIAN_POINT ( 'NONE',  ( 9.114089478082622264, -78.33640746566551627, -1.588185711488315111 ) ) ;
#56027 = CARTESIAN_POINT ( 'NONE',  ( 9.697390092161668917, -53.82767731314377357, 8.266602378548485675 ) ) ;
#56028 = CARTESIAN_POINT ( 'NONE',  ( 4.275724345439000373, -77.05780398220699112, -10.36997068233999997 ) ) ;
#56029 = LINE ( 'NONE', #25010, #42723 ) ;
#56030 = CARTESIAN_POINT ( 'NONE',  ( 8.977320902561999105, -79.16941197858199075, 3.091814932086999868 ) ) ;
#56031 = CARTESIAN_POINT ( 'NONE',  ( -1.462746796095000024, -81.40659681158000183, -0.3322225316158000097 ) ) ;
#56032 = FACE_OUTER_BOUND ( 'NONE', #33811, .T. ) ;
#56033 = CIRCLE ( 'NONE', #435, 4.299999999999999822 ) ;
#56034 = DIRECTION ( 'NONE',  ( -1.000000000000000000, 0.000000000000000000, 0.000000000000000000 ) ) ;
#56035 = ORIENTED_EDGE ( 'NONE', *, *, #56145, .F. ) ;
#56036 = CARTESIAN_POINT ( 'NONE',  ( -2.921318291229240138, -0.8958333333332216819, 1.685599492705018632 ) ) ;
#56037 = CARTESIAN_POINT ( 'NONE',  ( 2.402961585942242184, -78.97529329368650508, -2.655007460227098992 ) ) ;
#56038 = ORIENTED_EDGE ( 'NONE', *, *, #10862, .F. ) ;
#56039 = CARTESIAN_POINT ( 'NONE',  ( 0.1443438050804999873, -78.04448313310169283, 1.325798245762999983 ) ) ;
#56040 = CARTESIAN_POINT ( 'NONE',  ( -4.306297750730000651, -78.90007827033099375, -10.17515077672999979 ) ) ;
#56041 = CARTESIAN_POINT ( 'NONE',  ( 1.300393966725080341, -77.63618784400628670, -9.236768800945032609 ) ) ;
#56042 = CARTESIAN_POINT ( 'NONE',  ( -0.9999999970599000587, -81.20000000293998710, 6.999999982650000341 ) ) ;
#56043 = EDGE_LOOP ( 'NONE', ( #41012, #23447, #53993, #37137, #8989 ) ) ;
#56044 = ADVANCED_FACE ( 'NONE', ( #22060 ), #20765, .F. ) ;
#56045 = CARTESIAN_POINT ( 'NONE',  ( 12.10970598371999962, -77.58985457952199738, 2.037349774713999917 ) ) ;
#56046 = CARTESIAN_POINT ( 'NONE',  ( 10.95487136366999970, -78.29604510612898594, -1.495655693045000012 ) ) ;
#56047 = DIRECTION ( 'NONE',  ( 0.000000000000000000, -1.000000000000000000, 0.000000000000000000 ) ) ;
#56048 = EDGE_LOOP ( 'NONE', ( #20482, #33005, #57126, #11176 ) ) ;
#56049 = EDGE_LOOP ( 'NONE', ( #22637, #49392, #3365, #9360, #37673, #12746, #53211, #14639, #4279, #34603, #11555 ) ) ;
#56050 = EDGE_LOOP ( 'NONE', ( #959, #11600, #21865, #52713, #30950 ) ) ;
#56051 = CARTESIAN_POINT ( 'NONE',  ( -0.8920742119596244413, -80.53887022317101696, 0.8750902781345917258 ) ) ;
#56052 = CARTESIAN_POINT ( 'NONE',  ( 1.250000000000000000, -82.24999999999998579, 0.000000000000000000 ) ) ;
#56053 = CARTESIAN_POINT ( 'NONE',  ( -9.687172913667000174, -80.14036198365600683, -1.248753675804000096 ) ) ;
#56054 = AXIS2_PLACEMENT_3D ( 'NONE', #19403, #37394, #14959 ) ;
#56055 = ORIENTED_EDGE ( 'NONE', *, *, #54248, .F. ) ;
#56057 = EDGE_CURVE ( 'NONE', #53060, #29148, #55659, .T. ) ;
#56056 = CARTESIAN_POINT ( 'NONE',  ( -12.70451647735341005, -24.55458569106719224, -1.498866843992721076 ) ) ;
#56058 = CARTESIAN_POINT ( 'NONE',  ( 0.9322037676993999433, -78.70521297495899660, -10.87687281004000006 ) ) ;
#56059 = EDGE_LOOP ( 'NONE', ( #29309, #16114, #24957, #23147 ) ) ;
#56060 = CARTESIAN_POINT ( 'NONE',  ( -12.66008999772000010, -24.62705329347999950, -1.387101471715999956 ) ) ;
#56061 = ADVANCED_FACE ( 'NONE', ( #53077 ), #8201, .F. ) ;
#56062 = CARTESIAN_POINT ( 'NONE',  ( -3.399395987256130347, -78.72609999968184979, 0.06408526995191166087 ) ) ;
#56063 = DIRECTION ( 'NONE',  ( 0.000000000000000000, 0.000000000000000000, -1.000000000000000000 ) ) ;
#56064 = CARTESIAN_POINT ( 'NONE',  ( 1.500000000000000000, -80.25000000000000000, 0.000000000000000000 ) ) ;
#56065 = DIRECTION ( 'NONE',  ( 0.000000000000000000, 1.000000000000000000, 0.000000000000000000 ) ) ;
#56066 = CARTESIAN_POINT ( 'NONE',  ( -1.392423410630999929E-14, -75.80000000000001137, 0.000000000000000000 ) ) ;
#56067 = AXIS2_PLACEMENT_3D ( 'NONE', #42978, #34382, #52413 ) ;
#56068 = CARTESIAN_POINT ( 'NONE',  ( -12.74331394910258197, -18.47353206582842589, -1.980611464662582089 ) ) ;
#56069 = CARTESIAN_POINT ( 'NONE',  ( 1.379693150491080988, -79.13274274277868869, 0.6107116112576068678 ) ) ;
#56070 = CARTESIAN_POINT ( 'NONE',  ( -9.611650271896833075, -79.64166666666665151, -5.539808784079895077 ) ) ;
#56071 = CARTESIAN_POINT ( 'NONE',  ( 6.153863461931999623, -76.11465827134000506, -10.66140155521000032 ) ) ;
#56072 = DIRECTION ( 'NONE',  ( 0.000000000000000000, 1.000000000000000000, 0.000000000000000000 ) ) ;
#56073 = EDGE_CURVE ( 'NONE', #34639, #31619, #14136, .T. ) ;
#56074 = DIRECTION ( 'NONE',  ( 0.000000000000000000, -1.000000000000000000, 0.000000000000000000 ) ) ;
#56075 = CARTESIAN_POINT ( 'NONE',  ( 11.81418954875000082, -78.71961295229000655, 3.289986436736999753 ) ) ;
#56076 = CARTESIAN_POINT ( 'NONE',  ( -3.699256142337000064, -77.03324258761200838, 11.71059914860999918 ) ) ;
#56077 = CARTESIAN_POINT ( 'NONE',  ( -1.359416874709192810E-05, -0.8285695117701413759, -3.421591653122290300 ) ) ;
#56078 = CARTESIAN_POINT ( 'NONE',  ( 4.229028970798999865, -77.89639184420045126, 11.24885535038115592 ) ) ;
#56079 = CARTESIAN_POINT ( 'NONE',  ( 10.93160348586000019, -79.01798567075552171, 2.513594203403000105 ) ) ;
#56080 = ORIENTED_EDGE ( 'NONE', *, *, #16294, .T. ) ;
#56081 = CARTESIAN_POINT ( 'NONE',  ( -1.512396851278637433, -80.23374261172247657, 0.3224664540911364452 ) ) ;
#56082 = CARTESIAN_POINT ( 'NONE',  ( 2.642581390489999738, -77.18224640713208373, 9.340684087520999768 ) ) ;
#56083 = CARTESIAN_POINT ( 'NONE',  ( 1.249999999999999778, -79.26041666666667140, 0.1636246173744711763 ) ) ;
#56084 = CARTESIAN_POINT ( 'NONE',  ( -0.1636246173744726473, -82.88541666666664298, 1.249999999999999112 ) ) ;
#56085 = CARTESIAN_POINT ( 'NONE',  ( 1.229508168781000110, -2.945103494984999681, -3.669964256485999776 ) ) ;
#56086 = EDGE_CURVE ( 'NONE', #54376, #26901, #17643, .T. ) ;
#56087 = CARTESIAN_POINT ( 'NONE',  ( 7.599120132820000428, -78.26244375222299254, 9.499258065358000991 ) ) ;
#56088 = DIRECTION ( 'NONE',  ( 1.000000000000000000, 0.000000000000000000, 2.582622310454000054E-11 ) ) ;
#56090 = CARTESIAN_POINT ( 'NONE',  ( 9.462239583049713687, -76.98776041667790082, 1.239456478693297559 ) ) ;
#56089 = CARTESIAN_POINT ( 'NONE',  ( -10.85214655116546645, -76.16855472728988730, 4.504555557915027819 ) ) ;
#56091 = CARTESIAN_POINT ( 'NONE',  ( 3.413317904202999742, -79.37628491221198601, 10.36940822202999790 ) ) ;
#56092 = DIRECTION ( 'NONE',  ( 0.000000000000000000, 0.000000000000000000, -1.000000000000000000 ) ) ;
#56093 = VERTEX_POINT ( 'NONE', #46290 ) ;
#56094 = ADVANCED_FACE ( 'NONE', ( #14666 ), #5817, .F. ) ;
#56095 = DIRECTION ( 'NONE',  ( 0.9999548435846228323, 0.000000000000000000, 0.009503199022040218977 ) ) ;
#56096 = CARTESIAN_POINT ( 'NONE',  ( -0.2199206942898871420, -79.39661240347331272, -1.482330506908097201 ) ) ;
#56097 = CARTESIAN_POINT ( 'NONE',  ( -3.250000000000000000, -2.500000000000000000, 0.000000000000000000 ) ) ;
#56098 = CARTESIAN_POINT ( 'NONE',  ( -9.778543098509999254, -61.84857981670000271, 8.284584910426000093 ) ) ;
#56099 = VECTOR ( 'NONE', #35769, 1000.000000000000000 ) ;
#56100 = CARTESIAN_POINT ( 'NONE',  ( -10.97527124375647389, -80.09511974427576320, 0.7348162751891352817 ) ) ;
#56101 = CARTESIAN_POINT ( 'NONE',  ( 9.142801562799000692, -79.85277893010599826, 2.792903297447999922 ) ) ;
#56102 = CARTESIAN_POINT ( 'NONE',  ( -10.48543666025109289, -77.94166666666666288, -6.043427764450796325 ) ) ;
#56103 = DIRECTION ( 'NONE',  ( 0.000000000000000000, -1.000000000000000000, 0.000000000000000000 ) ) ;
#56104 = ORIENTED_EDGE ( 'NONE', *, *, #52241, .F. ) ;
#56105 = CARTESIAN_POINT ( 'NONE',  ( 11.09894631581144786, -76.10969828002846782, 1.375318052133717828 ) ) ;
#56106 = CARTESIAN_POINT ( 'NONE',  ( 10.61587740312611494, -79.26335282761201029, -5.228565026272720573 ) ) ;
#56107 = CARTESIAN_POINT ( 'NONE',  ( 1.978577013961021702, -78.62148120184446043, 3.425895126264470125 ) ) ;
#56108 = CARTESIAN_POINT ( 'NONE',  ( 11.97397552426821576, -77.69266700515451873, -1.561850544189498313 ) ) ;
#56110 = CARTESIAN_POINT ( 'NONE',  ( 1.149808842311183410, -81.38230583544610397, 0.4899631106986611084 ) ) ;
#56109 = CARTESIAN_POINT ( 'NONE',  ( 10.42531125074000009, -18.73514854687000053, 7.624341767140999870 ) ) ;
#56111 = CARTESIAN_POINT ( 'NONE',  ( -0.6620585326085253186, -78.73130076599741756, -1.088327036680617255 ) ) ;
#56112 = CARTESIAN_POINT ( 'NONE',  ( -0.1639543601470098144, -82.21523505733837567, -1.249472255457048098 ) ) ;
#56113 = CARTESIAN_POINT ( 'NONE',  ( 3.715424088830954208, -82.09527493484321781, -0.7897374049847233346 ) ) ;
#56114 = CARTESIAN_POINT ( 'NONE',  ( -1.223460966046000076, -77.56523657536999394, 0.2343682768462999888 ) ) ;
#56115 = CARTESIAN_POINT ( 'NONE',  ( -1.980464483675000054, -21.75560170741999855, 12.85140862641999959 ) ) ;
#56116 = CARTESIAN_POINT ( 'NONE',  ( -4.399313083005135461, -79.85792046749108408, 10.05553542149106150 ) ) ;
#56117 = CARTESIAN_POINT ( 'NONE',  ( 12.71162569430416944, -54.56025712733443811, -1.720540999444200914 ) ) ;
#56118 = ORIENTED_EDGE ( 'NONE', *, *, #167, .F. ) ;
#56119 = ORIENTED_EDGE ( 'NONE', *, *, #47202, .T. ) ;
#56120 = CARTESIAN_POINT ( 'NONE',  ( -12.24313050396999891, -77.30790438420399369, 2.928939827507999638 ) ) ;
#56121 = CARTESIAN_POINT ( 'NONE',  ( -3.172678955510176202, -78.70149065425773927, -10.30724250848049017 ) ) ;
#56122 = ORIENTED_EDGE ( 'NONE', *, *, #45586, .T. ) ;
#56123 = CARTESIAN_POINT ( 'NONE',  ( 9.317995624416001377, -16.86762134170999872, 8.588852714006002032 ) ) ;
#56124 = CARTESIAN_POINT ( 'NONE',  ( -9.470785009285748401, -79.39361871371332313, 0.7431805272417587593 ) ) ;
#56125 = CARTESIAN_POINT ( 'NONE',  ( -5.852825220451999932, -78.74677611781000053, 10.54665655014000158 ) ) ;
#56126 = DIRECTION ( 'NONE',  ( 0.000000000000000000, -1.000000000000000000, 0.000000000000000000 ) ) ;
#56127 = DIRECTION ( 'NONE',  ( 1.000000000000000000, 0.000000000000000000, 0.000000000000000000 ) ) ;
#56128 = LINE ( 'NONE', #56418, #33198 ) ;
#56129 = CARTESIAN_POINT ( 'NONE',  ( -5.394429334091999984, -79.98675840655589298, -9.834543342166998769 ) ) ;
#56130 = AXIS2_PLACEMENT_3D ( 'NONE', #2516, #34651, #43248 ) ;
#56131 = ORIENTED_EDGE ( 'NONE', *, *, #15009, .F. ) ;
#56132 = DIRECTION ( 'NONE',  ( 0.000000000000000000, -1.000000000000000000, 0.000000000000000000 ) ) ;
#56133 = VERTEX_POINT ( 'NONE', #5241 ) ;
#56134 = CARTESIAN_POINT ( 'NONE',  ( 8.679236020840834342, -77.37813114295693140, 3.200552027347492778 ) ) ;
#56135 = CARTESIAN_POINT ( 'NONE',  ( 12.50686498859614026, -61.10484291343465202, -1.423095205017603782 ) ) ;
#56136 = CIRCLE ( 'NONE', #47689, 10.69999999999999929 ) ;
#56137 = CARTESIAN_POINT ( 'NONE',  ( 0.1392768204836610790, -77.22392014045128406, 11.21615847476518901 ) ) ;
#56138 = UNCERTAINTY_MEASURE_WITH_UNIT (LENGTH_MEASURE( 1.000000000000000082E-05 ), #16650, 'distance_accuracy_value', 'NONE');
#56139 = CARTESIAN_POINT ( 'NONE',  ( 1.301389418711000223, -77.82021811561179447, -0.5625343731648000389 ) ) ;
#56140 = DIRECTION ( 'NONE',  ( 0.000000000000000000, -1.000000000000000000, 0.000000000000000000 ) ) ;
#56141 = EDGE_CURVE ( 'NONE', #6364, #9942, #557, .T. ) ;
#56142 = CARTESIAN_POINT ( 'NONE',  ( 10.75000000000000000, -80.75000000000000000, 3.489821576044999869E-14 ) ) ;
#56143 = CARTESIAN_POINT ( 'NONE',  ( 1.136899222205000060, -79.14306339479999508, 1.164526648744999893 ) ) ;
#56144 = CARTESIAN_POINT ( 'NONE',  ( -7.579884289019999777, -79.86509741874499468, 7.888812675972000754 ) ) ;
#56145 = EDGE_CURVE ( 'NONE', #39734, #40288, #37868, .T. ) ;
#56146 = CARTESIAN_POINT ( 'NONE',  ( 9.785129497364000173, -79.35060081380299835, -6.997026981537000090 ) ) ;
#56147 = CARTESIAN_POINT ( 'NONE',  ( -9.750000000000000000, -76.19999999999998863, 0.000000000000000000 ) ) ;
#56148 = CARTESIAN_POINT ( 'NONE',  ( -0.6864729959702000617, -83.54105886393099922, -3.479989155495999853 ) ) ;
#56149 = ORIENTED_EDGE ( 'NONE', *, *, #31266, .T. ) ;
#56150 = CARTESIAN_POINT ( 'NONE',  ( -11.68767212001978706, -79.42083333333333428, -3.140974612311364655 ) ) ;
#56151 = CARTESIAN_POINT ( 'NONE',  ( 1.386886761648000066, -79.53075525790998768, -0.9883168548346998872 ) ) ;
#56152 = CARTESIAN_POINT ( 'NONE',  ( 10.20085796994174743, -79.32408745329188093, -3.463766342026746159 ) ) ;
#56153 = CARTESIAN_POINT ( 'NONE',  ( 5.537129384246000541, -78.90287000084299507, 10.62336504503000079 ) ) ;
#56154 = CARTESIAN_POINT ( 'NONE',  ( -8.643969996075000495, -16.74046576158000121, 9.422817222712001950 ) ) ;
#56155 = CARTESIAN_POINT ( 'NONE',  ( -1.244679651825236766, -78.76789556114634649, -0.2779941050184971396 ) ) ;
#56156 = CARTESIAN_POINT ( 'NONE',  ( -3.192737306412670506, -2.215367439888774381, 1.482404185118484818 ) ) ;
#56157 = CARTESIAN_POINT ( 'NONE',  ( 8.169132698983039731, -80.90664037331559655, 6.987377867537430731 ) ) ;
#56158 = CARTESIAN_POINT ( 'NONE',  ( 6.852546780225999612, -78.33198617658298701, -6.611579150008999761 ) ) ;
#56159 = CARTESIAN_POINT ( 'NONE',  ( 0.9801489377500960387, -81.29702506321740429, -0.7880733966296984416 ) ) ;
#56160 = CARTESIAN_POINT ( 'NONE',  ( -10.68734765800000019, -76.97880296949000467, -2.735374635455000369 ) ) ;
#56161 = CARTESIAN_POINT ( 'NONE',  ( 0.000000000000000000, -76.75499999999999545, 0.000000000000000000 ) ) ;
#56162 = CARTESIAN_POINT ( 'NONE',  ( 2.000571476059000098, -81.16626456354109109, -10.72571703250999953 ) ) ;
#56163 = CARTESIAN_POINT ( 'NONE',  ( 0.05911904726909338048, -81.02111415281734708, 1.273296317862433025 ) ) ;
#56164 = ORIENTED_EDGE ( 'NONE', *, *, #6365, .F. ) ;
#56165 = ADVANCED_FACE ( 'NONE', ( #27371 ), #16972, .T. ) ;
#56166 = CARTESIAN_POINT ( 'NONE',  ( -0.6509962010243000030, -81.68124191782798960, 1.163950211895000031 ) ) ;
#56167 = CARTESIAN_POINT ( 'NONE',  ( 2.019183793707000074, -60.58720277209999949, -12.79944116707999946 ) ) ;
#56168 = CARTESIAN_POINT ( 'NONE',  ( -8.107762507646583572, -55.28308356097522847, 7.434020715870143903 ) ) ;
#56169 = CARTESIAN_POINT ( 'NONE',  ( 11.19952915612999966, -78.01168059572700031, -0.6234238306063999424 ) ) ;
#56170 = CARTESIAN_POINT ( 'NONE',  ( 8.318585563179999198, -78.23670594145998791, 7.159970128962999780 ) ) ;
#56171 = CARTESIAN_POINT ( 'NONE',  ( -0.3865739120649937521, -79.45398714331572876, -1.459136857207182114 ) ) ;
#56172 = CARTESIAN_POINT ( 'NONE',  ( 0.3829117639031977549, -85.09791667550908301, -4.033878987895386459 ) ) ;
#56173 = CARTESIAN_POINT ( 'NONE',  ( -12.25072062129000017, -77.00442731979100586, 0.6836512919489999840 ) ) ;
#56174 = CARTESIAN_POINT ( 'NONE',  ( 10.73992744223909845, -78.48307862101303556, 4.792036156107691625 ) ) ;
#56175 = CARTESIAN_POINT ( 'NONE',  ( 1.335937499394570516, -77.91406250010766144, 0.2110757592694599283 ) ) ;
#56176 = ORIENTED_EDGE ( 'NONE', *, *, #54768, .F. ) ;
#56177 = CARTESIAN_POINT ( 'NONE',  ( -0.9344580297550504344, -80.04259503167067180, 0.8300580218378730279 ) ) ;
#56178 = CARTESIAN_POINT ( 'NONE',  ( -7.396918292183171317, -78.05208333333331439, -5.684557159767958723 ) ) ;
#56179 = EDGE_CURVE ( 'NONE', #27205, #46904, #51005, .T. ) ;
#56180 =( GEOMETRIC_REPRESENTATION_CONTEXT ( 3 ) GLOBAL_UNCERTAINTY_ASSIGNED_CONTEXT ( ( #56138 ) ) GLOBAL_UNIT_ASSIGNED_CONTEXT ( ( #16650, #7787, #2498 ) ) REPRESENTATION_CONTEXT ( 'NONE', 'WORKASPACE' ) );
#56181 = CARTESIAN_POINT ( 'NONE',  ( 9.478197642333000772, -79.47463564708098716, 6.090377947633999867 ) ) ;
#56182 = CARTESIAN_POINT ( 'NONE',  ( -11.68767212001979061, -76.82083333333335418, -3.140974612311365988 ) ) ;
#56183 = CARTESIAN_POINT ( 'NONE',  ( 10.48543666025110710, -79.50833333333332575, -6.043427764450776785 ) ) ;
#56184 = CARTESIAN_POINT ( 'NONE',  ( 0.9992560168720977520, -78.90234941287772585, 0.7679384024261605157 ) ) ;
#56185 = B_SPLINE_CURVE_WITH_KNOTS ( 'NONE', 3,
 ( #21843, #18315, #12979, #7985, #49310, #8860, #36306, #54330, #30409, #53152 ),
 .UNSPECIFIED., .F., .F.,
 ( 4, 2, 2, 2, 4 ),
 ( 0.000000000000000000, 0.2499999999999998890, 0.4999999999999997780, 0.7499999999999998890, 1.000000000000000000 ),
 .UNSPECIFIED. ) ;
#56186 = CARTESIAN_POINT ( 'NONE',  ( 0.1761264049549336741, -82.21573302580067377, 1.536971449393705447 ) ) ;
#56187 = CARTESIAN_POINT ( 'NONE',  ( -0.4741829603392039294, -79.69437006906809984, -1.156353086730761870 ) ) ;
#56188 = AXIS2_PLACEMENT_3D ( 'NONE', #22814, #54413, #13359 ) ;
#56189 = ORIENTED_EDGE ( 'NONE', *, *, #10602, .T. ) ;
#56190 = LINE ( 'NONE', #34308, #16952 ) ;
#56191 = FILL_AREA_STYLE ('',( #29588 ) ) ;
#56192 = LINE ( 'NONE', #15739, #46935 ) ;
#56193 = ORIENTED_EDGE ( 'NONE', *, *, #8089, .T. ) ;
#56194 = ORIENTED_EDGE ( 'NONE', *, *, #28319, .T. ) ;
#56195 = CARTESIAN_POINT ( 'NONE',  ( -12.43640296263000167, -53.88252466098000326, 0.05222744260232999730 ) ) ;
#56196 = EDGE_CURVE ( 'NONE', #7434, #2543, #50418, .T. ) ;
#56197 = ORIENTED_EDGE ( 'NONE', *, *, #52861, .T. ) ;
#56198 = CARTESIAN_POINT ( 'NONE',  ( 5.749221480030474396, -79.92640261716472594, -7.622783030296528040 ) ) ;
#56199 = ORIENTED_EDGE ( 'NONE', *, *, #11105, .F. ) ;
#56200 = CARTESIAN_POINT ( 'NONE',  ( 0.4802748259353999960, -16.99473092717999734, 12.54896097834000024 ) ) ;
#56201 = CARTESIAN_POINT ( 'NONE',  ( 0.000000000000000000, -77.50000000000000000, 0.000000000000000000 ) ) ;
#56202 = DIRECTION ( 'NONE',  ( 0.000000000000000000, 0.000000000000000000, 1.000000000000000000 ) ) ;
#56203 = CARTESIAN_POINT ( 'NONE',  ( 1.500000000000000888, -78.23958333333330017, -0.1963495408493590444 ) ) ;
#56204 = CARTESIAN_POINT ( 'NONE',  ( -5.611728806388999402, -78.83398667140099292, -8.168780722191000265 ) ) ;
#56205 = CARTESIAN_POINT ( 'NONE',  ( 0.2313529605545296963, -78.22705442624081229, -9.247502900338933074 ) ) ;
#56206 = CARTESIAN_POINT ( 'NONE',  ( 8.984871306655115575, -79.27160451067341285, 2.508152175999946110 ) ) ;
#56207 = ORIENTED_EDGE ( 'NONE', *, *, #30881, .F. ) ;
#56208 = VERTEX_POINT ( 'NONE', #18535 ) ;
#56209 = CARTESIAN_POINT ( 'NONE',  ( -8.798468283297333770, -77.57506182485165880, 2.854659429539475823 ) ) ;
#56210 = DIRECTION ( 'NONE',  ( 0.000000000000000000, 1.000000000000000000, 0.000000000000000000 ) ) ;
#56211 = CARTESIAN_POINT ( 'NONE',  ( -12.43359700621999941, -61.50705514136999597, -0.8500729763766999847 ) ) ;
#56212 = CARTESIAN_POINT ( 'NONE',  ( -1.565122400816999937, -78.65773938804198906, 9.577113408380000692 ) ) ;
#56213 = LINE ( 'NONE', #52080, #38848 ) ;
#56214 = CARTESIAN_POINT ( 'NONE',  ( -10.18589234708000113, -18.71082434677000350, 7.641012386038000592 ) ) ;
#56215 = CARTESIAN_POINT ( 'NONE',  ( 6.878833068915999327, -78.91836173076998762, -9.726923957509001184 ) ) ;
#56216 = B_SPLINE_SURFACE_WITH_KNOTS ( 'NONE', 3, 3, ( 
 ( #8742, #4313, #22313, #21730 ),
 ( #49493, #17305, #35291, #16738 ),
 ( #12303, #43900, #39163, #30293 ),
 ( #45655, #50082, #509, #5197 ),
 ( #223, #54507, #18485, #36768 ),
 ( #37351, #23199, #14329, #36478 ),
 ( #18776, #14044, #4909, #41497 ),
 ( #54785, #31746, #36193, #41204 ) ),
 .UNSPECIFIED., .F., .F., .F.,
 ( 4, 1, 1, 1, 1, 4 ),
 ( 4, 4 ),
 ( -0.01200407345748999953, 0.000000000000000000, 0.3333333333333000081, 0.6666666666667000474, 1.000000000000000000, 1.011997855551999947 ),
 ( -0.3559705542741000150, 1.355970554273999928 ),
 .UNSPECIFIED. ) ;
#56217 = CARTESIAN_POINT ( 'NONE',  ( 0.5947595261268000533, -80.92336727174999567, -1.595643580583000043 ) ) ;
#56218 = CARTESIAN_POINT ( 'NONE',  ( 1.750000000000000000, -60.04999999966999980, 12.00000000000000000 ) ) ;
#56219 = CARTESIAN_POINT ( 'NONE',  ( -10.16113132621832094, -76.65749405865184940, 5.912008408672408066 ) ) ;
#56220 = FACE_OUTER_BOUND ( 'NONE', #5636, .T. ) ;
#56221 = CARTESIAN_POINT ( 'NONE',  ( -9.783235115917999991, -54.26434390361999505, 7.961033122292000108 ) ) ;
#56222 = CARTESIAN_POINT ( 'NONE',  ( -7.544159220956999867, -78.99926332859899958, -6.426939800899999611 ) ) ;
#56223 = CARTESIAN_POINT ( 'NONE',  ( 9.596002108778145967, -77.20208333333333428, 7.374560639699002884 ) ) ;
#56224 = CARTESIAN_POINT ( 'NONE',  ( -7.660431561281999535, -18.80820826823000047, -10.01749754194999831 ) ) ;
#56225 = B_SPLINE_CURVE_WITH_KNOTS ( 'NONE', 3,
 ( #30988, #21573, #39578, #17143 ),
 .UNSPECIFIED., .F., .F.,
 ( 4, 4 ),
 ( 0.000000000000000000, 1.000000000000000000 ),
 .UNSPECIFIED. ) ;
#56226 = AXIS2_PLACEMENT_3D ( 'NONE', #29639, #32676, #11375 ) ;
#56228 = CARTESIAN_POINT ( 'NONE',  ( 14.00000000000000000, -32.70420297070000260, 0.000000000000000000 ) ) ;
#56227 = CARTESIAN_POINT ( 'NONE',  ( -8.500000000000000000, -75.00000000000001421, 0.000000000000000000 ) ) ;
#56229 = CARTESIAN_POINT ( 'NONE',  ( -7.919595949288999570, -59.94999999969999749, -9.050966799188000067 ) ) ;
#56230 = LINE ( 'NONE', #15779, #21982 ) ;
#56231 = CARTESIAN_POINT ( 'NONE',  ( 1.432628882339999965, -2.507710179781999837, -3.526139092948999743 ) ) ;
#56232 = CARTESIAN_POINT ( 'NONE',  ( 3.516297666798653854, -0.9927055907450104133, -0.3226314711147756920 ) ) ;
#56233 = TOROIDAL_SURFACE ( 'NONE', #38308, 13.50000000000000000, 0.5000000000000000000 ) ;
#56234 = ORIENTED_EDGE ( 'NONE', *, *, #13539, .T. ) ;
#56235 = PLANE ( 'NONE',  #38597 ) ;
#56236 = ADVANCED_FACE ( 'NONE', ( #50129 ), #27071, .F. ) ;
#56237 = LINE ( 'NONE', #25215, #18192 ) ;
#56238 = CARTESIAN_POINT ( 'NONE',  ( -12.50240681834000078, -24.68234730741999883, 1.005418943852999902 ) ) ;
#56239 = CARTESIAN_POINT ( 'NONE',  ( 1.233647025524779339, -78.36298610943158849, 0.2016259055441099179 ) ) ;
#56240 = CIRCLE ( 'NONE', #5315, 3.600000000000000089 ) ;
#56241 = CARTESIAN_POINT ( 'NONE',  ( -7.398415933695000390, -79.51124522128699823, -6.012806692959999921 ) ) ;
#56242 = DIRECTION ( 'NONE',  ( -1.000000000000000000, 0.000000000000000000, 0.000000000000000000 ) ) ;
#56243 = CARTESIAN_POINT ( 'NONE',  ( 1.576170184330999868, -60.96086967183000382, 12.55466896108000086 ) ) ;
#56244 = CARTESIAN_POINT ( 'NONE',  ( -2.531359639385017068, -79.49391352960579127, 10.44770980819917838 ) ) ;
#56245 = CARTESIAN_POINT ( 'NONE',  ( -6.760013919724056741, -77.27291666666666003, -8.796335266379987416 ) ) ;
#56246 = FACE_BOUND ( 'NONE', #5280, .T. ) ;
#56247 = CARTESIAN_POINT ( 'NONE',  ( -10.95675378139999978, -77.79623596436198341, 1.482457388852999935 ) ) ;
#56248 = EDGE_CURVE ( 'NONE', #8867, #35775, #2861, .T. ) ;
#56249 = CARTESIAN_POINT ( 'NONE',  ( -9.367668485852000515, -77.09685739310599217, 5.826535979523000286 ) ) ;
#56250 = CARTESIAN_POINT ( 'NONE',  ( 9.345760913908002010, -78.42224514476065167, 2.683384691899999730 ) ) ;
#56251 = CARTESIAN_POINT ( 'NONE',  ( -1.494641324160000062, -79.36620647882999435, -0.7306109071898999607 ) ) ;
#56252 = DIRECTION ( 'NONE',  ( 0.000000000000000000, 0.000000000000000000, -1.000000000000000000 ) ) ;
#56253 = CARTESIAN_POINT ( 'NONE',  ( 1.813979036992999783, -79.48985194988500780, 9.381055131006998948 ) ) ;
#56254 = CARTESIAN_POINT ( 'NONE',  ( -6.760013919724099374, -77.52708333333332291, 8.796335266379958995 ) ) ;
#56255 = CARTESIAN_POINT ( 'NONE',  ( 5.984702975412354853, -80.27245023178548422, -8.929714566242253682 ) ) ;
#56256 = CARTESIAN_POINT ( 'NONE',  ( -1.250000000000000000, -78.50000000000000000, 0.000000000000000000 ) ) ;
#56257 = CARTESIAN_POINT ( 'NONE',  ( 6.582919022827243616, -79.71875000027529268, -6.583307224015771730 ) ) ;
#56258 = CARTESIAN_POINT ( 'NONE',  ( -11.60111135005000094, -79.22298198540099179, -3.181408645392000523 ) ) ;
#56259 = CARTESIAN_POINT ( 'NONE',  ( 0.000000000000000000, -28.92928575306000383, 0.000000000000000000 ) ) ;
#56260 = DIRECTION ( 'NONE',  ( -1.000000000000000000, 0.000000000000000000, 0.000000000000000000 ) ) ;
#56261 = ORIENTED_EDGE ( 'NONE', *, *, #21021, .T. ) ;
#56262 = CARTESIAN_POINT ( 'NONE',  ( 0.9591162783412999771, -78.25481147984399399, -11.89603288543000126 ) ) ;
#56263 = EDGE_CURVE ( 'NONE', #245, #42686, #842, .T. ) ;
#56264 = ORIENTED_EDGE ( 'NONE', *, *, #563, .T. ) ;
#56265 = CIRCLE ( 'NONE', #30774, 5.000000000000000000 ) ;
#56266 = ORIENTED_EDGE ( 'NONE', *, *, #25296, .T. ) ;
#56267 =( NAMED_UNIT ( * ) PLANE_ANGLE_UNIT ( ) SI_UNIT ( $, .RADIAN. ) );
#56268 = DIRECTION ( 'NONE',  ( 0.000000000000000000, -1.000000000000000000, 0.000000000000000000 ) ) ;
#56269 = AXIS2_PLACEMENT_3D ( 'NONE', #40069, #49541, #44508 ) ;
#56270 = CARTESIAN_POINT ( 'NONE',  ( -3.412272945380999900, -78.65351518583565849, 0.4936653998998999926 ) ) ;
#56271 = CARTESIAN_POINT ( 'NONE',  ( 7.654057555294024873, -79.20013708438366962, 5.626991512746083224 ) ) ;
#56272 = ORIENTED_EDGE ( 'NONE', *, *, #30956, .F. ) ;
#56273 = CARTESIAN_POINT ( 'NONE',  ( 0.3307596944394597949, -82.74658640164716417, -1.205731917451906554 ) ) ;
#56274 = AXIS2_PLACEMENT_3D ( 'NONE', #14309, #9608, #44744 ) ;
#56275 = ORIENTED_EDGE ( 'NONE', *, *, #39148, .T. ) ;
#56276 = CARTESIAN_POINT ( 'NONE',  ( -2.417766456716999635, -2.993540208250999868, 2.392442992385000355 ) ) ;
#56277 = ORIENTED_EDGE ( 'NONE', *, *, #18056, .F. ) ;
#56278 = CARTESIAN_POINT ( 'NONE',  ( -0.5546092031877057904, -79.51207562121919636, 1.122904892616682249 ) ) ;
#56279 = CARTESIAN_POINT ( 'NONE',  ( -1.433156267533250983, -78.72468943822306642, 0.4708507765673180523 ) ) ;
#56280 = CIRCLE ( 'NONE', #29871, 0.5000000000000000000 ) ;
#56281 = CARTESIAN_POINT ( 'NONE',  ( 0.2112907341303528197, -79.79999999999999716, -11.79160395029623487 ) ) ;
#56282 = CARTESIAN_POINT ( 'NONE',  ( -7.115719518657461329, -80.03287302791015634, 8.059270059204177272 ) ) ;
#56283 = CARTESIAN_POINT ( 'NONE',  ( 3.086108443883076813, -79.09545426945904012, -11.86945146775599724 ) ) ;
#56284 = DIRECTION ( 'NONE',  ( -0.9999999924279685537, 0.000000000000000000, -0.0001230612157848962919 ) ) ;
#56285 = CARTESIAN_POINT ( 'NONE',  ( -7.860507001410999450, -76.83870604836299378, 7.955276143908999842 ) ) ;
#56286 = CARTESIAN_POINT ( 'NONE',  ( 7.714905556308770507, -79.55033101189913225, -5.543136766205470245 ) ) ;
#56287 = CARTESIAN_POINT ( 'NONE',  ( -1.358260632703687021, -81.38578242155206510, -0.6678246071336888523 ) ) ;
#56288 = CARTESIAN_POINT ( 'NONE',  ( 9.824451308078000267, -76.60242220834099669, -5.196131110057000235 ) ) ;
#56289 = CARTESIAN_POINT ( 'NONE',  ( -4.767438741492489029, -78.68199087655180790, -7.927228674465881753 ) ) ;
#56290 = CARTESIAN_POINT ( 'NONE',  ( 0.000000000000000000, -92.13603921945998820, 0.000000000000000000 ) ) ;
#56291 = CARTESIAN_POINT ( 'NONE',  ( 9.252740428348991131, -77.07083333333333997, 2.486604901413179913 ) ) ;
#56292 = CARTESIAN_POINT ( 'NONE',  ( 2.948832248429000380, -80.48578455456799929, -2.327176499381999886 ) ) ;
#56293 = CARTESIAN_POINT ( 'NONE',  ( 8.621786563366999445, -78.88570433617398692, 7.917562470644999628 ) ) ;
#56294 = CARTESIAN_POINT ( 'NONE',  ( 11.05131777856872688, -76.22578125001119531, 4.579357959789169819 ) ) ;
#56295 = CARTESIAN_POINT ( 'NONE',  ( 0.8976219970198608955, -82.91185551150395838, 0.8696104471699304117 ) ) ;
#56296 = CARTESIAN_POINT ( 'NONE',  ( 0.000000000000000000, -39.30476017083000073, 0.000000000000000000 ) ) ;
#56297 = CARTESIAN_POINT ( 'NONE',  ( 3.232998594844000539, -82.42258068398498949, -1.191363634767000024 ) ) ;
#56298 = LINE ( 'NONE', #33840, #28941 ) ;
#56299 = CARTESIAN_POINT ( 'NONE',  ( 0.5668640726090544701, -24.91659694980802797, 12.50470739227063177 ) ) ;
#56300 = ADVANCED_FACE ( 'NONE', ( #27661, #40674, #264, #4951 ), #27868, .T. ) ;
#56301 = DIRECTION ( 'NONE',  ( 0.000000000000000000, 0.000000000000000000, -1.000000000000000000 ) ) ;
#56302 = CARTESIAN_POINT ( 'NONE',  ( 1.193978368322000216, -81.84759560537901280, -0.5941311122250999555 ) ) ;
#56303 = EDGE_CURVE ( 'NONE', #3192, #1897, #10400, .T. ) ;
#56304 = FACE_OUTER_BOUND ( 'NONE', #14939, .T. ) ;
#56305 = CARTESIAN_POINT ( 'NONE',  ( 12.54987272477000104, -25.05113590135999857, 0.1385846084899000075 ) ) ;
#56306 = AXIS2_PLACEMENT_3D ( 'NONE', #43800, #48796, #34905 ) ;
#56307 = CARTESIAN_POINT ( 'NONE',  ( -7.222015211734788664, -77.88356993406765127, 8.081286372382828986 ) ) ;
#56308 = CARTESIAN_POINT ( 'NONE',  ( 4.977885330626822480, -78.26203852219340718, -9.897304379485547088 ) ) ;
#56309 = CARTESIAN_POINT ( 'NONE',  ( -10.81649518602000093, -79.33643291229606120, 1.862108609190000097 ) ) ;
#56310 = CARTESIAN_POINT ( 'NONE',  ( -1.747928427208000013, -75.60822666423999294, -12.38958793587999985 ) ) ;
#56311 = VERTEX_POINT ( 'NONE', #6700 ) ;
#56312 = AXIS2_PLACEMENT_3D ( 'NONE', #707, #31357, #9536 ) ;
#56313 = CARTESIAN_POINT ( 'NONE',  ( 0.2778302777538999568, -85.39646544543099083, -3.953326594592999843 ) ) ;
#56314 = CARTESIAN_POINT ( 'NONE',  ( 5.194930721789999595, -80.11395898343219812, 10.15375755480999942 ) ) ;
#56315 = EDGE_CURVE ( 'NONE', #15875, #26901, #2003, .T. ) ;
#56316 = AXIS2_PLACEMENT_3D ( 'NONE', #44796, #17634, #54539 ) ;
#56317 = CARTESIAN_POINT ( 'NONE',  ( -1.310679582531386611, -81.54166666666668561, -0.7554284705563495406 ) ) ;
#56318 = CARTESIAN_POINT ( 'NONE',  ( 9.668695434387000631, -79.36723320854999031, -7.222620064924999639 ) ) ;
#56319 = DIRECTION ( 'NONE',  ( 0.000000000000000000, 1.000000000000000000, 0.000000000000000000 ) ) ;
#56320 = CARTESIAN_POINT ( 'NONE',  ( -8.711966356949998769, -77.29588578325397918, 3.874524904258000557 ) ) ;
#56321 = AXIS2_PLACEMENT_3D ( 'NONE', #46397, #46105, #32190 ) ;
#56322 = CARTESIAN_POINT ( 'NONE',  ( -3.349471176857000021, -83.06632269734298291, 2.487488346166999875 ) ) ;
#56323 = CARTESIAN_POINT ( 'NONE',  ( -12.00000000000000000, -78.89999999999999147, -1.868256502752000067E-14 ) ) ;
#56324 = DIRECTION ( 'NONE',  ( -0.7071067811865470176, -0.7071067811865470176, -3.647648880603240205E-08 ) ) ;
#56325 = ORIENTED_EDGE ( 'NONE', *, *, #35686, .T. ) ;
#56326 = CARTESIAN_POINT ( 'NONE',  ( 0.000000000000000000, -80.89999999999999147, 0.000000000000000000 ) ) ;
#56327 = CARTESIAN_POINT ( 'NONE',  ( -2.593635880370856572, -78.78614491170810652, -2.240786627949076237 ) ) ;
#56328 = ORIENTED_EDGE ( 'NONE', *, *, #27821, .F. ) ;
#56329 = CARTESIAN_POINT ( 'NONE',  ( -1.210921577777000158, -78.09993436228529617, 0.5587889421650999999 ) ) ;
#56330 = DIRECTION ( 'NONE',  ( 0.000000000000000000, 1.000000000000000000, 0.000000000000000000 ) ) ;
#56331 = DIRECTION ( 'NONE',  ( 0.000000000000000000, -1.000000000000000000, 0.000000000000000000 ) ) ;
#56332 = ORIENTED_EDGE ( 'NONE', *, *, #45725, .F. ) ;
#56333 = B_SPLINE_CURVE_WITH_KNOTS ( 'NONE', 3,
 ( #41615, #46359, #28606, #23319, #5884, #10042 ),
 .UNSPECIFIED., .F., .F.,
 ( 4, 2, 4 ),
 ( 0.000000000000000000, 0.5000000000000000000, 1.000000000000000000 ),
 .UNSPECIFIED. ) ;
#56334 = CARTESIAN_POINT ( 'NONE',  ( 8.118221194901000359, -77.64411321036999425, 9.213591238522999660 ) ) ;
#56335 = CARTESIAN_POINT ( 'NONE',  ( -4.735947112136000392, -77.71182432715698951, -10.40542313098000093 ) ) ;
#56336 = ORIENTED_EDGE ( 'NONE', *, *, #41177, .F. ) ;
#56337 = CARTESIAN_POINT ( 'NONE',  ( 0.5131766215739365089, -80.44137981884804844, 1.140404433670309858 ) ) ;
#56338 = CARTESIAN_POINT ( 'NONE',  ( 1.570796326794857478, -79.66458333333332575, 12.00000000000000533 ) ) ;
#56339 = CARTESIAN_POINT ( 'NONE',  ( 9.523132023602000729, -80.38931903029605053, 1.108936319727999997 ) ) ;
#56340 = ORIENTED_EDGE ( 'NONE', *, *, #27264, .T. ) ;
#56341 = CARTESIAN_POINT ( 'NONE',  ( -12.70299718800736777, -25.02583482805824389, -0.8845454261047099864 ) ) ;
#56342 = CARTESIAN_POINT ( 'NONE',  ( -0.2648292726109000017, -78.95034006197499821, 10.91353432424999959 ) ) ;
#56343 = ORIENTED_EDGE ( 'NONE', *, *, #8375, .F. ) ;
#56344 = CARTESIAN_POINT ( 'NONE',  ( -10.75000000000000000, -80.59999999999999432, 0.000000000000000000 ) ) ;
#56345 = CARTESIAN_POINT ( 'NONE',  ( 2.962511214703000384, -77.66009415034599783, -9.021140561863999707 ) ) ;
#56346 = MANIFOLD_SOLID_BREP ( 'Stock-MAS-694-1', #2267 ) ;
#56347 = AXIS2_PLACEMENT_3D ( 'NONE', #36863, #605, #55766 ) ;
#56348 = ADVANCED_FACE ( 'NONE', ( #37984 ), #55716, .T. ) ;
#56349 = CARTESIAN_POINT ( 'NONE',  ( 10.11462645678659200, -55.41287635801727163, 7.639895286212098569 ) ) ;
#56350 = CARTESIAN_POINT ( 'NONE',  ( -7.601397897754999633, -55.54999999966999980, 9.369164850722000892 ) ) ;
#56351 = CARTESIAN_POINT ( 'NONE',  ( -11.14527737854716527, -77.22513161494639178, -3.781945882020559591 ) ) ;
#56352 = CARTESIAN_POINT ( 'NONE',  ( -9.554603705186000440, -77.21387085810299311, 0.6301758013986999973 ) ) ;
#56353 = AXIS2_PLACEMENT_3D ( 'NONE', #34953, #24160, #56047 ) ;
#56354 = CARTESIAN_POINT ( 'NONE',  ( -0.08519377839585000334, -78.52556629197296445, 11.97951611939999950 ) ) ;
#56355 = CARTESIAN_POINT ( 'NONE',  ( 10.71369944335147473, -79.82916666666666572, -2.879226727952063580 ) ) ;
#56356 = CARTESIAN_POINT ( 'NONE',  ( -12.19234209666000091, -75.95901006652999854, -1.697737568323999913 ) ) ;
#56357 = CIRCLE ( 'NONE', #29000, 1.250000000000000444 ) ;
#56358 = CARTESIAN_POINT ( 'NONE',  ( -3.740889684922000136, -80.32832046129098558, -1.847238338933999913 ) ) ;
#56359 = CARTESIAN_POINT ( 'NONE',  ( -1.243547092045951263, -78.01458333333333428, -9.500000000000003553 ) ) ;
#56360 = CARTESIAN_POINT ( 'NONE',  ( 9.650948395536001811, -61.73402498629999968, -8.252474012569001260 ) ) ;
#56361 = AXIS2_PLACEMENT_3D ( 'NONE', #35452, #40488, #36637 ) ;
#56362 = DIRECTION ( 'NONE',  ( 1.000000000000000000, 0.000000000000000000, 0.000000000000000000 ) ) ;
#56363 = CARTESIAN_POINT ( 'NONE',  ( 9.406806676749999596, -76.82832889608799576, -7.895227358184000899 ) ) ;
#56364 = CARTESIAN_POINT ( 'NONE',  ( -12.50000000000000000, -23.25000000000000000, 1.250000000000000000 ) ) ;
#56365 = CARTESIAN_POINT ( 'NONE',  ( 7.720090653410608184, -77.86970692066191191, 9.274876966509804532 ) ) ;
#56366 = CARTESIAN_POINT ( 'NONE',  ( 0.3271848554491016414, -78.64583333333330017, -1.217465845835393967 ) ) ;
#56367 = ORIENTED_EDGE ( 'NONE', *, *, #49245, .T. ) ;
#56369 = ADVANCED_FACE ( 'NONE', ( #11148 ), #46876, .T. ) ;
#56368 = CARTESIAN_POINT ( 'NONE',  ( 1.226384192711576837, -79.95033587725438906, -0.8842796768856556744 ) ) ;
#56370 = CARTESIAN_POINT ( 'NONE',  ( 0.000000000000000000, -75.15999999999999659, 0.000000000000000000 ) ) ;
#56371 = CARTESIAN_POINT ( 'NONE',  ( -0.7554284705563480973, -78.58333333333332860, -1.310679582531387277 ) ) ;
#56372 = CARTESIAN_POINT ( 'NONE',  ( -1.406402020388000107, -2.287363919000000134, 3.437511342334000020 ) ) ;
#56373 = B_SPLINE_SURFACE_WITH_KNOTS ( 'NONE', 3, 3, ( 
 ( #34303, #52334, #11890, #47922 ),
 ( #7455, #25453, #22991, #27110 ),
 ( #49578, #22398, #41001, #594 ),
 ( #35973, #26814, #49874, #18576 ),
 ( #10007, #54586, #36851, #22697 ),
 ( #18281, #40710, #32122, #4398 ),
 ( #32410, #54296, #27985, #9125 ),
 ( #303, #36564, #13833, #44843 ) ),
 .UNSPECIFIED., .F., .F., .F.,
 ( 4, 1, 1, 1, 1, 4 ),
 ( 4, 4 ),
 ( -0.01200407347462000007, 0.000000000000000000, 0.3333333333333000081, 0.6666666666667000474, 1.000000000000000000, 1.011997855551999947 ),
 ( -0.3559705542741999906, 1.355970554273999928 ),
 .UNSPECIFIED. ) ;
#56374 = CARTESIAN_POINT ( 'NONE',  ( -10.77989530031999976, -78.47947827561399947, -5.637054895855999170 ) ) ;
#56375 = CARTESIAN_POINT ( 'NONE',  ( -9.721291027688000241, -77.26593683473198837, 0.5965459135819000114 ) ) ;
#56377 = CARTESIAN_POINT ( 'NONE',  ( 7.174506471390958318, -77.88110187774557858, -8.441707957340309321 ) ) ;
#56376 = CARTESIAN_POINT ( 'NONE',  ( -9.042463335936661295, -76.14465617035568812, 7.502879964933097945 ) ) ;
#56378 = CARTESIAN_POINT ( 'NONE',  ( 9.789168614380999500, -79.24010319720299833, -4.831929617604999727 ) ) ;
#56379 = DIRECTION ( 'NONE',  ( 0.000000000000000000, 1.000000000000000000, 0.000000000000000000 ) ) ;
#56380 = ORIENTED_EDGE ( 'NONE', *, *, #821, .F. ) ;
#56381 = DIRECTION ( 'NONE',  ( -1.000000000000000000, 0.000000000000000000, 0.000000000000000000 ) ) ;
#56382 = CARTESIAN_POINT ( 'NONE',  ( 9.499178638196321245, -79.00092112126561972, 0.1004274591880019996 ) ) ;
#56383 = ADVANCED_FACE ( 'NONE', ( #51590 ), #29123, .F. ) ;
#56384 = DIRECTION ( 'NONE',  ( 0.000000000000000000, -1.000000000000000000, 0.000000000000000000 ) ) ;
#56385 = CARTESIAN_POINT ( 'NONE',  ( -7.631896413346999530, -60.02122715173999978, 10.36221694968000051 ) ) ;
#56386 = CARTESIAN_POINT ( 'NONE',  ( -10.95656768982416374, -80.09333027791306847, 0.9740957217062806706 ) ) ;
#56387 = CARTESIAN_POINT ( 'NONE',  ( -6.834812918901999268, -79.58052574656798583, 6.841065568902999772 ) ) ;
#56388 = CARTESIAN_POINT ( 'NONE',  ( 7.374560639698994002, -78.07708333333332007, -9.596002108778151296 ) ) ;
#56389 = CARTESIAN_POINT ( 'NONE',  ( -8.796335266379978535, -78.65208333333333712, -6.760013919724068288 ) ) ;
#56390 = ORIENTED_EDGE ( 'NONE', *, *, #17914, .T. ) ;
#56391 = CARTESIAN_POINT ( 'NONE',  ( -11.24501830132000002, -78.77221245318798992, 0.6192963436278000611 ) ) ;
#56392 = CARTESIAN_POINT ( 'NONE',  ( 11.06827260339915497, -76.61133711981047156, 1.603586413861646021 ) ) ;
#56393 = CARTESIAN_POINT ( 'NONE',  ( -10.28470975277595123, -79.09086982037037217, -5.853606176233665082 ) ) ;
#56394 = CARTESIAN_POINT ( 'NONE',  ( -13.97864847851000114, -45.76668425569999954, -0.0001086640162462999885 ) ) ;
#56395 = CARTESIAN_POINT ( 'NONE',  ( 0.000000000000000000, -76.00000000000000000, 0.000000000000000000 ) ) ;
#56396 = CARTESIAN_POINT ( 'NONE',  ( 1.209689523629019714, -78.87441410267364006, -0.3994885700558234998 ) ) ;
#56397 = CARTESIAN_POINT ( 'NONE',  ( 1.249556443808253592, -82.34024392821149263, -0.1639605875127234658 ) ) ;
#56398 = CARTESIAN_POINT ( 'NONE',  ( 12.50745077494999968, -61.79994448255000350, 2.662030659623000237E-09 ) ) ;
#56399 = PRODUCT_RELATED_PRODUCT_CATEGORY ( 'part', '', ( #25743 ) ) ;
#56400 = AXIS2_PLACEMENT_3D ( 'NONE', #14053, #32048, #6070 ) ;
#56401 = CARTESIAN_POINT ( 'NONE',  ( -9.546815223803999828, -54.11472046612000497, -8.130854305859001485 ) ) ;
#56402 = FACE_OUTER_BOUND ( 'NONE', #1752, .T. ) ;
#56403 = B_SPLINE_CURVE_WITH_KNOTS ( 'NONE', 3,
 ( #38359, #51678, #56667, #46962, #16223, #15054, #37484, #28324, #51958, #10643 ),
 .UNSPECIFIED., .F., .F.,
 ( 4, 2, 2, 2, 4 ),
 ( 0.000000000000000000, 0.2500000000000000555, 0.5000000000000001110, 0.7500000000000002220, 1.000000000000000000 ),
 .UNSPECIFIED. ) ;
#56404 = CARTESIAN_POINT ( 'NONE',  ( -7.545891804452000251, -79.65480220322699267, 6.201630566990999682 ) ) ;
#56405 = VERTEX_POINT ( 'NONE', #34119 ) ;
#56406 = ORIENTED_EDGE ( 'NONE', *, *, #24691, .F. ) ;
#56407 = CARTESIAN_POINT ( 'NONE',  ( -10.04675991039999872, -76.77512878623900860, 7.585220848138000349 ) ) ;
#56408 = CARTESIAN_POINT ( 'NONE',  ( -0.4971289415107331133, -78.72148840043671214, -10.74989891806322539 ) ) ;
#56409 = ORIENTED_EDGE ( 'NONE', *, *, #22500, .T. ) ;
#56410 = CARTESIAN_POINT ( 'NONE',  ( 9.641218323609999530, -17.56606991914999938, 7.943737929428000832 ) ) ;
#56411 = EDGE_CURVE ( 'NONE', #2822, #15756, #13911, .T. ) ;
#56412 = CARTESIAN_POINT ( 'NONE',  ( -9.022399766209378669, -78.87991562074994079, -3.573531901437693392 ) ) ;
#56413 = CARTESIAN_POINT ( 'NONE',  ( -0.7022187824378000043, -82.19906693409399168, -1.095132696781000003 ) ) ;
#56414 = CARTESIAN_POINT ( 'NONE',  ( 11.63291926114999875, -77.45276987983000083, 5.337072863433999892 ) ) ;
#56415 = EDGE_CURVE ( 'NONE', #14353, #13828, #55568, .T. ) ;
#56416 = CARTESIAN_POINT ( 'NONE',  ( -5.414008284903408352, -79.68335750799590755, -9.393288886975321716 ) ) ;
#56417 = CARTESIAN_POINT ( 'NONE',  ( -12.00000000000000000, -23.15000000000000213, -0.8000000000000000444 ) ) ;
#56418 = CARTESIAN_POINT ( 'NONE',  ( 10.42531124905999995, -18.73514851523999880, -7.624341765453999997 ) ) ;
#56419 = CARTESIAN_POINT ( 'NONE',  ( 6.766402264611000028, -79.51042470825198905, -8.946167390840999545 ) ) ;
#56420 = EDGE_LOOP ( 'NONE', ( #19320, #32336, #17441, #12535 ) ) ;
#56421 = DIRECTION ( 'NONE',  ( -0.7071067811865975328, -0.7071067811864976127, 2.062933177233993779E-09 ) ) ;
#56422 = VERTEX_POINT ( 'NONE', #15117 ) ;
#56423 = CARTESIAN_POINT ( 'NONE',  ( 8.103228132958101071, -77.31002185566839557, -4.473611354302846621 ) ) ;
#56424 = CARTESIAN_POINT ( 'NONE',  ( 12.56594317825999951, -60.05000001354000005, -1.750000000000000000 ) ) ;
#56425 = DIRECTION ( 'NONE',  ( -0.7071067811865475727, 0.000000000000000000, -0.7071067811865475727 ) ) ;
#56426 = DIRECTION ( 'NONE',  ( -0.7071067811865475727, 0.000000000000000000, 0.7071067811865475727 ) ) ;
#56427 = CARTESIAN_POINT ( 'NONE',  ( 0.2897255177615999933, -78.96130845337700066, 1.387848051154999762 ) ) ;
#56428 = FACE_OUTER_BOUND ( 'NONE', #41376, .T. ) ;
#56429 = AXIS2_PLACEMENT_3D ( 'NONE', #30509, #12226, #56242 ) ;
#56430 = CARTESIAN_POINT ( 'NONE',  ( 9.499549289235639904, -79.50042064254546403, 0.05021470316550929319 ) ) ;
#56431 = CARTESIAN_POINT ( 'NONE',  ( 1.619712389308999967, -79.08738182501998892, 0.1587296492880999887 ) ) ;
#56432 = CARTESIAN_POINT ( 'NONE',  ( -7.640030264156999706, -23.30716680861999990, 10.18491080493000212 ) ) ;
#56433 = CARTESIAN_POINT ( 'NONE',  ( -9.839875214663999614, -79.89318977307699754, 4.781661263485999847 ) ) ;
#56434 = CARTESIAN_POINT ( 'NONE',  ( -9.625846388754000671, -79.20118265956556058, -7.214584339064000318 ) ) ;
#56435 = CARTESIAN_POINT ( 'NONE',  ( -7.342331066867000544, -59.94999999967000548, 8.190859204290999784 ) ) ;
#56436 = CARTESIAN_POINT ( 'NONE',  ( 0.2671998652489999682, -82.82582186680899383, 3.537396816914999853 ) ) ;
#56437 = VERTEX_POINT ( 'NONE', #28102 ) ;
#56438 = CARTESIAN_POINT ( 'NONE',  ( -8.905521014750718223, -77.20000000000000284, 6.316176128476434393 ) ) ;
#56439 = CARTESIAN_POINT ( 'NONE',  ( -8.485281374238999419, -59.94999999967000548, 8.485281374238999419 ) ) ;
#56440 = CARTESIAN_POINT ( 'NONE',  ( -6.606781056858329393, -79.17307604219098494, -8.596831229953354025 ) ) ;
#56441 = CARTESIAN_POINT ( 'NONE',  ( 8.272973658470998970, -78.18397787739699822, -8.664523719228998999 ) ) ;
#56442 = CARTESIAN_POINT ( 'NONE',  ( -7.647094085193999469, -18.63104695440999947, 10.00844048070000092 ) ) ;
#56443 = CARTESIAN_POINT ( 'NONE',  ( 1.239585895167351959, -78.48166632226170236, -0.2976318702780533787 ) ) ;
#56444 = CARTESIAN_POINT ( 'NONE',  ( -2.215970870699417006, -2.179180607209704856, 2.738679624322115203 ) ) ;
#56445 = CARTESIAN_POINT ( 'NONE',  ( 8.386770501422327939, -80.90424990314578224, 6.732465268853045970 ) ) ;
#56446 = CARTESIAN_POINT ( 'NONE',  ( -9.520207861471000399, -78.64464829700199289, -0.1897854149113999966 ) ) ;
#56447 = CARTESIAN_POINT ( 'NONE',  ( 2.065550207748000133, -55.37434920636000157, -12.82162303852000029 ) ) ;
#56448 = CARTESIAN_POINT ( 'NONE',  ( -4.570437647871999687, -78.36785646258199733, 10.04055945087000090 ) ) ;
#56449 = CARTESIAN_POINT ( 'NONE',  ( 1.897323258163000181, -80.38768166943580695, 10.74448230087999967 ) ) ;
#56450 = CARTESIAN_POINT ( 'NONE',  ( 1.264835035987859069, -80.90980377984654126, 0.1533566471899267813 ) ) ;
#56451 = ORIENTED_EDGE ( 'NONE', *, *, #31045, .F. ) ;
#56452 = CARTESIAN_POINT ( 'NONE',  ( -0.8000000000000000444, -23.15000000000000213, 12.00000000000000000 ) ) ;
#56453 = CARTESIAN_POINT ( 'NONE',  ( 11.44512976686996808, -76.96771873177330292, 3.079394274004417564 ) ) ;
#56454 = CARTESIAN_POINT ( 'NONE',  ( 0.5506765233276000870, -62.05954292211000478, -12.77514798316000011 ) ) ;
#56455 = CARTESIAN_POINT ( 'NONE',  ( -7.674614791488999721, -22.75100836106000202, -10.14948852564000070 ) ) ;
#56456 = EDGE_CURVE ( 'NONE', #26037, #10086, #43435, .T. ) ;
#56457 = CARTESIAN_POINT ( 'NONE',  ( 10.34070037867000202, -77.98444425272499814, -4.346035695907999319 ) ) ;
#56458 = CARTESIAN_POINT ( 'NONE',  ( -10.96673197750000206, -78.37304949611799998, -0.4413686857046000278 ) ) ;
#56459 = CARTESIAN_POINT ( 'NONE',  ( 9.996770077869998161, -24.15065455350000079, -7.758602204116000323 ) ) ;
#56460 = ADVANCED_FACE ( 'NONE', ( #2146 ), #48868, .F. ) ;
#56461 = CARTESIAN_POINT ( 'NONE',  ( -1.539461606647227976, -84.98229167426450203, -3.748297833576170746 ) ) ;
#56462 = CARTESIAN_POINT ( 'NONE',  ( -10.11462613664629195, -60.18712935448252210, 7.639894945646047653 ) ) ;
#56463 = CARTESIAN_POINT ( 'NONE',  ( 9.781558643814788567, -78.49484497342521649, 6.508323693118907904 ) ) ;
#56464 = CARTESIAN_POINT ( 'NONE',  ( -1.416666666666666741, -77.85000000000000853, 0.000000000000000000 ) ) ;
#56465 = EDGE_LOOP ( 'NONE', ( #55381, #26730, #23365, #34682 ) ) ;
#56466 = CARTESIAN_POINT ( 'NONE',  ( -0.4841670057754499656, -80.00688952560039979, 1.152271897791588229 ) ) ;
#56467 = CARTESIAN_POINT ( 'NONE',  ( -3.190103214945636534, -75.80000000000002558, -11.32367545015943122 ) ) ;
#56468 = CARTESIAN_POINT ( 'NONE',  ( -10.98029981754000062, -79.67128212740999516, 1.094250890400999987 ) ) ;
#56469 = CARTESIAN_POINT ( 'NONE',  ( 12.00000000000000000, -77.04999999999999716, 0.000000000000000000 ) ) ;
#56470 = PLANE ( 'NONE',  #7169 ) ;
#56471 = CARTESIAN_POINT ( 'NONE',  ( 1.092501263137524159, -78.89193896525061689, 0.6295016473291589199 ) ) ;
#56472 = CARTESIAN_POINT ( 'NONE',  ( -1.417317677626557471, -81.82097862065256777, 0.5276391229990249343 ) ) ;
#56473 = CARTESIAN_POINT ( 'NONE',  ( -0.8507816195585579111, -79.66573003440132084, -0.9156227843767963392 ) ) ;
#56475 = ADVANCED_FACE ( 'NONE', ( #13586 ), #15156, .F. ) ;
#56474 = VECTOR ( 'NONE', #15694, 1000.000000000000000 ) ;
#56476 = CARTESIAN_POINT ( 'NONE',  ( -7.792421629638690561, -54.50899070338012820, 10.18245656324170412 ) ) ;
#56477 = ORIENTED_EDGE ( 'NONE', *, *, #45866, .T. ) ;
#56478 = CARTESIAN_POINT ( 'NONE',  ( 1.799502287691000069, -23.30716680861999990, 12.60413670420000010 ) ) ;
#56479 = CARTESIAN_POINT ( 'NONE',  ( -12.79895559715999909, -23.80469146265000191, 2.015913954444999767 ) ) ;
#56480 = EDGE_LOOP ( 'NONE', ( #17181, #31462, #29443 ) ) ;
#56481 = VERTEX_POINT ( 'NONE', #43593 ) ;
#56482 = B_SPLINE_CURVE_WITH_KNOTS ( 'NONE', 3,
 ( #50743, #1732, #55146, #32985, #19725, #45435, #24144, #10284, #36558, #51031, #9998, #41574, #50157, #14692, #27978, #46027, #23849, #40995, #36845 ),
 .UNSPECIFIED., .F., .F.,
 ( 4, 1, 1, 1, 2, 2, 1, 1, 2, 2, 2, 4 ),
 ( 0.000000000000000000, 0.1250000000000000278, 0.1875000000000000000, 0.2187500000000001110, 0.2343750000000001388, 0.2500000000000001665, 0.3750000000000008327, 0.4375000000000009437, 0.4687500000000009992, 0.5000000000000011102, 0.7500000000000006661, 1.000000000000000000 ),
 .UNSPECIFIED. ) ;
#56483 = CARTESIAN_POINT ( 'NONE',  ( -12.83675912438999944, -55.57244613998999938, -2.062833085520999976 ) ) ;
#56484 = EDGE_LOOP ( 'NONE', ( #15606, #47933, #458, #38173, #7244 ) ) ;
#56485 = EDGE_LOOP ( 'NONE', ( #52766, #1314, #55904 ) ) ;
#56486 = CARTESIAN_POINT ( 'NONE',  ( -9.659853700179651170, -81.00000000000000000, -4.855990401126174305 ) ) ;
#56487 = CARTESIAN_POINT ( 'NONE',  ( 1.468061006981000061, -77.43767547371999171, 10.81758581523999929 ) ) ;
#56488 = AXIS2_PLACEMENT_3D ( 'NONE', #18591, #893, #14719 ) ;
#56489 = APPLICATION_PROTOCOL_DEFINITION ( 'draft international standard', 'automotive_design', 1998, #54170 ) ;
#56490 = CARTESIAN_POINT ( 'NONE',  ( 0.1963495408493638184, -78.13541666666668561, -1.499999999999999778 ) ) ;
#56491 = EDGE_CURVE ( 'NONE', #49068, #1594, #36502, .T. ) ;
#56492 = CARTESIAN_POINT ( 'NONE',  ( -3.365558374102000094, -78.59601332859899969, 9.202792326454000360 ) ) ;
#56493 = CARTESIAN_POINT ( 'NONE',  ( -9.010884632761600344, -79.47923677369759332, 2.413026703165237041 ) ) ;
#56494 = B_SPLINE_CURVE_WITH_KNOTS ( 'NONE', 3,
 ( #27951, #45411, #41547, #36819, #14668, #51007, #10258, #28240, #10557, #28540, #24121, #46587, #42139, #37699, #34417, #38279, #11151, #39147 ),
 .UNSPECIFIED., .F., .F.,
 ( 4, 2, 2, 2, 2, 2, 2, 2, 4 ),
 ( 0.000000000000000000, 0.1250000000000000278, 0.2500000000000000555, 0.3750000000000000000, 0.5000000000000000000, 0.6250000000000000000, 0.7500000000000000000, 0.8750000000000001110, 1.000000000000000000 ),
 .UNSPECIFIED. ) ;
#56495 = EDGE_LOOP ( 'NONE', ( #18450, #49037, #46319, #16809, #43494 ) ) ;
#56496 = VERTEX_POINT ( 'NONE', #16150 ) ;
#56497 = CARTESIAN_POINT ( 'NONE',  ( -5.966983627959768555, -77.53090078892917347, 7.069611082095726751 ) ) ;
#56498 = CARTESIAN_POINT ( 'NONE',  ( -12.70455691843901391, -24.56014620597534659, 1.489817752277837970 ) ) ;
#56499 = DIRECTION ( 'NONE',  ( 0.000000000000000000, -1.000000000000000000, 0.000000000000000000 ) ) ;
#56500 = CARTESIAN_POINT ( 'NONE',  ( 9.512131559252001267, -78.06429424374599080, -1.920953556448999899 ) ) ;
#56501 = CARTESIAN_POINT ( 'NONE',  ( -3.684198380124090733, -86.12610001270965654, 1.557781209248569221 ) ) ;
#56502 = CARTESIAN_POINT ( 'NONE',  ( 7.712213536753880661, -60.86179137582710297, 10.27334987167996694 ) ) ;
#56503 = CARTESIAN_POINT ( 'NONE',  ( 9.393203674808285442, -76.70833333333330017, -5.413904038987152667 ) ) ;
#56504 = CARTESIAN_POINT ( 'NONE',  ( 12.00000000000000000, -76.66041666666667709, 1.570796326794922093 ) ) ;
#56505 = CARTESIAN_POINT ( 'NONE',  ( 1.653747448240000084, -80.03913826020999522, 0.4061235413877000155 ) ) ;
#56506 = DIRECTION ( 'NONE',  ( 0.000000000000000000, 1.433670265775999799E-08, 0.9999999999999998890 ) ) ;
#56507 = CARTESIAN_POINT ( 'NONE',  ( -10.65162040723731174, -76.66484428198535284, 4.960591388563448056 ) ) ;
#56508 = CARTESIAN_POINT ( 'NONE',  ( -9.389188763448000685, -54.08956227294000740, 8.194870530143999687 ) ) ;
#56509 = CARTESIAN_POINT ( 'NONE',  ( -3.292576784871000140, -78.04116332859899785, -9.347695904456999827 ) ) ;
#56510 = B_SPLINE_CURVE_WITH_KNOTS ( 'NONE', 3,
 ( #5929, #5635, #50529, #50237, #33073, #45816 ),
 .UNSPECIFIED., .F., .F.,
 ( 4, 2, 4 ),
 ( 0.000000000000000000, 0.4999999999999998890, 1.000000000000000000 ),
 .UNSPECIFIED. ) ;
#56511 = CARTESIAN_POINT ( 'NONE',  ( -11.96278216175999987, -78.19743832925900051, 0.6386762756999999624 ) ) ;
#56512 = CARTESIAN_POINT ( 'NONE',  ( 1.799475295154000065, -20.24916621771999914, -12.69619287815999975 ) ) ;
#56514 = CARTESIAN_POINT ( 'NONE',  ( -0.9420598709024999851, -79.32273412940499213, -0.8215979549846998964 ) ) ;
#56513 = DIRECTION ( 'NONE',  ( 0.000000000000000000, -1.000000000000000000, 0.000000000000000000 ) ) ;
#56515 = CIRCLE ( 'NONE', #31021, 0.8000000000000000444 ) ;
#56516 = CARTESIAN_POINT ( 'NONE',  ( 9.500000000000000000, -78.14999999999999147, 0.000000000000000000 ) ) ;
#56517 = CARTESIAN_POINT ( 'NONE',  ( -8.926170656458999986, -80.10939231032499208, -6.915662452114000658 ) ) ;
#56518 = CARTESIAN_POINT ( 'NONE',  ( 3.772660615778999915, -2.112549966925000078, 0.5031134774969999723 ) ) ;
#56519 = LINE ( 'NONE', #15493, #44877 ) ;
#56520 = ORIENTED_EDGE ( 'NONE', *, *, #26680, .T. ) ;
#56521 = CARTESIAN_POINT ( 'NONE',  ( -3.250000000000000000, -1.600000000000000089, 0.000000000000000000 ) ) ;
#56522 = FACE_OUTER_BOUND ( 'NONE', #14417, .T. ) ;
#56523 = DIRECTION ( 'NONE',  ( 0.000000000000000000, 0.000000000000000000, -1.000000000000000000 ) ) ;
#56524 = CARTESIAN_POINT ( 'NONE',  ( 0.3102673461446125436, -78.45508004528514334, 1.211442227934462323 ) ) ;
#56525 = CARTESIAN_POINT ( 'NONE',  ( -8.708088497213999801, -79.42357724651299122, 3.880669710089999835 ) ) ;
#56526 = CIRCLE ( 'NONE', #15081, 9.599999999999999645 ) ;
#56527 = CARTESIAN_POINT ( 'NONE',  ( -2.813980853284178352, -76.99599360018594041, 10.47075201474027928 ) ) ;
#56528 = CARTESIAN_POINT ( 'NONE',  ( 0.9218200799623742503, -80.17708333333334281, -1.199500263597268912 ) ) ;
#56529 = CARTESIAN_POINT ( 'NONE',  ( -1.997276839918471714, -3.072916666666665186, -2.598917237794086788 ) ) ;
#56530 = VECTOR ( 'NONE', #4927, 1000.000000000000114 ) ;
#56531 = DIRECTION ( 'NONE',  ( 0.000000000000000000, -1.000000000000000000, 0.000000000000000000 ) ) ;
#56532 = CARTESIAN_POINT ( 'NONE',  ( -4.043784919593939264, -78.67389998729011324, 2.284880126142478485 ) ) ;
#56533 = CARTESIAN_POINT ( 'NONE',  ( -6.437501231206999464, -77.94579083114099660, -8.855128588742999796 ) ) ;
#56534 = CARTESIAN_POINT ( 'NONE',  ( 7.388277095310935572, -76.37882974025046678, -9.138970832679994771 ) ) ;
#56535 = CARTESIAN_POINT ( 'NONE',  ( 7.081068198472000752, -76.96067567809700449, 8.459326660559002065 ) ) ;
#56536 = CARTESIAN_POINT ( 'NONE',  ( -3.339615680725999791, -78.55289514476064028, 9.131854552393999569 ) ) ;
#56537 = CARTESIAN_POINT ( 'NONE',  ( 0.1224622883215999852, -79.19916176948999009, 1.659079133038000142 ) ) ;
#56538 = CARTESIAN_POINT ( 'NONE',  ( -0.7999999999999001243, -23.15000000002000036, 12.00000000000000000 ) ) ;
#56539 = CARTESIAN_POINT ( 'NONE',  ( -0.9218200799623775810, -78.92708333333332860, 1.199500263597266247 ) ) ;
#56540 = CARTESIAN_POINT ( 'NONE',  ( 2.324423181964641483, -3.413061686833799513, 2.330852653237942995 ) ) ;
#56541 = CARTESIAN_POINT ( 'NONE',  ( 6.477052170204919967, -80.27679150412248532, -8.581165962541923875 ) ) ;
#56542 = FACE_OUTER_BOUND ( 'NONE', #49377, .T. ) ;
#56543 = CARTESIAN_POINT ( 'NONE',  ( 12.00000000000000000, -75.80000000000001137, -2.990830162875999918E-13 ) ) ;
#56544 = EDGE_CURVE ( 'NONE', #41507, #38110, #47100, .T. ) ;
#56545 = CARTESIAN_POINT ( 'NONE',  ( 3.714552462503000196, -79.41612481817199409, 11.44155784250999908 ) ) ;
#56546 = CARTESIAN_POINT ( 'NONE',  ( -0.7681833999686477066, -81.92708333333332860, 0.9995835529977223910 ) ) ;
#56547 = CARTESIAN_POINT ( 'NONE',  ( 11.26004178396000199, -80.07190303803308495, -0.2131731071575000136 ) ) ;
#56548 = EDGE_LOOP ( 'NONE', ( #51557, #54743, #44083, #42908 ) ) ;
#56549 = CARTESIAN_POINT ( 'NONE',  ( 7.639893274949067781, -60.18715751166909911, 10.11462445492872320 ) ) ;
#56550 = VERTEX_POINT ( 'NONE', #52451 ) ;
#56551 = VERTEX_POINT ( 'NONE', #51596 ) ;
#56552 = CARTESIAN_POINT ( 'NONE',  ( -3.206516299415000049, -1.613032031399000088, -0.5298615117031000299 ) ) ;
#56553 = EDGE_LOOP ( 'NONE', ( #15094, #38953, #56055, #39473 ) ) ;
#56554 = EDGE_CURVE ( 'NONE', #2183, #36137, #23126, .T. ) ;
#56555 = CARTESIAN_POINT ( 'NONE',  ( 2.782519347732000270, -80.84699166913398471, -2.196032187189999707 ) ) ;
#56556 = CARTESIAN_POINT ( 'NONE',  ( 7.901592333655654166, -79.19663653965405103, 5.277476999614962416 ) ) ;
#56557 = VERTEX_POINT ( 'NONE', #3156 ) ;
#56558 = FACE_OUTER_BOUND ( 'NONE', #54689, .T. ) ;
#56559 = CARTESIAN_POINT ( 'NONE',  ( -2.312505707054999693, -2.621129995393999934, -2.494332668574000156 ) ) ;
#56560 = EDGE_LOOP ( 'NONE', ( #4634, #39872, #28502, #23148 ) ) ;
#56561 = CARTESIAN_POINT ( 'NONE',  ( 0.1647566600028030070, -79.46510844028065890, 1.241328820898986329 ) ) ;
#56562 = CARTESIAN_POINT ( 'NONE',  ( -1.342108659710564034, -78.28775969006993307, -0.6887887724524024424 ) ) ;
#56563 = AXIS2_PLACEMENT_3D ( 'NONE', #23422, #14263, #2171 ) ;
#56564 = CARTESIAN_POINT ( 'NONE',  ( -10.98362417419999915, -18.84999999999999787, 0.5999999999999999778 ) ) ;
#56565 = CARTESIAN_POINT ( 'NONE',  ( -7.233059401658657350, -80.03400354919075710, 7.953958400202933987 ) ) ;
#56566 = CIRCLE ( 'NONE', #43365, 1.750000000000001332 ) ;
#56567 = DIRECTION ( 'NONE',  ( 0.000000000000000000, 1.000000000000000000, 0.000000000000000000 ) ) ;
#56568 = CARTESIAN_POINT ( 'NONE',  ( -3.085863646355653689, -86.17851879815594884, 1.444211070176307565 ) ) ;
#56570 = ADVANCED_FACE ( 'NONE', ( #24717 ), #47471, .F. ) ;
#56569 = CARTESIAN_POINT ( 'NONE',  ( 11.06808393496999976, -76.59534390116400004, 1.603559079323000125 ) ) ;
#56571 = CARTESIAN_POINT ( 'NONE',  ( -9.351608161489666671, -79.87169043516298927, -2.636777050789346433 ) ) ;
#56572 = CARTESIAN_POINT ( 'NONE',  ( -0.8903047578514302618, -81.27444143548434852, 1.221612336925710807 ) ) ;
#56573 = EDGE_CURVE ( 'NONE', #20674, #7434, #21722, .T. ) ;
#56574 = CARTESIAN_POINT ( 'NONE',  ( -9.775444717333000355, -76.92096869264500469, 5.042056850663000134 ) ) ;
#56575 = CARTESIAN_POINT ( 'NONE',  ( -5.134245522647685078, -78.67830135142374104, -7.694191572061213513 ) ) ;
#56576 = CARTESIAN_POINT ( 'NONE',  ( 1.137658753740000028, -79.47180014421898875, 0.6959227610743999870 ) ) ;
#56577 = CARTESIAN_POINT ( 'NONE',  ( -10.40480953490025762, -80.12661506326949734, -3.571040318220447318 ) ) ;
#56578 = DIRECTION ( 'NONE',  ( 0.000000000000000000, 1.000000000000000000, 0.000000000000000000 ) ) ;
#56579 = CARTESIAN_POINT ( 'NONE',  ( 3.384763024812000420, -80.84267549782599360, 1.194619930221000104 ) ) ;
#56580 = CARTESIAN_POINT ( 'NONE',  ( -10.48016323062205402, -78.08210605472315535, 2.414871192752478191 ) ) ;
#56581 = DIRECTION ( 'NONE',  ( 0.000000000000000000, 1.000000000000000000, 0.000000000000000000 ) ) ;
#56582 = CARTESIAN_POINT ( 'NONE',  ( 8.096452064242996016, -56.01421830980998351, 13.15643568217000769 ) ) ;
#56583 = CARTESIAN_POINT ( 'NONE',  ( -2.856781450715000226, -84.90774735065198797, -2.098514601310999872 ) ) ;
#56584 = CARTESIAN_POINT ( 'NONE',  ( -8.320799520507147662, -76.26179927676547265, -8.295681968662517392 ) ) ;
#56585 = FACE_OUTER_BOUND ( 'NONE', #6674, .T. ) ;
#56586 = CARTESIAN_POINT ( 'NONE',  ( -8.478749451788999636, -61.67812788887000153, -9.108222796200999838 ) ) ;
#56587 = CARTESIAN_POINT ( 'NONE',  ( 0.000000000000000000, -75.09999999996229292, 0.000000000000000000 ) ) ;
#56588 = CARTESIAN_POINT ( 'NONE',  ( 9.369164850722000892, -18.75000000000000000, 7.601397897754999633 ) ) ;
#56589 = VECTOR ( 'NONE', #37398, 1000.000000000000000 ) ;
#56590 = B_SPLINE_CURVE_WITH_KNOTS ( 'NONE', 3,
 ( #13282, #26281, #8279, #18021, #21278, #40454, #7991, #25988, #35412, #21569, #46, #58163, #36014, #39285, #34840, #53443, #43733, #8569 ),
 .UNSPECIFIED., .F., .F.,
 ( 4, 2, 2, 2, 2, 2, 2, 2, 4 ),
 ( 0.000000000000000000, 0.1250000000000000000, 0.2500000000000000000, 0.3750000000000000000, 0.5000000000000000000, 0.6250000000000000000, 0.7500000000000000000, 0.8750000000000000000, 1.000000000000000000 ),
 .UNSPECIFIED. ) ;
#56591 = CARTESIAN_POINT ( 'NONE',  ( -12.49989298250000047, -18.80773379996000116, -1.666426105558000081 ) ) ;
#56592 = CARTESIAN_POINT ( 'NONE',  ( -3.201433918554999813, -77.94678050555000937, 12.61309089657999927 ) ) ;
#56593 = EDGE_CURVE ( 'NONE', #41153, #8320, #33049, .T. ) ;
#56594 = CARTESIAN_POINT ( 'NONE',  ( -5.104594291233171433, -78.03651714374842641, -9.559420401355287922 ) ) ;
#56595 = CARTESIAN_POINT ( 'NONE',  ( 5.891627775763704555, -78.36429044821750267, -10.19952481748152984 ) ) ;
#56596 = CARTESIAN_POINT ( 'NONE',  ( 1.199999995321999968, -75.00000000467838390, -7.199999972488000388 ) ) ;
#56597 = CARTESIAN_POINT ( 'NONE',  ( -5.822602226006999615, -76.66743281994000370, -10.90510414457000010 ) ) ;
#56598 = VERTEX_POINT ( 'NONE', #2576 ) ;
#56599 = CARTESIAN_POINT ( 'NONE',  ( -8.418594644163000851, -80.80783708579305369, -7.485750452785000064 ) ) ;
#56600 = DIRECTION ( 'NONE',  ( 8.659560562353647261E-17, -0.7071067811866525998, 0.7071067811864425456 ) ) ;
#56601 = CARTESIAN_POINT ( 'NONE',  ( 12.43571054531000186, -61.67980566386000163, 0.4385525234352000146 ) ) ;
#56602 = CARTESIAN_POINT ( 'NONE',  ( -10.06619577067999849, -78.63438750088999996, -7.895242330167000055 ) ) ;
#56603 = CARTESIAN_POINT ( 'NONE',  ( 12.79971535682999928, -55.00965922235999983, -2.019101350716999921 ) ) ;
#56604 = CARTESIAN_POINT ( 'NONE',  ( -8.705161348369998109, -77.92823810661599282, -4.119875709756000148 ) ) ;
#56605 = CARTESIAN_POINT ( 'NONE',  ( 1.579899301681999990, -82.16450739290000627, 0.5283722218587000308 ) ) ;
#56606 = CARTESIAN_POINT ( 'NONE',  ( 0.4236292209062061387, -79.97211130723771078, 10.75836326857063696 ) ) ;
#56607 = CARTESIAN_POINT ( 'NONE',  ( -1.397510954313999854, -79.53369273832200292, -0.8088121278437000461 ) ) ;
#56608 = ORIENTED_EDGE ( 'NONE', *, *, #14950, .F. ) ;
#56609 = CARTESIAN_POINT ( 'NONE',  ( 0.000000000000000000, -77.50000000000000000, 0.000000000000000000 ) ) ;
#56610 = AXIS2_PLACEMENT_3D ( 'NONE', #26392, #21684, #13700 ) ;
#56611 = AXIS2_PLACEMENT_3D ( 'NONE', #3160, #11729, #17298 ) ;
#56612 = CARTESIAN_POINT ( 'NONE',  ( 0.8389761809808545800, -78.91645938753869416, -3.390143433233239190 ) ) ;
#56613 = EDGE_LOOP ( 'NONE', ( #28447, #33357, #52614, #37301 ) ) ;
#56614 = CARTESIAN_POINT ( 'NONE',  ( -10.64215094251999894, -79.78966949086598959, 2.340290094375000240 ) ) ;
#56615 = CARTESIAN_POINT ( 'NONE',  ( -1.456717367586000012E-14, -79.29999999999999716, 0.000000000000000000 ) ) ;
#56616 = CARTESIAN_POINT ( 'NONE',  ( 0.1431601642728717039, -80.73480119803696198, -1.243017257267813758 ) ) ;
#56617 = ORIENTED_EDGE ( 'NONE', *, *, #27096, .F. ) ;
#56618 = CARTESIAN_POINT ( 'NONE',  ( 5.569438312554999548, -79.02790074527499087, 10.68535195481999978 ) ) ;
#56619 = CARTESIAN_POINT ( 'NONE',  ( 11.18830539140000013, -77.79468742103497902, -1.736105152156000031 ) ) ;
#56620 = ORIENTED_EDGE ( 'NONE', *, *, #25748, .F. ) ;
#56621 = ORIENTED_EDGE ( 'NONE', *, *, #49946, .F. ) ;
#56622 = CARTESIAN_POINT ( 'NONE',  ( 0.07224473200327397038, -80.47101823697612133, 1.250019735964936540 ) ) ;
#56623 = PRESENTATION_LAYER_ASSIGNMENT (  '', '', ( #17122 ) ) ;
#56624 = ADVANCED_FACE ( 'NONE', ( #28835 ), #3808, .F. ) ;
#56625 = CARTESIAN_POINT ( 'NONE',  ( -3.576074390260000069, -86.31452044231799903, 1.592170898656000144 ) ) ;
#56626 = CARTESIAN_POINT ( 'NONE',  ( 8.944729675425000082, -79.91305337584603308, 3.923329690209000908 ) ) ;
#56627 = ORIENTED_EDGE ( 'NONE', *, *, #31742, .F. ) ;
#56628 = CARTESIAN_POINT ( 'NONE',  ( 12.77649795258999887, -53.49168567723999956, -0.06462540730615000395 ) ) ;
#56629 = CARTESIAN_POINT ( 'NONE',  ( -5.128001663057999870, -78.48732223094400240, 9.637373342098999984 ) ) ;
#56630 = AXIS2_PLACEMENT_3D ( 'NONE', #47052, #6581, #56761 ) ;
#56631 = ADVANCED_FACE ( 'NONE', ( #56304 ), #16325, .F. ) ;
#56632 = VERTEX_POINT ( 'NONE', #39154 ) ;
#56633 = CARTESIAN_POINT ( 'NONE',  ( 1.245336569551569461, -79.38326152196685825, -0.2691890748858687399 ) ) ;
#56634 = CARTESIAN_POINT ( 'NONE',  ( 9.723174505952000501, -24.47697504198000118, 7.958760297001999717 ) ) ;
#56635 = CARTESIAN_POINT ( 'NONE',  ( 7.618394506877000261, -55.57286435768999411, 10.53494428257999971 ) ) ;
#56636 = CARTESIAN_POINT ( 'NONE',  ( 1.499999999999999778, -80.66041666666667709, 0.1963495408493654004 ) ) ;
#56637 = CYLINDRICAL_SURFACE ( 'NONE', #19467, 1.000000000000000000 ) ;
#56638 = CARTESIAN_POINT ( 'NONE',  ( -4.000000000000000000, -78.67389998644428317, 2.834003763004000336E-08 ) ) ;
#56639 = CARTESIAN_POINT ( 'NONE',  ( 0.5355496356945241843, -80.72104928547346958, 11.19811601257680600 ) ) ;
#56640 = EDGE_CURVE ( 'NONE', #54974, #16476, #9010, .T. ) ;
#56641 = CARTESIAN_POINT ( 'NONE',  ( 8.272973658470998970, -78.33566108400613359, -8.664523719228998999 ) ) ;
#56642 = CARTESIAN_POINT ( 'NONE',  ( 2.622047509604808369, -80.74270833505833878, -3.088315007378679589 ) ) ;
#56643 = CARTESIAN_POINT ( 'NONE',  ( -1.476182556144000069, -76.33256575806998967, 12.22114576030999977 ) ) ;
#56644 = CIRCLE ( 'NONE', #4808, 1.250000000000000444 ) ;
#56645 = CARTESIAN_POINT ( 'NONE',  ( 3.275079823525000045, -80.80932046129099433, -2.584646448766000137 ) ) ;
#56646 = AXIS2_PLACEMENT_3D ( 'NONE', #35920, #826, #53951 ) ;
#56647 = CARTESIAN_POINT ( 'NONE',  ( 9.574841743191999655, -78.09026001420200203, 2.407137649543000357 ) ) ;
#56648 = CARTESIAN_POINT ( 'NONE',  ( 9.395758989587999821, -61.50491532550999096, -8.188252216855000043 ) ) ;
#56649 = CARTESIAN_POINT ( 'NONE',  ( -5.531768889155999958, -79.03576085112999294, -10.94525552207000096 ) ) ;
#56650 = CARTESIAN_POINT ( 'NONE',  ( 8.135116633385999663, -76.81570000444999380, 9.200136113044999675 ) ) ;
#56651 = DIRECTION ( 'NONE',  ( 1.000000000000000000, 0.000000000000000000, 0.000000000000000000 ) ) ;
#56652 = CARTESIAN_POINT ( 'NONE',  ( 9.199999999999999289, -77.00000000000000000, 0.000000000000000000 ) ) ;
#56653 = CARTESIAN_POINT ( 'NONE',  ( 7.374560639698993114, -77.97708333333332575, -9.596002108778149520 ) ) ;
#56654 = ORIENTED_EDGE ( 'NONE', *, *, #53, .T. ) ;
#56655 = CARTESIAN_POINT ( 'NONE',  ( -0.6248080770815239715, -80.84104275701125175, -1.377230163493380788 ) ) ;
#56656 = CARTESIAN_POINT ( 'NONE',  ( -8.075449341071999854, -77.47831109735399480, 4.776159278919000606 ) ) ;
#56657 = CARTESIAN_POINT ( 'NONE',  ( 1.933650113856000052, -23.40786253026000097, 12.70909635754000000 ) ) ;
#56658 = DIRECTION ( 'NONE',  ( -0.9999999999999694689, -2.469236813514923644E-07, 1.229032068775961321E-12 ) ) ;
#56659 = ADVANCED_FACE ( 'NONE', ( #53026 ), #30857, .F. ) ;
#56660 = CARTESIAN_POINT ( 'NONE',  ( 1.130171038138000128, -3.119265194441000144, -3.373452425123000253 ) ) ;
#56661 = CARTESIAN_POINT ( 'NONE',  ( -5.775534476593000122, -77.85550402086698796, 10.70634074252000012 ) ) ;
#56662 = CARTESIAN_POINT ( 'NONE',  ( 9.738918081334000831, -77.52175129689300093, 0.1147619655163999997 ) ) ;
#56663 = DIRECTION ( 'NONE',  ( 0.000000000000000000, 1.000000000000000000, 0.000000000000000000 ) ) ;
#56664 = CARTESIAN_POINT ( 'NONE',  ( -1.376471765390000046, -82.17166142314999888, -0.5116381728330999801 ) ) ;
#56665 = CARTESIAN_POINT ( 'NONE',  ( -9.692003024890606611, -79.56447609509856989, 4.663514834557163091 ) ) ;
#56666 = ORIENTED_EDGE ( 'NONE', *, *, #36905, .T. ) ;
#56667 = CARTESIAN_POINT ( 'NONE',  ( -0.7186926218484306350, -80.98590376313251227, -1.352462990148321831 ) ) ;
#56668 = CARTESIAN_POINT ( 'NONE',  ( 5.024405752997999741, -79.03188383819500018, 10.94290901707999986 ) ) ;
#56669 = CARTESIAN_POINT ( 'NONE',  ( 2.375899324488051523, -79.10491627289971461, 9.218980594236693804 ) ) ;
#56670 = AXIS2_PLACEMENT_3D ( 'NONE', #1965, #20247, #5782 ) ;
#56671 = CARTESIAN_POINT ( 'NONE',  ( 1.250000000000000000, -23.25000000000000000, 12.50000000000000000 ) ) ;
#56672 = CARTESIAN_POINT ( 'NONE',  ( -7.645398488040000551, -60.01531609111000165, 10.18948971875999909 ) ) ;
#56673 = DIRECTION ( 'NONE',  ( -0.7071067811865475727, 0.000000000000000000, 0.7071067811865475727 ) ) ;
#56674 = CARTESIAN_POINT ( 'NONE',  ( -4.562954320814999853, -78.99378279017300031, 8.400624927051000057 ) ) ;
#56675 = DIRECTION ( 'NONE',  ( -0.7071067811865474617, 0.000000000000000000, -0.7071067811865474617 ) ) ;
#56676 = CARTESIAN_POINT ( 'NONE',  ( 2.879226727952094222, -78.74583333333333712, -10.71369944335146940 ) ) ;
#56677 = ORIENTED_EDGE ( 'NONE', *, *, #22628, .F. ) ;
#56678 = ADVANCED_FACE ( 'NONE', ( #16726 ), #3599, .F. ) ;
#56679 = CARTESIAN_POINT ( 'NONE',  ( 0.000000000000000000, 4.040000000000000036, 0.000000000000000000 ) ) ;
#56680 = CARTESIAN_POINT ( 'NONE',  ( 1.784652037779075551, -79.18669371328248019, -11.69830041377290542 ) ) ;
#56681 = CARTESIAN_POINT ( 'NONE',  ( -2.042798482360907997, -78.62148120184446043, 3.387993325967679770 ) ) ;
#56682 = CARTESIAN_POINT ( 'NONE',  ( 1.102516846580866128, -81.38947583744716496, 0.5887672520915298024 ) ) ;
#56683 = CARTESIAN_POINT ( 'NONE',  ( 1.617840321509000034, -80.09877138898998794, 0.3973055507782000118 ) ) ;
#56684 = ORIENTED_EDGE ( 'NONE', *, *, #6168, .F. ) ;
#56685 = CARTESIAN_POINT ( 'NONE',  ( 1.308909830689670484, -78.41327112893952744, 0.2203332426835378777 ) ) ;
#56686 = AXIS2_PLACEMENT_3D ( 'NONE', #5642, #50829, #18659 ) ;
#56687 = CARTESIAN_POINT ( 'NONE',  ( 0.5999999999999999778, -5.000000000000000000, -4.000000000000000000 ) ) ;
#56688 = CARTESIAN_POINT ( 'NONE',  ( 3.521764644577042080, -82.09527493484321781, -0.7485738383772502225 ) ) ;
#56689 = VECTOR ( 'NONE', #29870, 1000.000000000000000 ) ;
#56690 = CARTESIAN_POINT ( 'NONE',  ( 0.000000000000000000, 0.000000000000000000, -12.00000000000000000 ) ) ;
#56691 = ADVANCED_FACE ( 'NONE', ( #28476 ), #44627, .F. ) ;
#56692 = LINE ( 'NONE', #48136, #16774 ) ;
#56693 = EDGE_LOOP ( 'NONE', ( #52130, #54847, #9651, #46251 ) ) ;
#56694 = ORIENTED_EDGE ( 'NONE', *, *, #42819, .T. ) ;
#56695 = CARTESIAN_POINT ( 'NONE',  ( 12.37782695028000113, -77.06200795437399620, -2.293983437537999936 ) ) ;
#56696 = CARTESIAN_POINT ( 'NONE',  ( -5.679944600031325841, -78.68085203632810476, -9.133896387890597879 ) ) ;
#56697 = ADVANCED_FACE ( 'NONE', ( #30791 ), #47441, .F. ) ;
#56698 = ORIENTED_EDGE ( 'NONE', *, *, #33195, .T. ) ;
#56699 = CARTESIAN_POINT ( 'NONE',  ( 7.633502222236000279, -18.79895684643999942, 10.36289759016999845 ) ) ;
#56700 = CARTESIAN_POINT ( 'NONE',  ( 10.61613183210000066, -77.36922082312399596, -2.999913216257000137 ) ) ;
#56701 = FACE_OUTER_BOUND ( 'NONE', #5944, .T. ) ;
#56702 = CARTESIAN_POINT ( 'NONE',  ( 5.917523019358082337, -75.96666666666665435, -10.26699006316252394 ) ) ;
#56703 = CARTESIAN_POINT ( 'NONE',  ( 6.861116763436999832, -76.75513797953000505, -9.781075755418999762 ) ) ;
#56704 = CARTESIAN_POINT ( 'NONE',  ( -2.787192588043336805, -79.70418878019351894, -10.40599190913065719 ) ) ;
#56705 = LINE ( 'NONE', #43708, #35281 ) ;
#56706 = CARTESIAN_POINT ( 'NONE',  ( -2.350111744379427048, -86.09999999999998010, 3.172282531659214033 ) ) ;
#56707 = CARTESIAN_POINT ( 'NONE',  ( -1.472820794058999905, -78.44820733118199030, -10.90095403661999995 ) ) ;
#56708 = CARTESIAN_POINT ( 'NONE',  ( 3.536272283845561581, -79.94387417217693326, 8.547291296781429182 ) ) ;
#56709 = EDGE_CURVE ( 'NONE', #46904, #11745, #52870, .T. ) ;
#56710 = ORIENTED_EDGE ( 'NONE', *, *, #19989, .T. ) ;
#56711 = CARTESIAN_POINT ( 'NONE',  ( 8.130813118348999780, -54.11476110100999648, -9.546856411313999757 ) ) ;
#56712 = ORIENTED_EDGE ( 'NONE', *, *, #14771, .T. ) ;
#56713 = CARTESIAN_POINT ( 'NONE',  ( 7.485102092340309987, -77.30010087969016297, -5.434593418087672489 ) ) ;
#56714 = CARTESIAN_POINT ( 'NONE',  ( -0.5991125319583999742, -80.32943159551300027, -1.175427489992000085 ) ) ;
#56715 = CARTESIAN_POINT ( 'NONE',  ( -12.76303204517000012, -18.73514852243999940, 1.980584515753000208 ) ) ;
#56716 = CARTESIAN_POINT ( 'NONE',  ( -4.531967804315558013, -77.44181088446534034, -10.26074445566288063 ) ) ;
#56717 = UNCERTAINTY_MEASURE_WITH_UNIT (LENGTH_MEASURE( 1.000000000000000082E-05 ), #47884, 'distance_accuracy_value', 'NONE');
#56718 = CARTESIAN_POINT ( 'NONE',  ( 0.9474668951539000350, -77.91944336237389734, 1.054687619119999864 ) ) ;
#56719 = CARTESIAN_POINT ( 'NONE',  ( 13.86301033151699791, -46.43897132165000130, 0.1317488955328562639 ) ) ;
#56720 = CARTESIAN_POINT ( 'NONE',  ( 0.1982664792347280658, -81.63720639545748270, -1.259862767458886257 ) ) ;
#56721 = CARTESIAN_POINT ( 'NONE',  ( 0.1429208184976999974, -78.69761083655998846, 1.621183732314999792 ) ) ;
#56722 = LINE ( 'NONE', #35117, #29980 ) ;
#56723 = CARTESIAN_POINT ( 'NONE',  ( -1.249811141842820161, -79.10985391374313735, -0.1498213877793858617 ) ) ;
#56724 = CARTESIAN_POINT ( 'NONE',  ( -7.069392057028999865, -79.42331078153999613, 8.491265488204000178 ) ) ;
#56725 = CARTESIAN_POINT ( 'NONE',  ( 0.000000000000000000, -0.6500000000000000222, 0.000000000000000000 ) ) ;
#56726 = LINE ( 'NONE', #19841, #47025 ) ;
#56727 = CARTESIAN_POINT ( 'NONE',  ( -8.838834764832000701, -60.04999999966999980, -8.838834764832000701 ) ) ;
#56728 = ORIENTED_EDGE ( 'NONE', *, *, #17154, .F. ) ;
#56729 = CARTESIAN_POINT ( 'NONE',  ( -2.952210844699811432, -77.20000000000000284, 10.42826508716522227 ) ) ;
#56730 = AXIS2_PLACEMENT_3D ( 'NONE', #45628, #23170, #27004 ) ;
#56731 = CARTESIAN_POINT ( 'NONE',  ( 0.8102226603197999477, -80.22566409777999752, 1.363061245571999924 ) ) ;
#56732 = CARTESIAN_POINT ( 'NONE',  ( 9.931052046391080523, -60.92278631056069571, 7.764003813279091837 ) ) ;
#56733 = CARTESIAN_POINT ( 'NONE',  ( 2.956870837876000468, -78.85316765784999404, 11.44999256673999888 ) ) ;
#56734 = CARTESIAN_POINT ( 'NONE',  ( -9.469606800734000629, -80.05752053325198858, 5.597012331546999953 ) ) ;
#56735 = AXIS2_PLACEMENT_3D ( 'NONE', #31167, #18216, #9934 ) ;
#56736 = CARTESIAN_POINT ( 'NONE',  ( 1.104063888217883260, -78.95871505373607135, -0.6377135191370438827 ) ) ;
#56737 = CARTESIAN_POINT ( 'NONE',  ( -2.021854267373811354, -1.826358988587633680, -2.882029951968737791 ) ) ;
#56738 = CARTESIAN_POINT ( 'NONE',  ( 2.013632425233999879, -78.27165194988499763, -9.512575055159999238 ) ) ;
#56739 = CARTESIAN_POINT ( 'NONE',  ( -6.639445101857000431, -77.70666193574498948, -6.825550891425999467 ) ) ;
#56740 = CARTESIAN_POINT ( 'NONE',  ( 0.4517135710334128085, -81.25462243997134237, -1.165398785623916522 ) ) ;
#56741 = CARTESIAN_POINT ( 'NONE',  ( 8.060704535212000366, -78.21769278298098982, -7.362092663522000535 ) ) ;
#56742 = CARTESIAN_POINT ( 'NONE',  ( 7.293551704196000962, -80.70985390147936300, -8.114658963368000855 ) ) ;
#56743 = CARTESIAN_POINT ( 'NONE',  ( -0.3336506835427100470, -81.54586305396269097, 1.229856053167274421 ) ) ;
#56744 = ORIENTED_EDGE ( 'NONE', *, *, #23668, .F. ) ;
#56745 = CARTESIAN_POINT ( 'NONE',  ( -9.250000000000007105, -78.98958333333331439, 1.210822168571027868 ) ) ;
#56746 = CARTESIAN_POINT ( 'NONE',  ( 0.4802748259344000181, -61.80526907249000601, -12.54896097838000024 ) ) ;
#56747 = FACE_OUTER_BOUND ( 'NONE', #32391, .T. ) ;
#56748 = CARTESIAN_POINT ( 'NONE',  ( -9.505686244346000180, -79.32818954342899076, 5.486888517706000279 ) ) ;
#56749 = CARTESIAN_POINT ( 'NONE',  ( 9.966224254735001509, -23.66904904784999886, -7.657729124005999921 ) ) ;
#56750 = CARTESIAN_POINT ( 'NONE',  ( 1.036720466796444917, -85.13645834259065737, -3.915773151610196567 ) ) ;
#56751 = CARTESIAN_POINT ( 'NONE',  ( 8.164775677042001689, -76.39296509471499519, 9.001221300116000634 ) ) ;
#56752 = CARTESIAN_POINT ( 'NONE',  ( 1.250000000000000000, -76.29999999999999716, 0.6999999999999999556 ) ) ;
#56753 = CARTESIAN_POINT ( 'NONE',  ( -10.18248259422395385, -61.09095036164143266, 7.792398156856014779 ) ) ;
#56754 = ORIENTED_EDGE ( 'NONE', *, *, #2708, .F. ) ;
#56755 = EDGE_CURVE ( 'NONE', #16171, #16697, #7007, .T. ) ;
#56756 = CARTESIAN_POINT ( 'NONE',  ( 9.892383529026000488, -78.85464906837700028, -4.882876457188000785 ) ) ;
#56757 = CARTESIAN_POINT ( 'NONE',  ( -1.197877150778747124, -80.07738762097918084, 0.3567682535721993786 ) ) ;
#56758 = CARTESIAN_POINT ( 'NONE',  ( 0.000000000000000000, -78.49999999999998579, 0.000000000000000000 ) ) ;
#56759 = COLOUR_RGB ( '', 0.09019608, 0.27058824, 0.51372549) ;
#56760 = CARTESIAN_POINT ( 'NONE',  ( -1.319038368507000181, -78.35863250589198969, -11.07933831235000177 ) ) ;
#56761 = DIRECTION ( 'NONE',  ( 1.000000000000000000, 0.000000000000000000, 0.000000000000000000 ) ) ;
#56762 = DIRECTION ( 'NONE',  ( 2.622169155355999834E-09, -1.000000000000000000, 6.038616382182999929E-09 ) ) ;
#56763 = CARTESIAN_POINT ( 'NONE',  ( 1.218014849295945723, -78.87111806999728003, 0.3275086013355714143 ) ) ;
#56764 = CARTESIAN_POINT ( 'NONE',  ( 0.8897706433943217696, -82.17524539450347731, 1.268930192044961380 ) ) ;
#56765 = CARTESIAN_POINT ( 'NONE',  ( -0.6126584217143548061, -79.68445856097022784, -1.092851559434964814 ) ) ;
#56766 = DIRECTION ( 'NONE',  ( -1.000000000000000000, 0.000000000000000000, 0.000000000000000000 ) ) ;
#56767 = B_SPLINE_CURVE_WITH_KNOTS ( 'NONE', 3,
 ( #17242, #8383, #26381, #21955, #13390, #44401, #8681, #39967 ),
 .UNSPECIFIED., .F., .F.,
 ( 4, 2, 2, 4 ),
 ( 0.000000000000000000, 0.5000000000000026645, 0.7500000000000013323, 1.000000000000000000 ),
 .UNSPECIFIED. ) ;
#56768 = CARTESIAN_POINT ( 'NONE',  ( -12.66736977981000045, -24.23307288772000234, 1.690635117038000068 ) ) ;
#56769 = ORIENTED_EDGE ( 'NONE', *, *, #14422, .F. ) ;
#56770 = EDGE_LOOP ( 'NONE', ( #47205, #5277, #15149, #16616, #24133, #10369, #39420 ) ) ;
#56771 = DIRECTION ( 'NONE',  ( 0.000000000000000000, -1.000000000000000000, 0.000000000000000000 ) ) ;
#56772 = ADVANCED_FACE ( 'NONE', ( #44988 ), #35644, .F. ) ;
#56773 = CIRCLE ( 'NONE', #51136, 1.250000000000000000 ) ;
#56774 = VERTEX_POINT ( 'NONE', #37280 ) ;
#56775 = EDGE_LOOP ( 'NONE', ( #2092, #10229, #24237, #1967, #28286, #2449 ) ) ;
#56776 = CARTESIAN_POINT ( 'NONE',  ( 10.18114973714000016, -23.39009320411999937, 7.633087466104000463 ) ) ;
#56777 = CARTESIAN_POINT ( 'NONE',  ( -7.595061814885000651, -78.00963867675800145, 7.841581601742999119 ) ) ;
#56778 = CARTESIAN_POINT ( 'NONE',  ( 0.000000000000000000, -74.99999999999998579, 0.000000000000000000 ) ) ;
#56779 = CARTESIAN_POINT ( 'NONE',  ( 4.634092916811999530, -78.85731332859899112, -8.633860817301998836 ) ) ;
#56780 = DIRECTION ( 'NONE',  ( 0.000000000000000000, 0.000000000000000000, -1.000000000000000000 ) ) ;
#56781 = ADVANCED_FACE ( 'NONE', ( #50884 ), #14258, .F. ) ;
#56782 = ORIENTED_EDGE ( 'NONE', *, *, #36617, .F. ) ;
#56783 = ORIENTED_EDGE ( 'NONE', *, *, #43376, .T. ) ;
#56784 = CARTESIAN_POINT ( 'NONE',  ( -7.230939086545548733, -77.54644391223615685, 5.768963832296065242 ) ) ;
#56785 = CARTESIAN_POINT ( 'NONE',  ( 2.425729133266999670E-14, -6.000000000000000000, 0.000000000000000000 ) ) ;
#56786 = EDGE_CURVE ( 'NONE', #425, #1025, #32079, .T. ) ;
#56787 = LINE ( 'NONE', #31338, #38018 ) ;
#56788 = CARTESIAN_POINT ( 'NONE',  ( 9.690463944985998168, -78.57592316806800170, -0.5153813127049999832 ) ) ;
#56789 = CIRCLE ( 'NONE', #31304, 0.5000000000000006661 ) ;
#56790 = CARTESIAN_POINT ( 'NONE',  ( 1.592434616855475493, -86.09999999999978115, 3.669353075276663656 ) ) ;
#56791 = LINE ( 'NONE', #20202, #40750 ) ;
#56792 = CARTESIAN_POINT ( 'NONE',  ( 5.413904038987179312, -76.66666666666664298, -9.393203674808262349 ) ) ;
#56793 = CARTESIAN_POINT ( 'NONE',  ( -1.870137171474999915, -80.04186706810699548, -11.09839649295000008 ) ) ;
#56794 = CARTESIAN_POINT ( 'NONE',  ( -1.666294527194000175, -79.78650139976998901, -0.3511123450079000063 ) ) ;
#56795 = DIRECTION ( 'NONE',  ( 1.000000000000000000, 0.000000000000000000, 0.000000000000000000 ) ) ;
#56796 = B_SPLINE_CURVE_WITH_KNOTS ( 'NONE', 3,
 ( #27866, #45913, #5449, #23452, #19034, #16057, #16635, #29896, #34619, #33757, #3062, #21058, #38773, #43216, #34331, #47668, #7772, #2203, #11638, #24625, #56502, #2772, #7194, #39059 ),
 .UNSPECIFIED., .F., .F.,
 ( 4, 2, 2, 2, 2, 2, 2, 2, 2, 2, 2, 4 ),
 ( 0.000000000000000000, 0.1250000000000037748, 0.2500000000000075495, 0.3750000000000113243, 0.4375000000000126010, 0.5000000000000138778, 0.6250000000000164313, 0.7500000000000189848, 0.8125000000000188738, 0.8437500000000172085, 0.8750000000000156541, 1.000000000000000000 ),
 .UNSPECIFIED. ) ;
#56797 = CARTESIAN_POINT ( 'NONE',  ( -7.646944981205999525, -55.60364172484999301, 10.19022195329000091 ) ) ;
#56798 = CARTESIAN_POINT ( 'NONE',  ( 2.029274658824999911, -78.14848667140098826, -9.586470329786999756 ) ) ;
#56799 = CARTESIAN_POINT ( 'NONE',  ( -0.08519377839585000334, -78.57724874519199432, 11.97951611939999950 ) ) ;
#56800 = CARTESIAN_POINT ( 'NONE',  ( -8.359900899578630415E-07, -76.12787248224110215, -11.82848710057588626 ) ) ;
#56802 = CARTESIAN_POINT ( 'NONE',  ( 0.9781264271452999592, -17.05968856123000066, -12.65967462879000038 ) ) ;
#56801 = CARTESIAN_POINT ( 'NONE',  ( 7.642160924870000649, -56.01538333533000014, 10.55911395186000057 ) ) ;
#56803 = ADVANCED_FACE ( 'NONE', ( #46461 ), #34686, .F. ) ;
#56804 = DIRECTION ( 'NONE',  ( 0.000000000000000000, -1.000000000000000000, -7.916704280318000023E-14 ) ) ;
#56805 = CARTESIAN_POINT ( 'NONE',  ( 9.105092338905999227, -80.29234472691199187, 6.490636970390999849 ) ) ;
#56806 = CARTESIAN_POINT ( 'NONE',  ( -4.000000000000000000, -5.200000000000000178, -0.5999999999999999778 ) ) ;
#56807 = CARTESIAN_POINT ( 'NONE',  ( 10.83766451684999943, -77.55149375871098982, -3.062514061775999608 ) ) ;
#56808 = CARTESIAN_POINT ( 'NONE',  ( -17.50000000000000000, -21.00000000000000000, 0.000000000000000000 ) ) ;
#56809 = CARTESIAN_POINT ( 'NONE',  ( 0.4149022863988324206, -1.615298193465790844, 3.592925692889842537 ) ) ;
#56810 = ORIENTED_EDGE ( 'NONE', *, *, #11460, .F. ) ;
#56811 = CARTESIAN_POINT ( 'NONE',  ( 11.75000000000000000, -76.55000000000001137, 0.000000000000000000 ) ) ;
#56812 = DIRECTION ( 'NONE',  ( 0.000000000000000000, 1.000000000000000000, 0.000000000000000000 ) ) ;
#56813 = CARTESIAN_POINT ( 'NONE',  ( 9.723199429438999175, -17.52306056078000296, -7.958735708418001487 ) ) ;
#56814 = CARTESIAN_POINT ( 'NONE',  ( 1.248526980818341237, -78.35470678600303529, 0.07396862603816467541 ) ) ;
#56815 = CARTESIAN_POINT ( 'NONE',  ( -3.403714747353000281, -1.627194400157000009, 0.2011706747331999945 ) ) ;
#56816 = CARTESIAN_POINT ( 'NONE',  ( -4.800609161379000511, -79.47659213876198692, -8.362561951962998563 ) ) ;
#56817 = TOROIDAL_SURFACE ( 'NONE', #54906, 17.50000000000000000, 5.000000000000000000 ) ;
#56818 = CARTESIAN_POINT ( 'NONE',  ( 9.500000000000000000, -79.04999999999999716, 0.000000000000000000 ) ) ;
#56819 = CARTESIAN_POINT ( 'NONE',  ( 1.798336774605999944, -59.99644498018999883, 12.61277771568000006 ) ) ;
#56820 = LINE ( 'NONE', #34359, #13451 ) ;
#56821 = EDGE_CURVE ( 'NONE', #33149, #34959, #11383, .T. ) ;
#56822 = CARTESIAN_POINT ( 'NONE',  ( 10.71369944335147828, -77.42916666666667425, -2.879226727952064913 ) ) ;
#56823 = ADVANCED_FACE ( 'NONE', ( #49863, #41279 ), #18849, .F. ) ;
#56824 = DIRECTION ( 'NONE',  ( 0.000000000000000000, -1.000000000000000000, 0.000000000000000000 ) ) ;
#56825 = CARTESIAN_POINT ( 'NONE',  ( -3.891189893006000045, -77.71055683836598860, 10.34924028849999900 ) ) ;
#56826 = CARTESIAN_POINT ( 'NONE',  ( 8.472913207660081270, -76.38898086387824549, -8.150121671469577223 ) ) ;
#56827 = CARTESIAN_POINT ( 'NONE',  ( 9.509459933319000413, -76.93343933509500232, 5.592128946851999238 ) ) ;
#56828 = CARTESIAN_POINT ( 'NONE',  ( -1.085757491496805560, -82.05909138311299955, 0.6269543719623986711 ) ) ;
#56829 = CARTESIAN_POINT ( 'NONE',  ( -6.294203684166999935, -77.14093373070529935, 7.343715272572999275 ) ) ;
#56830 = CARTESIAN_POINT ( 'NONE',  ( 0.7554284705563453217, -78.83333333333332860, 1.310679582531389276 ) ) ;
#56831 = CARTESIAN_POINT ( 'NONE',  ( 2.879226727952049814, -77.45416666666666572, 10.71369944335148183 ) ) ;
#56832 = CARTESIAN_POINT ( 'NONE',  ( 6.197920565227482470, -80.27432104992929851, -8.783392821118267690 ) ) ;
#56833 = CARTESIAN_POINT ( 'NONE',  ( 9.983882708737807476, -79.88084066504498537, 4.071020308803501742 ) ) ;
#56834 = CARTESIAN_POINT ( 'NONE',  ( -8.121706841748752126, -17.16372996695940500, -9.841114038392955621 ) ) ;
#56835 = CIRCLE ( 'NONE', #52159, 1.750000000000001332 ) ;
#56836 = TOROIDAL_SURFACE ( 'NONE', #20057, 13.50000000000000000, 0.5000000000000000000 ) ;
#56837 = CARTESIAN_POINT ( 'NONE',  ( 2.377756013412999803, -79.13915084896299845, -11.79209151100000064 ) ) ;
#56838 = CARTESIAN_POINT ( 'NONE',  ( -12.50000000000000000, -23.25000000000000000, -1.250000000000000000 ) ) ;
#56839 = FACE_OUTER_BOUND ( 'NONE', #46915, .T. ) ;
#56840 = ORIENTED_EDGE ( 'NONE', *, *, #6751, .F. ) ;
#56841 = CARTESIAN_POINT ( 'NONE',  ( 12.50240633877000107, -17.31762602171999887, 1.005381409788000058 ) ) ;
#56842 = ORIENTED_EDGE ( 'NONE', *, *, #41347, .F. ) ;
#56843 = ORIENTED_EDGE ( 'NONE', *, *, #30277, .T. ) ;
#56844 = CARTESIAN_POINT ( 'NONE',  ( 0.000000000000000000, -6.000000000000000000, 0.000000000000000000 ) ) ;
#56845 = ORIENTED_EDGE ( 'NONE', *, *, #23986, .T. ) ;
#56846 = CARTESIAN_POINT ( 'NONE',  ( 0.7877959022907999875, -81.32799336705899407, 3.456059736074999833 ) ) ;
#56847 = CARTESIAN_POINT ( 'NONE',  ( 2.963863982283218679, -79.24946267513759324, 9.025665246861352742 ) ) ;
#56848 = VERTEX_POINT ( 'NONE', #4085 ) ;
#56849 = CARTESIAN_POINT ( 'NONE',  ( -4.839793374392999503, -78.41318513125000322, 11.17717652876000045 ) ) ;
#56850 = CARTESIAN_POINT ( 'NONE',  ( 7.889735440105552833, -55.04957415510977370, -7.666647577137438496 ) ) ;
#56851 = ORIENTED_EDGE ( 'NONE', *, *, #44468, .T. ) ;
#56852 = CARTESIAN_POINT ( 'NONE',  ( -8.630529134780177358, -79.58500282387936409, -4.101029964751555568 ) ) ;
#56853 = CARTESIAN_POINT ( 'NONE',  ( -1.515185110494049470, -78.75829941884984464, -0.1588823915039442869 ) ) ;
#56854 = AXIS2_PLACEMENT_3D ( 'NONE', #29342, #34635, #52663 ) ;
#56855 = DIRECTION ( 'NONE',  ( 0.000000000000000000, -1.000000000000000000, 0.000000000000000000 ) ) ;
#56856 = PRODUCT ( 'Body', 'Body', '', ( #5722 ) ) ;
#56857 = CARTESIAN_POINT ( 'NONE',  ( -4.459282313423081234, -80.00899937169181442, 9.789565273130554246 ) ) ;
#56858 = FACE_OUTER_BOUND ( 'NONE', #26989, .T. ) ;
#56859 = CARTESIAN_POINT ( 'NONE',  ( -1.432420283025999996, -76.21911477132699986, 11.09153081809999897 ) ) ;
#56860 = CARTESIAN_POINT ( 'NONE',  ( -4.828331629711049899, -79.06770833335490067, 10.85705384256994677 ) ) ;
#56861 = CARTESIAN_POINT ( 'NONE',  ( -9.611650271896857944, -78.65833333333331723, 5.539808784079855997 ) ) ;
#56862 = AXIS2_PLACEMENT_3D ( 'NONE', #25122, #43145, #16276 ) ;
#56863 = CARTESIAN_POINT ( 'NONE',  ( 2.063533415121999948, -76.25127502049299721, 10.92068915710999910 ) ) ;
#56864 = CARTESIAN_POINT ( 'NONE',  ( -10.12290050253000118, -23.24999997822999731, 7.648026768374000639 ) ) ;
#56865 = CARTESIAN_POINT ( 'NONE',  ( -7.065445606947000634, -77.44843667140099797, 6.380536996790000082 ) ) ;
#56866 = CARTESIAN_POINT ( 'NONE',  ( -1.261445002938999860, -79.23443596263800259, -0.1968185027220000216 ) ) ;
#56867 = CARTESIAN_POINT ( 'NONE',  ( -10.31854526085034252, -80.12852127511105493, -3.810993520750592278 ) ) ;
#56868 = CARTESIAN_POINT ( 'NONE',  ( -1.428377931972672377, -3.012610289119709517, 2.918575344840368402 ) ) ;
#56869 = CARTESIAN_POINT ( 'NONE',  ( 3.705853105876000253, -80.60603455456799793, -0.6148291195716999447 ) ) ;
#56870 = VECTOR ( 'NONE', #25149, 1000.000000000000000 ) ;
#56871 = CARTESIAN_POINT ( 'NONE',  ( -4.368592420383399677, -78.00830336871821657, 9.822916132917713483 ) ) ;
#56872 = EDGE_CURVE ( 'NONE', #14936, #37124, #28328, .T. ) ;
#56873 = CARTESIAN_POINT ( 'NONE',  ( 1.153972371676974751, -82.88143275804098664, 0.4803910728602110436 ) ) ;
#56874 = CARTESIAN_POINT ( 'NONE',  ( 0.000000000000000000, -63.10294702885996543, 12.53545825868000207 ) ) ;
#56875 = CARTESIAN_POINT ( 'NONE',  ( -3.380460507093999478, -86.15517953870899248, 0.3696235703980000342 ) ) ;
#56876 = CARTESIAN_POINT ( 'NONE',  ( -8.407949263131950346, -76.26097042042334806, -8.207523428525416165 ) ) ;
#56877 = CARTESIAN_POINT ( 'NONE',  ( -0.2977330905706521147, -79.35624198045864830, -1.239186237762031739 ) ) ;
#56878 = B_SPLINE_SURFACE_WITH_KNOTS ( 'NONE', 3, 3, ( 
 ( #48959, #12357, #30346, #52804, #16796, #39791, #17364, #30921, #35350, #48388, #2651, #7639, #7926, #20928, #43093, #43950, #8502, #3501, #43664, #12075, #20645, #38929, #25926, #21503, #57515, #56946, #35057, #52235, #29766, #34488, #52518, #47823, #17075, #25639, #7353 ),
 ( #30056, #31810, #9687, #54845, #22074, #855, #27386, #35649, #27674, #45128, #18259, #26793, #49852, #4680, #22678, #572, #17662, #13516, #40981, #31510, #58398, #14106, #13217, #9397, #22379, #32103, #31211, #18839, #13808, #36253, #45422, #18551, #22971, #36832, #40689 ),
 ( #5255, #49555, #44822, #54567, #50144, #35951, #27090, #40083, #26497, #58099, #44521, #36545, #45720, #53677, #23262, #41271, #4376, #14391, #53977, #32389, #54274, #4072, #50433, #49250, #8801, #40389, #17960, #9100, #44227, #43943, #12917, #21780, #26786, #17952, #58093 ),
 ( #53085, #30631, #16789, #17653, #3776, #49243, #17068, #34772, #35944, #9093, #57507, #8793, #39784, #57798, #44815, #45122, #30915, #48381, #30339, #35344, #21497, #22370, #35641, #53971, #52796, #12351, #48951, #21204, #44514, #13509, #40382, #57224, #53669, #35050, #17356 ) ),
 .UNSPECIFIED., .F., .F., .F.,
 ( 4, 4 ),
 ( 4, 1, 1, 1, 1, 1, 1, 1, 1, 1, 1, 1, 1, 1, 1, 1, 1, 1, 1, 1, 1, 1, 1, 1, 1, 1, 1, 1, 1, 1, 1, 1, 4 ),
 ( -0.05371687727926999917, 1.053716877278999986 ),
 ( -0.02000000000000000042, 0.01250000000000000069, 0.04499999999999999833, 0.07749999999999999944, 0.1100000000000000006, 0.1424999999999999878, 0.1749999999999999889, 0.2074999999999999900, 0.2399999999999999911, 0.2725000000000000200, 0.3049999999999999933, 0.3375000000000000222, 0.3699999999999999956, 0.4025000000000000244, 0.4349999999999999978, 0.4675000000000000266, 0.5000000000000000000, 0.5324999999999999734, 0.5649999999999999467, 0.5975000000000000311, 0.6300000000000000044, 0.6624999999999999778, 0.6949999999999999512, 0.7275000000000000355, 0.7600000000000000089, 0.7924999999999999822, 0.8249999999999999556, 0.8575000000000000400, 0.8900000000000000133, 0.9224999999999999867, 0.9549999999999999600, 0.9875000000000000444, 1.020000000000000018 ),
 .UNSPECIFIED. ) ;
#56879 = CARTESIAN_POINT ( 'NONE',  ( -7.969039355710000549, -61.42377467811000002, -9.934746417661001416 ) ) ;
#56880 = ADVANCED_FACE ( 'NONE', ( #32399 ), #23273, .F. ) ;
#56881 = DIRECTION ( 'NONE',  ( 0.000000000000000000, -1.000000000000000000, 0.000000000000000000 ) ) ;
#56882 = CARTESIAN_POINT ( 'NONE',  ( -0.7554284705563480973, -77.58333333333332860, -1.310679582531387277 ) ) ;
#56883 = CARTESIAN_POINT ( 'NONE',  ( -1.500000000000000000, -80.40000000000000568, 0.000000000000000000 ) ) ;
#56884 = DIRECTION ( 'NONE',  ( 0.000000000000000000, -1.000000000000000000, 0.000000000000000000 ) ) ;
#56885 = LINE ( 'NONE', #16441, #34217 ) ;
#56886 = CARTESIAN_POINT ( 'NONE',  ( -9.247932426686000795, -77.50168256874098915, -0.1955654147372000162 ) ) ;
#56887 = CARTESIAN_POINT ( 'NONE',  ( -8.890802410117000676, -75.93226843290000261, 8.804145862534999978 ) ) ;
#56888 = VERTEX_POINT ( 'NONE', #18563 ) ;
#56889 = EDGE_CURVE ( 'NONE', #17310, #56405, #44529, .T. ) ;
#56890 = CARTESIAN_POINT ( 'NONE',  ( -2.612980907336999614, -80.35637179573859612, -10.95817168551000087 ) ) ;
#56891 = CARTESIAN_POINT ( 'NONE',  ( 3.380118192976000469, -85.79678895079199208, -1.504925579245999900 ) ) ;
#56892 = CARTESIAN_POINT ( 'NONE',  ( 12.77562710770000187, -62.06233677629000312, 0.5428386295906000303 ) ) ;
#56893 = CARTESIAN_POINT ( 'NONE',  ( 9.560585210696000757, -78.88929468166000447, 8.500609442439998276 ) ) ;
#56894 = CARTESIAN_POINT ( 'NONE',  ( -1.667917367010000040, -18.71943307332999851, -12.49306752634999995 ) ) ;
#56895 = CARTESIAN_POINT ( 'NONE',  ( -7.316919381717999826, -78.90167637952698954, 6.093690752987000359 ) ) ;
#56896 = CARTESIAN_POINT ( 'NONE',  ( -0.7862640713001000092, -84.38281177079799988, 4.097787363367999980 ) ) ;
#56897 = CARTESIAN_POINT ( 'NONE',  ( 4.236362259395971996, -79.94289841385737816, 9.879967597326936968 ) ) ;
#56898 = CARTESIAN_POINT ( 'NONE',  ( 0.6263439973055000554, -79.33524224479700138, 1.488256452092999949 ) ) ;
#56899 = ORIENTED_EDGE ( 'NONE', *, *, #27046, .T. ) ;
#56900 = CARTESIAN_POINT ( 'NONE',  ( 9.172146100395819346, -77.30629003610285110, -5.638845386412532967 ) ) ;
#56901 = CARTESIAN_POINT ( 'NONE',  ( -5.706217103757095011, -79.02772280010032091, 7.378253461501310007 ) ) ;
#56902 = CARTESIAN_POINT ( 'NONE',  ( 3.003961014100700044, -78.99951684686710962, -2.201084085522161171 ) ) ;
#56903 = EDGE_CURVE ( 'NONE', #26175, #3300, #52825, .T. ) ;
#56904 = EDGE_LOOP ( 'NONE', ( #18760, #41283, #11212, #20186 ) ) ;
#56905 = CARTESIAN_POINT ( 'NONE',  ( 3.197825632618000125, -79.65857183731299074, 10.57600109144000022 ) ) ;
#56906 = AXIS2_PLACEMENT_3D ( 'NONE', #5808, #50121, #42130 ) ;
#56907 = CARTESIAN_POINT ( 'NONE',  ( -7.601397897754999633, -60.04999999657000131, -10.07627163191000008 ) ) ;
#56908 = CARTESIAN_POINT ( 'NONE',  ( -8.391469517572000214, -79.68773307352599033, 7.000674649436000152 ) ) ;
#56909 = VERTEX_POINT ( 'NONE', #52712 ) ;
#56910 = CARTESIAN_POINT ( 'NONE',  ( -11.79389253715000052, -77.73916203849999818, 2.981045019388999684 ) ) ;
#56911 = VERTEX_POINT ( 'NONE', #4972 ) ;
#56912 = ORIENTED_EDGE ( 'NONE', *, *, #15348, .F. ) ;
#56913 = CARTESIAN_POINT ( 'NONE',  ( -0.3222441879806262066, -80.49579513225657479, 1.208098981363385560 ) ) ;
#56914 = AXIS2_PLACEMENT_3D ( 'NONE', #33723, #15726, #34297 ) ;
#56915 = DIRECTION ( 'NONE',  ( -0.7071067811865475727, 0.000000000000000000, -0.7071067811865475727 ) ) ;
#56916 = CARTESIAN_POINT ( 'NONE',  ( -0.5483576180056000116, -79.75069008456101471, -9.751923335751000010 ) ) ;
#56917 = ORIENTED_EDGE ( 'NONE', *, *, #22640, .T. ) ;
#56918 = CARTESIAN_POINT ( 'NONE',  ( 12.54977952612999914, -53.75167110003000204, -0.03756586072996999370 ) ) ;
#56919 = VERTEX_POINT ( 'NONE', #9995 ) ;
#56920 = CARTESIAN_POINT ( 'NONE',  ( -6.353892679860843273, -78.46935512297507387, 10.19451981771113402 ) ) ;
#56921 = CARTESIAN_POINT ( 'NONE',  ( 3.485499217012000273, -78.91452042059380290, -1.287490079826536515E-15 ) ) ;
#56922 = CARTESIAN_POINT ( 'NONE',  ( 8.958657468006999025, -53.59887336276000269, 8.950049500612998088 ) ) ;
#56923 = CARTESIAN_POINT ( 'NONE',  ( 9.433537730491899254, -16.87202052679777253, -8.532653828096353976 ) ) ;
#56924 = CARTESIAN_POINT ( 'NONE',  ( -0.7554284705563540925, -78.31666666666669130, 1.310679582531384391 ) ) ;
#56925 = CARTESIAN_POINT ( 'NONE',  ( -5.765467378296696310, -78.97462913613841806, 7.831529694205842773 ) ) ;
#56926 = CARTESIAN_POINT ( 'NONE',  ( 0.000000000000000000, -72.89999999999999147, 0.000000000000000000 ) ) ;
#56927 = CARTESIAN_POINT ( 'NONE',  ( -1.041898385056842402, -77.78530095164687452, 1.092208633748498636 ) ) ;
#56928 = CARTESIAN_POINT ( 'NONE',  ( -3.770920640554758840, -81.78333334665865095, -1.371725514654604350 ) ) ;
#56929 = CARTESIAN_POINT ( 'NONE',  ( -7.685416442687999172, -76.51934360383999945, -9.616126112745998711 ) ) ;
#56930 = CARTESIAN_POINT ( 'NONE',  ( 3.934265133962999705, -81.04982046129099160, 1.388561475457000149 ) ) ;
#56931 = PLANE ( 'NONE',  #26657 ) ;
#56932 = CARTESIAN_POINT ( 'NONE',  ( 9.108250977419000805, -61.67811334458999539, -8.478720681770999690 ) ) ;
#56933 = CARTESIAN_POINT ( 'NONE',  ( -5.950798862880000151, -78.86331654267000602, 10.72320280238000123 ) ) ;
#56934 = CARTESIAN_POINT ( 'NONE',  ( -9.801255020792000394, -76.44685535970599233, 7.399866681860999940 ) ) ;
#56935 = CARTESIAN_POINT ( 'NONE',  ( -7.398464061242883361, -60.25160423312483715, -8.140250184784974863 ) ) ;
#56936 = DIRECTION ( 'NONE',  ( 0.000000000000000000, 0.000000000000000000, -1.000000000000000000 ) ) ;
#56937 = CARTESIAN_POINT ( 'NONE',  ( 9.596002108778172612, -77.99791666666665435, -7.374560639698962028 ) ) ;
#56938 = CARTESIAN_POINT ( 'NONE',  ( -1.090924692763506121, -80.81067774974684426, -1.044066399784976618 ) ) ;
#56939 = CARTESIAN_POINT ( 'NONE',  ( -9.146705800622001448, -77.53052983129099118, -1.122373973676000114 ) ) ;
#56940 = DIRECTION ( 'NONE',  ( 0.000000000000000000, -1.000000000000000000, 0.000000000000000000 ) ) ;
#56941 = LINE ( 'NONE', #2645, #24764 ) ;
#56942 = CARTESIAN_POINT ( 'NONE',  ( -1.347195692331000005, -2.374444768727999922, 3.292799928894000416 ) ) ;
#56943 = CARTESIAN_POINT ( 'NONE',  ( 8.400721904471998513, -78.12679717510499700, -8.798318138657000631 ) ) ;
#56944 = CARTESIAN_POINT ( 'NONE',  ( -9.662137344075999223, -78.26077085424698510, 1.225886475437000023 ) ) ;
#56946 = CARTESIAN_POINT ( 'NONE',  ( 0.5643133282633999714, -78.90211458439600278, -1.192525073705999805 ) ) ;
#56945 = CARTESIAN_POINT ( 'NONE',  ( 6.586108526242999694, -80.07391735373440156, 8.810401493720998900 ) ) ;
#56947 = CARTESIAN_POINT ( 'NONE',  ( -0.3643839585117999991, -81.47675258327998904, 1.301227969886000091 ) ) ;
#56948 = CARTESIAN_POINT ( 'NONE',  ( -10.74994525727461259, -79.59655355021966727, 0.4779014380844182064 ) ) ;
#56949 = VERTEX_POINT ( 'NONE', #13228 ) ;
#56950 = ADVANCED_FACE ( 'NONE', ( #14116 ), #31418, .F. ) ;
#56951 = CARTESIAN_POINT ( 'NONE',  ( -3.882040082920265700, -78.80112713863415763, 11.40455788431460249 ) ) ;
#56952 = CARTESIAN_POINT ( 'NONE',  ( -7.282623421190000279, -79.61782371684098791, 9.589350811714000500 ) ) ;
#56953 = CARTESIAN_POINT ( 'NONE',  ( 5.720594865934685025, -79.07369316860736319, 7.609982227002291211 ) ) ;
#56954 = FACE_OUTER_BOUND ( 'NONE', #34825, .T. ) ;
#56955 = CARTESIAN_POINT ( 'NONE',  ( -1.413307538656764395, -76.24661458376434098, -10.80338542964358517 ) ) ;
#56956 = CARTESIAN_POINT ( 'NONE',  ( -3.425387549877999760, -0.6331479618548999655, -0.04975834668854000470 ) ) ;
#56957 = CARTESIAN_POINT ( 'NONE',  ( -4.510937018225000372, -79.79379212038298874, -8.678390893359001268 ) ) ;
#56958 = CARTESIAN_POINT ( 'NONE',  ( -1.338466228091430121, -79.37677412509060559, -0.4637437491872735129 ) ) ;
#56959 = DIRECTION ( 'NONE',  ( -0.9999548435846228323, 0.000000000000000000, -0.009503199022040218977 ) ) ;
#56960 = ORIENTED_EDGE ( 'NONE', *, *, #55235, .F. ) ;
#56961 = DIRECTION ( 'NONE',  ( 1.000000000000000000, 0.000000000000000000, 0.000000000000000000 ) ) ;
#56962 = CARTESIAN_POINT ( 'NONE',  ( 3.686727602956580530, -78.89922203454568717, 11.17960410108377367 ) ) ;
#56963 = CARTESIAN_POINT ( 'NONE',  ( -5.141276782405999946, -79.83708667140099635, -8.146626593840000652 ) ) ;
#56964 = CARTESIAN_POINT ( 'NONE',  ( 3.437187628289000152, -78.54828564506388489, 0.000000000000000000 ) ) ;
#56965 = CARTESIAN_POINT ( 'NONE',  ( 0.7545134501129999727, -80.72642064884999513, 1.485250302772000097 ) ) ;
#56966 = ADVANCED_FACE ( 'NONE', ( #19359 ), #37647, .F. ) ;
#56967 = AXIS2_PLACEMENT_3D ( 'NONE', #15676, #20117, #51419 ) ;
#56968 = VERTEX_POINT ( 'NONE', #28782 ) ;
#56969 = CARTESIAN_POINT ( 'NONE',  ( -1.262741469898344793, -79.16064077602601401, -0.1731769364601504491 ) ) ;
#56970 = DIRECTION ( 'NONE',  ( 0.000000000000000000, 1.000000000000000000, 0.000000000000000000 ) ) ;
#56971 = DIRECTION ( 'NONE',  ( 2.250403632142151042E-08, -0.7071067811865473507, 0.7071067811865473507 ) ) ;
#56972 = CARTESIAN_POINT ( 'NONE',  ( -1.092232985442824100, -78.45833333333328596, 0.6295237254636200097 ) ) ;
#56973 = CARTESIAN_POINT ( 'NONE',  ( 5.411006671257999834, -79.03782169632599164, 8.131518144102999557 ) ) ;
#56974 = ORIENTED_EDGE ( 'NONE', *, *, #49486, .T. ) ;
#56975 = ORIENTED_EDGE ( 'NONE', *, *, #28938, .F. ) ;
#56976 = CARTESIAN_POINT ( 'NONE',  ( 12.54822461858999993, -76.57021509471499598, -1.007481608483999924 ) ) ;
#56977 = CARTESIAN_POINT ( 'NONE',  ( 4.122725566465639702, -78.75634067257766446, -9.928003433801906752 ) ) ;
#56978 = VERTEX_POINT ( 'NONE', #46538 ) ;
#56979 = EDGE_CURVE ( 'NONE', #18217, #57339, #14178, .T. ) ;
#56980 = CARTESIAN_POINT ( 'NONE',  ( 2.459440699436000077, -77.33600584965400060, -9.171074077620000153 ) ) ;
#56981 = CARTESIAN_POINT ( 'NONE',  ( -11.00000000000000000, -77.69999999999998863, 0.000000000000000000 ) ) ;
#56982 = CARTESIAN_POINT ( 'NONE',  ( 1.538071403320016461, -75.93541666666665435, -11.74999999999999822 ) ) ;
#56983 = CARTESIAN_POINT ( 'NONE',  ( 12.51393054458000087, -76.81064262049000035, -3.351762257813000190 ) ) ;
#56984 = DIRECTION ( 'NONE',  ( 0.000000000000000000, 1.000000000000000000, 0.000000000000000000 ) ) ;
#56985 = DIRECTION ( 'NONE',  ( -0.7071067811865474617, 0.7071067811865474617, -2.768420520316182841E-09 ) ) ;
#56986 = CARTESIAN_POINT ( 'NONE',  ( -8.485281374238999419, -60.74999999967048581, -8.485281374238999419 ) ) ;
#56987 = CARTESIAN_POINT ( 'NONE',  ( 11.14115696400000033, -79.07464322022299541, -1.301050381412999890 ) ) ;
#56988 = CARTESIAN_POINT ( 'NONE',  ( 5.266508667217213890, -79.92729844318292010, 7.604169021590073463 ) ) ;
#56989 = ORIENTED_EDGE ( 'NONE', *, *, #46934, .T. ) ;
#56990 = CARTESIAN_POINT ( 'NONE',  ( 9.687280504270265880, -78.09832047880331629, 6.727404250420961240 ) ) ;
#56991 = ORIENTED_EDGE ( 'NONE', *, *, #9555, .T. ) ;
#56992 = CARTESIAN_POINT ( 'NONE',  ( 4.757299607910999484, -78.96112282211998945, 10.21259197296000032 ) ) ;
#56993 = CARTESIAN_POINT ( 'NONE',  ( 7.610095849401467660, -77.30199033518762519, -5.258407757687174389 ) ) ;
#56994 = CARTESIAN_POINT ( 'NONE',  ( 0.6743760579952999823, -80.63286640014699458, 1.247107161604999792 ) ) ;
#56995 = CARTESIAN_POINT ( 'NONE',  ( -1.092232985442822102, -83.04166666666664298, -0.6295237254636245616 ) ) ;
#56996 = CARTESIAN_POINT ( 'NONE',  ( 10.75931538509122021, -78.12271945951098928, 3.171551892671853334 ) ) ;
#56997 = CARTESIAN_POINT ( 'NONE',  ( -0.9215294167384999735, -77.67138024546849806, -1.077461862040000051 ) ) ;
#56998 = DIRECTION ( 'NONE',  ( -0.7071067811865475727, 0.000000000000000000, -0.7071067811865475727 ) ) ;
#56999 = CARTESIAN_POINT ( 'NONE',  ( -4.100000000000000533, -75.19999999999998863, 0.000000000000000000 ) ) ;
#57000 = CARTESIAN_POINT ( 'NONE',  ( 4.000000000000000000, -5.000000000000000000, -0.5999999999999999778 ) ) ;
#57001 = CARTESIAN_POINT ( 'NONE',  ( -1.980584515756000030, -55.53514849873000259, 12.76303204337999908 ) ) ;
#57002 = CARTESIAN_POINT ( 'NONE',  ( -8.774483958462999666, -78.50395412067899770, 6.892026619272999532 ) ) ;
#57003 = CARTESIAN_POINT ( 'NONE',  ( -8.392392323321001157, -76.96776167140099290, 4.494354236621999732 ) ) ;
#57004 = FACE_OUTER_BOUND ( 'NONE', #7543, .T. ) ;
#57005 = DIRECTION ( 'NONE',  ( 1.000000000000000000, 0.000000000000000000, 0.000000000000000000 ) ) ;
#57006 = CARTESIAN_POINT ( 'NONE',  ( -12.55433072267391914, -60.18725213688281173, -1.749897784984652427 ) ) ;
#57007 = EDGE_LOOP ( 'NONE', ( #18717, #9284, #7764, #30608 ) ) ;
#57008 = CARTESIAN_POINT ( 'NONE',  ( -1.631971144587999856, -81.85307101349999925, -0.4862994432698999892 ) ) ;
#57009 = VECTOR ( 'NONE', #45265, 1000.000000000000000 ) ;
#57010 = CARTESIAN_POINT ( 'NONE',  ( 1.561568621681000080, -79.65723116178999419, 0.2753811681071999806 ) ) ;
#57011 = DIRECTION ( 'NONE',  ( -1.000000000000000000, 0.000000000000000000, 0.000000000000000000 ) ) ;
#57012 = CARTESIAN_POINT ( 'NONE',  ( -9.964549960864999889, -77.51927491423099070, 6.650098383618000319 ) ) ;
#57013 = CARTESIAN_POINT ( 'NONE',  ( 4.495149389856036848, -77.00000000000000000, 8.113504219799731132 ) ) ;
#57014 = CARTESIAN_POINT ( 'NONE',  ( 0.1162945074421486008, -79.11773129756168998, 1.269215488990788954 ) ) ;
#57015 = DIRECTION ( 'NONE',  ( 1.000000000000000000, 0.000000000000000000, 0.000000000000000000 ) ) ;
#57016 = CARTESIAN_POINT ( 'NONE',  ( -5.600962501326000265, -78.05390194988500241, 7.948110234177999445 ) ) ;
#57017 = CARTESIAN_POINT ( 'NONE',  ( 9.403616370364000332, -77.90562873964798030, 1.497456306884999977 ) ) ;
#57018 = CARTESIAN_POINT ( 'NONE',  ( -10.67318205552422761, -76.59044953065486538, 1.292397307245511717 ) ) ;
#57019 = FACE_OUTER_BOUND ( 'NONE', #4485, .T. ) ;
#57020 = CARTESIAN_POINT ( 'NONE',  ( 10.90723107005969084, -75.97980330752400846, 4.369188860919290818 ) ) ;
#57021 = CARTESIAN_POINT ( 'NONE',  ( -1.274109108748103569, -82.15011936437316820, 0.001084848989539045992 ) ) ;
#57022 = VERTEX_POINT ( 'NONE', #46828 ) ;
#57023 = CARTESIAN_POINT ( 'NONE',  ( -11.74860111630057524, -78.68560678359739313, 2.073359527469779806 ) ) ;
#57024 = B_SPLINE_CURVE_WITH_KNOTS ( 'NONE', 3,
 ( #51095, #10647, #33920, #29773, #34205, #12081, #47549, #12650, #38936, #48113, #11798, #48678, #52524, #52242, #38651, #16802, #30063, #7645, #7074, #11516, #16513, #47829, #43375, #52811, #34495, #25076, #57521, #25645, #15933, #43671, #30643, #43100, #30352, #7360, #20367, #3229, #21218, #17082, #12363, #48395, #25359, #39225, #21510, #8222, #34786, #35063, #20934, #2933, #2657, #42806, #56669, #39516, #57238, #56953, #7932, #25933, #43959, #16225, #3508, #53100, #2369, #20651, #38360, #56382 ),
 .UNSPECIFIED., .F., .F.,
 ( 4, 2, 2, 2, 2, 2, 2, 2, 2, 2, 2, 2, 2, 2, 1, 1, 1, 1, 1, 2, 2, 2, 2, 2, 2, 2, 2, 2, 1, 2, 2, 2, 2, 2, 4 ),
 ( 0.5000000000000000000, 0.5312499999999996669, 0.5624999999999993339, 0.5937499999999990008, 0.6249999999999986677, 0.6406249999999985567, 0.6562499999999983347, 0.6718749999999982236, 0.6874999999999980016, 0.7031249999999977796, 0.7187499999999976685, 0.7343749999999975575, 0.7421874999999974465, 0.7460937499999973355, 0.7480468749999973355, 0.7490234374999973355, 0.7495117187499973355, 0.7497558593749973355, 0.7498779296874973355, 0.7499389648437473355, 0.7499999999999973355, 0.7812499999999976685, 0.8124999999999980016, 0.8281249999999982236, 0.8437499999999983347, 0.8593749999999984457, 0.8749999999999986677, 0.8906249999999987788, 0.9062499999999988898, 0.9218749999999991118, 0.9374999999999993339, 0.9531249999999994449, 0.9687499999999995559, 0.9843749999999997780, 1.000000000000000000 ),
 .UNSPECIFIED. ) ;
#57025 = EDGE_CURVE ( 'NONE', #5930, #22602, #2522, .T. ) ;
#57026 = CARTESIAN_POINT ( 'NONE',  ( 0.000000000000000000, -23.25000000000000000, -12.00000000000000000 ) ) ;
#57027 = AXIS2_PLACEMENT_3D ( 'NONE', #16964, #25526, #52978 ) ;
#57028 = CARTESIAN_POINT ( 'NONE',  ( -11.61792497750000130, -79.30050612125899079, 3.950725441919999970 ) ) ;
#57029 = CARTESIAN_POINT ( 'NONE',  ( 3.962812355711000212, -78.54828561723799396, -1.463672932855430986E-15 ) ) ;
#57030 = EDGE_CURVE ( 'NONE', #52919, #43451, #21096, .T. ) ;
#57031 = CARTESIAN_POINT ( 'NONE',  ( 5.263131812197999970, -77.99776011999799152, -9.905430536777000583 ) ) ;
#57032 = CARTESIAN_POINT ( 'NONE',  ( 0.2613587267741000475, -79.49674366942500114, -10.97249781033000104 ) ) ;
#57033 = CARTESIAN_POINT ( 'NONE',  ( 10.52693147740000157, -23.42153431750000436, -7.606024891108000396 ) ) ;
#57034 = CARTESIAN_POINT ( 'NONE',  ( 0.8898229089127220881, -16.97675468816218114, 12.70296869045103527 ) ) ;
#57035 = CARTESIAN_POINT ( 'NONE',  ( 4.613038445363000228, -76.78576930215800189, 11.49595188101000076 ) ) ;
#57036 = CARTESIAN_POINT ( 'NONE',  ( 0.000000000000000000, -3.500000000000000000, 0.000000000000000000 ) ) ;
#57037 = LINE ( 'NONE', #3022, #39030 ) ;
#57038 = ORIENTED_EDGE ( 'NONE', *, *, #34529, .F. ) ;
#57039 = CARTESIAN_POINT ( 'NONE',  ( 5.650974246042000715, -78.47334026635199677, 9.474609463724998903 ) ) ;
#57040 = CARTESIAN_POINT ( 'NONE',  ( -1.025450104155645858, -80.05165854934456604, 0.7168883596936641567 ) ) ;
#57041 = CARTESIAN_POINT ( 'NONE',  ( 12.89999999994999769, -2.999999999951000085, 1.886268220167000189E-09 ) ) ;
#57042 = EDGE_CURVE ( 'NONE', #15888, #8754, #37749, .T. ) ;
#57043 = CARTESIAN_POINT ( 'NONE',  ( 0.1325202778310999863, -79.05325033209098251, 11.26549478459000042 ) ) ;
#57044 = DIRECTION ( 'NONE',  ( 4.275554269583999736E-12, 1.000000000000000000, -1.682668868129999999E-10 ) ) ;
#57045 = FACE_OUTER_BOUND ( 'NONE', #4276, .T. ) ;
#57046 = CARTESIAN_POINT ( 'NONE',  ( 0.6297746568761206643, -78.93358075575952171, 1.092604805766054010 ) ) ;
#57047 = CARTESIAN_POINT ( 'NONE',  ( -0.2222643924572317575, -81.96268533019295432, -1.494766702788131507 ) ) ;
#57048 = CARTESIAN_POINT ( 'NONE',  ( 0.04273675807453811148, -79.72806120046924150, -1.249183804664953268 ) ) ;
#57049 = CARTESIAN_POINT ( 'NONE',  ( 2.299999999999999822, -77.50000000000000000, 0.000000000000000000 ) ) ;
#57050 = DIRECTION ( 'NONE',  ( -1.000000000000000000, 0.000000000000000000, 0.000000000000000000 ) ) ;
#57051 = CONICAL_SURFACE ( 'NONE', #44786, 13.94999999994999840, 0.7853981633972997312 ) ;
#57052 = LINE ( 'NONE', #12459, #9194 ) ;
#57053 = ORIENTED_EDGE ( 'NONE', *, *, #47840, .T. ) ;
#57054 = ORIENTED_EDGE ( 'NONE', *, *, #6153, .T. ) ;
#57055 = CARTESIAN_POINT ( 'NONE',  ( -12.43569863936000175, -53.91799904124000165, -0.4278707626187999713 ) ) ;
#57056 = AXIS2_PLACEMENT_3D ( 'NONE', #46411, #19237, #23656 ) ;
#57057 = ORIENTED_EDGE ( 'NONE', *, *, #51038, .T. ) ;
#57058 = B_SPLINE_CURVE_WITH_KNOTS ( 'NONE', 3,
 ( #42854, #15981, #33971, #18014, #30975, #53434, #49013, #35709, #40143, #36006, #3843, #8559, #31562, #31265, #48442, #49308, #13273, #26550, #3557, #44579, #49611, #16850, #3277, #58155 ),
 .UNSPECIFIED., .F., .F.,
 ( 4, 2, 2, 2, 2, 2, 2, 2, 2, 2, 2, 4 ),
 ( 0.000000000000000000, 0.1249999999999984457, 0.2499999999999968914, 0.3749999999999953371, 0.4374999999999954481, 0.4999999999999955591, 0.6249999999999957812, 0.7499999999999960032, 0.8124999999999968914, 0.8437499999999971134, 0.8749999999999974465, 1.000000000000000000 ),
 .UNSPECIFIED. ) ;
#57059 = ORIENTED_EDGE ( 'NONE', *, *, #46369, .T. ) ;
#57060 = CARTESIAN_POINT ( 'NONE',  ( 0.9218200799623694763, -81.82291666667074992, 1.199500263597272465 ) ) ;
#57061 = CARTESIAN_POINT ( 'NONE',  ( 9.605397716210999803, -76.78400324167699864, -5.187648860687999353 ) ) ;
#57062 = AXIS2_PLACEMENT_3D ( 'NONE', #53367, #8494, #7919 ) ;
#57063 = CARTESIAN_POINT ( 'NONE',  ( 6.797895215277000247, -78.44203667140099867, -7.211733462747999646 ) ) ;
#57064 = CIRCLE ( 'NONE', #32512, 12.69999999999999929 ) ;
#57065 = CARTESIAN_POINT ( 'NONE',  ( -8.382198119002001846, -79.75615640372498660, -7.453647783897999979 ) ) ;
#57066 = ORIENTED_EDGE ( 'NONE', *, *, #17692, .F. ) ;
#57067 = ORIENTED_EDGE ( 'NONE', *, *, #51935, .F. ) ;
#57068 = CARTESIAN_POINT ( 'NONE',  ( -2.588076551402957115, -77.49760603155162642, 8.885074677331601833 ) ) ;
#57069 = CARTESIAN_POINT ( 'NONE',  ( -1.776188306762000124, -77.42168691014599347, -10.89629776253999971 ) ) ;
#57070 = EDGE_CURVE ( 'NONE', #38980, #33666, #51886, .T. ) ;
#57071 = CARTESIAN_POINT ( 'NONE',  ( -12.54673765600000124, -61.62199238204999574, -0.9174244429635999287 ) ) ;
#57072 = CARTESIAN_POINT ( 'NONE',  ( -8.771427373352999268, -77.86532743984299998, -4.151237309591000013 ) ) ;
#57073 = DIRECTION ( 'NONE',  ( 0.000000000000000000, 0.000000000000000000, -1.000000000000000000 ) ) ;
#57074 = CARTESIAN_POINT ( 'NONE',  ( 10.47020627418439531, -76.72916666666667140, -2.813789756862242974 ) ) ;
#57075 = CARTESIAN_POINT ( 'NONE',  ( 1.791008777272000030, -80.23213113446799127, 11.11143388882000060 ) ) ;
#57076 = CARTESIAN_POINT ( 'NONE',  ( -0.4334656432294999862, -80.16545669043000544, 1.646792182271999971 ) ) ;
#57077 = CARTESIAN_POINT ( 'NONE',  ( -1.249999999999999778, -81.01041666666665719, -0.1636246173744686228 ) ) ;
#57078 = ORIENTED_EDGE ( 'NONE', *, *, #38361, .F. ) ;
#57079 = CARTESIAN_POINT ( 'NONE',  ( -8.351691841945999784, -76.51493262182999899, 7.546656452382999980 ) ) ;
#57080 = LINE ( 'NONE', #16067, #55054 ) ;
#57081 = CARTESIAN_POINT ( 'NONE',  ( -7.762982794245000484, -17.83910040287999621, -9.991998894192999359 ) ) ;
#57083 = DIRECTION ( 'NONE',  ( 1.000000000000000000, 0.000000000000000000, 0.000000000000000000 ) ) ;
#57082 = CARTESIAN_POINT ( 'NONE',  ( 7.668949790007999923, -56.02870851050000311, 10.21381326472999795 ) ) ;
#57084 = LINE ( 'NONE', #7207, #54377 ) ;
#57085 = CARTESIAN_POINT ( 'NONE',  ( -5.099062320646999602, -80.14465347566299158, -10.07485988244000019 ) ) ;
#57086 = CARTESIAN_POINT ( 'NONE',  ( -5.883052656872999719, -77.74214815972399606, 9.603314844095001135 ) ) ;
#57087 = CARTESIAN_POINT ( 'NONE',  ( -8.599842724110780878, -79.63167486684267260, -3.562057441230364052 ) ) ;
#57088 = CARTESIAN_POINT ( 'NONE',  ( 4.382699061554999886, -81.04870889205099616, -10.08957852304999925 ) ) ;
#57089 = ORIENTED_EDGE ( 'NONE', *, *, #44844, .F. ) ;
#57090 = CARTESIAN_POINT ( 'NONE',  ( -1.250000000000000000, -76.29999999999999716, 0.000000000000000000 ) ) ;
#57091 = CARTESIAN_POINT ( 'NONE',  ( 0.000000000000000000, -87.70000000000000284, 0.000000000000000000 ) ) ;
#57092 = CARTESIAN_POINT ( 'NONE',  ( -12.71798269385000069, -18.70221245812999911, 1.931086388578000079 ) ) ;
#57093 = CARTESIAN_POINT ( 'NONE',  ( -3.554538774556999847, -2.649302049814999727, -0.8106109833587000768 ) ) ;
#57094 = B_SPLINE_CURVE_WITH_KNOTS ( 'NONE', 3,
 ( #23995, #19874, #55292, #14841, #33432, #15138, #32254, #51175, #24297, #10429, #5409, #5987, #51469, #42012, #42311, #18995, #5128, #14257 ),
 .UNSPECIFIED., .F., .F.,
 ( 4, 2, 2, 2, 2, 2, 2, 2, 4 ),
 ( 0.000000000000000000, 0.1250000000000000000, 0.2500000000000000000, 0.3750000000000000000, 0.5000000000000000000, 0.6250000000000000000, 0.7500000000000000000, 0.8750000000000000000, 1.000000000000000000 ),
 .UNSPECIFIED. ) ;
#57095 = EDGE_CURVE ( 'NONE', #26282, #8334, #47700, .T. ) ;
#57096 = CARTESIAN_POINT ( 'NONE',  ( 3.771615891982000424, -80.17905589940099276, -8.483472276358000386 ) ) ;
#57097 = CARTESIAN_POINT ( 'NONE',  ( -12.78037507859000144, -54.50670131396999807, 1.812742845509000000 ) ) ;
#57098 = CARTESIAN_POINT ( 'NONE',  ( -7.342331066867000544, -55.64999999967000122, 8.190859204290999784 ) ) ;
#57099 = CARTESIAN_POINT ( 'NONE',  ( 1.801750019961000149, -60.19007426689000084, 12.59656967656000148 ) ) ;
#57100 = CARTESIAN_POINT ( 'NONE',  ( -7.954951288349001004, -55.54999999966999980, -9.722718241315000398 ) ) ;
#57101 = CARTESIAN_POINT ( 'NONE',  ( -2.935661446561999899, -76.94999999999998863, -9.035036904803998681 ) ) ;
#57102 = FACE_OUTER_BOUND ( 'NONE', #20976, .T. ) ;
#57103 = CARTESIAN_POINT ( 'NONE',  ( 3.875771953607000331, -77.65343742103499380, 10.35502414757000089 ) ) ;
#57104 = B_SPLINE_CURVE_WITH_KNOTS ( 'NONE', 3,
 ( #56945, #12356, #30920, #11790 ),
 .UNSPECIFIED., .F., .F.,
 ( 4, 4 ),
 ( 0.000000000000000000, 1.000000000000000000 ),
 .UNSPECIFIED. ) ;
#57105 = EDGE_CURVE ( 'NONE', #4102, #52807, #58250, .T. ) ;
#57106 = CARTESIAN_POINT ( 'NONE',  ( 10.39516313037050743, -76.41088147063496194, -5.479998801784073947 ) ) ;
#57107 = CARTESIAN_POINT ( 'NONE',  ( -0.8117802668354000550, -77.26027545111699624, -11.00194288205000070 ) ) ;
#57108 = CARTESIAN_POINT ( 'NONE',  ( 0.2234679122977781540, -81.96125120072602499, 1.229696476816594108 ) ) ;
#57109 = ADVANCED_FACE ( 'NONE', ( #34656 ), #15831, .F. ) ;
#57110 = CARTESIAN_POINT ( 'NONE',  ( 2.309272084855999996, -76.85373069405538615, -9.392260232199999948 ) ) ;
#57111 = CARTESIAN_POINT ( 'NONE',  ( 8.082524092276894834, -78.29166666666665719, 4.658475568430803904 ) ) ;
#57112 = CARTESIAN_POINT ( 'NONE',  ( -1.636761686205420396, -2.583333333333333037, -2.839805762151339508 ) ) ;
#57113 = CARTESIAN_POINT ( 'NONE',  ( -4.051423106035414001, -80.19464027527671135, -9.957102339836081839 ) ) ;
#57114 = FACE_OUTER_BOUND ( 'NONE', #3409, .T. ) ;
#57115 = CARTESIAN_POINT ( 'NONE',  ( 11.02509224276342259, -75.79999999999999716, 4.905407213634159547 ) ) ;
#57116 = CARTESIAN_POINT ( 'NONE',  ( 7.520016693046000178, -79.67705620421800461, -9.389162645085001202 ) ) ;
#57117 = CARTESIAN_POINT ( 'NONE',  ( 0.000000000000000000, -0.2000000000000000111, -10.20000000000000107 ) ) ;
#57118 = CARTESIAN_POINT ( 'NONE',  ( -5.416162833245999231, -79.90848498002219458, -9.874165520190000933 ) ) ;
#57119 = CARTESIAN_POINT ( 'NONE',  ( 10.47007982758580447, -77.37089620502051446, 2.813809139533428372 ) ) ;
#57120 = VERTEX_POINT ( 'NONE', #41721 ) ;
#57121 = CARTESIAN_POINT ( 'NONE',  ( -1.430139897903401236, -0.7500000000000001110, 3.215437163636295725 ) ) ;
#57122 = ORIENTED_EDGE ( 'NONE', *, *, #52048, .F. ) ;
#57123 = VERTEX_POINT ( 'NONE', #1299 ) ;
#57124 = DIRECTION ( 'NONE',  ( 0.000000000000000000, -1.000000000000000000, 0.000000000000000000 ) ) ;
#57125 = EDGE_CURVE ( 'NONE', #40036, #27720, #47216, .T. ) ;
#57126 = ORIENTED_EDGE ( 'NONE', *, *, #9956, .F. ) ;
#57127 = B_SPLINE_CURVE_WITH_KNOTS ( 'NONE', 3,
 ( #52889, #57313, #44607, #12721, #30714, #25726, #30141, #17155, #48465, #30433, #39590, #4161, #53171, #16877, #34857, #22160, #57595, #40167 ),
 .UNSPECIFIED., .F., .F.,
 ( 4, 2, 2, 2, 2, 2, 2, 2, 4 ),
 ( 0.000000000000000000, 0.1249999999999999722, 0.2500000000000000000, 0.3750000000000000000, 0.5000000000000001110, 0.6250000000000001110, 0.7500000000000000000, 0.8750000000000000000, 1.000000000000000000 ),
 .UNSPECIFIED. ) ;
#57128 = CARTESIAN_POINT ( 'NONE',  ( -1.193759951361000216, -82.04949591394598940, -3.337651942004999484 ) ) ;
#57129 = CARTESIAN_POINT ( 'NONE',  ( -6.642891787447657848, -79.33646197186951099, 6.791764226237924973 ) ) ;
#57130 = VECTOR ( 'NONE', #14105, 1000.000000000000000 ) ;
#57131 = EDGE_LOOP ( 'NONE', ( #33078, #45274, #12137, #15940 ) ) ;
#57132 = CARTESIAN_POINT ( 'NONE',  ( -9.003055988996001346, -78.97756055792000041, -8.248189893095000613 ) ) ;
#57133 = ORIENTED_EDGE ( 'NONE', *, *, #21768, .F. ) ;
#57134 = CARTESIAN_POINT ( 'NONE',  ( 9.250000000000000000, -79.74999999999998579, 1.907449677260999760E-14 ) ) ;
#57135 = ORIENTED_EDGE ( 'NONE', *, *, #26142, .T. ) ;
#57136 = CARTESIAN_POINT ( 'NONE',  ( 0.000000000000000000, -23.15000000000000213, 12.00000000000000000 ) ) ;
#57137 = CARTESIAN_POINT ( 'NONE',  ( -10.98961866300655466, -18.48267221963240914, 0.4810437121599021593 ) ) ;
#57138 = AXIS2_PLACEMENT_3D ( 'NONE', #39217, #2926, #4071 ) ;
#57139 = EDGE_CURVE ( 'NONE', #353, #54955, #49077, .T. ) ;
#57140 = CARTESIAN_POINT ( 'NONE',  ( -10.24633426275284265, -80.07555679980247021, 3.252597035816566784 ) ) ;
#57141 = CARTESIAN_POINT ( 'NONE',  ( -8.838834764832000701, -23.25000000000000000, 8.838834764832000701 ) ) ;
#57142 = CARTESIAN_POINT ( 'NONE',  ( -1.427561782742997831, -86.25171435493597016, -3.126711714967702171 ) ) ;
#57143 = CARTESIAN_POINT ( 'NONE',  ( 10.12567350656000009, -76.11878700336998804, 4.748118780173999909 ) ) ;
#57144 = CARTESIAN_POINT ( 'NONE',  ( -5.947256583267294339, -79.07291666668990615, 10.29299386049553711 ) ) ;
#57145 = EDGE_CURVE ( 'NONE', #28272, #40983, #22265, .T. ) ;
#57146 = CARTESIAN_POINT ( 'NONE',  ( -8.796335266380014062, -78.64791666666667425, 6.760013919724027431 ) ) ;
#57147 = CARTESIAN_POINT ( 'NONE',  ( 10.88552170588999957, -76.72031315673200424, 1.577109214857000064 ) ) ;
#57148 = FACE_OUTER_BOUND ( 'NONE', #15816, .T. ) ;
#57149 = CARTESIAN_POINT ( 'NONE',  ( -0.6211595220380999871, -80.71795433454799706, -1.084739991049000096 ) ) ;
#57150 = CARTESIAN_POINT ( 'NONE',  ( 8.190859204290999784, -59.94999999967000548, 7.342331066867000544 ) ) ;
#57151 = CARTESIAN_POINT ( 'NONE',  ( 2.275600661772546829, -2.913783080248345314, 2.319952847705075705 ) ) ;
#57152 = CARTESIAN_POINT ( 'NONE',  ( 1.377051302669000110, -80.61375264934798679, -3.266296602878999700 ) ) ;
#57153 = CARTESIAN_POINT ( 'NONE',  ( 1.153116094663966251, -82.88157216681773320, 0.4824474276636376846 ) ) ;
#57154 = CARTESIAN_POINT ( 'NONE',  ( 1.096098671195999907, -84.23744503318798138, 3.373444835455999602 ) ) ;
#57155 = CARTESIAN_POINT ( 'NONE',  ( 3.665025684363000025, -3.510954567059000109, -1.025097465345000236 ) ) ;
#57156 = CARTESIAN_POINT ( 'NONE',  ( 10.35747158362999976, -23.31584477285000290, 7.626500902217000721 ) ) ;
#57157 = CARTESIAN_POINT ( 'NONE',  ( -7.631889049370999878, -60.02121504819000108, -10.36222434951000082 ) ) ;
#57158 = DIRECTION ( 'NONE',  ( 0.000000000000000000, 0.000000000000000000, -1.000000000000000000 ) ) ;
#57159 = CARTESIAN_POINT ( 'NONE',  ( -0.05395919428434999693, -80.84366592615199920, -1.332567581519000122 ) ) ;
#57160 = CARTESIAN_POINT ( 'NONE',  ( -9.500000000000000000, -78.89999999999999147, 0.000000000000000000 ) ) ;
#57161 = CARTESIAN_POINT ( 'NONE',  ( 12.49997170191999984, -23.19201514549000009, 1.666513530428999967 ) ) ;
#57162 = CARTESIAN_POINT ( 'NONE',  ( 1.684372618195999927, -78.17228479878399128, 10.84559388857000073 ) ) ;
#57163 = LINE ( 'NONE', #25003, #40459 ) ;
#57164 = CARTESIAN_POINT ( 'NONE',  ( 11.59740219448999987, -75.80332143684999835, -4.280683990382000204 ) ) ;
#57165 = ORIENTED_EDGE ( 'NONE', *, *, #34683, .F. ) ;
#57166 = CARTESIAN_POINT ( 'NONE',  ( 10.86112223246497344, -80.98224957254201684, -2.453532618892452444 ) ) ;
#57167 = CARTESIAN_POINT ( 'NONE',  ( 7.745630616141999880, -80.09064385942969011, 8.037401158237999610 ) ) ;
#57168 = EDGE_CURVE ( 'NONE', #12394, #5899, #17011, .T. ) ;
#57169 =( REPRESENTATION_RELATIONSHIP ('NONE','NONE', #58051, #33899 ) REPRESENTATION_RELATIONSHIP_WITH_TRANSFORMATION ( #25469 )SHAPE_REPRESENTATION_RELATIONSHIP( ) );
#57170 = CARTESIAN_POINT ( 'NONE',  ( 12.79972228485999963, -60.59021513420999838, 2.019125729023000027 ) ) ;
#57171 = CARTESIAN_POINT ( 'NONE',  ( 9.787591575112999820, -79.28015235882000411, -7.311436768013999554 ) ) ;
#57172 = CARTESIAN_POINT ( 'NONE',  ( 0.000000000000000000, -75.20000000000000284, 0.000000000000000000 ) ) ;
#57173 = CARTESIAN_POINT ( 'NONE',  ( 4.108390852610000366, -78.61743808823698032, -8.590197950816000017 ) ) ;
#57174 = ADVANCED_FACE ( 'NONE', ( #25738 ), #18912, .T. ) ;
#57175 = CARTESIAN_POINT ( 'NONE',  ( 4.043590400160999465, -84.02206052499799682, 1.029295458530999907 ) ) ;
#57176 = CARTESIAN_POINT ( 'NONE',  ( -12.60354432325999952, -19.24899162885999715, 1.750000000000000000 ) ) ;
#57177 = DIRECTION ( 'NONE',  ( 0.7071067811865474617, 0.000000000000000000, -0.7071067811865474617 ) ) ;
#57178 = VERTEX_POINT ( 'NONE', #6870 ) ;
#57179 = VECTOR ( 'NONE', #25444, 1000.000000000000000 ) ;
#57180 = DIRECTION ( 'NONE',  ( 0.9999999999998321343, 0.000000000000000000, 5.794542749929189768E-07 ) ) ;
#57181 = CARTESIAN_POINT ( 'NONE',  ( -1.439896632895337980, -78.81458333333334565, -11.00000000000000178 ) ) ;
#57182 = CARTESIAN_POINT ( 'NONE',  ( -3.485499217011999828, -78.91452042059380290, -1.462502484024984119E-14 ) ) ;
#57183 = CIRCLE ( 'NONE', #31713, 13.79999999999999893 ) ;
#57184 = ORIENTED_EDGE ( 'NONE', *, *, #25470, .F. ) ;
#57185 = VECTOR ( 'NONE', #49015, 1000.000000000000000 ) ;
#57186 = CARTESIAN_POINT ( 'NONE',  ( -8.171144579308439404, -55.45989902438520858, -7.364280830341621176 ) ) ;
#57187 = CARTESIAN_POINT ( 'NONE',  ( 8.665370346175000904, -80.06605154712399042, -7.125084804452000320 ) ) ;
#57188 = AXIS2_PLACEMENT_3D ( 'NONE', #32598, #1637, #50352 ) ;
#57189 = ORIENTED_EDGE ( 'NONE', *, *, #20043, .F. ) ;
#57190 = AXIS2_PLACEMENT_3D ( 'NONE', #31771, #42110, #27924 ) ;
#57191 = ORIENTED_EDGE ( 'NONE', *, *, #29906, .T. ) ;
#57192 = VERTEX_POINT ( 'NONE', #40108 ) ;
#57193 = EDGE_CURVE ( 'NONE', #38464, #24242, #53704, .T. ) ;
#57194 = CARTESIAN_POINT ( 'NONE',  ( -1.886823409076000102, -18.23680315638000238, 12.68610076205999881 ) ) ;
#57195 = CARTESIAN_POINT ( 'NONE',  ( 1.532229595823858759, -60.92298962908745352, 12.51228690890383177 ) ) ;
#57196 = CARTESIAN_POINT ( 'NONE',  ( 8.249323304235000265, -80.45505077665451665, -5.229696851825000437 ) ) ;
#57197 = ORIENTED_EDGE ( 'NONE', *, *, #45373, .F. ) ;
#57198 = CARTESIAN_POINT ( 'NONE',  ( -3.247771509845949200, -2.590611485816939119, 0.4256070685482727933 ) ) ;
#57199 = EDGE_LOOP ( 'NONE', ( #26383, #20364, #23547, #48927 ) ) ;
#57200 = CARTESIAN_POINT ( 'NONE',  ( -1.307210027570999911, -79.16650217667631750, -12.19386267984000050 ) ) ;
#57201 = CARTESIAN_POINT ( 'NONE',  ( 3.621447497675000182, -78.99318692614357929, -1.355252715606880543E-15 ) ) ;
#57202 = CARTESIAN_POINT ( 'NONE',  ( 7.961057357800999768, -54.26431744618999886, 9.783210913615000948 ) ) ;
#57203 = CARTESIAN_POINT ( 'NONE',  ( 1.460959015002472494, -81.17083333333333428, 0.3926218265389232465 ) ) ;
#57204 = PLANE ( 'NONE',  #27706 ) ;
#57205 = ADVANCED_FACE ( 'NONE', ( #3030 ), #43473, .F. ) ;
#57206 = CARTESIAN_POINT ( 'NONE',  ( 12.76303204298000082, -60.06485150663000638, -1.980584515756000030 ) ) ;
#57207 = CARTESIAN_POINT ( 'NONE',  ( -0.7928179559538000021, -78.76973013078654162, -11.95355612867000339 ) ) ;
#57208 = CARTESIAN_POINT ( 'NONE',  ( 9.369164850722000892, -60.04999999966999980, -7.601397897754999633 ) ) ;
#57209 = CARTESIAN_POINT ( 'NONE',  ( -7.758897894424999997, -24.30081253449000300, 10.31443085083000000 ) ) ;
#57210 = AXIS2_PLACEMENT_3D ( 'NONE', #41886, #9720, #41302 ) ;
#57211 = CARTESIAN_POINT ( 'NONE',  ( 3.494616459463999902, -79.60055496681158616, 2.279850439600000112 ) ) ;
#57212 = CARTESIAN_POINT ( 'NONE',  ( -9.250000000000007105, -77.98958333333334281, 1.210822168571027868 ) ) ;
#57213 = CARTESIAN_POINT ( 'NONE',  ( -12.66232176275999954, -16.86513311418999805, 0.5079086068997000769 ) ) ;
#57214 = DIRECTION ( 'NONE',  ( 0.000000000000000000, 1.000000000000000000, 0.000000000000000000 ) ) ;
#57215 = CARTESIAN_POINT ( 'NONE',  ( 0.000000000000000000, -82.50000000000000000, 0.000000000000000000 ) ) ;
#57216 = CARTESIAN_POINT ( 'NONE',  ( -0.5875803945788578009, -81.33860554734724246, -1.187789484363859893 ) ) ;
#57217 = VECTOR ( 'NONE', #13793, 1000.000000000000000 ) ;
#57218 = CARTESIAN_POINT ( 'NONE',  ( -3.712316210013999918, -1.805555703421999780, -0.5582186464255000091 ) ) ;
#57219 = CARTESIAN_POINT ( 'NONE',  ( -6.043427764450786555, -77.88333333333332575, -10.48543666025110177 ) ) ;
#57220 = ADVANCED_FACE ( 'NONE', ( #12171 ), #29013, .F. ) ;
#57221 = AXIS2_PLACEMENT_3D ( 'NONE', #56926, #35326, #48086 ) ;
#57222 = CARTESIAN_POINT ( 'NONE',  ( 0.9056516610957285884, -81.07384114603890168, 1.208906470985191106 ) ) ;
#57223 = CARTESIAN_POINT ( 'NONE',  ( 7.618592589353999855, -77.25777915476199098, 5.659247346374999488 ) ) ;
#57224 = CARTESIAN_POINT ( 'NONE',  ( -1.393431170853000056, -79.36590538786700222, 0.8158852592188999830 ) ) ;
#57225 = CIRCLE ( 'NONE', #50684, 11.70000000000000107 ) ;
#57226 = CARTESIAN_POINT ( 'NONE',  ( 3.113304451009999863, -78.49783470746899638, -10.55022916317000181 ) ) ;
#57227 = CARTESIAN_POINT ( 'NONE',  ( 3.385164732404000176, -2.693653522605000017, -1.094590136342000086 ) ) ;
#57228 = CARTESIAN_POINT ( 'NONE',  ( 3.002529760384999857, -78.79598695555699805, 11.62679918156999825 ) ) ;
#57229 = CARTESIAN_POINT ( 'NONE',  ( 12.90000000000000036, -3.000000000000000000, 0.000000000000000000 ) ) ;
#57231 = CARTESIAN_POINT ( 'NONE',  ( -7.639893379697016762, -18.61284423925064146, 10.11462454831194435 ) ) ;
#57230 = CARTESIAN_POINT ( 'NONE',  ( -11.79999999999999893, -23.15000000000999947, -0.5999999999999999778 ) ) ;
#57232 = CARTESIAN_POINT ( 'NONE',  ( -1.183213148269000259, -81.53991179838999415, 0.6526699808710000328 ) ) ;
#57233 = CARTESIAN_POINT ( 'NONE',  ( -5.896991955202756763, -79.52120778372643883, 8.992014754021855794 ) ) ;
#57234 = ORIENTED_EDGE ( 'NONE', *, *, #31045, .T. ) ;
#57235 = CARTESIAN_POINT ( 'NONE',  ( -9.797890753601748770, -78.85056356931703192, 7.009672782845664862 ) ) ;
#57236 = B_SPLINE_CURVE_WITH_KNOTS ( 'NONE', 3,
 ( #33648, #42814, #6500, #43384, #47262, #46973 ),
 .UNSPECIFIED., .F., .F.,
 ( 4, 2, 4 ),
 ( 0.000000000000000000, 0.5000000000000000000, 1.000000000000000000 ),
 .UNSPECIFIED. ) ;
#57237 = CARTESIAN_POINT ( 'NONE',  ( 4.220196950471000186, -79.60564988871099956, 11.40022119696999958 ) ) ;
#57238 = CARTESIAN_POINT ( 'NONE',  ( 4.680902262334169173, -79.08410081236472422, 8.289971767921159085 ) ) ;
#57239 = CARTESIAN_POINT ( 'NONE',  ( -3.924507919822526780, -80.00000000000002842, -8.550991966546336087 ) ) ;
#57240 = CARTESIAN_POINT ( 'NONE',  ( -8.260136572142998901, -61.74034376533999335, 9.643347111204001010 ) ) ;
#57241 = CARTESIAN_POINT ( 'NONE',  ( 3.687443820737999811, -0.8745872626717998699, -0.3192645131365000055 ) ) ;
#57242 = CARTESIAN_POINT ( 'NONE',  ( -6.990927307832999205, -79.70827722813399419, 6.997322775002999151 ) ) ;
#57243 = CARTESIAN_POINT ( 'NONE',  ( 11.68767212001979239, -78.12916666666666288, -3.140974612311342451 ) ) ;
#57244 = CARTESIAN_POINT ( 'NONE',  ( -0.3862712429687000237, -78.00000000000000000, 1.188820645369000006 ) ) ;
#57245 = ORIENTED_EDGE ( 'NONE', *, *, #44633, .T. ) ;
#57246 = DIRECTION ( 'NONE',  ( 0.000000000000000000, 1.000000000000000000, 0.000000000000000000 ) ) ;
#57247 = CARTESIAN_POINT ( 'NONE',  ( 11.00000000000000000, -81.00000000000000000, -2.369510767747999942E-13 ) ) ;
#57248 = DIRECTION ( 'NONE',  ( 0.000000000000000000, -1.000000000000000000, 0.000000000000000000 ) ) ;
#57249 = CARTESIAN_POINT ( 'NONE',  ( -1.310679582531386389, -78.44166666666667709, -0.7554284705563492075 ) ) ;
#57250 = CARTESIAN_POINT ( 'NONE',  ( 0.5818457612699999837, -80.98300040053000259, -1.560998038830999857 ) ) ;
#57251 = ORIENTED_EDGE ( 'NONE', *, *, #27168, .T. ) ;
#57252 = CARTESIAN_POINT ( 'NONE',  ( 9.067898462393999992, -77.63025123080397805, -6.404597993423999824 ) ) ;
#57253 = CARTESIAN_POINT ( 'NONE',  ( -0.04193593714361701363, -53.78990258635174371, -12.50649570002511979 ) ) ;
#57254 = CARTESIAN_POINT ( 'NONE',  ( -1.667936688463999895, -22.76486430425999785, 12.53239398059000109 ) ) ;
#57255 = CONICAL_SURFACE ( 'NONE', #12949, 5.249999999862000166, 0.7853981633972997312 ) ;
#57256 = EDGE_CURVE ( 'NONE', #54593, #48994, #32820, .T. ) ;
#57257 = CARTESIAN_POINT ( 'NONE',  ( -12.53239398060000021, -56.03513569577999931, 1.667936688463999895 ) ) ;
#57258 = CARTESIAN_POINT ( 'NONE',  ( 8.596576764504078483, -78.40209458680075727, 6.606494579572424364 ) ) ;
#57259 = CARTESIAN_POINT ( 'NONE',  ( 12.72966282068020227, -55.03110224949036677, -1.931329623869370238 ) ) ;
#57260 = ORIENTED_EDGE ( 'NONE', *, *, #1000, .T. ) ;
#57261 = AXIS2_PLACEMENT_3D ( 'NONE', #48775, #44926, #39897 ) ;
#57262 = ORIENTED_EDGE ( 'NONE', *, *, #10109, .T. ) ;
#57263 = CARTESIAN_POINT ( 'NONE',  ( 3.138727503548000008, -77.40410827300999586, -12.06897532934999973 ) ) ;
#57264 = CARTESIAN_POINT ( 'NONE',  ( 5.072952311206533338, -78.76416732819434685, -9.477694199498785110 ) ) ;
#57265 = CARTESIAN_POINT ( 'NONE',  ( 0.6885956969122000171, -77.97809706267000252, 1.243482171564999961 ) ) ;
#57266 = CIRCLE ( 'NONE', #33715, 1.000000000000000000 ) ;
#57267 = ORIENTED_EDGE ( 'NONE', *, *, #12027, .F. ) ;
#57268 = CARTESIAN_POINT ( 'NONE',  ( -4.802567994450000377, -77.27295584965399655, -8.191018798270000900 ) ) ;
#57269 = CARTESIAN_POINT ( 'NONE',  ( -12.56594317982999875, -55.55000000504000468, 1.750000000000000000 ) ) ;
#57270 = AXIS2_PLACEMENT_3D ( 'NONE', #30654, #35368, #25945 ) ;
#57271 = CARTESIAN_POINT ( 'NONE',  ( 9.396085398178630754, -75.99791666666666856, -7.220923959705230821 ) ) ;
#57272 = CARTESIAN_POINT ( 'NONE',  ( -12.60796396291999955, -78.26141106207001030, -0.9189346901731000328 ) ) ;
#57273 = CARTESIAN_POINT ( 'NONE',  ( -5.859445663532000026, -77.66873914051188876, 9.564779511708000115 ) ) ;
#57275 = ADVANCED_FACE ( 'NONE', ( #2455 ), #31139, .F. ) ;
#57274 = CYLINDRICAL_SURFACE ( 'NONE', #53210, 1.750000000000001332 ) ;
#57276 = FACE_OUTER_BOUND ( 'NONE', #52908, .T. ) ;
#57277 = DIRECTION ( 'NONE',  ( 0.000000000000000000, -1.000000000000000000, 0.000000000000000000 ) ) ;
#57278 = DIRECTION ( 'NONE',  ( 1.776356839400000238E-14, 1.000000000000000000, 2.516505522483999811E-14 ) ) ;
#57279 = VERTEX_POINT ( 'NONE', #25165 ) ;
#57280 = CARTESIAN_POINT ( 'NONE',  ( -8.272053489104999713, -78.68019927879299757, -7.648664291178000063 ) ) ;
#57281 = CARTESIAN_POINT ( 'NONE',  ( 7.645574991865955461, -77.30253601357824778, -5.206776502330282774 ) ) ;
#57282 = CARTESIAN_POINT ( 'NONE',  ( -1.294028136707999987, -80.72633258256199440, 0.2571518259264999884 ) ) ;
#57283 = CARTESIAN_POINT ( 'NONE',  ( 0.000000000000000000, -75.67500000000001137, 0.000000000000000000 ) ) ;
#57284 = CARTESIAN_POINT ( 'NONE',  ( -0.6983046762106999150, -78.01866860913609969, 1.233867887851000100 ) ) ;
#57285 = CARTESIAN_POINT ( 'NONE',  ( -7.678657038162065795, -60.59377623463994667, -10.03844138482057247 ) ) ;
#57286 = CARTESIAN_POINT ( 'NONE',  ( 12.60552511010000032, -23.28917723430000208, 1.799501877793999949 ) ) ;
#57287 = CARTESIAN_POINT ( 'NONE',  ( -9.250000000000000000, -77.59999999999999432, 0.000000000000000000 ) ) ;
#57288 = EDGE_CURVE ( 'NONE', #12596, #15875, #43189, .T. ) ;
#57289 = DIRECTION ( 'NONE',  ( -1.000000000000000000, 0.000000000000000000, 0.000000000000000000 ) ) ;
#57290 = CARTESIAN_POINT ( 'NONE',  ( -1.222545847381571127, -79.11929213067102751, -0.2981043881531356132 ) ) ;
#57291 = CARTESIAN_POINT ( 'NONE',  ( -10.97221500190000043, -79.57146358532099839, -2.025363574538999956 ) ) ;
#57292 = CARTESIAN_POINT ( 'NONE',  ( 4.290841056834999279, -77.78051332859898537, 8.395152818089000490 ) ) ;
#57293 = DIRECTION ( 'NONE',  ( -1.000000000000000000, 0.000000000000000000, 0.000000000000000000 ) ) ;
#57294 = CARTESIAN_POINT ( 'NONE',  ( -9.393203674808267678, -79.54166666666665719, -5.413904038987171319 ) ) ;
#57295 = CARTESIAN_POINT ( 'NONE',  ( -3.740947899408999966, -80.29067215926599488, -1.847123254877999887 ) ) ;
#57296 = ADVANCED_FACE ( 'NONE', ( #16320 ), #56373, .F. ) ;
#57297 = DIRECTION ( 'NONE',  ( -0.3090169943748909409, 0.000000000000000000, -0.9510565162951718499 ) ) ;
#57298 = VERTEX_POINT ( 'NONE', #45739 ) ;
#57299 = CARTESIAN_POINT ( 'NONE',  ( -4.245633743941748861, -77.20000000000000284, 9.989790920463677892 ) ) ;
#57300 = CARTESIAN_POINT ( 'NONE',  ( -1.359874270581000077, -81.42584665852999137, 0.5545210745837000355 ) ) ;
#57301 = CARTESIAN_POINT ( 'NONE',  ( 10.68063106575048593, -79.33970932340548643, -1.407236774638731980 ) ) ;
#57302 = CARTESIAN_POINT ( 'NONE',  ( -8.148905501844000199, -78.56378829332899727, -8.781309899900000104 ) ) ;
#57303 = CARTESIAN_POINT ( 'NONE',  ( -12.70299804978423097, -16.97411689985228378, 0.8844418155559133909 ) ) ;
#57304 = CARTESIAN_POINT ( 'NONE',  ( 0.8286895765316001361, -81.54474391552000156, 1.445177540541999983 ) ) ;
#57305 = DIRECTION ( 'NONE',  ( 0.000000000000000000, -1.000000000000000000, 0.000000000000000000 ) ) ;
#57306 = CARTESIAN_POINT ( 'NONE',  ( -9.601739433208001273, -79.14265194988499275, -1.533141744029000053 ) ) ;
#57307 = DIRECTION ( 'NONE',  ( 0.000000000000000000, 1.000000000000000000, 0.000000000000000000 ) ) ;
#57308 = LINE ( 'NONE', #6850, #20582 ) ;
#57309 = CARTESIAN_POINT ( 'NONE',  ( 10.60049343523006016, -75.98544560680211646, 5.111788561552529586 ) ) ;
#57310 = CARTESIAN_POINT ( 'NONE',  ( 1.144405438199589842, -81.86389269102102162, -0.5616028373579852184 ) ) ;
#57311 = EDGE_LOOP ( 'NONE', ( #7653, #29161, #50682, #22037, #50748 ) ) ;
#57312 = CARTESIAN_POINT ( 'NONE',  ( -1.624989163556999772E-14, -74.69999999881999031, 0.000000000000000000 ) ) ;
#57313 = CARTESIAN_POINT ( 'NONE',  ( 3.248050210770150326, -2.340893247460261062, -0.4258979702238827048 ) ) ;
#57314 = CARTESIAN_POINT ( 'NONE',  ( 7.803849947780999052, -79.64674332227700404, 9.470181462888000112 ) ) ;
#57315 = VECTOR ( 'NONE', #10367, 1000.000000000000000 ) ;
#57316 = CARTESIAN_POINT ( 'NONE',  ( 3.999999999999885425, -78.69999999999998863, -1.477225460011499791E-15 ) ) ;
#57317 = CARTESIAN_POINT ( 'NONE',  ( -11.21668965365999959, -77.83434206198700167, -0.06311738993059998193 ) ) ;
#57318 = CARTESIAN_POINT ( 'NONE',  ( -2.928603948516999900, -78.76634245677499280, 10.57767911662999971 ) ) ;
#57319 = CARTESIAN_POINT ( 'NONE',  ( -0.8804656547847903303, -16.97196605292977623, 12.70299681151712612 ) ) ;
#57320 = CARTESIAN_POINT ( 'NONE',  ( -10.68812519998999910, -76.89896751707298961, 6.261071428515000648 ) ) ;
#57321 = CARTESIAN_POINT ( 'NONE',  ( -10.86862532138029458, -79.68584017775069128, 1.957230818804138517 ) ) ;
#57322 = CARTESIAN_POINT ( 'NONE',  ( -10.42531125072000009, -55.53514854654000032, -7.624341767124000135 ) ) ;
#57323 = ORIENTED_EDGE ( 'NONE', *, *, #36891, .F. ) ;
#57324 = CARTESIAN_POINT ( 'NONE',  ( 10.36875976864000037, -78.41886758034799243, 3.767035497191999927 ) ) ;
#57325 = CARTESIAN_POINT ( 'NONE',  ( 1.138160268254951646, -79.88425004917058914, 0.5165142851595377893 ) ) ;
#57326 = CIRCLE ( 'NONE', #39413, 9.499999999999996447 ) ;
#57327 = CARTESIAN_POINT ( 'NONE',  ( -8.796335266380014062, -78.14791666666667425, 6.760013919724027431 ) ) ;
#57328 = CARTESIAN_POINT ( 'NONE',  ( 9.178372771442999678, -77.94661130901299373, -6.069379357596000446 ) ) ;
#57329 = DIRECTION ( 'NONE',  ( -0.9999999999999998890, -1.433670265775999799E-08, 0.000000000000000000 ) ) ;
#57330 = CARTESIAN_POINT ( 'NONE',  ( 10.25000000000000000, -82.09999999999999432, 0.000000000000000000 ) ) ;
#57331 = CARTESIAN_POINT ( 'NONE',  ( -1.169763865275986525, -82.90402275785740471, -0.9575444884849958482 ) ) ;
#57332 = PRODUCT_DEFINITION_SHAPE ( 'NONE', 'NONE',  #21399 ) ;
#57333 = CARTESIAN_POINT ( 'NONE',  ( -0.7154746835691508933, -79.67666239307115461, -1.026037770346891698 ) ) ;
#57334 = ORIENTED_EDGE ( 'NONE', *, *, #29794, .F. ) ;
#57335 = CARTESIAN_POINT ( 'NONE',  ( 0.000000000000000000, -76.29999999995945359, -10.59999999995999964 ) ) ;
#57336 = CARTESIAN_POINT ( 'NONE',  ( 1.799475295154000065, -21.75083378359999742, 12.69619287811000063 ) ) ;
#57337 = DIRECTION ( 'NONE',  ( 1.000000000000000000, 0.000000000000000000, 0.000000000000000000 ) ) ;
#57338 = ORIENTED_EDGE ( 'NONE', *, *, #20365, .F. ) ;
#57339 = VERTEX_POINT ( 'NONE', #5275 ) ;
#57340 = CARTESIAN_POINT ( 'NONE',  ( 0.000000000000000000, -75.67500000000001137, 0.000000000000000000 ) ) ;
#57341 = ORIENTED_EDGE ( 'NONE', *, *, #28961, .F. ) ;
#57342 = CARTESIAN_POINT ( 'NONE',  ( -4.435886197818010857, -79.83672437013201773, -8.483855872844232593 ) ) ;
#57343 = ORIENTED_EDGE ( 'NONE', *, *, #3507, .F. ) ;
#57344 = CARTESIAN_POINT ( 'NONE',  ( -3.834123575518456395, -81.00000000000002842, -10.21712803629676536 ) ) ;
#57345 = CARTESIAN_POINT ( 'NONE',  ( 2.897215155706000189, -77.21978472970600649, -10.52527958449999979 ) ) ;
#57346 = ITEM_DEFINED_TRANSFORMATION ( 'NONE', 'NONE', #48948,  #43526 ) ;
#57347 = AXIS2_PLACEMENT_3D ( 'NONE', #12418, #7411, #8272 ) ;
#57349 = EDGE_CURVE ( 'NONE', #20811, #49641, #16634, .T. ) ;
#57348 = CARTESIAN_POINT ( 'NONE',  ( 9.525749612248999298, -78.52913667140100529, 2.735063621234999687 ) ) ;
#57350 = CARTESIAN_POINT ( 'NONE',  ( -1.407736081117633375, -78.21296968607886413, -9.142491334826452487 ) ) ;
#57351 = CARTESIAN_POINT ( 'NONE',  ( 6.879576957522999692, -79.02077514267600122, 8.859431780707000215 ) ) ;
#57352 = ORIENTED_EDGE ( 'NONE', *, *, #26031, .F. ) ;
#57354 = ORIENTED_EDGE ( 'NONE', *, *, #22297, .T. ) ;
#57353 = EDGE_CURVE ( 'NONE', #13623, #29156, #34980, .T. ) ;
#57355 = CARTESIAN_POINT ( 'NONE',  ( -4.388972190985573008, -77.51444041639624061, 8.142476534846730729 ) ) ;
#57356 = CARTESIAN_POINT ( 'NONE',  ( 0.000000000000000000, -18.75000000000000000, -12.00000000000000000 ) ) ;
#57357 = CARTESIAN_POINT ( 'NONE',  ( 0.000000000000000000, -82.29687500001199396, 0.000000000000000000 ) ) ;
#57358 = CARTESIAN_POINT ( 'NONE',  ( -12.66316452100000056, -61.97866137636000161, 0.04044945982128999445 ) ) ;
#57359 = CARTESIAN_POINT ( 'NONE',  ( -2.183112477083999803, -77.72320829419898303, 9.455407409464999802 ) ) ;
#57360 = CARTESIAN_POINT ( 'NONE',  ( 7.654537165467999671, -18.71943464842000182, 10.01332852689000141 ) ) ;
#57361 = CIRCLE ( 'NONE', #39450, 10.50000000000000000 ) ;
#57362 = DIRECTION ( 'NONE',  ( 0.000000000000000000, 1.000000000000000000, 0.000000000000000000 ) ) ;
#57363 = CARTESIAN_POINT ( 'NONE',  ( 9.841113773926924324, -53.96371975908724750, -8.121706172282767255 ) ) ;
#57364 = CARTESIAN_POINT ( 'NONE',  ( -4.017143116098000455, -80.21358937413599222, 10.51352533724000082 ) ) ;
#57365 = DIRECTION ( 'NONE',  ( 0.000000000000000000, 1.000000000000000000, 0.000000000000000000 ) ) ;
#57366 = CARTESIAN_POINT ( 'NONE',  ( -0.6081994495308999937, -82.21302711298000077, -1.142242026498999863 ) ) ;
#57367 = ADVANCED_FACE ( 'NONE', ( #54864 ), #14411, .F. ) ;
#57368 = CARTESIAN_POINT ( 'NONE',  ( -9.571781413763634561, -76.65043581209883428, 6.814946930798515545 ) ) ;
#57369 = ORIENTED_EDGE ( 'NONE', *, *, #7385, .F. ) ;
#57370 = CARTESIAN_POINT ( 'NONE',  ( -12.06632373222999988, -79.58087695312399035, -0.6505690833180000077 ) ) ;
#57371 = CARTESIAN_POINT ( 'NONE',  ( -7.606021555054999439, -55.37841460039999930, 10.52692944503000128 ) ) ;
#57372 = CARTESIAN_POINT ( 'NONE',  ( 10.99419336675999936, -78.98418847654799890, 4.758540471090999979 ) ) ;
#57373 = CARTESIAN_POINT ( 'NONE',  ( -10.30768118225000052, -18.25239703915999812, -7.634415485503000198 ) ) ;
#57375 = CARTESIAN_POINT ( 'NONE',  ( -0.005928781627584999749, -16.79886949736999924, -12.66336824419000173 ) ) ;
#57374 = CARTESIAN_POINT ( 'NONE',  ( 8.081978225942579641, -78.39170613804414245, 4.658214607401315988 ) ) ;
#57376 = DIRECTION ( 'NONE',  ( 0.000000000000000000, 1.000000000000000000, 0.000000000000000000 ) ) ;
#57377 = SURFACE_SIDE_STYLE ('',( #25787 ) ) ;
#57378 = DIRECTION ( 'NONE',  ( 1.000000000000000000, 0.000000000000000000, 0.000000000000000000 ) ) ;
#57379 = CARTESIAN_POINT ( 'NONE',  ( 4.292950718366999929, -76.97953055567299430, -10.41175003194000048 ) ) ;
#57380 = CARTESIAN_POINT ( 'NONE',  ( 1.588866964187630071, -3.499999999999999556, 2.959281665799033512 ) ) ;
#57381 = CARTESIAN_POINT ( 'NONE',  ( 4.228967157898000373, -80.66775882426230737, 10.43118177971000016 ) ) ;
#57382 = ORIENTED_EDGE ( 'NONE', *, *, #53892, .T. ) ;
#57383 = LINE ( 'NONE', #16943, #46169 ) ;
#57384 = DIRECTION ( 'NONE',  ( 0.000000000000000000, 1.000000000000000000, 0.000000000000000000 ) ) ;
#57385 = B_SPLINE_CURVE_WITH_KNOTS ( 'NONE', 3,
 ( #10618, #28600, #29749, #15618, #7623, #21196, #38336, #3206, #2061, #56359, #33613, #7052, #43352, #20062, #15910, #2346, #38629, #51656 ),
 .UNSPECIFIED., .F., .F.,
 ( 4, 2, 2, 2, 2, 2, 2, 2, 4 ),
 ( 0.000000000000000000, 0.1249999999999999445, 0.2499999999999998890, 0.3749999999999998335, 0.4999999999999997780, 0.6249999999999997780, 0.7499999999999997780, 0.8749999999999997780, 1.000000000000000000 ),
 .UNSPECIFIED. ) ;
#57386 = CARTESIAN_POINT ( 'NONE',  ( 7.624341766647000362, -18.73514853758999976, -10.42531125024999916 ) ) ;
#57387 = CARTESIAN_POINT ( 'NONE',  ( 2.162366405920999490, -2.955934344712999984, 2.935303670011000232 ) ) ;
#57388 = CARTESIAN_POINT ( 'NONE',  ( 7.653972382670000130, -79.72123425335998093, -5.499357303777000716 ) ) ;
#57389 = CARTESIAN_POINT ( 'NONE',  ( -12.72397198031000087, -55.57854962903999763, 1.930909771329999858 ) ) ;
#57390 = CARTESIAN_POINT ( 'NONE',  ( 9.873180114738437041, -77.20000000000000284, 4.400785053488170284 ) ) ;
#57391 = CARTESIAN_POINT ( 'NONE',  ( 0.000000000000000000, -55.54999999966999980, -12.00000000000000000 ) ) ;
#57392 = DIRECTION ( 'NONE',  ( 0.000000000000000000, -1.000000000000000000, 0.000000000000000000 ) ) ;
#57393 = CARTESIAN_POINT ( 'NONE',  ( 4.174648323465000033, -85.50899735065199536, 0.04371857074945000032 ) ) ;
#57394 = VECTOR ( 'NONE', #12287, 1000.000000000000114 ) ;
#57395 = CYLINDRICAL_SURFACE ( 'NONE', #2798, 1.250000000000000000 ) ;
#57396 = B_SPLINE_CURVE_WITH_KNOTS ( 'NONE', 3,
 ( #27936, #23234, #18234, #14079, #37386, #31480, #45097, #251, #31780, #49823, #19683, #20838, #37683, #33241, #32947, #29682, #55699, #29397 ),
 .UNSPECIFIED., .F., .F.,
 ( 4, 2, 2, 2, 2, 2, 2, 2, 4 ),
 ( 0.000000000000000000, 0.1250000000000000833, 0.2500000000000001665, 0.3750000000000001110, 0.5000000000000001110, 0.6250000000000001110, 0.7500000000000000000, 0.8750000000000000000, 1.000000000000000000 ),
 .UNSPECIFIED. ) ;
#57397 = CARTESIAN_POINT ( 'NONE',  ( 10.64494183963000040, -78.10762918024498447, -1.773784135661999883 ) ) ;
#57398 = CARTESIAN_POINT ( 'NONE',  ( 10.99484708662753185, -76.42110442038233487, -4.160114065378057724 ) ) ;
#57399 = CARTESIAN_POINT ( 'NONE',  ( -11.07095105964000048, -78.19956549158798964, 1.299477954992000139 ) ) ;
#57400 = CARTESIAN_POINT ( 'NONE',  ( 0.8960442985632506296, -81.91201433914557128, 0.8711734550944890687 ) ) ;
#57401 = CARTESIAN_POINT ( 'NONE',  ( -0.6945049390072000062, -78.92075392059999217, -1.511688483436000041 ) ) ;
#57402 = CARTESIAN_POINT ( 'NONE',  ( -3.591972190522999764, -77.11482436373709959, 8.980252640667000463 ) ) ;
#57403 = CARTESIAN_POINT ( 'NONE',  ( -2.364557222828000072, -79.40474415034600497, 9.257622954664000758 ) ) ;
#57404 = CARTESIAN_POINT ( 'NONE',  ( -2.772200916640183976, -0.7825520741520030077, -2.131510823956923151 ) ) ;
#57405 = CARTESIAN_POINT ( 'NONE',  ( 1.469922439804874026, -80.23638809882929479, -10.65449918043788635 ) ) ;
#57406 = EDGE_CURVE ( 'NONE', #37071, #4000, #40654, .T. ) ;
#57407 = DIRECTION ( 'NONE',  ( 1.000000000000000000, 0.000000000000000000, 0.000000000000000000 ) ) ;
#57408 = CARTESIAN_POINT ( 'NONE',  ( 10.12072861152395298, -79.63538404776677737, 4.836575372680795404 ) ) ;
#57409 = AXIS2_PLACEMENT_3D ( 'NONE', #57356, #39055, #4206 ) ;
#57410 = CARTESIAN_POINT ( 'NONE',  ( -5.092641036025000290, -79.47589207986699478, 10.89826376711000044 ) ) ;
#57411 = CARTESIAN_POINT ( 'NONE',  ( 0.6295237254636211199, -81.83333333333334281, 1.092232985442824322 ) ) ;
#57412 = CARTESIAN_POINT ( 'NONE',  ( 4.801746450173999925, -79.66335789300599401, 10.18710928510000002 ) ) ;
#57413 = CARTESIAN_POINT ( 'NONE',  ( 0.000000000000000000, -81.10000000285099020, 5.900000002850999792 ) ) ;
#57414 = EDGE_LOOP ( 'NONE', ( #43268, #7606, #22201, #48391 ) ) ;
#57415 = LINE ( 'NONE', #29949, #506 ) ;
#57416 = ORIENTED_EDGE ( 'NONE', *, *, #34032, .F. ) ;
#57417 = ORIENTED_EDGE ( 'NONE', *, *, #4006, .F. ) ;
#57418 = CARTESIAN_POINT ( 'NONE',  ( 1.997276839918466829, -1.322916666666666963, 2.598917237794090784 ) ) ;
#57419 = CARTESIAN_POINT ( 'NONE',  ( 11.75000000000000178, -77.53958333333331154, -1.538071403319980268 ) ) ;
#57420 = CARTESIAN_POINT ( 'NONE',  ( -3.960513469484321813, -79.30881237240771497, 8.637712416346211342 ) ) ;
#57421 = ORIENTED_EDGE ( 'NONE', *, *, #13353, .F. ) ;
#57422 = CARTESIAN_POINT ( 'NONE',  ( 7.921848887473175616, -78.29045646104971468, -7.357746221004406451 ) ) ;
#57423 = CARTESIAN_POINT ( 'NONE',  ( 11.12418552951999828, -78.71975279073001275, -5.383704713749000170 ) ) ;
#57424 = ORIENTED_EDGE ( 'NONE', *, *, #43089, .T. ) ;
#57425 = CARTESIAN_POINT ( 'NONE',  ( -10.53562597590999950, -60.00558297591999946, 7.620013358898000355 ) ) ;
#57427 = ORIENTED_EDGE ( 'NONE', *, *, #11235, .F. ) ;
#57426 = EDGE_CURVE ( 'NONE', #40455, #1033, #25022, .T. ) ;
#57428 = LINE ( 'NONE', #53000, #41427 ) ;
#57429 = CARTESIAN_POINT ( 'NONE',  ( 2.774709120699121456, -79.79999999999999716, 11.60977811668827364 ) ) ;
#57430 = CARTESIAN_POINT ( 'NONE',  ( -6.857072527857152267, -80.03044501592233928, 8.278933358856727764 ) ) ;
#57431 = CARTESIAN_POINT ( 'NONE',  ( 8.838834764832000701, -23.25000000000000000, -8.838834764832000701 ) ) ;
#57432 = CIRCLE ( 'NONE', #32929, 12.50000000000000000 ) ;
#57433 = DIRECTION ( 'NONE',  ( 0.000000000000000000, -1.000000000000000000, 0.000000000000000000 ) ) ;
#57434 = CARTESIAN_POINT ( 'NONE',  ( -0.6316792277967039348, -85.98317637962277615, 3.377175175332928880 ) ) ;
#57435 = DIRECTION ( 'NONE',  ( 0.000000000000000000, -1.000000000000000000, 0.000000000000000000 ) ) ;
#57436 = CARTESIAN_POINT ( 'NONE',  ( -12.60246356036999948, -77.25062674423000431, -0.9915196953554998860 ) ) ;
#57437 = CARTESIAN_POINT ( 'NONE',  ( -5.138289791457000710, -76.61246662722099643, -9.595228483104000006 ) ) ;
#57438 = EDGE_CURVE ( 'NONE', #35853, #50685, #1071, .T. ) ;
#57439 = CARTESIAN_POINT ( 'NONE',  ( -9.156831961090404093, -78.61148368715173262, -1.313898468327503899 ) ) ;
#57440 = CARTESIAN_POINT ( 'NONE',  ( -4.030735489442000663, -81.94082221650599251, -0.9009357681566000364 ) ) ;
#57441 = CYLINDRICAL_SURFACE ( 'NONE', #54411, 12.00000000000000000 ) ;
#57442 = CARTESIAN_POINT ( 'NONE',  ( -1.245586717227264106, -3.007515495460388433, 3.001037710528552616 ) ) ;
#57443 = CARTESIAN_POINT ( 'NONE',  ( -0.05200060359788999387, -79.84105496681198133, 3.546668618212000190 ) ) ;
#57444 = AXIS2_PLACEMENT_3D ( 'NONE', #6315, #37022, #42044 ) ;
#57445 = FACE_OUTER_BOUND ( 'NONE', #18578, .T. ) ;
#57446 = CARTESIAN_POINT ( 'NONE',  ( 3.133033872897999839, -82.55394503318800048, 1.663074877879000102 ) ) ;
#57447 = CARTESIAN_POINT ( 'NONE',  ( 1.068619641472000170, -1.895647048966000003, -3.652926003266999899 ) ) ;
#57448 = CARTESIAN_POINT ( 'NONE',  ( 1.268713167172250245, -80.00820858014098746, 0.1245986402332493470 ) ) ;
#57449 = CARTESIAN_POINT ( 'NONE',  ( -7.658894224196000522, -60.00939395830999956, -10.01676912202999858 ) ) ;
#57450 = CARTESIAN_POINT ( 'NONE',  ( -9.250000000000000000, -79.49999999999998579, 1.813240672189999963E-14 ) ) ;
#57451 = CARTESIAN_POINT ( 'NONE',  ( -1.179157772963000061, -82.09565872228399996, 0.6230118014947999550 ) ) ;
#57452 = CARTESIAN_POINT ( 'NONE',  ( -5.762329935654880941, -78.97333333333331495, -7.594666746517801492 ) ) ;
#57453 = CYLINDRICAL_SURFACE ( 'NONE', #20607, 12.00000000000000000 ) ;
#57454 = CARTESIAN_POINT ( 'NONE',  ( -0.09713983013762958474, -79.51964965042942879, -1.537455523586754857 ) ) ;
#57455 = LINE ( 'NONE', #16156, #41518 ) ;
#57456 = CARTESIAN_POINT ( 'NONE',  ( -4.097539515550000289, -75.98334464165999691, 11.66336447688000000 ) ) ;
#57457 = ORIENTED_EDGE ( 'NONE', *, *, #7484, .T. ) ;
#57458 = CARTESIAN_POINT ( 'NONE',  ( 11.00000000000000000, -81.00000000000000000, -2.369510767747999942E-13 ) ) ;
#57459 = DIRECTION ( 'NONE',  ( 0.000000000000000000, -1.000000000000000000, 0.000000000000000000 ) ) ;
#57460 = CARTESIAN_POINT ( 'NONE',  ( 12.43422056534000042, -61.23655741401000085, 1.197404442626999854 ) ) ;
#57461 = CARTESIAN_POINT ( 'NONE',  ( -1.799502287691000069, -23.30716680861999990, -12.60413670420000010 ) ) ;
#57462 = CARTESIAN_POINT ( 'NONE',  ( 4.710185975415000392, -77.55872832793998839, -8.400437955132002088 ) ) ;
#57463 = CARTESIAN_POINT ( 'NONE',  ( 0.2926765216785000012, -85.10431426239898656, -4.162260556948999657 ) ) ;
#57464 = CARTESIAN_POINT ( 'NONE',  ( -1.738099071051254940, -79.98838542116494921, 10.60879108008627902 ) ) ;
#57465 = CARTESIAN_POINT ( 'NONE',  ( -1.390602365772999782, -80.58707595801800494, 0.2763432473779000587 ) ) ;
#57466 = ORIENTED_EDGE ( 'NONE', *, *, #2361, .F. ) ;
#57467 = EDGE_CURVE ( 'NONE', #409, #16887, #15274, .T. ) ;
#57468 = CARTESIAN_POINT ( 'NONE',  ( -10.71369944335147117, -78.72083333333330302, -2.879226727952077791 ) ) ;
#57469 = CARTESIAN_POINT ( 'NONE',  ( 1.111733232284327855, -78.92199391444442824, -3.740299636916243564 ) ) ;
#57470 = ORIENTED_EDGE ( 'NONE', *, *, #25665, .T. ) ;
#57471 = ADVANCED_FACE ( 'NONE', ( #7020 ), #26699, .F. ) ;
#57472 = CARTESIAN_POINT ( 'NONE',  ( -9.781527233834999890, -78.90776930244898324, -4.899953194656999855 ) ) ;
#57473 = CARTESIAN_POINT ( 'NONE',  ( 12.58335110162999904, -58.54888345776999614, 1.667961430005999945 ) ) ;
#57474 = CARTESIAN_POINT ( 'NONE',  ( 8.751463191605999725, -80.00217580634098624, -7.195874488014000647 ) ) ;
#57475 = ORIENTED_EDGE ( 'NONE', *, *, #34364, .T. ) ;
#57476 = AXIS2_PLACEMENT_3D ( 'NONE', #8895, #35153, #8021 ) ;
#57477 = EDGE_LOOP ( 'NONE', ( #6079, #42912, #58004, #699 ) ) ;
#57478 = ORIENTED_EDGE ( 'NONE', *, *, #9886, .T. ) ;
#57479 = AXIS2_PLACEMENT_3D ( 'NONE', #35161, #12742, #8907 ) ;
#57480 = CARTESIAN_POINT ( 'NONE',  ( -3.047098712557896771, -78.09418507123076836, 11.37766269708934708 ) ) ;
#57481 = DIRECTION ( 'NONE',  ( 0.7071067812094172789, -2.924115120139070516E-07, 0.7071067811636172484 ) ) ;
#57482 = ORIENTED_EDGE ( 'NONE', *, *, #21366, .F. ) ;
#57484 = EDGE_CURVE ( 'NONE', #30606, #1677, #42517, .T. ) ;
#57483 = ORIENTED_EDGE ( 'NONE', *, *, #5230, .F. ) ;
#57485 = CARTESIAN_POINT ( 'NONE',  ( -0.01872868506982610856, -79.52637485864291023, 1.273763531464531695 ) ) ;
#57486 = CARTESIAN_POINT ( 'NONE',  ( 3.851650068367000745, -78.96264283715740362, -1.429791614965258972E-15 ) ) ;
#57487 = CARTESIAN_POINT ( 'NONE',  ( 7.620037552694999938, -55.59433113521999559, 10.53559761426999764 ) ) ;
#57488 = CARTESIAN_POINT ( 'NONE',  ( -7.000000000000000000, -81.99999999999998579, 0.000000000000000000 ) ) ;
#57489 = CARTESIAN_POINT ( 'NONE',  ( -4.716969250163658423, -79.63541666666263552, 8.182319322371521153 ) ) ;
#57490 = CARTESIAN_POINT ( 'NONE',  ( 12.70253258978874733, -61.77063167637336960, -0.9890392130593611553 ) ) ;
#57491 = CARTESIAN_POINT ( 'NONE',  ( -1.344070316215177030, -77.81207131835833479, 0.6864365363003362974 ) ) ;
#57492 = EDGE_CURVE ( 'NONE', #19229, #44346, #46249, .T. ) ;
#57493 = CARTESIAN_POINT ( 'NONE',  ( 8.617899982024150418, -78.82053113868873595, -3.361248075313672423 ) ) ;
#57494 = AXIS2_PLACEMENT_3D ( 'NONE', #9085, #39496, #17062 ) ;
#57495 = CARTESIAN_POINT ( 'NONE',  ( -10.36292431357999888, -23.20096201633999655, 7.633479737313000335 ) ) ;
#57496 = EDGE_CURVE ( 'NONE', #16250, #19958, #46327, .T. ) ;
#57497 = CARTESIAN_POINT ( 'NONE',  ( -1.508376887600999972, -78.93025264934789220, -3.892856298602999754 ) ) ;
#57498 = CARTESIAN_POINT ( 'NONE',  ( -9.741854131801998662, -77.26208667140099351, -0.6374903164020000457 ) ) ;
#57499 = CARTESIAN_POINT ( 'NONE',  ( -0.6295237254636286695, -83.41666666666668561, 1.092232985442819881 ) ) ;
#57500 = CARTESIAN_POINT ( 'NONE',  ( 12.76303204294999993, -23.26485150694999859, -1.980584515756000030 ) ) ;
#57501 = CARTESIAN_POINT ( 'NONE',  ( -6.018890980713000438, -75.91407976174099304, 10.70471907396000155 ) ) ;
#57502 = DIRECTION ( 'NONE',  ( -1.000000000000000000, 0.000000000000000000, 0.000000000000000000 ) ) ;
#57503 = CARTESIAN_POINT ( 'NONE',  ( 12.50412785605847432, -24.51985834634450256, -1.235051469881349506 ) ) ;
#57504 = CARTESIAN_POINT ( 'NONE',  ( -1.217465845835394411, -78.52083333333332860, -0.3271848554491003647 ) ) ;
#57505 = CARTESIAN_POINT ( 'NONE',  ( 1.238215446118554164, -80.15090966697889030, 0.9263567608796238195 ) ) ;
#57506 = CARTESIAN_POINT ( 'NONE',  ( 2.240069435031999845, -77.16499869373629394, -9.110799550206998276 ) ) ;
#57507 = CARTESIAN_POINT ( 'NONE',  ( -0.7952960770845000082, -78.32404029686399838, 1.405246626978000180 ) ) ;
#57508 = CARTESIAN_POINT ( 'NONE',  ( -13.63885489310999510, -19.21421830981000056, -7.254376133916000668 ) ) ;
#57509 = CARTESIAN_POINT ( 'NONE',  ( 0.2030686677330999779, -3.598078325257000110, -3.551685225877000196 ) ) ;
#57510 = AXIS2_PLACEMENT_3D ( 'NONE', #22385, #40396, #13819 ) ;
#57511 = CARTESIAN_POINT ( 'NONE',  ( -3.162453476786999840, -77.97768216442000266, -11.86569286591000072 ) ) ;
#57512 = CARTESIAN_POINT ( 'NONE',  ( 1.500000000000000000, -80.76041666666668561, 0.1963495408493652339 ) ) ;
#57513 = EDGE_CURVE ( 'NONE', #5930, #10595, #17318, .T. ) ;
#57515 = CARTESIAN_POINT ( 'NONE',  ( -0.2380956042587999977, -78.85250196101499398, -1.297642515519999984 ) ) ;
#57514 = CARTESIAN_POINT ( 'NONE',  ( 1.883721702039359291, -75.80000000000002558, 11.98327435467166602 ) ) ;
#57516 = CARTESIAN_POINT ( 'NONE',  ( -1.477496145247999992, -82.67709261769098816, 0.5756751103899000466 ) ) ;
#57517 = CARTESIAN_POINT ( 'NONE',  ( -6.422077643389767942, -79.52599266752667972, 8.620883091140045806 ) ) ;
#57518 = ORIENTED_EDGE ( 'NONE', *, *, #39730, .F. ) ;
#57519 = CARTESIAN_POINT ( 'NONE',  ( -1.217465845835394411, -82.02083333333330017, -0.3271848554491003647 ) ) ;
#57520 = CARTESIAN_POINT ( 'NONE',  ( 1.162094749123000037, -79.12624453345600273, 12.10061229221000012 ) ) ;
#57521 = CARTESIAN_POINT ( 'NONE',  ( -9.450981695478892775, -79.25824793529314150, -0.9830935124726688512 ) ) ;
#57522 = CARTESIAN_POINT ( 'NONE',  ( 2.220128896776556893, -80.00000000000000000, -9.233834223992447576 ) ) ;
#57523 = CARTESIAN_POINT ( 'NONE',  ( -9.611650271896857944, -79.05833333333333712, 5.539808784079855997 ) ) ;
#57524 = CARTESIAN_POINT ( 'NONE',  ( 3.428456835174999995, -1.314283069271000137, 0.8759089407426000617 ) ) ;
#57525 = CARTESIAN_POINT ( 'NONE',  ( 9.363799758325001221, -78.88336945908598352, -1.158156830125999903 ) ) ;
#57526 = CARTESIAN_POINT ( 'NONE',  ( 12.77651065749000026, -25.30896598096000005, 0.04308629978603999849 ) ) ;
#57527 = CARTESIAN_POINT ( 'NONE',  ( -1.799502287743000029, -60.10716934574000447, 12.60413652834999887 ) ) ;
#57528 = ORIENTED_EDGE ( 'NONE', *, *, #51094, .T. ) ;
#57529 = EDGE_CURVE ( 'NONE', #22028, #38753, #36390, .T. ) ;
#57530 = FACE_OUTER_BOUND ( 'NONE', #10821, .T. ) ;
#57531 = DIRECTION ( 'NONE',  ( 0.000000000000000000, 1.000000000000000000, 0.000000000000000000 ) ) ;
#57532 = CARTESIAN_POINT ( 'NONE',  ( 7.342331066867000544, -55.64999999967000122, 8.190859204290999784 ) ) ;
#57533 = EDGE_CURVE ( 'NONE', #28878, #48346, #18107, .T. ) ;
#57534 = CARTESIAN_POINT ( 'NONE',  ( 0.1963495408493637351, -78.53541666666669130, -1.499999999999999778 ) ) ;
#57535 = CARTESIAN_POINT ( 'NONE',  ( -2.266963109989999836, -84.47167953870898316, 2.728631686324999972 ) ) ;
#57536 = ORIENTED_EDGE ( 'NONE', *, *, #46270, .F. ) ;
#57537 = VECTOR ( 'NONE', #47987, 999.9999999999998863 ) ;
#57538 = DIRECTION ( 'NONE',  ( -1.000000000000000000, 0.000000000000000000, 0.000000000000000000 ) ) ;
#57539 = CARTESIAN_POINT ( 'NONE',  ( 9.546819346760999636, -61.48527546573999558, -8.130850182902999990 ) ) ;
#57540 = CARTESIAN_POINT ( 'NONE',  ( -1.750000000001000089, -55.55000001292999912, -12.56594318049000059 ) ) ;
#57541 = ORIENTED_EDGE ( 'NONE', *, *, #30039, .F. ) ;
#57542 = CARTESIAN_POINT ( 'NONE',  ( -7.974020021219000220, -54.16898233660000272, -9.929669236765001017 ) ) ;
#57543 =( NAMED_UNIT ( * ) PLANE_ANGLE_UNIT ( ) SI_UNIT ( $, .RADIAN. ) );
#57544 = CARTESIAN_POINT ( 'NONE',  ( -7.479908383216000267, -79.32543322980198752, -6.281056869080000382 ) ) ;
#57545 = EDGE_LOOP ( 'NONE', ( #56842, #6009, #40948, #7894, #31533, #35023 ) ) ;
#57546 = ORIENTED_EDGE ( 'NONE', *, *, #37431, .F. ) ;
#57547 = CARTESIAN_POINT ( 'NONE',  ( -0.6708319208533000122, -76.31181275097399919, -12.33441669056000123 ) ) ;
#57548 = CARTESIAN_POINT ( 'NONE',  ( -10.45176477158148742, -78.61882830641657449, -2.514439583694316305 ) ) ;
#57549 = ORIENTED_EDGE ( 'NONE', *, *, #25689, .T. ) ;
#57550 = CARTESIAN_POINT ( 'NONE',  ( -5.597970637881999778, -77.11533084965400064, 7.669424558767000022 ) ) ;
#57551 = CIRCLE ( 'NONE', #17030, 1.750000000000000000 ) ;
#57552 = CARTESIAN_POINT ( 'NONE',  ( -4.100000000000000533, -78.69999999999998863, 0.000000000000000000 ) ) ;
#57553 = CARTESIAN_POINT ( 'NONE',  ( -1.750000000000000000, -76.50000000000000000, 0.000000000000000000 ) ) ;
#57554 = CARTESIAN_POINT ( 'NONE',  ( -3.291354266399999950, -77.06423739310000087, 12.36836470155000001 ) ) ;
#57555 = CARTESIAN_POINT ( 'NONE',  ( -4.647088938219000376, -78.15899331454487253, 10.20895072913000057 ) ) ;
#57556 = CARTESIAN_POINT ( 'NONE',  ( -10.39315812627616431, -78.40567703563392854, 6.510797611460747092 ) ) ;
#57557 = CARTESIAN_POINT ( 'NONE',  ( 4.358902656273683007, -86.39318692756700102, 0.5003316865777546196 ) ) ;
#57558 = CARTESIAN_POINT ( 'NONE',  ( 5.865103843792000227, -78.57046857046199761, -9.561319920857000554 ) ) ;
#57559 = CARTESIAN_POINT ( 'NONE',  ( 3.483691356461174227, -79.94435685530504543, 8.568905828578699868 ) ) ;
#57560 = CARTESIAN_POINT ( 'NONE',  ( 0.000000000000000000, -74.64999999999999147, 0.000000000000000000 ) ) ;
#57561 = ORIENTED_EDGE ( 'NONE', *, *, #51735, .T. ) ;
#57562 = CARTESIAN_POINT ( 'NONE',  ( 4.019191877497999776, -79.46678520010797797, 10.52497178225999974 ) ) ;
#57563 = CARTESIAN_POINT ( 'NONE',  ( 6.634060730155967534, -77.28871036968435249, -6.446087520221595923 ) ) ;
#57564 = CARTESIAN_POINT ( 'NONE',  ( -0.6144861720749000833, -80.82555782932399779, -1.073086222052999972 ) ) ;
#57565 = DIRECTION ( 'NONE',  ( -1.000000000000000000, 1.534883903844000000E-11, 4.134220892123999815E-14 ) ) ;
#57566 = CARTESIAN_POINT ( 'NONE',  ( 1.668607604626967778, -60.59381631189521755, -12.52787843855117345 ) ) ;
#57567 = CARTESIAN_POINT ( 'NONE',  ( 3.328509078748080441, -3.072971510259623784, -1.143234280529020763 ) ) ;
#57568 = CARTESIAN_POINT ( 'NONE',  ( 12.87022657272000004, -22.78485473281999774, 2.062597299672999540 ) ) ;
#57569 = CARTESIAN_POINT ( 'NONE',  ( 7.947168433127743015, -78.27084849470611516, 9.085795500190322116 ) ) ;
#57570 = CARTESIAN_POINT ( 'NONE',  ( -12.60552522436000089, -18.71082434677000350, -1.799501877760999902 ) ) ;
#57571 = DIRECTION ( 'NONE',  ( 0.7071067811865475727, 0.000000000000000000, 0.7071067811865475727 ) ) ;
#57572 = CARTESIAN_POINT ( 'NONE',  ( -10.83342013959000028, -79.03770885299998383, 2.669945268378000058 ) ) ;
#57573 = CARTESIAN_POINT ( 'NONE',  ( 10.18589234708000113, -18.71082434677000350, -7.641012386038000592 ) ) ;
#57574 = CARTESIAN_POINT ( 'NONE',  ( 5.753255980621002408, -78.98433428202568507, 10.26026234797696723 ) ) ;
#57575 = CARTESIAN_POINT ( 'NONE',  ( 3.979600690714999889, -82.46144529440799431, 0.4014307432961000122 ) ) ;
#57576 = CARTESIAN_POINT ( 'NONE',  ( 1.500000000000000000, -80.15000000000000568, 0.000000000000000000 ) ) ;
#57577 = AXIS2_PLACEMENT_3D ( 'NONE', #28862, #56330, #15882 ) ;
#57578 = VERTEX_POINT ( 'NONE', #48344 ) ;
#57579 = CARTESIAN_POINT ( 'NONE',  ( -1.608404438602769160, -77.20000000000000284, 10.70099509088003487 ) ) ;
#57580 = CARTESIAN_POINT ( 'NONE',  ( -0.4670233199325999895, -80.85741372253998804, 1.392241846115000126 ) ) ;
#57581 = CARTESIAN_POINT ( 'NONE',  ( -10.40626589979188488, -79.12100314181128624, -2.787243473566140661 ) ) ;
#57582 = CARTESIAN_POINT ( 'NONE',  ( 11.88382656225999945, -78.23823650824398612, -1.513515996960000054 ) ) ;
#57583 = MANIFOLD_SOLID_BREP ( 'Stock-MAS-694-1', #54131 ) ;
#57584 = CARTESIAN_POINT ( 'NONE',  ( -12.71005124797314778, -17.70500926713873469, 1.687536500553408647 ) ) ;
#57585 = CARTESIAN_POINT ( 'NONE',  ( -1.000564195253814015, -79.19723941947405876, 0.7893538131252750834 ) ) ;
#57586 = DIRECTION ( 'NONE',  ( 1.000000000000000000, 0.000000000000000000, 0.000000000000000000 ) ) ;
#57587 = CARTESIAN_POINT ( 'NONE',  ( -3.230363664242999810, -78.28820584965400542, -9.171071524558000121 ) ) ;
#57588 = CARTESIAN_POINT ( 'NONE',  ( -1.173259754689000234, -78.82221935430098370, -9.559114633834001395 ) ) ;
#57590 = EDGE_CURVE ( 'NONE', #36712, #34390, #55755, .T. ) ;
#57589 = CARTESIAN_POINT ( 'NONE',  ( -1.798368564629000188, -55.60363242921000193, -12.61278090839000043 ) ) ;
#57591 = CARTESIAN_POINT ( 'NONE',  ( 11.55626480159407876, -75.96425890079613907, 2.125201638845596097 ) ) ;
#57592 = CARTESIAN_POINT ( 'NONE',  ( -2.759932835650348526, -86.02148118236286223, 3.725476775316406641 ) ) ;
#57593 = ORIENTED_EDGE ( 'NONE', *, *, #54501, .T. ) ;
#57594 = DIRECTION ( 'NONE',  ( 0.000000000000000000, -1.000000000000000000, 0.000000000000000000 ) ) ;
#57595 = CARTESIAN_POINT ( 'NONE',  ( -3.249633467300476308, -2.111888578168985120, -0.4260072675962560673 ) ) ;
#57596 = CARTESIAN_POINT ( 'NONE',  ( 0.2436306363661999985, -79.70001058397200211, 12.26886527195999932 ) ) ;
#57597 = B_SPLINE_CURVE_WITH_KNOTS ( 'NONE', 3,
 ( #4410, #25960, #22413, #12677 ),
 .UNSPECIFIED., .F., .F.,
 ( 4, 4 ),
 ( 0.000000000000000000, 1.000000000000000000 ),
 .UNSPECIFIED. ) ;
#57598 = CARTESIAN_POINT ( 'NONE',  ( 6.612939829087000732, -79.75369307542398190, 8.759739992124000452 ) ) ;
#57599 = CARTESIAN_POINT ( 'NONE',  ( 0.5668640726082777581, -17.08340305019257244, -12.50470739226994965 ) ) ;
#57600 = CARTESIAN_POINT ( 'NONE',  ( -11.31839317768999997, -76.97443299368299563, -5.033003383563999122 ) ) ;
#57601 = DIRECTION ( 'NONE',  ( -0.3090169943750105674, 0.000000000000000000, 0.9510565162951329921 ) ) ;
#57602 = CARTESIAN_POINT ( 'NONE',  ( 0.000000000000000000, -72.39999999999999147, 0.000000000000000000 ) ) ;
#57603 = ORIENTED_EDGE ( 'NONE', *, *, #22873, .T. ) ;
#57604 = AXIS2_PLACEMENT_3D ( 'NONE', #8472, #9657, #5227 ) ;
#57605 = CARTESIAN_POINT ( 'NONE',  ( -4.084105282113999813, -79.23595787040198957, -10.24801534084000032 ) ) ;
#57606 = CARTESIAN_POINT ( 'NONE',  ( -0.001903571469574895196, -79.97561236326164646, 1.249706230131253593 ) ) ;
#57607 = CARTESIAN_POINT ( 'NONE',  ( 7.376264119752973691, -75.80000000000003979, -9.324595548898168218 ) ) ;
#57608 = EDGE_CURVE ( 'NONE', #52412, #7313, #54520, .T. ) ;
#57609 = CARTESIAN_POINT ( 'NONE',  ( 9.855576673225998618, -79.45423432486698800, -5.230603033304000782 ) ) ;
#57610 = DIRECTION ( 'NONE',  ( 0.000000000000000000, 1.000000000000000000, 1.232687704540000236E-14 ) ) ;
#57611 = CARTESIAN_POINT ( 'NONE',  ( 8.838834764832000701, -18.75000000000000000, -8.838834764832000701 ) ) ;
#57612 = CARTESIAN_POINT ( 'NONE',  ( 0.04625940550791253492, -81.47683375462607103, -1.511023559015027162 ) ) ;
#57613 = CARTESIAN_POINT ( 'NONE',  ( -9.933360547807000174, -78.37660472681200474, -7.219704108085999827 ) ) ;
#57614 = ADVANCED_FACE ( 'NONE', ( #22921 ), #17615, .F. ) ;
#57615 = CARTESIAN_POINT ( 'NONE',  ( -2.813789756862300262, -79.39583333333331439, 10.47020627418438465 ) ) ;
#57616 = DIRECTION ( 'NONE',  ( 0.000000000000000000, -1.000000000000000000, 0.000000000000000000 ) ) ;
#57617 = SHAPE_REPRESENTATION_RELATIONSHIP ( 'NONE' , 'NONE' ,  #1422, #1805 ) ;
#57618 = EDGE_CURVE ( 'NONE', #55907, #47968, #51043, .T. ) ;
#57619 = DIRECTION ( 'NONE',  ( -1.000000000000000000, 0.000000000000000000, 0.000000000000000000 ) ) ;
#57620 = ORIENTED_EDGE ( 'NONE', *, *, #8442, .T. ) ;
#57621 = VERTEX_POINT ( 'NONE', #49804 ) ;
#57622 = AXIS2_PLACEMENT_3D ( 'NONE', #25819, #3393, #21389 ) ;
#57623 = CARTESIAN_POINT ( 'NONE',  ( 10.54436264862384043, -78.83449620097776744, -2.092280515037520772 ) ) ;
#57624 = CARTESIAN_POINT ( 'NONE',  ( 8.638761211478000135, -76.97991332859899671, 4.306371860147999442 ) ) ;
#57625 = B_SPLINE_CURVE_WITH_KNOTS ( 'NONE', 3,
 ( #32442, #18892, #50487, #19184, #1773, #1482, #18609, #19472, #41909, #14734, #36885, #32733, #37465, #55486, #41035 ),
 .UNSPECIFIED., .F., .F.,
 ( 4, 1, 1, 1, 1, 1, 1, 1, 1, 1, 1, 1, 4 ),
 ( 0.000000000000000000, 0.08333615544490723115, 0.1666676869327075872, 0.2500040218909077572, 0.3333307224267462732, 0.4166666700929356204, 0.4999999877701112316, 0.5833333064412306035, 0.6666692871879731364, 0.7499959940605083197, 0.8333323080421526363, 0.9166638616780954374, 1.000000000000000000 ),
 .UNSPECIFIED. ) ;
#57626 = ORIENTED_EDGE ( 'NONE', *, *, #26342, .F. ) ;
#57627 = CARTESIAN_POINT ( 'NONE',  ( -9.113568214466768680, -79.77523700399514439, -2.981120847293889486 ) ) ;
#57628 = ORIENTED_EDGE ( 'NONE', *, *, #11911, .T. ) ;
#57629 = CARTESIAN_POINT ( 'NONE',  ( -10.51004847261784114, -80.99999999999998579, -2.396571149024055547 ) ) ;
#57630 = CARTESIAN_POINT ( 'NONE',  ( 10.72166763895999964, -76.83847592767999402, 2.054558110510000368 ) ) ;
#57631 = CARTESIAN_POINT ( 'NONE',  ( -7.502741683071000089, -78.18383998579800220, -6.127813063941999872 ) ) ;
#57632 = CARTESIAN_POINT ( 'NONE',  ( -8.411043104783766822, -78.13496630202740789, -3.922096619641943782 ) ) ;
#57633 = CARTESIAN_POINT ( 'NONE',  ( -5.394429334091999984, -79.85118130000350334, -9.834543342166998769 ) ) ;
#57634 = ORIENTED_EDGE ( 'NONE', *, *, #3038, .F. ) ;
#57635 = VERTEX_POINT ( 'NONE', #27338 ) ;
#57636 = CARTESIAN_POINT ( 'NONE',  ( -6.541840594602032155, -77.53768247343118958, 6.539477767634727101 ) ) ;
#57637 = AXIS2_PLACEMENT_3D ( 'NONE', #34246, #51714, #6529 ) ;
#57638 = CARTESIAN_POINT ( 'NONE',  ( 9.391860901740999523, -77.16389274916278396, 5.803232400709999794 ) ) ;
#57639 = CARTESIAN_POINT ( 'NONE',  ( -0.7554284705563544255, -77.91666666666668561, 1.310679582531384169 ) ) ;
#57640 = AXIS2_PLACEMENT_3D ( 'NONE', #44698, #21952, #13386 ) ;
#57641 = CARTESIAN_POINT ( 'NONE',  ( -9.446433787353997857, -78.34853253503598580, -2.221620594898999990 ) ) ;
#57642 = CARTESIAN_POINT ( 'NONE',  ( 7.718368845809999712, -20.25199022618999933, 10.07722254369999959 ) ) ;
#57643 = CARTESIAN_POINT ( 'NONE',  ( -3.507835537823156713, -79.49465701644101046, -8.848935139560099472 ) ) ;
#57644 = CARTESIAN_POINT ( 'NONE',  ( -9.254388464354001087, -79.80752053325198858, 5.469807505829999528 ) ) ;
#57645 = CARTESIAN_POINT ( 'NONE',  ( -11.09141466634999951, -79.79597772074998829, 1.909950515085000022 ) ) ;
#57646 = CARTESIAN_POINT ( 'NONE',  ( 12.54980553589999914, -16.95222688865000293, 0.05649961219511000221 ) ) ;
#57647 = CARTESIAN_POINT ( 'NONE',  ( 1.092232985442823212, -78.20833333333332860, -0.6295237254636224522 ) ) ;
#57648 = DIRECTION ( 'NONE',  ( -1.000000000000000000, 6.386283326366000088E-09, 1.411454291414999872E-10 ) ) ;
#57649 = EDGE_LOOP ( 'NONE', ( #5099, #57262, #48570, #51701 ) ) ;
#57650 = CARTESIAN_POINT ( 'NONE',  ( -9.555168389065999079, -79.12901475210699687, -7.397172803072000313 ) ) ;
#57651 = CARTESIAN_POINT ( 'NONE',  ( -7.631889106307999882, -55.57878585374000124, 10.36222439673000117 ) ) ;
#57652 = CARTESIAN_POINT ( 'NONE',  ( 2.697636866285999968, -77.84475722874999803, -11.67213861177999945 ) ) ;
#57653 = CARTESIAN_POINT ( 'NONE',  ( -8.596775676242998543, -16.86467110163999905, -9.310147894694001280 ) ) ;
#57655 = CARTESIAN_POINT ( 'NONE',  ( -1.295048492660999973, -17.47106480873999956, -12.54716442236999896 ) ) ;
#57654 = CARTESIAN_POINT ( 'NONE',  ( 7.718346056099999686, -58.54888345776999614, 10.07719973192999952 ) ) ;
#57656 = CARTESIAN_POINT ( 'NONE',  ( 12.50000000000000000, -55.54999999966999980, 1.250000000000000000 ) ) ;
#57657 = CARTESIAN_POINT ( 'NONE',  ( 11.11690205930000097, -80.32095930235598757, 1.979307181865000098 ) ) ;
#57658 = CARTESIAN_POINT ( 'NONE',  ( 7.596835002782722057, -78.49791666666666856, -5.838193839761678383 ) ) ;
#57659 = CARTESIAN_POINT ( 'NONE',  ( -8.763613300111000370, -76.77071859265899434, 6.838397221053000408 ) ) ;
#57660 = CARTESIAN_POINT ( 'NONE',  ( 3.250000000000000444, -1.760416666666666963, 0.4254240051736247197 ) ) ;
#57661 = CARTESIAN_POINT ( 'NONE',  ( -11.22958316615000207, -80.82884494028411382, -0.7682314979056000803 ) ) ;
#57662 = ORIENTED_EDGE ( 'NONE', *, *, #54019, .F. ) ;
#57663 = DIRECTION ( 'NONE',  ( -0.6489586447440029993, 0.04890182322787019892, 0.7592504784964030362 ) ) ;
#57664 = CARTESIAN_POINT ( 'NONE',  ( 0.4802748259362999983, -53.79473092685000069, 12.54896097830000024 ) ) ;
#57665 = CARTESIAN_POINT ( 'NONE',  ( -12.49168433580000048, -18.70150862776000267, 1.667916687244999974 ) ) ;
#57666 = CARTESIAN_POINT ( 'NONE',  ( 3.641686272398999780, -3.385219557569000060, 0.1721552302819999991 ) ) ;
#57667 = STYLED_ITEM ( 'NONE', ( #14423 ), #51784 ) ;
#57668 = CARTESIAN_POINT ( 'NONE',  ( 7.155101792066000499, -78.37967353048000518, -8.354909834651998324 ) ) ;
#57669 = CARTESIAN_POINT ( 'NONE',  ( -8.300970689365446020, -77.34166666666666856, -4.784380313523547201 ) ) ;
#57670 = LINE ( 'NONE', #25799, #20399 ) ;
#57671 = CARTESIAN_POINT ( 'NONE',  ( -1.669724228651999987, -60.16897676502000536, 12.48434610070000161 ) ) ;
#57672 = CARTESIAN_POINT ( 'NONE',  ( 4.855043705795149656, -79.06749999999999545, -8.214633846514242776 ) ) ;
#57673 = CARTESIAN_POINT ( 'NONE',  ( 3.687580507110999939, -82.62299735065199968, 1.957438939482999851 ) ) ;
#57674 = CARTESIAN_POINT ( 'NONE',  ( -11.44999999999999929, -75.00000000000000000, 0.000000000000000000 ) ) ;
#57675 = EDGE_CURVE ( 'NONE', #34134, #27162, #45375, .T. ) ;
#57676 = CARTESIAN_POINT ( 'NONE',  ( 5.913553462076830414, -77.11893306552236993, -10.46716446491110553 ) ) ;
#57677 = CARTESIAN_POINT ( 'NONE',  ( 7.154950478465999630, -77.02840274250999641, 8.547589380727000474 ) ) ;
#57678 = CARTESIAN_POINT ( 'NONE',  ( 1.223541343054339592, -81.86652669252035253, 0.2554005638053010174 ) ) ;
#57679 = CARTESIAN_POINT ( 'NONE',  ( -0.8896911107955999265, -78.81702590002998932, 1.268128527205000022 ) ) ;
#57680 = DIRECTION ( 'NONE',  ( 0.7071067811865474617, 3.445410891336226740E-11, -0.7071067811865474617 ) ) ;
#57681 = CARTESIAN_POINT ( 'NONE',  ( -7.396918292183181975, -78.44791666666665719, 5.684557159767943624 ) ) ;
#57682 = TOROIDAL_SURFACE ( 'NONE', #9655, 1.250000000000000000, 0.5000000000000000000 ) ;
#57683 = CARTESIAN_POINT ( 'NONE',  ( 8.838834764832000701, -18.75000000000000000, -8.838834764832000701 ) ) ;
#57684 = CARTESIAN_POINT ( 'NONE',  ( -5.040219434754469319, -80.18634211511320586, -9.501857774222978392 ) ) ;
#57685 = CARTESIAN_POINT ( 'NONE',  ( -10.75000000000000000, -77.01041666666665719, -1.407171709420429018 ) ) ;
#57686 = CARTESIAN_POINT ( 'NONE',  ( -9.848035041027015879, -17.17131634292993070, -8.114786739979949814 ) ) ;
#57687 = VECTOR ( 'NONE', #18791, 1000.000000000000000 ) ;
#57688 = VERTEX_POINT ( 'NONE', #14342 ) ;
#57689 = CARTESIAN_POINT ( 'NONE',  ( 4.847151869481000297, -78.84031454048799503, 11.00961342987999991 ) ) ;
#57690 = CARTESIAN_POINT ( 'NONE',  ( -0.6295237254636286695, -81.91666666666665719, 1.092232985442819881 ) ) ;
#57691 = EDGE_CURVE ( 'NONE', #38899, #14050, #17346, .T. ) ;
#57692 = CARTESIAN_POINT ( 'NONE',  ( 10.53539001158999966, -80.04466669503129594, -3.979889026714000355 ) ) ;
#57693 = LINE ( 'NONE', #15597, #6369 ) ;
#57694 = ORIENTED_EDGE ( 'NONE', *, *, #2262, .T. ) ;
#57695 = CARTESIAN_POINT ( 'NONE',  ( 0.2584144827583641502, -25.22845396923335670, 12.70558781487846645 ) ) ;
#57696 = ORIENTED_EDGE ( 'NONE', *, *, #39537, .T. ) ;
#57697 = CARTESIAN_POINT ( 'NONE',  ( 1.750000000001000089, -55.55000001292999912, 12.56594318049000059 ) ) ;
#57698 = ORIENTED_EDGE ( 'NONE', *, *, #43056, .F. ) ;
#57699 = CARTESIAN_POINT ( 'NONE',  ( 2.879448115664242636, -3.500000000000000000, -1.991622112753421714 ) ) ;
#57700 = SURFACE_SIDE_STYLE ('',( #41882 ) ) ;
#57701 = DIRECTION ( 'NONE',  ( 0.000000000000000000, 1.000000000000000000, 0.000000000000000000 ) ) ;
#57702 = CARTESIAN_POINT ( 'NONE',  ( 1.070392484793000198, -79.44059423600799619, 10.86414404906000009 ) ) ;
#57703 = CARTESIAN_POINT ( 'NONE',  ( -0.4701041210472999832, -25.00796934423999929, -12.54901038416000070 ) ) ;
#57704 = CARTESIAN_POINT ( 'NONE',  ( 3.643490673409000014, -82.73863223182399906, -0.2401527247155999800 ) ) ;
#57705 = CARTESIAN_POINT ( 'NONE',  ( -7.140373151351809611, -79.34225595484394944, 6.275840911652932341 ) ) ;
#57706 = ORIENTED_EDGE ( 'NONE', *, *, #47501, .F. ) ;
#57707 = DIRECTION ( 'NONE',  ( -1.000000000000000000, 0.000000000000000000, -1.158066155992000204E-14 ) ) ;
#57708 = CARTESIAN_POINT ( 'NONE',  ( -4.781706919269999467, -78.32610428151998860, 11.04302977649000006 ) ) ;
#57709 = ORIENTED_EDGE ( 'NONE', *, *, #35949, .T. ) ;
#57710 = DIRECTION ( 'NONE',  ( 0.000000000000000000, 1.000000000000000000, 0.000000000000000000 ) ) ;
#57711 = EDGE_CURVE ( 'NONE', #53636, #47936, #48219, .T. ) ;
#57712 = CARTESIAN_POINT ( 'NONE',  ( 1.170174673132000187, -80.01170039560800262, 0.6397400908730001001 ) ) ;
#57713 = DIRECTION ( 'NONE',  ( -1.000000000000000000, 0.000000000000000000, 0.000000000000000000 ) ) ;
#57714 = CARTESIAN_POINT ( 'NONE',  ( 2.694001289665987287, -86.09999999999979536, -3.783547376762387060 ) ) ;
#57715 = CARTESIAN_POINT ( 'NONE',  ( 3.286810233406375126, -85.82387870112127359, 1.426083493365460475 ) ) ;
#57716 = CARTESIAN_POINT ( 'NONE',  ( 11.95031029473000039, -77.78939249822001045, 5.399609419473999417 ) ) ;
#57717 = CARTESIAN_POINT ( 'NONE',  ( -1.251342548660999920, -81.04921328099999300, 0.5102646838515999539 ) ) ;
#57718 = CARTESIAN_POINT ( 'NONE',  ( 0.000000000000000000, -76.08749999999699298, 0.000000000000000000 ) ) ;
#57719 = CARTESIAN_POINT ( 'NONE',  ( -9.219307557399826436, -78.60653449301742057, -0.7524715728064156339 ) ) ;
#57720 = CARTESIAN_POINT ( 'NONE',  ( 6.695659669993999863, -77.19396167140099863, -6.767563488957999418 ) ) ;
#57721 = CARTESIAN_POINT ( 'NONE',  ( -2.046211057035999481, -80.13706584928699783, 3.587692015901000175 ) ) ;
#57722 = CIRCLE ( 'NONE', #22882, 2.799999999999999822 ) ;
#57723 = CARTESIAN_POINT ( 'NONE',  ( 12.56594317823000040, -18.74999998606000062, 1.750000000000000000 ) ) ;
#57724 = CARTESIAN_POINT ( 'NONE',  ( -1.245573248748376605, -3.007515109725281910, 3.001042606595181628 ) ) ;
#57725 = CARTESIAN_POINT ( 'NONE',  ( 2.782570779226999580, -80.73400264934798543, -2.195965310924000047 ) ) ;
#57726 = CARTESIAN_POINT ( 'NONE',  ( -14.00000000000000000, -32.88214388149999934, 0.000000000000000000 ) ) ;
#57727 = CARTESIAN_POINT ( 'NONE',  ( -0.9004183036393477169, -80.98178841101156422, 10.71218087055294532 ) ) ;
#57728 = CARTESIAN_POINT ( 'NONE',  ( 11.22355342542000045, -80.65854382077790774, 0.9700744431168999427 ) ) ;
#57729 = CARTESIAN_POINT ( 'NONE',  ( -2.422546195149999804, -2.177904343863999781, 2.935532677474999907 ) ) ;
#57730 = CARTESIAN_POINT ( 'NONE',  ( -1.193790227340263632, -79.72197934125595964, 0.4455434364240217215 ) ) ;
#57731 = ORIENTED_EDGE ( 'NONE', *, *, #33558, .T. ) ;
#57732 = CARTESIAN_POINT ( 'NONE',  ( -8.596418555780440229, -80.05208333333332860, -6.606377239730328199 ) ) ;
#57733 = CARTESIAN_POINT ( 'NONE',  ( -11.79999999988000070, -18.85000000520999919, -0.5999999998848000171 ) ) ;
#57734 = CARTESIAN_POINT ( 'NONE',  ( -0.8719406389885000497, -81.29017953658200213, -1.009106372638000071 ) ) ;
#57735 = CARTESIAN_POINT ( 'NONE',  ( -8.708326823944164019, -78.93333333333330870, -3.879233584792522116 ) ) ;
#57737 = CARTESIAN_POINT ( 'NONE',  ( 7.411516475408999050, -77.22522017305000475, -10.69619859711000132 ) ) ;
#57736 = B_SPLINE_CURVE_WITH_KNOTS ( 'NONE', 3,
 ( #35025, #48639, #12325, #27051, #31175, #31472, #4640, #4035, #49515, #40652, #8765, #243, #30312, #26184, #22041, #48353, #12889, #7893, #49216 ),
 .UNSPECIFIED., .F., .F.,
 ( 4, 1, 1, 1, 1, 1, 1, 1, 1, 1, 1, 1, 1, 1, 1, 1, 4 ),
 ( 0.000000000000000000, 0.04500688274078824824, 0.1100060414497904537, 0.1750052001587747708, 0.2400043588678306694, 0.3050035175767074613, 0.3700026762857634433, 0.4350018349948194252, 0.5000009937036962171, 0.5650001524127522545, 0.6299993111216289909, 0.6949984698306849173, 0.7599976285397409548, 0.8249967872486176912, 0.8899959459576736176, 0.9549951046667297661, 1.000000000000000000 ),
 .UNSPECIFIED. ) ;
#57738 = CONICAL_SURFACE ( 'NONE', #44550, 13.89999999994999946, 0.7853981633972997312 ) ;
#57739 = CARTESIAN_POINT ( 'NONE',  ( 0.5999999999999999778, -5.000000000000000000, -4.000000000000000000 ) ) ;
#57740 = CARTESIAN_POINT ( 'NONE',  ( 5.038785450664000187, -76.65236125213000662, -11.45299339640000014 ) ) ;
#57741 = ORIENTED_EDGE ( 'NONE', *, *, #22266, .F. ) ;
#57742 = TOROIDAL_SURFACE ( 'NONE', #29461, 1.250000000000000000, 0.5000000000000000000 ) ;
#57743 = B_SPLINE_CURVE_WITH_KNOTS ( 'NONE', 3,
 ( #35289, #8161, #58337, #53319, #35888, #8441 ),
 .UNSPECIFIED., .F., .F.,
 ( 4, 2, 4 ),
 ( 0.000000000000000000, 0.5000000000000000000, 1.000000000000000000 ),
 .UNSPECIFIED. ) ;
#57744 = EDGE_CURVE ( 'NONE', #11731, #45320, #2935, .T. ) ;
#57745 = CARTESIAN_POINT ( 'NONE',  ( 0.000000000000000000, -18.84999999999999787, 12.00000000000000000 ) ) ;
#57746 = ADVANCED_FACE ( 'NONE', ( #35904 ), #53631, .T. ) ;
#57747 = CARTESIAN_POINT ( 'NONE',  ( 12.44210192982000152, -60.88432059783999506, 1.464837683472000052 ) ) ;
#57748 = CARTESIAN_POINT ( 'NONE',  ( -1.799501877760999902, -23.28917565320000094, -12.60552522436000089 ) ) ;
#57749 = CARTESIAN_POINT ( 'NONE',  ( -3.877711979005999954, -77.98508576487398614, -8.815699619024998768 ) ) ;
#57750 = CARTESIAN_POINT ( 'NONE',  ( 3.044567270945999660, -84.14231094026499136, 2.853188146245999590 ) ) ;
#57751 = CARTESIAN_POINT ( 'NONE',  ( -1.347939806071310143, -79.98541859949588684, 10.66559394157654950 ) ) ;
#57752 = CARTESIAN_POINT ( 'NONE',  ( -1.402375016663000018, -80.09094972420699321, 0.2083355298385999865 ) ) ;
#57753 = EDGE_LOOP ( 'NONE', ( #3268, #44648, #53286, #8706, #809 ) ) ;
#57754 = CARTESIAN_POINT ( 'NONE',  ( -4.478752552746194660, -77.19081009185403275, -9.773648971711729416 ) ) ;
#57755 = CARTESIAN_POINT ( 'NONE',  ( 5.539808784079872872, -78.86666666666668846, -9.611650271896849063 ) ) ;
#57756 = CARTESIAN_POINT ( 'NONE',  ( -3.485499217012028694, -78.91452042059381711, 6.970998434024015644 ) ) ;
#57757 = ORIENTED_EDGE ( 'NONE', *, *, #11136, .F. ) ;
#57758 = EDGE_LOOP ( 'NONE', ( #32700, #30815, #39829, #41880 ) ) ;
#57759 = CARTESIAN_POINT ( 'NONE',  ( -5.736605348686000028, -78.28973750712998481, 9.315534093342000332 ) ) ;
#57760 = DIRECTION ( 'NONE',  ( 0.000000000000000000, 1.000000000000000000, 0.000000000000000000 ) ) ;
#57761 = ADVANCED_FACE ( 'NONE', ( #14057 ), #8570, .T. ) ;
#57762 = CARTESIAN_POINT ( 'NONE',  ( 10.49379773601000032, -80.14957387780098941, 3.966822966890999780 ) ) ;
#57763 = EDGE_LOOP ( 'NONE', ( #24617, #24607, #44423, #4644 ) ) ;
#57764 = CARTESIAN_POINT ( 'NONE',  ( -12.11185258877999971, -77.76629135392300896, -1.133824260204999934 ) ) ;
#57765 = CIRCLE ( 'NONE', #43621, 12.50000000000000000 ) ;
#57766 = VERTEX_POINT ( 'NONE', #49506 ) ;
#57767 = ORIENTED_EDGE ( 'NONE', *, *, #6153, .F. ) ;
#57768 = AXIS2_PLACEMENT_3D ( 'NONE', #25917, #48097, #39204 ) ;
#57769 = CARTESIAN_POINT ( 'NONE',  ( 9.799999999999998934, -92.13603921945998820, -1.131976457013999809E-12 ) ) ;
#57770 = FACE_OUTER_BOUND ( 'NONE', #58299, .T. ) ;
#57771 = B_SPLINE_SURFACE_WITH_KNOTS ( 'NONE', 3, 3, ( 
 ( #24890, #3041, #33737, #52627 ),
 ( #47932, #20469, #11324, #2749 ),
 ( #29302, #12182, #38463, #6881 ),
 ( #56479, #39040, #30167, #48216 ),
 ( #7748, #56768, #34310, #52343 ),
 ( #11897, #45521, #13914, #31316 ),
 ( #35163, #49360, #57911, #53485 ),
 ( #49950, #54079, #54375, #27479 ),
 ( #31907, #5067, #49655, #9495 ),
 ( #8611, #4484, #23063, #13026 ),
 ( #31615, #35756, #3887, #40491 ) ),
 .UNSPECIFIED., .F., .F., .F.,
 ( 4, 1, 1, 1, 1, 1, 1, 1, 4 ),
 ( 4, 4 ),
 ( -0.02001474922154999891, 0.000000000000000000, 0.1666666666667000196, 0.3333333333333000081, 0.5000000000000000000, 0.6666666666667000474, 0.8333333333333000637, 1.000000000000000000, 1.020283381528000133 ),
 ( -0.3582002740325999635, 1.358862457854000061 ),
 .UNSPECIFIED. ) ;
#57772 = EDGE_LOOP ( 'NONE', ( #32458, #4780, #18853, #31924 ) ) ;
#57773 = CARTESIAN_POINT ( 'NONE',  ( -0.1961711567845059734, -81.78556630387674886, 1.499955683888876123 ) ) ;
#57774 = VERTEX_POINT ( 'NONE', #54224 ) ;
#57775 = CARTESIAN_POINT ( 'NONE',  ( 1.164640101142631723, -79.93981338681913940, 0.6367143138937826352 ) ) ;
#57776 = CARTESIAN_POINT ( 'NONE',  ( -0.03689308533088261205, -78.91452044229970397, -3.914326904521404860 ) ) ;
#57777 = CIRCLE ( 'NONE', #37050, 1.749999999999997558 ) ;
#57778 = CARTESIAN_POINT ( 'NONE',  ( 7.765024210398999926, -54.70905971351000119, 9.830784063398999351 ) ) ;
#57779 = DIRECTION ( 'NONE',  ( -0.7071067811865475727, 0.000000000000000000, 0.7071067811865475727 ) ) ;
#57780 = CARTESIAN_POINT ( 'NONE',  ( 1.500000000000000000, -81.75000000000000000, 0.000000000000000000 ) ) ;
#57781 = AXIS2_PLACEMENT_3D ( 'NONE', #5839, #23272, #13821 ) ;
#57782 = CARTESIAN_POINT ( 'NONE',  ( 11.06070397063424693, -80.58681085545528333, -1.829055307137330111 ) ) ;
#57783 = CARTESIAN_POINT ( 'NONE',  ( 7.682331425181999407, -56.03513569577999931, -10.04115011118999945 ) ) ;
#57784 = CARTESIAN_POINT ( 'NONE',  ( 7.000000000000000000, -81.19999999999998863, 0.000000000000000000 ) ) ;
#57785 = CARTESIAN_POINT ( 'NONE',  ( -9.038948602518001252, -25.33262223864999640, 9.029786144013998594 ) ) ;
#57786 = CARTESIAN_POINT ( 'NONE',  ( -1.199500263597270244, -79.95208333333334849, -0.9218200799623728070 ) ) ;
#57787 = CARTESIAN_POINT ( 'NONE',  ( -3.741267609786000481, -80.32205496681199008, -1.847424956918999772 ) ) ;
#57788 = EDGE_CURVE ( 'NONE', #3286, #29384, #45669, .T. ) ;
#57789 = CARTESIAN_POINT ( 'NONE',  ( 1.877525114294000153, -77.11648667140100599, 9.580448975616000951 ) ) ;
#57790 = LINE ( 'NONE', #53360, #55894 ) ;
#57791 = CARTESIAN_POINT ( 'NONE',  ( -5.539808784079933268, -78.01666666666665151, 9.611650271896811759 ) ) ;
#57792 = CARTESIAN_POINT ( 'NONE',  ( -11.94395460750000204, -76.97963095766999686, 2.857367593729999822 ) ) ;
#57793 = CARTESIAN_POINT ( 'NONE',  ( 11.59999999999999964, -90.29999999999999716, 0.000000000000000000 ) ) ;
#57794 = CARTESIAN_POINT ( 'NONE',  ( -3.682737394452999968, -1.757324315393999914, 1.849092470328999926 ) ) ;
#57795 = CARTESIAN_POINT ( 'NONE',  ( -6.090475762158000350, -79.58000095943376095, 7.362120511650999788 ) ) ;
#57796 = CARTESIAN_POINT ( 'NONE',  ( -0.2603338869383251541, -80.96066229293080596, -1.489115581560273460 ) ) ;
#57797 = CARTESIAN_POINT ( 'NONE',  ( 12.77649794763000024, -62.10831393445000259, 0.06464137375187999079 ) ) ;
#57798 = CARTESIAN_POINT ( 'NONE',  ( -1.107979503908000041, -78.47287816700719532, -1.174561767264999945 ) ) ;
#57799 = FACE_OUTER_BOUND ( 'NONE', #29730, .T. ) ;
#57800 = CARTESIAN_POINT ( 'NONE',  ( -10.57583826563999985, -77.04653003390299659, -2.706834349011999930 ) ) ;
#57801 = CARTESIAN_POINT ( 'NONE',  ( -12.03507225495000199, -78.35749258035299647, 2.439839133843999974 ) ) ;
#57802 = CARTESIAN_POINT ( 'NONE',  ( -0.9218200799623775810, -80.92708333333335702, 1.199500263597266247 ) ) ;
#57804 = CARTESIAN_POINT ( 'NONE',  ( 0.000000000000000000, -80.99999999999998579, -7.000000000000000000 ) ) ;
#57803 = DIRECTION ( 'NONE',  ( -0.9999999923520045408, 0.000000000000000000, -0.0001236769620547006605 ) ) ;
#57805 = CARTESIAN_POINT ( 'NONE',  ( 1.385204701026000018, -82.86641278936299670, -0.4875042294149000144 ) ) ;
#57806 = CARTESIAN_POINT ( 'NONE',  ( -3.736121491853147791, -79.50337531813939052, 10.07978767405712617 ) ) ;
#57807 = VERTEX_POINT ( 'NONE', #51551 ) ;
#57808 = CARTESIAN_POINT ( 'NONE',  ( -10.53003223724000037, -18.67547470641000018, -7.612971414716000140 ) ) ;
#57809 = VECTOR ( 'NONE', #58386, 1000.000000000000000 ) ;
#57810 = CARTESIAN_POINT ( 'NONE',  ( -5.602477186682999211, -79.77762550192599633, -10.65853832389000111 ) ) ;
#57811 = CARTESIAN_POINT ( 'NONE',  ( -11.16943811108000162, -80.64298588867529816, -0.2596301638153999947 ) ) ;
#57812 = EDGE_CURVE ( 'NONE', #40525, #30548, #49121, .T. ) ;
#57813 = CARTESIAN_POINT ( 'NONE',  ( 0.000000000000000000, -76.00000000000000000, 0.000000000000000000 ) ) ;
#57814 = CARTESIAN_POINT ( 'NONE',  ( -10.18127202940000053, -60.18645218919000683, 7.633406483317000557 ) ) ;
#57815 = CARTESIAN_POINT ( 'NONE',  ( -3.246123984833999998, -1.511824315393999862, 1.406516975900000022 ) ) ;
#57816 = CARTESIAN_POINT ( 'NONE',  ( -4.131840341030999397, -80.11747182528499422, 8.602031057089000399 ) ) ;
#57817 = CARTESIAN_POINT ( 'NONE',  ( 10.12290050255000118, -60.04999997790999799, -7.648026768390999486 ) ) ;
#57818 = CARTESIAN_POINT ( 'NONE',  ( -2.062597265787999845, -56.01538333533000014, 12.87024489158000051 ) ) ;
#57819 = ORIENTED_EDGE ( 'NONE', *, *, #46462, .F. ) ;
#57820 = CONICAL_SURFACE ( 'NONE', #25761, 13.94999999997000018, 0.7853981633972997312 ) ;
#57821 = CARTESIAN_POINT ( 'NONE',  ( 9.369164850722000892, -18.75000000000000000, 7.601397897754999633 ) ) ;
#57822 = CARTESIAN_POINT ( 'NONE',  ( 8.441176281578332663, -24.91652561799148913, -9.243148034841571103 ) ) ;
#57823 = CARTESIAN_POINT ( 'NONE',  ( -12.50239399164999909, -17.31640749886000208, 1.003653729363000124 ) ) ;
#57824 = AXIS2_PLACEMENT_3D ( 'NONE', #44537, #48122, #25653 ) ;
#57825 = CARTESIAN_POINT ( 'NONE',  ( -10.24998526315000014, -58.55083378327000077, -7.705142895592000052 ) ) ;
#57826 = CARTESIAN_POINT ( 'NONE',  ( 2.588536891983000299, -84.11092953870900146, 2.425701832561999893 ) ) ;
#57827 = EDGE_CURVE ( 'NONE', #1239, #29230, #55431, .T. ) ;
#57828 = ORIENTED_EDGE ( 'NONE', *, *, #6097, .T. ) ;
#57829 = FACE_OUTER_BOUND ( 'NONE', #52481, .T. ) ;
#57830 = CARTESIAN_POINT ( 'NONE',  ( -9.397034021637606926, -77.75095410432449228, -7.223315580355283316 ) ) ;
#57831 = CARTESIAN_POINT ( 'NONE',  ( -1.733997378016417734, -55.27616783188626925, -12.54437956609219640 ) ) ;
#57832 = ADVANCED_FACE ( 'NONE', ( #19960 ), #51960, .F. ) ;
#57833 = ORIENTED_EDGE ( 'NONE', *, *, #57788, .F. ) ;
#57834 = B_SPLINE_CURVE_WITH_KNOTS ( 'NONE', 3,
 ( #9699, #45433, #4975, #22390, #26806, #5267, #9116, #40401, #23276, #4390, #50445, #49569, #58112, #13825, #49865, #27102, #17675, #18851 ),
 .UNSPECIFIED., .F., .F.,
 ( 4, 2, 2, 2, 2, 2, 2, 2, 4 ),
 ( 0.000000000000000000, 0.1250000000000000000, 0.2500000000000000000, 0.3750000000000000000, 0.5000000000000000000, 0.6250000000000000000, 0.7500000000000000000, 0.8750000000000000000, 1.000000000000000000 ),
 .UNSPECIFIED. ) ;
#57835 = CARTESIAN_POINT ( 'NONE',  ( -8.798041828522000785, -53.86186490677999927, -8.790609562984000647 ) ) ;
#57836 = CARTESIAN_POINT ( 'NONE',  ( 5.496668217546000434, -79.94241373670298856, -8.073860231047000013 ) ) ;
#57837 = VERTEX_POINT ( 'NONE', #11394 ) ;
#57838 = ORIENTED_EDGE ( 'NONE', *, *, #13535, .F. ) ;
#57839 = CARTESIAN_POINT ( 'NONE',  ( 8.104433285180000723, -76.94079223774500065, 9.165435814006000825 ) ) ;
#57840 = DIRECTION ( 'NONE',  ( 0.000000000000000000, -1.000000000000000000, 0.000000000000000000 ) ) ;
#57841 = EDGE_LOOP ( 'NONE', ( #14922, #17627, #57343, #56035, #14933, #3876, #57267 ) ) ;
#57842 = CARTESIAN_POINT ( 'NONE',  ( -7.591316436381999821, -77.24143084965399453, -5.703451837412999659 ) ) ;
#57843 = CARTESIAN_POINT ( 'NONE',  ( -5.351380825403158958, -77.77138628471922743, 8.095464844688041950 ) ) ;
#57844 = EDGE_CURVE ( 'NONE', #8174, #23335, #32125, .T. ) ;
#57845 = CARTESIAN_POINT ( 'NONE',  ( 1.160010371456533518, -80.31977958019837160, -0.4654735999135473090 ) ) ;
#57846 = CARTESIAN_POINT ( 'NONE',  ( -13.07887593023000150, -78.00016851287999486, -0.9532572298037998992 ) ) ;
#57847 = CARTESIAN_POINT ( 'NONE',  ( -10.58728162385000005, -77.72321182651586469, 3.705074683290000337 ) ) ;
#57848 = CARTESIAN_POINT ( 'NONE',  ( 0.000000000000000000, -15.69705297114000331, 12.53545825868000207 ) ) ;
#57849 = B_SPLINE_CURVE_WITH_KNOTS ( 'NONE', 3,
 ( #38074, #6489, #37782, #55803, #15354, #33348, #51380, #8220, #48111, #26221, #20932, #30350, #40086, #53097, #4077, #57519, #3227, #25643 ),
 .UNSPECIFIED., .F., .F.,
 ( 4, 2, 2, 2, 2, 2, 2, 2, 4 ),
 ( 0.000000000000000000, 0.1250000000000000833, 0.2500000000000001110, 0.3750000000000000000, 0.4999999999999999445, 0.6249999999999998890, 0.7499999999999997780, 0.8749999999999998890, 1.000000000000000000 ),
 .UNSPECIFIED. ) ;
#57850 = CARTESIAN_POINT ( 'NONE',  ( 3.184161977317844894, -86.31452042059399332, -1.417680250971349754 ) ) ;
#57851 = AXIS2_PLACEMENT_3D ( 'NONE', #20472, #11900, #34313 ) ;
#57852 = CARTESIAN_POINT ( 'NONE',  ( 3.371435477143000181, -79.55097691852699882, -10.69820234502000034 ) ) ;
#57853 = CARTESIAN_POINT ( 'NONE',  ( 0.2479736929933408496, -79.97326530669452893, 9.253379769800089250 ) ) ;
#57854 = CARTESIAN_POINT ( 'NONE',  ( 9.848035041034458814, -17.17131634295486720, 8.114786739975425434 ) ) ;
#57855 = ORIENTED_EDGE ( 'NONE', *, *, #25244, .T. ) ;
#57856 = CARTESIAN_POINT ( 'NONE',  ( -10.07307375010999984, -79.15776930244898324, -5.046000355766999235 ) ) ;
#57857 = CARTESIAN_POINT ( 'NONE',  ( 12.17088485526999975, -75.77930627215999948, 1.845041276493999849 ) ) ;
#57858 = CARTESIAN_POINT ( 'NONE',  ( 1.413837046361000160, -79.54138868576299615, -0.1054710693050000120 ) ) ;
#57860 = EDGE_CURVE ( 'NONE', #42268, #13828, #14216, .T. ) ;
#57859 = CARTESIAN_POINT ( 'NONE',  ( 0.1427930653877000078, -78.02442767348290431, 1.311554697429999861 ) ) ;
#57861 = CIRCLE ( 'NONE', #53147, 9.950000000000001066 ) ;
#57862 = CARTESIAN_POINT ( 'NONE',  ( 1.711446453831659831, -3.183809200564340802, 3.074675725082612221 ) ) ;
#57863 = CARTESIAN_POINT ( 'NONE',  ( 9.500000000000000000, -77.04999999999999716, 0.000000000000000000 ) ) ;
#57864 = CARTESIAN_POINT ( 'NONE',  ( -12.69619287815999975, -20.24916621771999914, -1.799475295154000065 ) ) ;
#57865 = CARTESIAN_POINT ( 'NONE',  ( -8.385799987731649807, -61.68809827200743712, -9.298537617325708382 ) ) ;
#57866 = ADVANCED_FACE ( 'NONE', ( #37363 ), #33516, .F. ) ;
#57867 = CARTESIAN_POINT ( 'NONE',  ( -2.205131412320000095, -78.44776941201399723, 10.93750404997000025 ) ) ;
#57868 = CARTESIAN_POINT ( 'NONE',  ( -9.734394856890000725, -77.37743998579799154, 0.2324636006574999636 ) ) ;
#57869 = CARTESIAN_POINT ( 'NONE',  ( 10.04116292118000153, -19.23537109840999904, -7.682344222590000271 ) ) ;
#57870 = CARTESIAN_POINT ( 'NONE',  ( -0.6663465976954637826, -83.01994639268885123, 1.061158757155598042 ) ) ;
#57871 = CARTESIAN_POINT ( 'NONE',  ( 11.21485848424000054, -79.99849401882083555, -0.2123177049684000228 ) ) ;
#57872 = ORIENTED_EDGE ( 'NONE', *, *, #1402, .F. ) ;
#57873 = CARTESIAN_POINT ( 'NONE',  ( 0.7887820451556000201, -81.72691005693999955, 1.375581554690999964 ) ) ;
#57874 = CARTESIAN_POINT ( 'NONE',  ( 1.511505244404999893, -80.66777860354999063, 0.4793209935110999687 ) ) ;
#57875 = CARTESIAN_POINT ( 'NONE',  ( 4.000000000000000000, -75.00000000000001421, -0.5999999999999999778 ) ) ;
#57876 = CARTESIAN_POINT ( 'NONE',  ( 0.4844284812283000119, -77.37009841468399429, 11.97002061314999999 ) ) ;
#57877 = CARTESIAN_POINT ( 'NONE',  ( -10.75000000000000000, -78.10000000000000853, 0.000000000000000000 ) ) ;
#57878 = CARTESIAN_POINT ( 'NONE',  ( 0.6304340365998000184, -82.55529135728299650, 1.542015542100000136 ) ) ;
#57879 = CARTESIAN_POINT ( 'NONE',  ( 2.945718361321999712, -78.93144108438299611, 11.40680644849000025 ) ) ;
#57880 = CARTESIAN_POINT ( 'NONE',  ( -5.764562846862999912, -79.05555194988498613, 7.830301022820999712 ) ) ;
#57881 = CARTESIAN_POINT ( 'NONE',  ( -8.954089450906998593, -78.73694786691399372, -3.546476007522999740 ) ) ;
#57882 = CARTESIAN_POINT ( 'NONE',  ( 0.5045596072233999863, -53.66471086928999767, -12.66210649705999991 ) ) ;
#57883 = CARTESIAN_POINT ( 'NONE',  ( 10.85853326491538162, -75.98070578024562849, 4.488588818805364866 ) ) ;
#57884 = CARTESIAN_POINT ( 'NONE',  ( -3.605449341531122176, -85.88547955769999476, 1.524483932633625027 ) ) ;
#57885 = ORIENTED_EDGE ( 'NONE', *, *, #11660, .F. ) ;
#57886 = CARTESIAN_POINT ( 'NONE',  ( 2.078959492154019983, -78.15749999999999886, 9.312872062229846648 ) ) ;
#57887 = CARTESIAN_POINT ( 'NONE',  ( 10.42531125070999920, -60.06485145371000556, -7.624341767111000756 ) ) ;
#57888 = CARTESIAN_POINT ( 'NONE',  ( -3.643839868884810151, -78.79973254024228879, -11.20904019331054258 ) ) ;
#57889 = TOROIDAL_SURFACE ( 'NONE', #32420, 1.250000000000000000, 0.5000000000000000000 ) ;
#57890 = CARTESIAN_POINT ( 'NONE',  ( 2.318769295210185710, -78.62148118236265759, -4.014936526035610243 ) ) ;
#57891 = CARTESIAN_POINT ( 'NONE',  ( -1.552248384014999871, -82.80004243524099650, 0.6048007385293000526 ) ) ;
#57892 = CARTESIAN_POINT ( 'NONE',  ( -10.90760146693999921, -78.93901479977699864, -1.219937219691999974 ) ) ;
#57893 = CARTESIAN_POINT ( 'NONE',  ( -1.779623408249566774, -17.86369130975115738, 12.71471627657126291 ) ) ;
#57894 = CARTESIAN_POINT ( 'NONE',  ( 6.027877668513000664, -76.10658001266899930, -10.82135396111999981 ) ) ;
#57895 = DIRECTION ( 'NONE',  ( 0.000000000000000000, -1.000000000000000000, 0.000000000000000000 ) ) ;
#57896 = CARTESIAN_POINT ( 'NONE',  ( 0.000000000000000000, -92.39999999999999147, 0.000000000000000000 ) ) ;
#57897 = VERTEX_POINT ( 'NONE', #29089 ) ;
#57898 = CARTESIAN_POINT ( 'NONE',  ( -9.575027280576000166, -79.09977615539300189, 5.479104576271000226 ) ) ;
#57899 = CARTESIAN_POINT ( 'NONE',  ( -0.01465444447223758842, -79.97640258770987032, 1.249640596461801145 ) ) ;
#57900 = CARTESIAN_POINT ( 'NONE',  ( 11.00000000000000178, -77.94292008887532575, -0.9786566581934403874 ) ) ;
#57901 = B_SPLINE_CURVE_WITH_KNOTS ( 'NONE', 3,
 ( #41941, #6797, #20378, #15945, #24222, #33933 ),
 .UNSPECIFIED., .F., .F.,
 ( 4, 2, 4 ),
 ( 0.000000000000000000, 0.1428612160184655755, 0.2857224320369311510 ),
 .UNSPECIFIED. ) ;
#57902 = AXIS2_PLACEMENT_3D ( 'NONE', #52755, #21163, #33861 ) ;
#57903 = B_SPLINE_SURFACE_WITH_KNOTS ( 'NONE', 3, 3, ( 
 ( #30770, #15846, #48803, #6984, #28824, #6697, #46873, #48518, #15260, #2283, #12774, #39642, #19694, #57370, #15555, #6400, #29119, #8349, #20279, #56005, #24415, #8063, #38272, #33548, #26347, #12492, #57650, #24705, #37981, #26058, #44084, #47165, #2000, #44364, #56293 ),
 ( #3635, #33834, #51587, #37694, #30490, #17206, #42717, #11145, #21638, #35194, #51872, #19994, #55713, #11426, #51294, #29406, #10851, #42431, #47459, #24988, #16929, #43008, #2565, #20566, #38564, #34910, #52942, #27804, #4807, #45260, #54406, #22808, #13651, #36380, #39928 ),
 ( #36093, #40226, #13944, #31940, #3917, #35787, #13354, #57944, #40819, #26929, #49984, #58238, #17498, #700, #49092, #18682, #14231, #27513, #49393, #36674, #35486, #23099, #17801, #27221, #53516, #53817, #5100, #411, #54690, #13057, #31352, #18097, #32230, #26629, #8942 ),
 ( #41109, #44960, #4515, #45554, #18389, #31056, #50272, #9527, #9820, #49689, #54110, #21920, #119, #8644, #31646, #44664, #22516, #4218, #22215, #40526, #9235, #18970, #28386, #10115, #11282, #28095, #23678, #23391, #20140, #46144, #19846, #46434, #42283, #24558, #33693 ) ),
 .UNSPECIFIED., .F., .F., .F.,
 ( 4, 4 ),
 ( 4, 1, 1, 1, 1, 1, 1, 1, 1, 1, 1, 1, 1, 1, 1, 1, 1, 1, 1, 1, 1, 1, 1, 1, 1, 1, 1, 1, 1, 1, 1, 1, 4 ),
 ( -0.1772706441294000235, 1.177270644128999955 ),
 ( 0.3465776244131999473, 0.3673974550078999979, 0.3882172856025000174, 0.4090371161971999570, 0.4298569467919000076, 0.4506767773865999471, 0.4714966079812999977, 0.4923164385759000172, 0.5131362691705999568, 0.5339560997653000074, 0.5547759303600000580, 0.5755957609545999665, 0.5964155915493000171, 0.6172354221440000677, 0.6380552527387000072, 0.6588750833333999468, 0.6796949139279999663, 0.7005147445227000169, 0.7213345751173999565, 0.7421544057121000071, 0.7629742363067000266, 0.7837940669013999662, 0.8046138974961000168, 0.8254337280908000674, 0.8462535586855000069, 0.8670733892801000264, 0.8878932198747999660, 0.9087130504695000166, 0.9295328810641999562, 0.9503527116587999757, 0.9711725422535000263, 0.9919923728481999659, 1.012812203443000048 ),
 .UNSPECIFIED. ) ;
#57904 = CARTESIAN_POINT ( 'NONE',  ( 10.89322882296999850, -79.51041903353198848, 2.414366480783999958 ) ) ;
#57905 = LINE ( 'NONE', #21882, #3419 ) ;
#57906 = DIRECTION ( 'NONE',  ( -3.788556036780999566E-11, -1.000000000000000000, 0.000000000000000000 ) ) ;
#57907 = CARTESIAN_POINT ( 'NONE',  ( 7.091067894987999942, -79.00057898155800729, -10.02559399679999963 ) ) ;
#57908 = CARTESIAN_POINT ( 'NONE',  ( -7.712209501855907590, -54.73822238195494805, 10.27335463208971866 ) ) ;
#57909 = DIRECTION ( 'NONE',  ( 1.000000000000000000, 0.000000000000000000, 0.000000000000000000 ) ) ;
#57910 = DIRECTION ( 'NONE',  ( -1.000000000000000000, 0.000000000000000000, 0.000000000000000000 ) ) ;
#57911 = CARTESIAN_POINT ( 'NONE',  ( -12.54673349184999864, -24.82806887810999896, 0.9076721992841999542 ) ) ;
#57912 = VERTEX_POINT ( 'NONE', #23497 ) ;
#57913 = ORIENTED_EDGE ( 'NONE', *, *, #7840, .T. ) ;
#57914 = DIRECTION ( 'NONE',  ( 0.000000000000000000, 0.000000000000000000, -1.000000000000000000 ) ) ;
#57915 = CARTESIAN_POINT ( 'NONE',  ( 7.488372721267999133, -77.82613998579800807, -5.914808301684000291 ) ) ;
#57916 = ORIENTED_EDGE ( 'NONE', *, *, #3159, .T. ) ;
#57917 = DIRECTION ( 'NONE',  ( 0.000000000000000000, -1.000000000000000000, 0.000000000000000000 ) ) ;
#57918 = ORIENTED_EDGE ( 'NONE', *, *, #28354, .T. ) ;
#57919 = CARTESIAN_POINT ( 'NONE',  ( 9.643350356168998161, -24.94034317039000115, 8.260133465584999612 ) ) ;
#57920 = CARTESIAN_POINT ( 'NONE',  ( 5.066356038949999530, -77.47816619513099567, 9.799682181994000985 ) ) ;
#57921 = ADVANCED_FACE ( 'NONE', ( #10222 ), #50964, .F. ) ;
#57922 = CARTESIAN_POINT ( 'NONE',  ( -0.1638756991376206507, -82.48607747092580667, 1.249557844123856398 ) ) ;
#57923 = ADVANCED_FACE ( 'NONE', ( #24672 ), #29306, .F. ) ;
#57924 = CARTESIAN_POINT ( 'NONE',  ( -5.860166239445133485, -78.17045350272391602, -7.156831644022663141 ) ) ;
#57925 = CARTESIAN_POINT ( 'NONE',  ( 9.453938376997999882, -78.99353879967499381, 6.036651369377000087 ) ) ;
#57926 = CARTESIAN_POINT ( 'NONE',  ( -1.170441605159127318, -79.57192497548669508, 0.4385201796425973741 ) ) ;
#57927 = VECTOR ( 'NONE', #33252, 1000.000000000000000 ) ;
#57928 = ORIENTED_EDGE ( 'NONE', *, *, #47997, .F. ) ;
#57929 = EDGE_LOOP ( 'NONE', ( #29729, #47337, #12832, #40933 ) ) ;
#57930 = B_SPLINE_CURVE_WITH_KNOTS ( 'NONE', 3,
 ( #43347, #43067, #3762, #53353, #25330, #35035, #30033, #52495, #39768, #25044, #8193, #16198, #56639, #3200, #47796, #48649, #43928, #57782, #2625, #38623, #39192, #43641, #26196, #34176, #12900, #25618, #2904, #7617, #20904, #47518, #17336, #52781, #12335, #29744, #52212 ),
 .UNSPECIFIED., .F., .F.,
 ( 4, 1, 1, 1, 1, 1, 1, 1, 1, 1, 1, 1, 1, 1, 1, 1, 1, 1, 1, 1, 1, 1, 1, 1, 1, 1, 1, 1, 1, 1, 1, 1, 4 ),
 ( 0.000000000000000000, 0.01250051965580525719, 0.04500048563628020193, 0.07750045161695787166, 0.1100004175974328147, 0.1425003835781102624, 0.1750003495585852054, 0.2075003155390599263, 0.2400002815197375960, 0.2725002475002122893, 0.3050002134806872323, 0.3375001794613649020, 0.3700001454418396230, 0.4025001114225172927, 0.4350000774029922357, 0.4675000433834667346, 0.5000000093641446819, 0.5324999753446193473, 0.5649999413252972946, 0.5974999073057719601, 0.6299998732862467365, 0.6624998392669243508, 0.6949998052473993493, 0.7274997712280767415, 0.7599997372085517400, 0.7924997031890266275, 0.8249996691697041307, 0.8574996351501790182, 0.8899996011308567434, 0.9224995671113316309, 0.9549995330918061853, 0.9874994990724837995, 1.000000000000000000 ),
 .UNSPECIFIED. ) ;
#57931 = CARTESIAN_POINT ( 'NONE',  ( 1.731393780109722336, -77.46006980321932645, 9.086687499499138454 ) ) ;
#57932 = CARTESIAN_POINT ( 'NONE',  ( -11.00724581733999941, -77.80340341412998839, 0.8512868710715000287 ) ) ;
#57933 = CARTESIAN_POINT ( 'NONE',  ( -7.596835002782708735, -77.45208333333332007, -5.838193839761694370 ) ) ;
#57934 = CARTESIAN_POINT ( 'NONE',  ( 3.585273492103000059, -75.68288930031000916, 11.57765943471000014 ) ) ;
#57935 = CARTESIAN_POINT ( 'NONE',  ( -9.242397610492675497, -79.41824321304214607, -2.209549243808804686 ) ) ;
#57936 = CARTESIAN_POINT ( 'NONE',  ( 0.4192948356380000186, -79.35872016573999588, -1.440205485619000081 ) ) ;
#57937 = CARTESIAN_POINT ( 'NONE',  ( 10.52776997023000050, -80.14860880379099228, 3.979665013433000720 ) ) ;
#57938 = EDGE_CURVE ( 'NONE', #23344, #50686, #26465, .T. ) ;
#57939 = CARTESIAN_POINT ( 'NONE',  ( 12.49837451347000084, -18.79042109296999641, -1.667049596275999912 ) ) ;
#57940 = AXIS2_PLACEMENT_3D ( 'NONE', #31092, #448, #44997 ) ;
#57941 = CARTESIAN_POINT ( 'NONE',  ( -0.3271848554490991434, -78.10416666666665719, -1.217465845835395299 ) ) ;
#57942 = CARTESIAN_POINT ( 'NONE',  ( 9.250000000000001776, -78.73958333333334281, -1.210822168571047186 ) ) ;
#57943 = ORIENTED_EDGE ( 'NONE', *, *, #49091, .F. ) ;
#57944 = CARTESIAN_POINT ( 'NONE',  ( 10.99809925207999939, -79.65397460938399377, -5.545072090542999987 ) ) ;
#57945 = CARTESIAN_POINT ( 'NONE',  ( -7.647094085174999556, -55.43104695408000282, 10.00844048069000003 ) ) ;
#57946 = CARTESIAN_POINT ( 'NONE',  ( -7.077166588276162962, -78.03223210419182010, 8.091922746255471921 ) ) ;
#57947 = CARTESIAN_POINT ( 'NONE',  ( -10.26943924278000075, -78.59084813818699899, 6.168847710360999770 ) ) ;
#57948 = CARTESIAN_POINT ( 'NONE',  ( -8.652389292596000203, -16.73734871878000163, -9.414476472810001439 ) ) ;
#57950 = CARTESIAN_POINT ( 'NONE',  ( -1.389926494651000155, -17.37618663744999736, -12.65988803923000106 ) ) ;
#57949 = CARTESIAN_POINT ( 'NONE',  ( 7.682344222575999915, -56.03537109808000594, 10.04116292115999975 ) ) ;
#57951 = DIRECTION ( 'NONE',  ( 0.7071067811865475727, 0.000000000000000000, 0.7071067811865475727 ) ) ;
#57952 = CARTESIAN_POINT ( 'NONE',  ( 10.42274798266000069, -57.04634220890999785, -7.691916945423999508 ) ) ;
#57953 = DIRECTION ( 'NONE',  ( 0.000000000000000000, 1.000000000000000000, 0.000000000000000000 ) ) ;
#57954 = CARTESIAN_POINT ( 'NONE',  ( -2.318770996637999904, -77.71491181672199389, 11.02076520135999971 ) ) ;
#57955 = CARTESIAN_POINT ( 'NONE',  ( -12.00000000000000000, -78.29999999999999716, 0.000000000000000000 ) ) ;
#57956 = CARTESIAN_POINT ( 'NONE',  ( -10.82155256717999947, -80.34558659221879395, -3.096403820615999614 ) ) ;
#57957 = EDGE_LOOP ( 'NONE', ( #23278, #51500, #42299, #36859, #10090, #50966, #57698, #12103, #54095, #22923, #22411, #48736 ) ) ;
#57958 = CARTESIAN_POINT ( 'NONE',  ( 0.4255534434941637967, -1.466224065903919183, 3.247433857139228053 ) ) ;
#57959 = ADVANCED_FACE ( 'NONE', ( #41510 ), #38754, .F. ) ;
#57960 = CARTESIAN_POINT ( 'NONE',  ( -1.288488638075999893, -54.26435060599999360, 12.54709296479000002 ) ) ;
#57961 = CARTESIAN_POINT ( 'NONE',  ( 8.500000000000000000, -5.000000000000000000, 0.000000000000000000 ) ) ;
#57962 = CARTESIAN_POINT ( 'NONE',  ( -1.324107598017000065, -2.036037460020000189, 3.396848078622999978 ) ) ;
#57963 = DIRECTION ( 'NONE',  ( 0.000000000000000000, 1.000000000000000000, 0.000000000000000000 ) ) ;
#57964 = CARTESIAN_POINT ( 'NONE',  ( 9.366332946604000398, -79.77967956987598086, 1.047869802319999932 ) ) ;
#57965 = CARTESIAN_POINT ( 'NONE',  ( 6.002063118397120256, -77.76911124895428884, 7.255260483856941889 ) ) ;
#57966 = CARTESIAN_POINT ( 'NONE',  ( 8.030130101452463975, -77.19999999999998863, 7.236483772011231608 ) ) ;
#57967 = CARTESIAN_POINT ( 'NONE',  ( -1.389926494650000066, -61.42381336221999533, 12.65988803926999928 ) ) ;
#57968 = CARTESIAN_POINT ( 'NONE',  ( 12.82202470520000048, -18.57373556878999921, 2.066041976111999467 ) ) ;
#57969 = CARTESIAN_POINT ( 'NONE',  ( -3.863495128750999985, -86.32224116883999443, 1.091154501922000142 ) ) ;
#57970 = LINE ( 'NONE', #4243, #26323 ) ;
#57971 = CARTESIAN_POINT ( 'NONE',  ( 11.33104788502155813, -77.23012181351045058, 4.018671469886728964 ) ) ;
#57972 = CIRCLE ( 'NONE', #45778, 14.00000000000000000 ) ;
#57973 = CARTESIAN_POINT ( 'NONE',  ( -4.665811493888000427, -78.18558352699498926, 10.25008134894000023 ) ) ;
#57974 = CARTESIAN_POINT ( 'NONE',  ( 1.154393885937252007, -81.88139355081031567, 0.4793241423197361351 ) ) ;
#57975 = CARTESIAN_POINT ( 'NONE',  ( -0.6263700131298999274, -79.48520473737998771, -1.416660022192000046 ) ) ;
#57976 = VECTOR ( 'NONE', #10612, 1000.000000000000000 ) ;
#57977 = CARTESIAN_POINT ( 'NONE',  ( -3.321932689530000093, -81.00000000000000000, 10.22385755016999909 ) ) ;
#57978 = CARTESIAN_POINT ( 'NONE',  ( -1.500000000000000000, -83.24999999999998579, 0.000000000000000000 ) ) ;
#57979 = CARTESIAN_POINT ( 'NONE',  ( -12.43569926720000041, -61.68202092968000727, 0.4277578398253000236 ) ) ;
#57980 = CARTESIAN_POINT ( 'NONE',  ( 0.01100736988436660027, -80.22531903115304885, -10.74985747427674632 ) ) ;
#57981 = CARTESIAN_POINT ( 'NONE',  ( 0.000000000000000000, -81.19999999999998863, -7.000000000000000000 ) ) ;
#57982 = CARTESIAN_POINT ( 'NONE',  ( 8.733980040321597471, -78.54593032769474803, -7.038404617877435321 ) ) ;
#57983 = CARTESIAN_POINT ( 'NONE',  ( 1.176643243505789638, -81.82277510417709721, -0.4220517775147419326 ) ) ;
#57984 = CIRCLE ( 'NONE', #15563, 5.000000000000000000 ) ;
#57985 = CARTESIAN_POINT ( 'NONE',  ( 0.000000000000000000, -76.00000000000000000, 0.000000000000000000 ) ) ;
#57986 = CARTESIAN_POINT ( 'NONE',  ( 3.350422000336999773, -79.54043055640599391, -10.63152260923000014 ) ) ;
#57987 = CARTESIAN_POINT ( 'NONE',  ( 2.299999999264999762, -77.49999999927000260, 2.080610816276000257E-10 ) ) ;
#57988 = EDGE_LOOP ( 'NONE', ( #51079, #7397, #17848, #58222 ) ) ;
#57989 = EDGE_LOOP ( 'NONE', ( #12264, #32642, #6808, #33565 ) ) ;
#57990 = CARTESIAN_POINT ( 'NONE',  ( -3.441958447202120297, -0.7500000000000001110, 0.7329790778750402414 ) ) ;
#57991 = ORIENTED_EDGE ( 'NONE', *, *, #26849, .F. ) ;
#57992 = CARTESIAN_POINT ( 'NONE',  ( 9.931063218505961743, -54.67724209143890590, -7.763994034022205781 ) ) ;
#57993 = EDGE_LOOP ( 'NONE', ( #15784, #42031, #26976, #49737 ) ) ;
#57994 = CARTESIAN_POINT ( 'NONE',  ( 3.250000000000000444, -1.260416666666666963, 0.4254240051736247197 ) ) ;
#57995 = EDGE_CURVE ( 'NONE', #27498, #35000, #33800, .T. ) ;
#57996 = CARTESIAN_POINT ( 'NONE',  ( -3.399818433794747019, -78.73854166371795316, -0.5489011716033136423 ) ) ;
#57997 = CARTESIAN_POINT ( 'NONE',  ( 11.02987528609000023, -79.88963010244600582, -0.2088156359816000229 ) ) ;
#57998 = CARTESIAN_POINT ( 'NONE',  ( 1.295048492660999973, -24.52893519126000044, -12.54716442236999896 ) ) ;
#57999 = CARTESIAN_POINT ( 'NONE',  ( 2.948777743849000377, -81.09520976391398506, -2.327247371573999857 ) ) ;
#58000 = CARTESIAN_POINT ( 'NONE',  ( 1.487313896732463725, -79.26245606279938727, 9.382830533248572635 ) ) ;
#58001 = ORIENTED_EDGE ( 'NONE', *, *, #47046, .T. ) ;
#58002 = DIRECTION ( 'NONE',  ( 0.000000000000000000, 0.000000000000000000, 1.000000000000000000 ) ) ;
#58003 = CARTESIAN_POINT ( 'NONE',  ( -3.894252032411999576, -78.51770906870001454, -11.57248695932000082 ) ) ;
#58004 = ORIENTED_EDGE ( 'NONE', *, *, #9736, .F. ) ;
#58005 = ORIENTED_EDGE ( 'NONE', *, *, #46449, .F. ) ;
#58006 = CARTESIAN_POINT ( 'NONE',  ( 0.000000000000000000, 4.040000000000000036, 0.000000000000000000 ) ) ;
#58007 = CARTESIAN_POINT ( 'NONE',  ( 1.170174673132000187, -80.05547441318699953, 0.6397400908730001001 ) ) ;
#58008 = CARTESIAN_POINT ( 'NONE',  ( 7.256139241522999939, -77.51733095546998698, 6.443535727668999513 ) ) ;
#58009 = CARTESIAN_POINT ( 'NONE',  ( -3.667511737244591785, -86.36264283715696877, -2.559636160674789718 ) ) ;
#58010 = CARTESIAN_POINT ( 'NONE',  ( 2.126156167813490150, -85.88434721301992170, 2.769575613414034798 ) ) ;
#58011 = DIRECTION ( 'NONE',  ( 0.000000000000000000, 0.1122098755727947705, 0.9936845293270585300 ) ) ;
#58012 = EDGE_CURVE ( 'NONE', #52771, #40996, #50679, .T. ) ;
#58013 = CARTESIAN_POINT ( 'NONE',  ( 11.45970853605999906, -76.52906641171999524, 5.337786833297999856 ) ) ;
#58014 = AXIS2_PLACEMENT_3D ( 'NONE', #25870, #2586, #53034 ) ;
#58015 = CARTESIAN_POINT ( 'NONE',  ( -9.568646597019998978, -76.48705691727600708, 5.187623148002000306 ) ) ;
#58016 = CARTESIAN_POINT ( 'NONE',  ( -9.247438236293723079, -78.60230166250890704, -0.2676552778266205190 ) ) ;
#58017 = CARTESIAN_POINT ( 'NONE',  ( -3.959055338030000204, -80.49395764150798982, 0.1785245326323999793 ) ) ;
#58018 = AXIS2_PLACEMENT_3D ( 'NONE', #12617, #30614, #7616 ) ;
#58019 = CARTESIAN_POINT ( 'NONE',  ( -10.55910102243999837, -59.58485473249000108, 7.642147947533000085 ) ) ;
#58020 = CARTESIAN_POINT ( 'NONE',  ( -2.312235755821637539, -3.038362080394761744, 2.283552099544162051 ) ) ;
#58021 = CARTESIAN_POINT ( 'NONE',  ( -1.193739508925000026, -81.93650264934798599, -3.337658129978000154 ) ) ;
#58022 = CARTESIAN_POINT ( 'NONE',  ( 12.00000000000000533, -77.54258394437167112, -1.118314842272786214 ) ) ;
#58023 = CARTESIAN_POINT ( 'NONE',  ( -0.8464931918749931672, -80.98139962866328290, 10.71653294235299292 ) ) ;
#58024 = CARTESIAN_POINT ( 'NONE',  ( 1.328862289696999932, -80.19948534945449126, 11.18676134159000135 ) ) ;
#58025 = CARTESIAN_POINT ( 'NONE',  ( 3.772660615778999915, -2.043216633591999898, 0.5031134774969999723 ) ) ;
#58026 = CARTESIAN_POINT ( 'NONE',  ( 0.08741542428476450910, -80.11951995081831512, 1.271648086810047706 ) ) ;
#58027 = ORIENTED_EDGE ( 'NONE', *, *, #4555, .T. ) ;
#58028 = CARTESIAN_POINT ( 'NONE',  ( 9.249769291450279596, -78.85065788838248579, 0.06519237146997462762 ) ) ;
#58029 = EDGE_CURVE ( 'NONE', #18786, #4693, #43483, .T. ) ;
#58030 = DIRECTION ( 'NONE',  ( 0.000000000000000000, 1.000000000000000000, 0.000000000000000000 ) ) ;
#58031 = CARTESIAN_POINT ( 'NONE',  ( 0.2153359604882000011, -82.04020749310099347, 1.316133176457000120 ) ) ;
#58032 = CARTESIAN_POINT ( 'NONE',  ( 2.561895579250705435, -79.04666666666665265, -9.182597689054190937 ) ) ;
#58033 = CARTESIAN_POINT ( 'NONE',  ( 7.411516475408999050, -77.19055350637998458, -10.69619859711000132 ) ) ;
#58034 = CARTESIAN_POINT ( 'NONE',  ( 5.624272343092999726, -79.39536001420199796, 7.680093418580999476 ) ) ;
#58035 = CARTESIAN_POINT ( 'NONE',  ( 12.49168433580000048, -18.70150862776000267, -1.667916687244999974 ) ) ;
#58036 = ORIENTED_EDGE ( 'NONE', *, *, #8159, .F. ) ;
#58037 = FACE_OUTER_BOUND ( 'NONE', #25249, .T. ) ;
#58038 = CARTESIAN_POINT ( 'NONE',  ( -2.049109721976000387, -77.06873060082338611, 11.08635720663000157 ) ) ;
#58039 = CARTESIAN_POINT ( 'NONE',  ( 0.4811021089508000226, -81.95005443991800576, -1.323757477563000107 ) ) ;
#58040 = CARTESIAN_POINT ( 'NONE',  ( -10.48543666025109289, -78.94166666666666288, -6.043427764450796325 ) ) ;
#58041 = CARTESIAN_POINT ( 'NONE',  ( -5.250896469870999006, -77.87841853088399091, 7.943454065752000304 ) ) ;
#58043 = CARTESIAN_POINT ( 'NONE',  ( -1.488596180559999871, -0.9121139388282000215, -3.730054860412999940 ) ) ;
#58042 = CARTESIAN_POINT ( 'NONE',  ( 0.2897064650623000226, -84.90343479341399302, -4.120022288451000492 ) ) ;
#58044 = CARTESIAN_POINT ( 'NONE',  ( -1.931086388455000025, -60.09778595451999905, -12.71798280857999863 ) ) ;
#58045 = CARTESIAN_POINT ( 'NONE',  ( -0.5815971981373999622, -79.69404873715900806, -1.292982629223000002 ) ) ;
#58046 = EDGE_CURVE ( 'NONE', #39544, #19092, #42049, .T. ) ;
#58047 = ORIENTED_EDGE ( 'NONE', *, *, #57406, .F. ) ;
#58048 = CARTESIAN_POINT ( 'NONE',  ( -2.489408411739813420, -77.20657166405426608, -10.45779613294925348 ) ) ;
#58049 = CARTESIAN_POINT ( 'NONE',  ( 2.879226727952061360, -78.84583333333328881, -10.71369944335147650 ) ) ;
#58050 = CARTESIAN_POINT ( 'NONE',  ( 0.000000000000000000, -77.00000000000000000, 0.000000000000000000 ) ) ;
#58051 = SHAPE_REPRESENTATION ( 'MAS-694', ( #46161, #1821, #19717, #15026, #7490, #48948, #25386, #31958, #38585 ), #14060 ) ;
#58052 = ORIENTED_EDGE ( 'NONE', *, *, #21984, .F. ) ;
#58053 = ORIENTED_EDGE ( 'NONE', *, *, #5281, .T. ) ;
#58054 = CARTESIAN_POINT ( 'NONE',  ( 7.294482259529999624, -79.55389345209998453, -8.153425347847999660 ) ) ;
#58055 = DIRECTION ( 'NONE',  ( -1.000000000000000000, 0.000000000000000000, 0.000000000000000000 ) ) ;
#58056 = CIRCLE ( 'NONE', #55196, 9.199999999999999289 ) ;
#58057 = CARTESIAN_POINT ( 'NONE',  ( -10.73093511375999753, -79.77125540420298933, -3.969369046568999693 ) ) ;
#58058 = EDGE_LOOP ( 'NONE', ( #40769, #41305, #11194, #54452 ) ) ;
#58059 = CARTESIAN_POINT ( 'NONE',  ( -11.99726733138999890, -77.69856428951000282, -1.123097615067000010 ) ) ;
#58060 = ORIENTED_EDGE ( 'NONE', *, *, #36471, .F. ) ;
#58061 = VECTOR ( 'NONE', #47886, 1000.000000000000000 ) ;
#58062 = ORIENTED_EDGE ( 'NONE', *, *, #44919, .F. ) ;
#58063 = CARTESIAN_POINT ( 'NONE',  ( -2.884042199509171400, -2.639263732757689773, -1.497520329303954512 ) ) ;
#58064 = CARTESIAN_POINT ( 'NONE',  ( -11.68767212001979594, -78.77916666666666856, 3.140974612311315806 ) ) ;
#58065 = LINE ( 'NONE', #17626, #47816 ) ;
#58066 = ORIENTED_EDGE ( 'NONE', *, *, #47268, .F. ) ;
#58067 = DIRECTION ( 'NONE',  ( 0.000000000000000000, -1.000000000000000000, 0.000000000000000000 ) ) ;
#58068 = EDGE_LOOP ( 'NONE', ( #53633, #28208, #4823, #51335 ) ) ;
#58069 = CARTESIAN_POINT ( 'NONE',  ( 1.273811252452706766, -80.40095636055373518, 0.01856756060433174121 ) ) ;
#58070 = CARTESIAN_POINT ( 'NONE',  ( -3.523652525393907720, -78.91452042059378869, -1.990986658322625669 ) ) ;
#58071 = CARTESIAN_POINT ( 'NONE',  ( -8.485281374238999419, -60.04999999966999980, 8.485281374238999419 ) ) ;
#58072 = CARTESIAN_POINT ( 'NONE',  ( -7.640030139755999983, -23.30716934606000024, -10.18491068059999805 ) ) ;
#58073 = CARTESIAN_POINT ( 'NONE',  ( -0.7698740312961022125, -77.31791980077814230, -11.75340416254214659 ) ) ;
#58074 = EDGE_CURVE ( 'NONE', #26014, #45976, #25559, .T. ) ;
#58075 = CARTESIAN_POINT ( 'NONE',  ( -9.000000000000000000, -0.5000000000000000000, 0.000000000000000000 ) ) ;
#58076 = CARTESIAN_POINT ( 'NONE',  ( 8.049666437455634593, -77.33396340929790824, -8.806025772650324157 ) ) ;
#58077 = DIRECTION ( 'NONE',  ( 0.7071067811865475727, 0.000000000000000000, 0.7071067811865475727 ) ) ;
#58078 = EDGE_CURVE ( 'NONE', #3332, #55842, #8614, .T. ) ;
#58079 = DIRECTION ( 'NONE',  ( -1.000000000000000000, 0.000000000000000000, 0.000000000000000000 ) ) ;
#58080 = CARTESIAN_POINT ( 'NONE',  ( 1.199500263597271577, -80.09791666666669130, -0.9218200799623702535 ) ) ;
#58081 = CARTESIAN_POINT ( 'NONE',  ( -4.072048464454999461, -81.76505496681200214, -0.9102108328765000644 ) ) ;
#58082 = CARTESIAN_POINT ( 'NONE',  ( -3.703509300394999926, -77.72626001420199771, 9.151787782534000826 ) ) ;
#58083 = CARTESIAN_POINT ( 'NONE',  ( 1.092232985442820992, -83.29166666666665719, 0.6295237254636267821 ) ) ;
#58084 = CARTESIAN_POINT ( 'NONE',  ( -1.250000000000000000, -60.24678171298000251, 12.50000000000000000 ) ) ;
#58085 = CARTESIAN_POINT ( 'NONE',  ( 0.5999999999999999778, -18.84999999999999787, 10.98362417419999915 ) ) ;
#58086 = DIRECTION ( 'NONE',  ( 0.000000000000000000, 1.000000000000000000, 0.000000000000000000 ) ) ;
#58087 = CARTESIAN_POINT ( 'NONE',  ( -3.517590690533999975, -84.74982851107797899, -0.4594732892919000111 ) ) ;
#58088 = CARTESIAN_POINT ( 'NONE',  ( -3.522236695112999971, -1.250894741108000030, 2.142266609051000081 ) ) ;
#58089 = CARTESIAN_POINT ( 'NONE',  ( 5.645287065787000458, -79.47470095943376123, 7.708789581145001790 ) ) ;
#58090 = EDGE_CURVE ( 'NONE', #33386, #31248, #43263, .T. ) ;
#58091 = CARTESIAN_POINT ( 'NONE',  ( 1.476627061896669924, -81.08212518682249481, -0.3264197646420510246 ) ) ;
#58092 = CARTESIAN_POINT ( 'NONE',  ( 12.66001556635999847, -61.43260856911000189, -1.381621105853999998 ) ) ;
#58093 = CARTESIAN_POINT ( 'NONE',  ( -1.071041487988000140, -79.40975894690099324, -0.9340865940840999970 ) ) ;
#58094 = CARTESIAN_POINT ( 'NONE',  ( -10.35747158362999976, -23.31584477285000290, -7.626500902217000721 ) ) ;
#58095 = CARTESIAN_POINT ( 'NONE',  ( 5.122310662682999727, -78.19045643997900186, -9.640399341584998893 ) ) ;
#58096 = CARTESIAN_POINT ( 'NONE',  ( 1.675539995062999887, -78.73730299628599028, 11.92720225554999836 ) ) ;
#58097 = CARTESIAN_POINT ( 'NONE',  ( -0.1963495408493673433, -80.88541666666669983, 1.499999999999999334 ) ) ;
#58099 = CARTESIAN_POINT ( 'NONE',  ( 0.1641065589886999965, -78.21905598575500562, 1.507319194642999793 ) ) ;
#58098 = DIRECTION ( 'NONE',  ( 1.000000000000000000, 0.000000000000000000, 0.000000000000000000 ) ) ;
#58100 = AXIS2_PLACEMENT_3D ( 'NONE', #53908, #44170, #31137 ) ;
#58101 = ORIENTED_EDGE ( 'NONE', *, *, #4029, .F. ) ;
#58102 = CIRCLE ( 'NONE', #9103, 9.000000000000000000 ) ;
#58103 = CARTESIAN_POINT ( 'NONE',  ( -10.35747145892000098, -18.68415268018999953, -7.626500777237000150 ) ) ;
#58104 = CARTESIAN_POINT ( 'NONE',  ( -4.600316697258000076, -80.98327349430469724, 9.793279191701000030 ) ) ;
#58105 = AXIS2_PLACEMENT_3D ( 'NONE', #16430, #24990, #29981 ) ;
#58106 = CARTESIAN_POINT ( 'NONE',  ( -11.99999999979999821, -23.14999999072999870, 0.7999999997951999786 ) ) ;
#58107 = CARTESIAN_POINT ( 'NONE',  ( -1.159355627281299705, -85.90729167298438540, 3.242290418978912570 ) ) ;
#58108 = CARTESIAN_POINT ( 'NONE',  ( -3.244487197725999916, -76.93554274292699802, -10.73738397614000029 ) ) ;
#58109 = CARTESIAN_POINT ( 'NONE',  ( -9.395758989587999821, -61.50491532550999096, 8.188252216855000043 ) ) ;
#58110 = CARTESIAN_POINT ( 'NONE',  ( 7.919085842678998510, -79.02973936012098477, -5.669895566145999766 ) ) ;
#58111 = CARTESIAN_POINT ( 'NONE',  ( -2.273545738020000151, -1.203822672877000066, -2.920649130850999864 ) ) ;
#58112 = CARTESIAN_POINT ( 'NONE',  ( 3.261893290220421182, -76.44721653378499582, -11.36034884816034563 ) ) ;
#58113 = FACE_OUTER_BOUND ( 'NONE', #34626, .T. ) ;
#58114 = CARTESIAN_POINT ( 'NONE',  ( -1.799475295154000065, -57.04916621739000249, 12.69619287815999975 ) ) ;
#58115 = EDGE_LOOP ( 'NONE', ( #34923, #56845, #55434, #49266 ) ) ;
#58116 = DIRECTION ( 'NONE',  ( 0.7071067811865969777, -0.7071067811864980568, 6.518241473468980170E-10 ) ) ;
#58117 = LINE ( 'NONE', #26233, #40048 ) ;
#58118 = CARTESIAN_POINT ( 'NONE',  ( -3.206516299415000049, -1.613032031399000088, -0.5298615117031000299 ) ) ;
#58119 = CARTESIAN_POINT ( 'NONE',  ( -10.42274798264000069, -58.55365779174999830, -7.691916945401000127 ) ) ;
#58120 = CARTESIAN_POINT ( 'NONE',  ( 0.9441861370063999725, -79.71587320708998448, 1.372505234203999835 ) ) ;
#58121 = CARTESIAN_POINT ( 'NONE',  ( -14.00000000000000000, -91.29999999999999716, 8.108919984112999312E-14 ) ) ;
#58122 = VERTEX_POINT ( 'NONE', #47419 ) ;
#58123 = CARTESIAN_POINT ( 'NONE',  ( 1.250000000000000000, -78.35000000000000853, 0.000000000000000000 ) ) ;
#58124 = CARTESIAN_POINT ( 'NONE',  ( -11.43989337263541373, -77.72004047834380458, -3.071150918567757238 ) ) ;
#58125 = CARTESIAN_POINT ( 'NONE',  ( -1.799502287743000029, -23.30716934606000024, 12.60413652831999975 ) ) ;
#58126 = EDGE_CURVE ( 'NONE', #15737, #8049, #30729, .T. ) ;
#58127 = ORIENTED_EDGE ( 'NONE', *, *, #14386, .F. ) ;
#58128 = CARTESIAN_POINT ( 'NONE',  ( -12.64502302236999931, -59.57129148919000272, 1.799490220168999954 ) ) ;
#58129 = DIRECTION ( 'NONE',  ( 0.000000000000000000, 1.000000000000000000, 0.000000000000000000 ) ) ;
#58130 = CARTESIAN_POINT ( 'NONE',  ( -9.387315177295000979, -79.74757778715598988, 2.697965643110000311 ) ) ;
#58131 = ORIENTED_EDGE ( 'NONE', *, *, #18932, .T. ) ;
#58132 = ORIENTED_EDGE ( 'NONE', *, *, #49593, .T. ) ;
#58133 = CARTESIAN_POINT ( 'NONE',  ( -10.57243353979999867, -76.14788179775399612, 6.388556512783999608 ) ) ;
#58134 = CARTESIAN_POINT ( 'NONE',  ( -10.45298374846471567, -78.61878984457777619, -2.509360686428254272 ) ) ;
#58135 = CARTESIAN_POINT ( 'NONE',  ( 1.248120568784000017, -78.57661456821999479, 1.076606392262000167 ) ) ;
#58136 = ORIENTED_EDGE ( 'NONE', *, *, #34300, .T. ) ;
#58137 = CARTESIAN_POINT ( 'NONE',  ( 10.53562613913999968, -18.79442116269000351, 7.620013630324000253 ) ) ;
#58138 = VECTOR ( 'NONE', #31963, 1000.000000000000000 ) ;
#58139 = CARTESIAN_POINT ( 'NONE',  ( -3.907294856124924110, -77.94192925949296580, -8.882954164993476454 ) ) ;
#58140 = CARTESIAN_POINT ( 'NONE',  ( 0.5435567983843210271, -80.26107177751177346, -1.125492201572247719 ) ) ;
#58141 = CARTESIAN_POINT ( 'NONE',  ( 3.425937024882473377E-06, -77.82827182887865547, -1.422119424801547627 ) ) ;
#58142 = CIRCLE ( 'NONE', #20455, 30.49999999999998934 ) ;
#58143 = CARTESIAN_POINT ( 'NONE',  ( -0.02522423216716376468, -78.37478882719507567, -11.17055116352559452 ) ) ;
#58144 = CARTESIAN_POINT ( 'NONE',  ( 12.51072239526000196, -15.69705297114000331, -0.7871079366006996647 ) ) ;
#58145 = CARTESIAN_POINT ( 'NONE',  ( 1.473002020459766470, -86.40321104920799655, 3.394151594327763366 ) ) ;
#58146 = CARTESIAN_POINT ( 'NONE',  ( -9.805641529082999241, -79.44203154651999910, -5.446788484474000214 ) ) ;
#58147 = DIRECTION ( 'NONE',  ( -0.7071067811865475727, 0.000000000000000000, -0.7071067811865475727 ) ) ;
#58148 = CARTESIAN_POINT ( 'NONE',  ( -12.50000000000000000, -18.75000000240999753, -1.750000000000000000 ) ) ;
#58149 = EDGE_LOOP ( 'NONE', ( #8245, #38026, #35601, #46732 ) ) ;
#58150 = DIRECTION ( 'NONE',  ( -0.7071067811865474617, -0.7071067811865474617, -3.646389762765242273E-10 ) ) ;
#58151 = EDGE_CURVE ( 'NONE', #393, #44413, #11469, .T. ) ;
#58152 = CARTESIAN_POINT ( 'NONE',  ( -7.450482419345999752, -76.12526934845000426, -9.799277032148999922 ) ) ;
#58153 = CARTESIAN_POINT ( 'NONE',  ( 1.185193155257999953, -80.09864567164899540, -1.096599795159000079 ) ) ;
#58154 = CARTESIAN_POINT ( 'NONE',  ( -1.804337680682123857, -2.766036367877359847, 3.091116340519547645 ) ) ;
#58155 = CARTESIAN_POINT ( 'NONE',  ( -7.624341766647000362, -18.73514853758999976, 10.42531125024999916 ) ) ;
#58156 = CARTESIAN_POINT ( 'NONE',  ( -9.801255020792000394, -76.65022101953400124, 7.399866681860999940 ) ) ;
#58157 = CARTESIAN_POINT ( 'NONE',  ( 1.568318300085000120E-14, -0.05000000003700048185, 0.000000000000000000 ) ) ;
#58158 = CARTESIAN_POINT ( 'NONE',  ( 6.657089793739999983, -79.81660374219698895, 8.818222636911000833 ) ) ;
#58159 = CARTESIAN_POINT ( 'NONE',  ( 5.376571573888999644, -77.20778998579800145, 8.118187030778999613 ) ) ;
#58160 = CARTESIAN_POINT ( 'NONE',  ( 12.05967318610715466, -76.80230997908272172, 0.3521930913432630428 ) ) ;
#58161 = CARTESIAN_POINT ( 'NONE',  ( -6.606377239730330864, -79.57291666666665719, -8.596418555780440229 ) ) ;
#58162 = CARTESIAN_POINT ( 'NONE',  ( -8.838834764832000701, -55.54999999966999980, 8.838834764832000701 ) ) ;
#58163 = CARTESIAN_POINT ( 'NONE',  ( 5.413904038987143785, -77.83333333333332860, 9.393203674808290771 ) ) ;
#58164 = EDGE_CURVE ( 'NONE', #57912, #31243, #25092, .T. ) ;
#58165 = VERTEX_POINT ( 'NONE', #57117 ) ;
#58166 = CARTESIAN_POINT ( 'NONE',  ( 0.6237791458550000501, -83.11657026302199824, -1.329415719495999904 ) ) ;
#58167 = CARTESIAN_POINT ( 'NONE',  ( 0.4719577028681999908, -81.17336727174999567, -1.266186157272999768 ) ) ;
#58168 = CARTESIAN_POINT ( 'NONE',  ( 1.034214221880000141E-14, 0.2999999999999999334, 0.000000000000000000 ) ) ;
#58169 = CARTESIAN_POINT ( 'NONE',  ( 4.458743082292000004, -77.34296909926000296, 11.11915799896999957 ) ) ;
#58170 = CYLINDRICAL_SURFACE ( 'NONE', #33450, 10.75000000000000000 ) ;
#58171 = CARTESIAN_POINT ( 'NONE',  ( 1.531359430757999851, -82.48818925093098642, -0.6558942768039000004 ) ) ;
#58172 = CARTESIAN_POINT ( 'NONE',  ( 1.628430890020000188, -78.94048418952499446, 11.59185972383999896 ) ) ;
#58173 = CARTESIAN_POINT ( 'NONE',  ( 2.013632425233999879, -78.21154805011499889, -9.512575055159999238 ) ) ;
#58174 = CARTESIAN_POINT ( 'NONE',  ( 1.236990682704000033, -77.50769513184299342, 9.441410396910001168 ) ) ;
#58175 = CARTESIAN_POINT ( 'NONE',  ( -9.346069275190213688, -25.16527745691412221, -8.620894635682162743 ) ) ;
#58176 = DIRECTION ( 'NONE',  ( 0.000000000000000000, -1.000000000000000000, 0.000000000000000000 ) ) ;
#58177 = CARTESIAN_POINT ( 'NONE',  ( -1.733234625524999961, -80.13890251626278882, -10.77827740047999860 ) ) ;
#58178 = CARTESIAN_POINT ( 'NONE',  ( 3.751322949195259326, -86.02148118236286223, 2.724698623988329071 ) ) ;
#58179 = VERTEX_POINT ( 'NONE', #12247 ) ;
#58180 = CARTESIAN_POINT ( 'NONE',  ( 0.3023719455682365442, -78.17250000000001364, 9.537307262745171599 ) ) ;
#58181 = CARTESIAN_POINT ( 'NONE',  ( -3.785489411603719212, -77.09933145171892477, 11.15228598470222110 ) ) ;
#58182 = CARTESIAN_POINT ( 'NONE',  ( 10.88639046104558794, -78.91824007476243708, -4.509380154451887002 ) ) ;
#58183 = CARTESIAN_POINT ( 'NONE',  ( 3.485499217012000273, -78.48547957940618858, -1.287490079826536515E-15 ) ) ;
#58184 = CARTESIAN_POINT ( 'NONE',  ( -1.458706046781999888, -81.73027866961000143, 0.8046341008317999810 ) ) ;
#58185 = CARTESIAN_POINT ( 'NONE',  ( 8.212410987726999068, -78.18463944979998814, -6.936771999183999782 ) ) ;
#58186 = DIRECTION ( 'NONE',  ( 0.7071067811864980568, 0.7071067811865969777, 8.066391729469968668E-09 ) ) ;
#58187 = CARTESIAN_POINT ( 'NONE',  ( -1.134051983850000056, -76.89122910487600393, 12.21726166519999879 ) ) ;
#58188 = CARTESIAN_POINT ( 'NONE',  ( 5.660454042118933771, -78.53486099951153676, 10.30159814769029580 ) ) ;
#58189 = CARTESIAN_POINT ( 'NONE',  ( 4.316049272395066083, -76.84239669216790958, 9.924321351449295392 ) ) ;
#58190 = ORIENTED_EDGE ( 'NONE', *, *, #10862, .T. ) ;
#58191 = AXIS2_PLACEMENT_3D ( 'NONE', #25849, #43005, #2562 ) ;
#58192 = CARTESIAN_POINT ( 'NONE',  ( 6.010232441408999371, -80.10679326027729985, 9.524218016016000377 ) ) ;
#58193 = CARTESIAN_POINT ( 'NONE',  ( 9.022184164167814657, -77.23121341071495749, -2.164508873546484580 ) ) ;
#58194 = FACE_OUTER_BOUND ( 'NONE', #13107, .T. ) ;
#58195 = DIRECTION ( 'NONE',  ( 0.000000000000000000, -1.000000000000000000, 0.000000000000000000 ) ) ;
#58196 = VECTOR ( 'NONE', #18812, 1000.000000000000000 ) ;
#58197 = CARTESIAN_POINT ( 'NONE',  ( 7.917622607290999426, -78.55527898622098348, 7.861478989701000231 ) ) ;
#58198 = CARTESIAN_POINT ( 'NONE',  ( -12.50657384680346240, -53.82752586700246411, 0.3552647085964846241 ) ) ;
#58199 = AXIS2_PLACEMENT_3D ( 'NONE', #19638, #16086, #29925 ) ;
#58200 = CARTESIAN_POINT ( 'NONE',  ( 1.206033450961812248, -81.54768710939626430, -0.9139931269966713456 ) ) ;
#58201 = CARTESIAN_POINT ( 'NONE',  ( -8.771511755855000203, -77.88827704918399775, -8.593972346821999508 ) ) ;
#58202 = EDGE_CURVE ( 'NONE', #27498, #33741, #10530, .T. ) ;
#58203 = DIRECTION ( 'NONE',  ( 0.7071067811865470176, -0.7071067811865470176, 3.647649194621239524E-08 ) ) ;
#58204 = CARTESIAN_POINT ( 'NONE',  ( -1.668607604626823449, -60.59381631189516781, 12.52787843855104910 ) ) ;
#58205 = EDGE_CURVE ( 'NONE', #57688, #7670, #44440, .T. ) ;
#58206 = CARTESIAN_POINT ( 'NONE',  ( -7.601397897754999633, -60.04999999966999980, 9.369164850722000892 ) ) ;
#58207 = CARTESIAN_POINT ( 'NONE',  ( 11.90000000000000036, -21.00000000000000000, -0.6999999999999999556 ) ) ;
#58208 = EDGE_LOOP ( 'NONE', ( #16079, #51844, #41738 ) ) ;
#58209 = ORIENTED_EDGE ( 'NONE', *, *, #39753, .F. ) ;
#58210 = CARTESIAN_POINT ( 'NONE',  ( 10.55352543338477389, -78.83484157365509759, -2.045682359817731832 ) ) ;
#58211 = VERTEX_POINT ( 'NONE', #13692 ) ;
#58212 = CARTESIAN_POINT ( 'NONE',  ( 3.367278140553823462, -79.59625721410608890, 8.916401300557922127 ) ) ;
#58213 = EDGE_LOOP ( 'NONE', ( #15082, #55759, #24572, #52531, #30288 ) ) ;
#58214 = CARTESIAN_POINT ( 'NONE',  ( 8.220407391935999897, -24.81950084232000364, 9.523310056108000410 ) ) ;
#58215 = CARTESIAN_POINT ( 'NONE',  ( 1.606468910658999993, -77.77776596815100163, -10.91425636589999826 ) ) ;
#58216 = DIRECTION ( 'NONE',  ( -0.7071067811865470176, -0.7071067811865470176, -3.680441204124245327E-08 ) ) ;
#58217 = CARTESIAN_POINT ( 'NONE',  ( 7.103190263045000563, -78.00082999526600247, 6.271635551916999951 ) ) ;
#58218 = CARTESIAN_POINT ( 'NONE',  ( -12.50000000000000000, -24.68359816828999698, -1.003641515615000035 ) ) ;
#58219 = CARTESIAN_POINT ( 'NONE',  ( -2.710423231297999891, -79.66052689899100869, 10.88447134676999895 ) ) ;
#58220 = CARTESIAN_POINT ( 'NONE',  ( 0.7692036342426435969, -79.42240521102286266, 0.9862270034562748977 ) ) ;
#58221 = ORIENTED_EDGE ( 'NONE', *, *, #21868, .F. ) ;
#58222 = ORIENTED_EDGE ( 'NONE', *, *, #54972, .F. ) ;
#58223 = ADVANCED_FACE ( 'NONE', ( #45598, #36422 ), #54448, .T. ) ;
#58224 = CARTESIAN_POINT ( 'NONE',  ( 2.425090211683515573, -77.45404813181065151, 8.927162646165987425 ) ) ;
#58225 = CARTESIAN_POINT ( 'NONE',  ( 2.386167682861000117, -77.28781509216399570, 10.77916482977000001 ) ) ;
#58226 = CONICAL_SURFACE ( 'NONE', #24272, 4.199999999630000147, 0.7853981633972997312 ) ;
#58227 = CARTESIAN_POINT ( 'NONE',  ( 5.927986824875999261, -78.06774951115899341, -7.683077610609999830 ) ) ;
#58228 = CARTESIAN_POINT ( 'NONE',  ( -9.683064706975999414, -75.68874058712000874, 8.142089017637001547 ) ) ;
#58229 = CARTESIAN_POINT ( 'NONE',  ( -7.065921977188095227, -79.45798876533616806, -6.351589347257088569 ) ) ;
#58230 = CARTESIAN_POINT ( 'NONE',  ( 9.433537730344784933, -53.67202052640185883, -8.532653828180887245 ) ) ;
#58231 = CARTESIAN_POINT ( 'NONE',  ( 1.791008777272000030, -80.35273698580898838, 11.11143388882000060 ) ) ;
#58232 = DIRECTION ( 'NONE',  ( 0.000000000000000000, 0.000000000000000000, 1.000000000000000000 ) ) ;
#58233 = CARTESIAN_POINT ( 'NONE',  ( 12.50000000000000000, -61.48359816765000119, 1.003641516062000250 ) ) ;
#58234 = VECTOR ( 'NONE', #13987, 1000.000000000000000 ) ;
#58235 = CARTESIAN_POINT ( 'NONE',  ( 1.243096656778429177, -79.16484084040288849, 9.498104304983947088 ) ) ;
#58236 = EDGE_CURVE ( 'NONE', #8584, #47685, #25600, .T. ) ;
#58237 = EDGE_LOOP ( 'NONE', ( #4748, #39969, #57943, #55025 ) ) ;
#58238 = CARTESIAN_POINT ( 'NONE',  ( -7.388677236831999728, -79.51494008599399876, -9.854616049676000245 ) ) ;
#58239 = CARTESIAN_POINT ( 'NONE',  ( 2.909452169864999771, -76.42760485387299241, 10.87394468084000110 ) ) ;
#58240 = CARTESIAN_POINT ( 'NONE',  ( -5.260139927115998759, -78.01577672530346774, 9.375410799120500016 ) ) ;
#58241 = EDGE_CURVE ( 'NONE', #616, #6742, #25718, .T. ) ;
#58242 = CARTESIAN_POINT ( 'NONE',  ( -0.08519377839585000334, -78.50946019191600556, 11.97951611939999950 ) ) ;
#58243 = CARTESIAN_POINT ( 'NONE',  ( 0.8506806241676515556, -3.354166666666666963, 3.165411199172028844 ) ) ;
#58245 = CARTESIAN_POINT ( 'NONE',  ( -0.4802748259354999716, -16.99473092717999734, -12.54896097834000024 ) ) ;
#58244 = CARTESIAN_POINT ( 'NONE',  ( -1.250000000000000000, -76.40000000064199526, 0.000000000000000000 ) ) ;
#58246 = CONICAL_SURFACE ( 'NONE', #16748, 3.699999993671000187, 0.7853981633972997312 ) ;
#58247 = CARTESIAN_POINT ( 'NONE',  ( 8.485281374238999419, -55.54999999966999980, -8.485281374238999419 ) ) ;
#58248 = CARTESIAN_POINT ( 'NONE',  ( 5.439600774063181099, -80.93322674150709872, 9.274161813587999958 ) ) ;
#58249 = CARTESIAN_POINT ( 'NONE',  ( 10.35845616725999996, -55.50221404479999876, -7.627487606591000002 ) ) ;
#58250 = B_SPLINE_CURVE_WITH_KNOTS ( 'NONE', 3,
 ( #43537, #26093, #11956, #39101, #29934, #34078 ),
 .UNSPECIFIED., .F., .F.,
 ( 4, 1, 1, 4 ),
 ( 0.000000000000000000, 0.3333333333333000081, 0.6666666666667000474, 1.000000000000000000 ),
 .UNSPECIFIED. ) ;
#58251 = CARTESIAN_POINT ( 'NONE',  ( -0.6878299077642000547, -82.23020250931300268, -1.043738481606000024 ) ) ;
#58252 = CARTESIAN_POINT ( 'NONE',  ( -10.79885705035999877, -76.91107590507699854, -2.763914921897999921 ) ) ;
#58253 = CARTESIAN_POINT ( 'NONE',  ( 10.48543666025108401, -78.09166666666666856, 6.043427764450814976 ) ) ;
#58254 = CARTESIAN_POINT ( 'NONE',  ( -5.246654900278999278, -80.97711506270789528, -9.828008984874001541 ) ) ;
#58255 = ORIENTED_EDGE ( 'NONE', *, *, #6596, .T. ) ;
#58256 = CARTESIAN_POINT ( 'NONE',  ( 12.76303204298000082, -60.06485150663000638, -1.980584515756000030 ) ) ;
#58257 = CARTESIAN_POINT ( 'NONE',  ( -0.9113424693959999434, -53.97464206407000376, 12.54674099554000044 ) ) ;
#58258 = CARTESIAN_POINT ( 'NONE',  ( -12.82904091339000097, -18.67547470641000018, 2.062673488738000049 ) ) ;
#58259 = CARTESIAN_POINT ( 'NONE',  ( -3.553391519525000319, -1.842240405599000042, -1.760552736492000170 ) ) ;
#58260 = CARTESIAN_POINT ( 'NONE',  ( -9.384564006317999585, -80.01346083593999481, 0.8695881376670999696 ) ) ;
#58261 = CARTESIAN_POINT ( 'NONE',  ( 7.000000000000000000, -81.10000000285099020, 0.000000000000000000 ) ) ;
#58262 = CARTESIAN_POINT ( 'NONE',  ( -8.838834764832000701, -60.04999999966999980, -8.838834764832000701 ) ) ;
#58263 = CARTESIAN_POINT ( 'NONE',  ( 12.83675912440999944, -18.77244614031999959, 2.062833085520999976 ) ) ;
#58264 = CARTESIAN_POINT ( 'NONE',  ( 4.040434065196999214, -83.94574735065199889, -1.050948307445999985 ) ) ;
#58265 = EDGE_CURVE ( 'NONE', #326, #17731, #17245, .T. ) ;
#58266 = DIRECTION ( 'NONE',  ( 1.000000000000000000, 0.000000000000000000, 0.000000000000000000 ) ) ;
#58267 = CARTESIAN_POINT ( 'NONE',  ( -11.72607011526379672, -76.97216391817583769, -2.880960420985590797 ) ) ;
#58268 = CARTESIAN_POINT ( 'NONE',  ( -10.18558922015999890, -78.70658632805000821, 7.214292160837000090 ) ) ;
#58269 = B_SPLINE_SURFACE_WITH_KNOTS ( 'NONE', 3, 3, ( 
 ( #20050, #10903, #54878, #19751 ),
 ( #28589, #14716, #28879, #46926 ),
 ( #28291, #46341, #32424, #15315 ),
 ( #6453, #32714, #50469, #33601 ),
 ( #50766, #24468, #19457, #23874 ),
 ( #14429, #56060, #5572, #46047 ),
 ( #37161, #38038, #33309, #51640 ),
 ( #27999, #46633, #36866, #1756 ),
 ( #33010, #23581, #15607, #5865 ),
 ( #2050, #51344, #1176, #11195 ),
 ( #42481, #24172, #6163, #29171 ) ),
 .UNSPECIFIED., .F., .F., .F.,
 ( 4, 1, 1, 1, 1, 1, 1, 1, 4 ),
 ( 4, 4 ),
 ( -0.01994534136797000007, 0.000000000000000000, 0.1666666666667000196, 0.3333333333333000081, 0.5000000000000000000, 0.6666666666667000474, 0.8333333333333000637, 1.000000000000000000, 1.020519780480000138 ),
 ( -0.3582002740325999635, 1.358566136073000141 ),
 .UNSPECIFIED. ) ;
#58270 = CARTESIAN_POINT ( 'NONE',  ( -9.495603837127998048, -78.32176524200400536, -6.055366803880999349 ) ) ;
#58271 = CARTESIAN_POINT ( 'NONE',  ( 0.2845710395804645909, -81.95718609884063710, 1.217605880370489446 ) ) ;
#58272 = CARTESIAN_POINT ( 'NONE',  ( 1.545390935813999889, -78.14884706267000070, 0.1070856457118000010 ) ) ;
#58273 = CARTESIAN_POINT ( 'NONE',  ( 1.208267226953838591, -61.62590682120165297, 12.70228502427621997 ) ) ;
#58274 = CARTESIAN_POINT ( 'NONE',  ( -1.035861440536891553, -82.81476822920818393, -1.098648061763779937 ) ) ;
#58275 = DIRECTION ( 'NONE',  ( 0.000000000000000000, -1.000000000000000000, 0.000000000000000000 ) ) ;
#58276 = CARTESIAN_POINT ( 'NONE',  ( 2.126420427321150441, -80.24120890908154990, -10.53736461004005953 ) ) ;
#58277 = CARTESIAN_POINT ( 'NONE',  ( 12.50000000000000000, -18.55321828668999729, -1.250000000000000000 ) ) ;
#58278 = CARTESIAN_POINT ( 'NONE',  ( 3.371482348195443457, -79.49920233275777548, -10.69835107572759902 ) ) ;
#58279 = CARTESIAN_POINT ( 'NONE',  ( 12.52785477533552516, -55.00586572896404647, -1.668513102962561945 ) ) ;
#58280 = ADVANCED_FACE ( 'NONE', ( #31982 ), #39971, .T. ) ;
#58281 = DIRECTION ( 'NONE',  ( 0.000000000000000000, 0.000000000000000000, -1.000000000000000000 ) ) ;
#58282 = CARTESIAN_POINT ( 'NONE',  ( 8.796335266379987416, -79.40208333333335133, 6.760013919724053189 ) ) ;
#58283 = CARTESIAN_POINT ( 'NONE',  ( 2.392795665116000059, -80.24857547445330397, 10.66634390655999987 ) ) ;
#58284 = CARTESIAN_POINT ( 'NONE',  ( -0.6295237254636235624, -80.08333333333331439, -1.092232985442822990 ) ) ;
#58285 = VERTEX_POINT ( 'NONE', #17542 ) ;
#58286 = ORIENTED_EDGE ( 'NONE', *, *, #16533, .F. ) ;
#58287 = CARTESIAN_POINT ( 'NONE',  ( -0.1437691919948000108, -81.10984761958199840, -1.608273716018000066 ) ) ;
#58288 = EDGE_LOOP ( 'NONE', ( #46143, #34965, #15470, #54382 ) ) ;
#58289 = CARTESIAN_POINT ( 'NONE',  ( 0.5999999999999999778, -23.15000000000999947, -11.79999999999999893 ) ) ;
#58290 = ORIENTED_EDGE ( 'NONE', *, *, #9493, .T. ) ;
#58291 = CARTESIAN_POINT ( 'NONE',  ( 1.102622140505636006, -80.38934177173996432, 0.5889613092908587699 ) ) ;
#58292 = CARTESIAN_POINT ( 'NONE',  ( 8.693423296916000353, -80.04523846126194542, -7.148151291522000683 ) ) ;
#58293 = AXIS2_PLACEMENT_3D ( 'NONE', #36849, #41578, #9122 ) ;
#58294 = DIRECTION ( 'NONE',  ( 1.000000000000000000, 0.000000000000000000, 0.000000000000000000 ) ) ;
#58295 = CARTESIAN_POINT ( 'NONE',  ( 6.654794014482000364, -79.31766689940799608, -8.798605060253001042 ) ) ;
#58296 = CARTESIAN_POINT ( 'NONE',  ( -0.9113424693944000010, -24.82535793559999959, -12.54674099557999867 ) ) ;
#58297 = CARTESIAN_POINT ( 'NONE',  ( 1.764864478548999971, -80.01295594358298047, 3.316115785640000091 ) ) ;
#58298 = CARTESIAN_POINT ( 'NONE',  ( -3.585728412114033148, -79.30548461880201216, 8.797105590405882580 ) ) ;
#58299 = EDGE_LOOP ( 'NONE', ( #8534, #17912, #23693, #26176 ) ) ;
#58300 = CARTESIAN_POINT ( 'NONE',  ( 2.993649408183152616, -77.20255476765863989, 10.33029624542498226 ) ) ;
#58301 = CARTESIAN_POINT ( 'NONE',  ( 7.050117653951000207, -79.09252343021999820, -9.969126685360000906 ) ) ;
#58303 = ORIENTED_EDGE ( 'NONE', *, *, #10059, .T. ) ;
#58302 = APPLICATION_CONTEXT ( 'automotive_design' ) ;
#58304 = ORIENTED_EDGE ( 'NONE', *, *, #36825, .F. ) ;
#58305 = LINE ( 'NONE', #4872, #41440 ) ;
#58306 = CARTESIAN_POINT ( 'NONE',  ( -1.499999999971000086, -77.75000000002998490, -1.761798912373000190E-09 ) ) ;
#58307 = CARTESIAN_POINT ( 'NONE',  ( -0.9102058945833000347, -80.65666449956201234, 0.9747214924314999696 ) ) ;
#58308 = CARTESIAN_POINT ( 'NONE',  ( 7.405962610586999340, -77.40363563895398613, -6.270759699041999369 ) ) ;
#58309 = CARTESIAN_POINT ( 'NONE',  ( -3.808769407548595165, -86.12610001270962812, -2.658222959242257044 ) ) ;
#58310 = CARTESIAN_POINT ( 'NONE',  ( -3.106054822367000146, -86.10000002299598520, 1.382903988153999952 ) ) ;
#58311 = CARTESIAN_POINT ( 'NONE',  ( 5.690325051763000630, -78.25735805811000034, 11.64023780191999968 ) ) ;
#58312 = CARTESIAN_POINT ( 'NONE',  ( -1.155570385622000096, -76.86209425748999990, -12.58848097821000067 ) ) ;
#58313 = CARTESIAN_POINT ( 'NONE',  ( 7.355956161948723704, -77.74587193750340930, -5.927457667800279495 ) ) ;
#58314 = DIRECTION ( 'NONE',  ( -0.7071067811865475727, 0.000000000000000000, 0.7071067811865475727 ) ) ;
#58315 = CARTESIAN_POINT ( 'NONE',  ( 9.161831023485000003, -77.27878667140099367, 2.587011072425999814 ) ) ;
#58316 = CARTESIAN_POINT ( 'NONE',  ( 3.737172096265999777, -81.33571061287598525, 1.318914288780999922 ) ) ;
#58317 = CARTESIAN_POINT ( 'NONE',  ( 12.00000000000000000, -76.54999999999999716, 0.000000000000000000 ) ) ;
#58318 = FACE_OUTER_BOUND ( 'NONE', #55905, .T. ) ;
#58319 = CARTESIAN_POINT ( 'NONE',  ( -2.717002840909000128, -78.81000264934789357, -2.276623835180000111 ) ) ;
#58320 = AXIS2_PLACEMENT_3D ( 'NONE', #31075, #14251, #54707 ) ;
#58321 = CARTESIAN_POINT ( 'NONE',  ( 12.00000000000000000, -77.54999999999999716, 0.000000000000000000 ) ) ;
#58322 = CARTESIAN_POINT ( 'NONE',  ( 10.07210119001000059, -80.68864150678149372, 5.045985883512999592 ) ) ;
#58323 = CARTESIAN_POINT ( 'NONE',  ( 3.772660615778999915, -2.008549966925000430, 0.5031134774969999723 ) ) ;
#58324 = CARTESIAN_POINT ( 'NONE',  ( 0.4533703023547435151, -79.40394685360605820, -1.191177121937188721 ) ) ;
#58325 = ORIENTED_EDGE ( 'NONE', *, *, #22348, .F. ) ;
#58326 = CARTESIAN_POINT ( 'NONE',  ( 9.249938314532530015, -78.85038283385668478, 0.03259585398855812527 ) ) ;
#58327 = CYLINDRICAL_SURFACE ( 'NONE', #24188, 12.00000000000000000 ) ;
#58328 = CARTESIAN_POINT ( 'NONE',  ( -0.8218343019581000330, -80.75027928519300247, -1.050237832603999832 ) ) ;
#58329 = CARTESIAN_POINT ( 'NONE',  ( -12.66319948256999872, -16.81851729361000380, -0.1456213732515000137 ) ) ;
#58330 = CARTESIAN_POINT ( 'NONE',  ( -9.692839446179998930, -78.43249358183999220, 7.074522137259999788 ) ) ;
#58331 = VECTOR ( 'NONE', #33968, 1000.000000000000114 ) ;
#58332 = ADVANCED_FACE ( 'NONE', ( #739 ), #4558, .T. ) ;
#58333 = CARTESIAN_POINT ( 'NONE',  ( 8.925918906643000028, -79.22628667140099878, -3.612080431657000101 ) ) ;
#58334 = CARTESIAN_POINT ( 'NONE',  ( 12.87024489156999962, -22.78461666469000235, -2.062597265787999845 ) ) ;
#58335 = ORIENTED_EDGE ( 'NONE', *, *, #4837, .F. ) ;
#58336 = CARTESIAN_POINT ( 'NONE',  ( 0.000000000000000000, -87.20000000000000284, 0.000000000000000000 ) ) ;
#58337 = CARTESIAN_POINT ( 'NONE',  ( 8.718213946484933530, -76.96041666667038328, -3.877033208488974925 ) ) ;
#58338 = CARTESIAN_POINT ( 'NONE',  ( 0.8482627942206000249, -81.62088116725298903, 1.124385767671000069 ) ) ;
#58339 = CARTESIAN_POINT ( 'NONE',  ( -1.000000000000000000, -78.00000000000000000, -7.200000000000000178 ) ) ;
#58340 = CARTESIAN_POINT ( 'NONE',  ( 7.120006596302999924, -77.76472321436799007, 6.322648361264000094 ) ) ;
#58342 = CARTESIAN_POINT ( 'NONE',  ( 2.301364338783000285, -1.456223928488999952, -3.291430154679999998 ) ) ;
#58341 = CARTESIAN_POINT ( 'NONE',  ( -3.328554525807000175, -84.66293396287998974, -2.445248093468999961 ) ) ;
#58343 = CARTESIAN_POINT ( 'NONE',  ( 0.6295237254636211199, -82.33333333333335702, 1.092232985442824322 ) ) ;
#58344 = CARTESIAN_POINT ( 'NONE',  ( -1.410851365044999861, -79.59482349039599569, 0.1398492253880000147 ) ) ;
#58345 = ORIENTED_EDGE ( 'NONE', *, *, #48146, .T. ) ;
#58346 = CARTESIAN_POINT ( 'NONE',  ( -2.015531751727218435, -77.21013824102965373, -10.56028365160725535 ) ) ;
#58347 = CARTESIAN_POINT ( 'NONE',  ( -1.500000000000000000, -79.40884741929301072, -0.1667699247263852436 ) ) ;
#58348 = CARTESIAN_POINT ( 'NONE',  ( -3.962812355711000212, -78.85171438276199751, -1.662781298490902161E-14 ) ) ;
#58349 = ORIENTED_EDGE ( 'NONE', *, *, #23912, .T. ) ;
#58351 = ADVANCED_FACE ( 'NONE', ( #21960 ), #18997, .T. ) ;
#58350 = ORIENTED_EDGE ( 'NONE', *, *, #4837, .T. ) ;
#58352 = CARTESIAN_POINT ( 'NONE',  ( 6.591600424694998850, -79.69435522376399206, 8.731473042948000085 ) ) ;
#58353 = CARTESIAN_POINT ( 'NONE',  ( -5.944540622819851627, -76.10208333280840520, -10.31217357874345630 ) ) ;
#58354 = CARTESIAN_POINT ( 'NONE',  ( -2.600000000000000089, -77.49999999999998579, 0.000000000000000000 ) ) ;
#58355 = VERTEX_POINT ( 'NONE', #53560 ) ;
#58356 = CARTESIAN_POINT ( 'NONE',  ( 0.3886576371541999864, -77.31875387357798957, -11.81216847760999933 ) ) ;
#58357 = ORIENTED_EDGE ( 'NONE', *, *, #23570, .T. ) ;
#58358 = EDGE_LOOP ( 'NONE', ( #35741, #10292, #45227, #54814, #34600 ) ) ;
#58359 = CARTESIAN_POINT ( 'NONE',  ( -1.232277669651724583, -2.694870653336070454, -3.006800154367852862 ) ) ;
#58360 = AXIS2_PLACEMENT_3D ( 'NONE', #25341, #39780, #21201 ) ;
#58361 = EDGE_CURVE ( 'NONE', #13326, #9068, #1108, .T. ) ;
#58362 = CARTESIAN_POINT ( 'NONE',  ( -12.00019890019965096, -76.39977373798492977, -1.177339121803222359E-06 ) ) ;
#58363 = CARTESIAN_POINT ( 'NONE',  ( 8.193575559979001000, -79.54581634543151836, 5.316613930189999948 ) ) ;
#58364 = EDGE_CURVE ( 'NONE', #28435, #27557, #54813, .T. ) ;
#58365 = ORIENTED_EDGE ( 'NONE', *, *, #32682, .T. ) ;
#58366 = ORIENTED_EDGE ( 'NONE', *, *, #30225, .T. ) ;
#58367 = CARTESIAN_POINT ( 'NONE',  ( -3.962108358898298821, -78.85171438276199751, 0.07469349987780400657 ) ) ;
#58368 = CARTESIAN_POINT ( 'NONE',  ( 10.18949731070000020, -55.58470987670000341, 7.645392562244000878 ) ) ;
#58369 = AXIS2_PLACEMENT_3D ( 'NONE', #17563, #51346, #56063 ) ;
#58370 = CARTESIAN_POINT ( 'NONE',  ( -7.668936932623999780, -22.77152778045000048, -10.21380041493000057 ) ) ;
#58371 = CARTESIAN_POINT ( 'NONE',  ( 3.074306947300566861, -77.34369429684161901, -11.43804941158839306 ) ) ;
#58372 = CARTESIAN_POINT ( 'NONE',  ( -11.75000000000000000, -78.79999999999999716, 1.318041981624000073E-14 ) ) ;
#58373 = CARTESIAN_POINT ( 'NONE',  ( 7.691916945401000127, -58.55365779174999830, -10.42274798264000069 ) ) ;
#58374 = CARTESIAN_POINT ( 'NONE',  ( 7.258298179997606958, -78.79682822265634456, -5.734190774355525377 ) ) ;
#58375 = CARTESIAN_POINT ( 'NONE',  ( -9.641208724080000181, -24.43394297700999829, 7.943747389698999406 ) ) ;
#58377 = EDGE_CURVE ( 'NONE', #21227, #55354, #4610, .T. ) ;
#58376 = DIRECTION ( 'NONE',  ( 1.000000000000000000, 0.000000000000000000, 0.000000000000000000 ) ) ;
#58378 = CARTESIAN_POINT ( 'NONE',  ( 0.5579309975780000208, -79.05050264934789084, -4.137430296115999440 ) ) ;
#58379 = CARTESIAN_POINT ( 'NONE',  ( 9.794900829080001259, -77.58066001420199598, 1.237383733679000120 ) ) ;
#58380 = CARTESIAN_POINT ( 'NONE',  ( -12.66322081671000177, -16.81838367322000138, 0.1487102037789999887 ) ) ;
#58381 = CARTESIAN_POINT ( 'NONE',  ( -11.00000000000000888, -78.08958333333330870, 1.439896632895276252 ) ) ;
#58382 = DIRECTION ( 'NONE',  ( 0.000000000000000000, -1.000000000000000000, 0.000000000000000000 ) ) ;
#58383 = CARTESIAN_POINT ( 'NONE',  ( -3.023821996898440112, -79.99699371105347723, 10.64354645710085023 ) ) ;
#58384 = CARTESIAN_POINT ( 'NONE',  ( -2.858933815907000131, -84.87007892634498774, -2.100251748468999757 ) ) ;
#58385 = CARTESIAN_POINT ( 'NONE',  ( 1.829579065110999991, -1.222748962127999883, -3.127009326567999903 ) ) ;
#58386 = DIRECTION ( 'NONE',  ( 0.07798810159162851419, -0.04890177460079911387, 0.9957542229139811907 ) ) ;
#58387 = AXIS2_PLACEMENT_3D ( 'NONE', #178, #18151, #36147 ) ;
#58388 = CARTESIAN_POINT ( 'NONE',  ( -1.320768259162522273, -80.80883367555978225, 0.7383452188593548904 ) ) ;
#58389 = CARTESIAN_POINT ( 'NONE',  ( 12.57354097144999905, -60.52384125708999818, -1.757953070309000054 ) ) ;
#58390 = DIRECTION ( 'NONE',  ( 1.000000000000000000, 0.000000000000000000, 0.000000000000000000 ) ) ;
#58391 = LINE ( 'NONE', #8794, #42718 ) ;
#58392 = CARTESIAN_POINT ( 'NONE',  ( 7.977342298186999692, -77.83638398095499156, 7.452340293345999456 ) ) ;
#58393 = CARTESIAN_POINT ( 'NONE',  ( 1.747513281931999840, -77.07779697871899316, -11.88039736288000014 ) ) ;
#58394 = CARTESIAN_POINT ( 'NONE',  ( -9.700000000000001066, -90.29999999999999716, 0.000000000000000000 ) ) ;
#58395 = CIRCLE ( 'NONE', #34777, 0.6999999999999999556 ) ;
#58396 = CARTESIAN_POINT ( 'NONE',  ( -8.596418555780431348, -79.05208333333331439, -6.606377239730338857 ) ) ;
#58398 = CARTESIAN_POINT ( 'NONE',  ( -0.6374375075192000306, -78.70942315521899957, 1.266385724874999896 ) ) ;
#58397 = CARTESIAN_POINT ( 'NONE',  ( 0.000000000000000000, -81.89999999962999766, 0.000000000000000000 ) ) ;
#58399 = CARTESIAN_POINT ( 'NONE',  ( 0.8470819118255000779, -81.60354343447998815, 1.477252506412999988 ) ) ;
#58400 = ORIENTED_EDGE ( 'NONE', *, *, #33671, .F. ) ;
#58401 = CARTESIAN_POINT ( 'NONE',  ( -2.400545987948000004, -84.79521544543099765, 2.889418808065000288 ) ) ;
#58402 = CARTESIAN_POINT ( 'NONE',  ( 1.140106547902999923, -78.99079040463000467, 11.87165445709000089 ) ) ;
#58403 = CARTESIAN_POINT ( 'NONE',  ( 11.16260469787999909, -80.88779469070068728, -0.4690387474302000204 ) ) ;
#58404 = DIRECTION ( 'NONE',  ( 0.000000000000000000, -1.000000000000000000, 0.000000000000000000 ) ) ;
#58405 = CARTESIAN_POINT ( 'NONE',  ( -3.317802080653412311, -84.63541667694400417, 0.9251688977279969306 ) ) ;
#58406 = CARTESIAN_POINT ( 'NONE',  ( 7.199825537761999961, -77.15343348694199221, 8.601198917431998936 ) ) ;
#58407 = DIRECTION ( 'NONE',  ( -3.552713678800000476E-14, -1.000000000000000000, -1.110223024625000030E-13 ) ) ;
#58408 = NEXT_ASSEMBLY_USAGE_OCCURRENCE ( 'NAUO1', ' ', ' ', #21399, #39775, $ ) ;
#58409 = NEXT_ASSEMBLY_USAGE_OCCURRENCE ( 'NAUO2', ' ', ' ', #21399, #518, $ ) ;
#58410 = NEXT_ASSEMBLY_USAGE_OCCURRENCE ( 'NAUO3', ' ', ' ', #21399, #54603, $ ) ;
#58411 = NEXT_ASSEMBLY_USAGE_OCCURRENCE ( 'NAUO4', ' ', ' ', #21399, #4815, $ ) ;
#58412 = NEXT_ASSEMBLY_USAGE_OCCURRENCE ( 'NAUO5', ' ', ' ', #21399, #55670, $ ) ;
#58413 = NEXT_ASSEMBLY_USAGE_OCCURRENCE ( 'NAUO6', ' ', ' ', #21399, #49537, $ ) ;
#58414 = NEXT_ASSEMBLY_USAGE_OCCURRENCE ( 'NAUO7', ' ', ' ', #21399, #45957, $ ) ;
#58415 = NEXT_ASSEMBLY_USAGE_OCCURRENCE ( 'NAUO8', ' ', ' ', #21399, #10957, $ ) ;
ENDSEC;
END-ISO-10303-21;
